#50967 = CARTESIAN_POINT ( 'NONE',  ( 171.6880688175457408, 289.7684859944451432, 2.704731161792437888 ) ) ;
#50968 = DIRECTION ( 'NONE',  ( -0.8660254037844387076, -0.4999999999999998890, -0.000000000000000000 ) ) ;
#50969 = CARTESIAN_POINT ( 'NONE',  ( 81.17742577809939064, 43.43109523646555203, -9.910019672670513202 ) ) ;
#50970 = DIRECTION ( 'NONE',  ( -0.7492053821869066876, -0.6623377501714446947, 0.000000000000000000 ) ) ;
#50971 = CARTESIAN_POINT ( 'NONE',  ( 14.51920287573142510, 173.0643266524160424, 9.188101187500095079 ) ) ;
#50972 = CARTESIAN_POINT ( 'NONE',  ( 101.9066655502961964, 220.4548013555409511, -4.594050593750042211 ) ) ;
#50973 = CARTESIAN_POINT ( 'NONE',  ( 44.69460199273694911, 186.6115022471902023, -5.000000000000041744 ) ) ;
#50974 = CARTESIAN_POINT ( 'NONE',  ( 186.5064012131073810, 296.3665785887476432, -7.270687472978205612 ) ) ;
#50975 = CARTESIAN_POINT ( 'NONE',  ( 78.18546057057351106, 52.16385450527234013, 15.57755498089799850 ) ) ;
#50976 = DIRECTION ( 'NONE',  ( 0.5000000000000014433, -0.8660254037844378194, 0.000000000000000000 ) ) ;
#50977 = CARTESIAN_POINT ( 'NONE',  ( 153.1747891862213748, 277.6390251779605478, -8.000862867047169757 ) ) ;
#50978 = CARTESIAN_POINT ( 'NONE',  ( 194.8708600166808651, 293.1207648669033006, -14.79199694356877970 ) ) ;
#50979 = EDGE_CURVE ( 'NONE', #22323, #76711, #55182, .T. ) ;
#50980 = CARTESIAN_POINT ( 'NONE',  ( 84.19352825665725959, 50.57172232247530275, 13.77707419306082670 ) ) ;
#50981 = CARTESIAN_POINT ( 'NONE',  ( 182.9159104275373977, 268.0747678481671414, -14.89985435326638630 ) ) ;
#50982 = VECTOR ( 'NONE', #33107, 1000.000000000000000 ) ;
#50983 = CARTESIAN_POINT ( 'NONE',  ( 178.7452121208765448, 291.6717820129654228, -9.156458492754065759 ) ) ;
#50984 = EDGE_CURVE ( 'NONE', #52516, #76128, #70894, .T. ) ;
#50985 = CARTESIAN_POINT ( 'NONE',  ( 172.5304191843750345, 263.6019457708129039, -15.41392963016842721 ) ) ;
#50986 = CARTESIAN_POINT ( 'NONE',  ( 74.78872445064843077, 223.1744531367911293, 4.594050593750047540 ) ) ;
#50987 = EDGE_CURVE ( 'NONE', #82530, #23627, #71400, .T. ) ;
#50988 = EDGE_CURVE ( 'NONE', #49426, #85879, #40954, .T. ) ;
#50989 = CARTESIAN_POINT ( 'NONE',  ( -14.45613220355349426, 103.0143348366940046, 11.63587646907208573 ) ) ;
#50991 = CARTESIAN_POINT ( 'NONE',  ( 86.16743810126995129, 43.04331322985106567, -1.056965546583657822 ) ) ;
#50990 = CARTESIAN_POINT ( 'NONE',  ( 157.0848929289108469, 258.5679796760466047, 17.57466231005294688 ) ) ;
#50992 = CARTESIAN_POINT ( 'NONE',  ( 148.9671336697298045, 272.6283511565604840, 12.24371685916078611 ) ) ;
#50993 = CARTESIAN_POINT ( 'NONE',  ( 199.0363797504450929, 285.9058730480928716, -17.12190301149298222 ) ) ;
#50994 = CARTESIAN_POINT ( 'NONE',  ( 160.6734846709049691, 282.6943762970620924, -6.583290857611773461 ) ) ;
#50995 = CARTESIAN_POINT ( 'NONE',  ( 28.71100085020356474, 39.68290643055189548, 3.479690158560446702E-15 ) ) ;
#50996 = CARTESIAN_POINT ( 'NONE',  ( 192.6679047218190135, 296.9363953644068488, -13.34486378385621386 ) ) ;
#50997 = CARTESIAN_POINT ( 'NONE',  ( 127.3796741259112792, 255.8967562850346553, -4.648177544792955347E-16 ) ) ;
#50998 = EDGE_LOOP ( 'NONE', ( #89984, #28745, #24049, #60020 ) ) ;
#50999 = CARTESIAN_POINT ( 'NONE',  ( 20.42541317417268942, 33.83396525600390703, -2.839279412974133887 ) ) ;
#51000 = CARTESIAN_POINT ( 'NONE',  ( -29.91485116994501325, 25.08783183303773967, 10.00000000000000000 ) ) ;
#51001 = CARTESIAN_POINT ( 'NONE',  ( 192.4743214706506365, 297.2716913909250707, -12.17804856100553046 ) ) ;
#51002 = CARTESIAN_POINT ( 'NONE',  ( 60.28305926085680966, 205.6115022471902591, 10.00000000000009592 ) ) ;
#51003 = EDGE_CURVE ( 'NONE', #3615, #8702, #3502, .T. ) ;
#51004 = EDGE_CURVE ( 'NONE', #16059, #66385, #57663, .T. ) ;
#51005 = VERTEX_POINT ( 'NONE', #11103 ) ;
#51006 = CARTESIAN_POINT ( 'NONE',  ( 70.83557099577411975, 60.89137392342752975, 14.54819139492075841 ) ) ;
#51007 = DIRECTION ( 'NONE',  ( -0.8560416229147732592, -0.5169068966820244970, 0.000000000000000000 ) ) ;
#51008 = CARTESIAN_POINT ( 'NONE',  ( 193.8475705658754578, 288.0377294361514373, 16.93899091255358869 ) ) ;
#51009 = CARTESIAN_POINT ( 'NONE',  ( -19.65312891409030271, 93.06504152958497400, 10.00000000000000888 ) ) ;
#51010 = CARTESIAN_POINT ( 'NONE',  ( 130.8641296692885305, 256.3615022471903444, 5.000000000000046185 ) ) ;
#51011 = CARTESIAN_POINT ( 'NONE',  ( 205.1300674467857164, 275.3512963525735131, -12.60245643603069610 ) ) ;
#51012 = CARTESIAN_POINT ( 'NONE',  ( 75.37222269001998143, 53.48600193327490615, 16.03910331961625246 ) ) ;
#51013 = VERTEX_POINT ( 'NONE', #96720 ) ;
#51014 = CARTESIAN_POINT ( 'NONE',  ( 190.5844311467533316, 299.4370547860769989, -6.522056084446611557 ) ) ;
#51015 = CARTESIAN_POINT ( 'NONE',  ( 188.7150346277363155, 272.5491880637262057, 16.57045186533353487 ) ) ;
#51016 = ORIENTED_EDGE ( 'NONE', *, *, #92741, .T. ) ;
#51017 = CARTESIAN_POINT ( 'NONE',  ( 163.2442700311756596, 247.8996255919473697, 11.14021925110252020 ) ) ;
#51018 = CARTESIAN_POINT ( 'NONE',  ( 81.51603451045065185, 42.23037173800174315, -8.032388100303403888 ) ) ;
#51019 = CARTESIAN_POINT ( 'NONE',  ( 77.30032487123098406, 63.32994978619627346, -15.17488454575836521 ) ) ;
#51020 = ORIENTED_EDGE ( 'NONE', *, *, #83508, .F. ) ;
#51021 = CARTESIAN_POINT ( 'NONE',  ( 191.1374494863389373, 291.0598754717474890, 14.59185211929525749 ) ) ;
#51022 = CARTESIAN_POINT ( 'NONE',  ( 158.8391802440265508, 255.5294649151923636, 17.60341940305819364 ) ) ;
#51023 = CARTESIAN_POINT ( 'NONE',  ( 151.1618603905361624, 248.8923013555409796, 4.594050593750050204 ) ) ;
#51024 = CARTESIAN_POINT ( 'NONE',  ( 205.1877054856971938, 273.8747620413109871, 10.81913124959201689 ) ) ;
#51025 = CARTESIAN_POINT ( 'NONE',  ( 201.1755594471486859, 282.2007051268825535, -18.15567516623250910 ) ) ;
#51026 = AXIS2_PLACEMENT_3D ( 'NONE', #43719, #98947, #30019 ) ;
#51027 = CARTESIAN_POINT ( 'NONE',  ( 34.90123498099573851, 22.01110640527294393, 2.839279412974134775 ) ) ;
#51028 = FACE_OUTER_BOUND ( 'NONE', #7815, .T. ) ;
#51029 = FACE_OUTER_BOUND ( 'NONE', #74837, .T. ) ;
#51031 = VECTOR ( 'NONE', #15286, 1000.000000000000000 ) ;
#51030 = CARTESIAN_POINT ( 'NONE',  ( 87.64858773784966672, 45.45714736155468927, 6.714362014711301896 ) ) ;
#51032 = EDGE_LOOP ( 'NONE', ( #78816, #52304, #48168, #76488 ) ) ;
#51033 = CARTESIAN_POINT ( 'NONE',  ( 86.70911053808110580, 46.89117940024963360, 10.21290512048939902 ) ) ;
#51035 = CARTESIAN_POINT ( 'NONE',  ( 162.7552554279882031, 272.8056902114326476, -16.37138898352977634 ) ) ;
#51034 = CARTESIAN_POINT ( 'NONE',  ( 163.8040269124969939, 246.9300982336122559, 6.025552750865228013 ) ) ;
#51036 = CARTESIAN_POINT ( 'NONE',  ( 85.54106661513783649, 48.65811287445264810, 12.45824154186499833 ) ) ;
#51037 = CYLINDRICAL_SURFACE ( 'NONE', #26276, 10.00000000000010658 ) ;
#51038 = CARTESIAN_POINT ( 'NONE',  ( 152.5423653171682474, 268.4358682943698682, -15.78187745328793490 ) ) ;
#51039 = CARTESIAN_POINT ( 'NONE',  ( 82.15463706511576447, 40.84277258114416753, 1.595534587534163995 ) ) ;
#51040 = CARTESIAN_POINT ( 'NONE',  ( 167.1313658916855900, 286.5916946420441604, -4.904932445929851781 ) ) ;
#51041 = CARTESIAN_POINT ( 'NONE',  ( 169.5532941354267962, 267.3202395055815259, 16.92450780793635090 ) ) ;
#51042 = CARTESIAN_POINT ( 'NONE',  ( 180.9973211531476238, 256.8713260056199488, 4.953687155094200101 ) ) ;
#51043 = CARTESIAN_POINT ( 'NONE',  ( 100.7969837277561282, 222.8768266524159856, -9.188101187500091527 ) ) ;
#51044 = VERTEX_POINT ( 'NONE', #65278 ) ;
#51045 = CARTESIAN_POINT ( 'NONE',  ( 190.8623743139412454, 300.0636657654615647, 8.577953960666059530 ) ) ;
#51046 = CARTESIAN_POINT ( 'NONE',  ( 166.8260628573998474, 278.3289732347862468, -13.29658692297307176 ) ) ;
#51047 = EDGE_LOOP ( 'NONE', ( #58789, #79890 ) ) ;
#51048 = AXIS2_PLACEMENT_3D ( 'NONE', #9684, #49651, #32952 ) ;
#51049 = ORIENTED_EDGE ( 'NONE', *, *, #32096, .T. ) ;
#51050 = CARTESIAN_POINT ( 'NONE',  ( 87.10310940712852812, 46.00011840676027219, -8.174603884307702018 ) ) ;
#51051 = CARTESIAN_POINT ( 'NONE',  ( 176.9023546970497875, 292.4662729303109927, -2.727046248897896596 ) ) ;
#51052 = CARTESIAN_POINT ( 'NONE',  ( 157.5520850189458884, 257.7587792392113215, 16.71892742266126319 ) ) ;
#51053 = CARTESIAN_POINT ( 'NONE',  ( 7.357472841178069878, 27.18080186712591484, 3.090169943749475401 ) ) ;
#51054 = LINE ( 'NONE', #97211, #18824 ) ;
#51055 = EDGE_LOOP ( 'NONE', ( #59994, #14792, #49814, #80658, #61751, #87391, #36961, #44258, #12701, #46519, #19920, #88098, #69944, #34124, #23713, #89691, #93946, #26144, #96073, #94059 ) ) ;
#51056 = VECTOR ( 'NONE', #31018, 1000.000000000000227 ) ;
#51057 =( BOUNDED_CURVE ( )  B_SPLINE_CURVE ( 2, ( #55698, #1036, #49137, #23818, #17218, #31915, #62819, #85692, #93775 ),
 .UNSPECIFIED., .F., .F. ) 
 B_SPLINE_CURVE_WITH_KNOTS ( ( 3, 2, 2, 2, 3 ),
 ( 0.4959677419354838745, 0.4973118279569892497, 0.5000000000000000000, 0.5026881720430107503, 0.5040322580645161255 ),
 .UNSPECIFIED. ) 
 CURVE ( )  GEOMETRIC_REPRESENTATION_ITEM ( )  RATIONAL_B_SPLINE_CURVE ( ( 0.9330127018922194093, 0.9330127018922194093, 1.000000000000000000, 0.8660254037844387076, 1.000000000000000000, 0.8660254037844387076, 1.000000000000000000, 0.9330127018922194093, 0.9330127018922194093 ) ) 
 REPRESENTATION_ITEM ( '' )  );
#51058 = CARTESIAN_POINT ( 'NONE',  ( 187.1504858166771896, 267.1035762790165222, -14.63698944013293968 ) ) ;
#51059 = DIRECTION ( 'NONE',  ( -0.5000000000000011102, -0.8660254037844380415, 0.000000000000000000 ) ) ;
#51060 = ORIENTED_EDGE ( 'NONE', *, *, #86050, .F. ) ;
#51061 = CARTESIAN_POINT ( 'NONE',  ( 70.78770575672112386, 64.97714170464311678, 12.24875154412454314 ) ) ;
#51062 = ADVANCED_FACE ( 'NONE', ( #58168 ), #89152, .F. ) ;
#51063 = CARTESIAN_POINT ( 'NONE',  ( 191.4217213000991364, 263.9549948794881971, -7.974474884843431255 ) ) ;
#51064 = CARTESIAN_POINT ( 'NONE',  ( 13.95070015838929400, 188.8615022471903160, 5.000000000000046185 ) ) ;
#51065 = CARTESIAN_POINT ( 'NONE',  ( 83.42856800471859913, 47.51705139073896333, 11.98419555216981003 ) ) ;
#51067 = CARTESIAN_POINT ( 'NONE',  ( 69.64257305926975050, 62.32707857316431443, -13.51840679933402711 ) ) ;
#51066 = CARTESIAN_POINT ( 'NONE',  ( 127.4808708382166316, 256.6589784336661637, -6.496448406907675876E-16 ) ) ;
#51068 = PLANE ( 'NONE',  #13891 ) ;
#51069 = ORIENTED_EDGE ( 'NONE', *, *, #31427, .F. ) ;
#51070 = CARTESIAN_POINT ( 'NONE',  ( 204.9134960529544287, 275.7264090101555212, 14.56629498631681408 ) ) ;
#51071 = CARTESIAN_POINT ( 'NONE',  ( 81.82384807472087118, 49.02608080520630551, 13.57111770008744500 ) ) ;
#51072 = CARTESIAN_POINT ( 'NONE',  ( 82.36513698948819240, 40.35680866276053536, -0.9065428034150362357 ) ) ;
#51073 = CARTESIAN_POINT ( 'NONE',  ( 192.9064638172013417, 270.9369261147751331, 14.92505667092759758 ) ) ;
#51075 = EDGE_CURVE ( 'NONE', #21534, #88756, #41080, .T. ) ;
#51074 = CARTESIAN_POINT ( 'NONE',  ( 178.6016452153454850, 285.1529245495667624, 13.66975983559747831 ) ) ;
#51076 = CARTESIAN_POINT ( 'NONE',  ( 76.12676022442599333, 51.56486861732116012, -16.17662836183246711 ) ) ;
#51077 = ADVANCED_FACE ( 'NONE', ( #66279 ), #41620, .T. ) ;
#51078 = CARTESIAN_POINT ( 'NONE',  ( 196.0123035030964047, 280.0493583844649947, -16.77947975799478542 ) ) ;
#51079 = CARTESIAN_POINT ( 'NONE',  ( 142.9371257517045137, 259.7655487066560340, -7.305945665944389766 ) ) ;
#51080 = CARTESIAN_POINT ( 'NONE',  ( 79.32243881128263752, 47.71223523376870190, 13.60867400304461050 ) ) ;
#51081 = CARTESIAN_POINT ( 'NONE',  ( 206.8014039808918199, 271.9024147334357053, 6.414352906864584369 ) ) ;
#51082 = CARTESIAN_POINT ( 'NONE',  ( 206.8317058779879574, 272.4039721336197317, -10.41591514895975834 ) ) ;
#51083 = LINE ( 'NONE', #59164, #9507 ) ;
#51084 = CARTESIAN_POINT ( 'NONE',  ( 163.3723087697842971, 247.6778559913402091, -10.08585062664141319 ) ) ;
#51085 = EDGE_CURVE ( 'NONE', #95597, #31449, #22062, .T. ) ;
#51086 = DIRECTION ( 'NONE',  ( -0.8660254037844387076, -0.4999999999999998890, -0.000000000000000000 ) ) ;
#51087 = VECTOR ( 'NONE', #72913, 1000.000000000000000 ) ;
#51088 = CARTESIAN_POINT ( 'NONE',  ( 185.9501193373536125, 265.4400708382679568, 13.68843392893370314 ) ) ;
#51089 = CARTESIAN_POINT ( 'NONE',  ( -22.47745507583526958, 59.95093256704510054, -10.00000000000000000 ) ) ;
#51090 = CARTESIAN_POINT ( 'NONE',  ( 29.61202869050421427, 35.83478043621390441, -8.090169943749479842 ) ) ;
#51091 = CARTESIAN_POINT ( 'NONE',  ( -57.88150100324660485, 35.92665207732902388, -10.00000000000000000 ) ) ;
#51092 = LINE ( 'NONE', #64824, #33060 ) ;
#51093 = CARTESIAN_POINT ( 'NONE',  ( 50.40832357593285451, 87.79023373031367328, -10.00000000000000000 ) ) ;
#51094 = AXIS2_PLACEMENT_3D ( 'NONE', #5829, #52419, #4855 ) ;
#51095 = CARTESIAN_POINT ( 'NONE',  ( 83.98302130751108052, 43.28427656522794820, -6.397989684056143211 ) ) ;
#51096 = EDGE_CURVE ( 'NONE', #48833, #40485, #20906, .T. ) ;
#51097 = CARTESIAN_POINT ( 'NONE',  ( 15.54743449484293372, 179.7833772461660544, -9.188101187500095079 ) ) ;
#51098 = CARTESIAN_POINT ( 'NONE',  ( 207.3567728362337732, 271.1044343289145218, 2.587868728010163100 ) ) ;
#51099 = ORIENTED_EDGE ( 'NONE', *, *, #27553, .F. ) ;
#51100 = EDGE_CURVE ( 'NONE', #73348, #41972, #26001, .T. ) ;
#51101 = CARTESIAN_POINT ( 'NONE',  ( 87.19358828159984398, 46.06351791880832991, 8.846884648199045742 ) ) ;
#51102 = ADVANCED_FACE ( 'NONE', ( #93424 ), #18397, .T. ) ;
#51103 = DIRECTION ( 'NONE',  ( -0.3074612162317687525, 0.9515606131578174809, 0.000000000000000000 ) ) ;
#51104 = CARTESIAN_POINT ( 'NONE',  ( 164.4405316900629259, 245.8276396196081350, -6.144538123479245328 ) ) ;
#51105 = CARTESIAN_POINT ( 'NONE',  ( -19.65312891409030271, 93.06504152958497400, -10.00000000000000888 ) ) ;
#51106 = CARTESIAN_POINT ( 'NONE',  ( 51.43353571204313823, 194.3768266524159856, -9.188101187500093303 ) ) ;
#51107 = CARTESIAN_POINT ( 'NONE',  ( 86.78549426258130950, 45.83013854792883990, 8.849882187839872572 ) ) ;
#51108 = CARTESIAN_POINT ( 'NONE',  ( 171.5767533171608932, 286.7469205890667467, 7.455704898055432572 ) ) ;
#51109 = CARTESIAN_POINT ( 'NONE',  ( 190.4240181651484818, 300.8229208869809668, -4.214281362166949485 ) ) ;
#51110 = CARTESIAN_POINT ( 'NONE',  ( 42.17466224797323804, 36.30066082961425877, -10.00000000000000533 ) ) ;
#51111 = CARTESIAN_POINT ( 'NONE',  ( 178.3571982967953602, 292.6181790745828835, -7.174879954037646002 ) ) ;
#51112 = CARTESIAN_POINT ( 'NONE',  ( 147.0721334091522294, 275.9105878882373304, 0.7242168585908188572 ) ) ;
#51113 = EDGE_CURVE ( 'NONE', #16838, #77804, #86342, .T. ) ;
#51114 = VECTOR ( 'NONE', #5486, 1000.000000000000000 ) ;
#51115 = CARTESIAN_POINT ( 'NONE',  ( 176.1048462933576388, 274.8593126533075974, 17.09347264305319314 ) ) ;
#51116 = LINE ( 'NONE', #80076, #29537 ) ;
#51117 = CARTESIAN_POINT ( 'NONE',  ( 68.55506308078156508, 67.87136273880065573, -7.775597205189836991 ) ) ;
#51118 = EDGE_CURVE ( 'NONE', #87111, #28084, #96763, .T. ) ;
#51119 = CARTESIAN_POINT ( 'NONE',  ( 88.69951781898578247, 222.0177522451418781, -10.00000000000009592 ) ) ;
#51120 = ADVANCED_FACE ( 'NONE', ( #88853 ), #73592, .F. ) ;
#51121 = CARTESIAN_POINT ( 'NONE',  ( -4.429217378738782962, 26.01694505731172313, -10.00000000000000000 ) ) ;
#51122 = CARTESIAN_POINT ( 'NONE',  ( 105.6772241758911832, 218.4865022471901455, 1.119607411625061291E-15 ) ) ;
#51123 = FACE_OUTER_BOUND ( 'NONE', #45277, .T. ) ;
#51124 = CARTESIAN_POINT ( 'NONE',  ( 161.6384288741144815, 267.7291502596664259, -17.04636140397435895 ) ) ;
#51125 = VERTEX_POINT ( 'NONE', #12294 ) ;
#51126 = CARTESIAN_POINT ( 'NONE',  ( 64.42391676880970408, 201.8768266524159856, -9.188101187500091527 ) ) ;
#51127 = VERTEX_POINT ( 'NONE', #43153 ) ;
#51128 = CARTESIAN_POINT ( 'NONE',  ( 11.62691283633230377, 30.21091486745859811, -1.111400068045478839E-16 ) ) ;
#51129 = CARTESIAN_POINT ( 'NONE',  ( 146.8201187048455267, 276.3470901603510015, 4.112223577763169047 ) ) ;
#51130 = CARTESIAN_POINT ( 'NONE',  ( 67.17471155831628948, 67.15864351149404854, -8.572145057571571414 ) ) ;
#51131 = ORIENTED_EDGE ( 'NONE', *, *, #43638, .F. ) ;
#51132 = CARTESIAN_POINT ( 'NONE',  ( 171.3634068529735828, 286.5179807154004834, 7.728413769772275899 ) ) ;
#51133 = CARTESIAN_POINT ( 'NONE',  ( 207.2824254892180704, 271.6233028670009162, 6.274396967990798046 ) ) ;
#51134 = CARTESIAN_POINT ( 'NONE',  ( 78.08206365161463225, 61.83366292688850763, -15.70979438352861735 ) ) ;
#51135 = CARTESIAN_POINT ( 'NONE',  ( 28.38624132378439313, 39.49540643055189548, 3.479690158560446702E-15 ) ) ;
#51136 = CARTESIAN_POINT ( 'NONE',  ( 185.9440050421480919, 263.4269226037905014, 11.01369690752849984 ) ) ;
#51137 = CARTESIAN_POINT ( 'NONE',  ( 174.5432515410337544, 282.4104588529930311, -15.15290805577315680 ) ) ;
#51138 = CARTESIAN_POINT ( 'NONE',  ( 204.3531539698473978, 276.6969499677158524, 13.47943239092699841 ) ) ;
#51139 = ORIENTED_EDGE ( 'NONE', *, *, #17486, .F. ) ;
#51140 = CARTESIAN_POINT ( 'NONE',  ( 11.72364552993787967, 24.95586893147754282, 7.433330006724141015 ) ) ;
#51141 = LINE ( 'NONE', #81109, #33274 ) ;
#51142 = CARTESIAN_POINT ( 'NONE',  ( 70.89819722514211264, 70.25179532443134178, -6.076314343069640245 ) ) ;
#51143 = DIRECTION ( 'NONE',  ( -0.000000000000000000, 0.000000000000000000, -1.000000000000000000 ) ) ;
#51144 = ORIENTED_EDGE ( 'NONE', *, *, #85057, .F. ) ;
#51145 = CARTESIAN_POINT ( 'NONE',  ( 181.7035363212127379, 283.7571070694220907, 14.95731429925001343 ) ) ;
#51146 = B_SPLINE_CURVE_WITH_KNOTS ( 'NONE', 3,
 ( #66945, #58349, #28448, #28964, #82212, #81702, #66459, #13276, #4667, #76081, #89327, #82709, #97384, #27952, #50750, #43136, #58833, #52731, #83694, #21360, #45142, #89799, #19880, #51244 ),
 .UNSPECIFIED., .F., .F.,
 ( 4, 2, 2, 2, 2, 2, 2, 2, 2, 2, 2, 4 ),
 ( 0.000000000000000000, 0.1249999999999907851, 0.2499999999999815703, 0.3749999999999723554, 0.4374999999999739098, 0.4999999999999754641, 0.5624999999999769074, 0.6249999999999784617, 0.6874999999999799050, 0.7499999999999814593, 0.8749999999999906741, 1.000000000000000000 ),
 .UNSPECIFIED. ) ;
#51147 = CARTESIAN_POINT ( 'NONE',  ( 190.8860811105559208, 300.0226043892405414, 8.636347304323541252 ) ) ;
#51148 = CARTESIAN_POINT ( 'NONE',  ( 206.0930919633010774, 273.6832889610345774, -9.866500005465628220 ) ) ;
#51149 = ORIENTED_EDGE ( 'NONE', *, *, #31981, .T. ) ;
#51150 = ORIENTED_EDGE ( 'NONE', *, *, #49173, .F. ) ;
#51152 = FACE_OUTER_BOUND ( 'NONE', #12680, .T. ) ;
#51151 = CARTESIAN_POINT ( 'NONE',  ( 161.5757715694810770, 250.7895496999525449, -14.51803553215175135 ) ) ;
#51153 = CARTESIAN_POINT ( 'NONE',  ( -14.83262083840144996, 124.7156766241961208, 37.49999999999998579 ) ) ;
#51154 = ORIENTED_EDGE ( 'NONE', *, *, #22347, .F. ) ;
#51155 = CARTESIAN_POINT ( 'NONE',  ( 65.93191908977979665, 69.03888066652848465, -2.102623230407007604 ) ) ;
#51156 = CARTESIAN_POINT ( 'NONE',  ( 47.57035326562169075, 72.63383583914733777, -10.00000000000000000 ) ) ;
#51157 = CARTESIAN_POINT ( 'NONE',  ( 48.23560136428436351, 110.1272893647940521, 177.5919119679930134 ) ) ;
#51158 = CARTESIAN_POINT ( 'NONE',  ( 78.26468621063266085, 61.69794584189649811, -15.76854286150912010 ) ) ;
#51159 = EDGE_CURVE ( 'NONE', #43174, #98545, #35578, .T. ) ;
#51160 = CARTESIAN_POINT ( 'NONE',  ( 129.3483248890680954, 254.6744531367911577, 4.594050593750047540 ) ) ;
#51161 = CARTESIAN_POINT ( 'NONE',  ( 191.0900422946452011, 299.6693332556258724, 8.872191398975367349 ) ) ;
#51162 = CARTESIAN_POINT ( 'NONE',  ( 72.21491844529387549, 53.64441083166271085, 0.000000000000000000 ) ) ;
#51163 = CARTESIAN_POINT ( 'NONE',  ( 183.6064328101875844, 289.8855053871136533, -13.59221500815075423 ) ) ;
#51164 = AXIS2_PLACEMENT_3D ( 'NONE', #243, #16437, #78257 ) ;
#51165 = ORIENTED_EDGE ( 'NONE', *, *, #66531, .F. ) ;
#51166 = CARTESIAN_POINT ( 'NONE',  ( 163.9354095869165633, 246.7025367662834014, -7.289870401565430313 ) ) ;
#51167 = ORIENTED_EDGE ( 'NONE', *, *, #38061, .T. ) ;
#51168 = ORIENTED_EDGE ( 'NONE', *, *, #37013, .T. ) ;
#51169 = CARTESIAN_POINT ( 'NONE',  ( 159.6898930778639283, 254.0559870643349143, 16.90891900388599822 ) ) ;
#51170 = DIRECTION ( 'NONE',  ( 1.000000000000000000, 0.000000000000000000, 0.000000000000000000 ) ) ;
#51171 = CARTESIAN_POINT ( 'NONE',  ( 79.95842099707557793, 204.7202760586659167, -5.415160957724236172E-17 ) ) ;
#51172 = ORIENTED_EDGE ( 'NONE', *, *, #24311, .T. ) ;
#51173 = CARTESIAN_POINT ( 'NONE',  ( 47.46694519036041982, 73.19305994210745325, 177.5919119679930134 ) ) ;
#51174 = CARTESIAN_POINT ( 'NONE',  ( 150.4255120825602887, 270.1023656488765710, 15.17857413906334507 ) ) ;
#51175 = CARTESIAN_POINT ( 'NONE',  ( 171.8445276903575518, 276.6680178762132982, 16.23204015318158966 ) ) ;
#51176 = ORIENTED_EDGE ( 'NONE', *, *, #28876, .F. ) ;
#51177 = CARTESIAN_POINT ( 'NONE',  ( 75.74815782865833569, 62.74121906712248631, -15.01347554402796192 ) ) ;
#51178 = CARTESIAN_POINT ( 'NONE',  ( 201.4463813434794019, 281.7316278426353620, -17.16864527463587820 ) ) ;
#51179 = CARTESIAN_POINT ( 'NONE',  ( 203.0862352702880003, 278.8913175244117610, -15.09542727681365015 ) ) ;
#51180 = EDGE_LOOP ( 'NONE', ( #28267, #32713 ) ) ;
#51181 = CARTESIAN_POINT ( 'NONE',  ( 191.9824032073976241, 287.6194387751458521, -17.05427143794285882 ) ) ;
#51182 = CARTESIAN_POINT ( 'NONE',  ( 163.8291868588114255, 260.4160011549212754, -16.17568023803453414 ) ) ;
#51183 = CARTESIAN_POINT ( 'NONE',  ( 77.35605062658235909, 53.90549147004347930, -16.44166418353362502 ) ) ;
#51184 = EDGE_CURVE ( 'NONE', #56966, #17015, #44155, .T. ) ;
#51185 = CARTESIAN_POINT ( 'NONE',  ( 53.12030748017507165, 208.1427522451419350, 10.00000000000009415 ) ) ;
#51186 = CARTESIAN_POINT ( 'NONE',  ( 1.638219116881074022, 26.38162155862026736, 177.5919119679930134 ) ) ;
#51187 = CYLINDRICAL_SURFACE ( 'NONE', #85297, 70.00000000000002842 ) ;
#51188 = CARTESIAN_POINT ( 'NONE',  ( 126.7502486777147794, 253.1744531367911009, 4.594050593750047540 ) ) ;
#51189 = ORIENTED_EDGE ( 'NONE', *, *, #86793, .F. ) ;
#51190 = AXIS2_PLACEMENT_3D ( 'NONE', #35865, #3010, #66766 ) ;
#51191 = CARTESIAN_POINT ( 'NONE',  ( 191.0862225170008628, 299.6759493045793192, -9.402218231374108726 ) ) ;
#51192 = CARTESIAN_POINT ( 'NONE',  ( 87.11349487006070547, 46.19076519147612458, 8.411924245371466213 ) ) ;
#51193 = CARTESIAN_POINT ( 'NONE',  ( 205.4608097893652996, 273.5822659152986489, -10.72688443308411088 ) ) ;
#51194 = EDGE_CURVE ( 'NONE', #57311, #57476, #80741, .T. ) ;
#51195 = VECTOR ( 'NONE', #19331, 1000.000000000000114 ) ;
#51196 = CARTESIAN_POINT ( 'NONE',  ( 204.8189571845487080, 275.8901551335242175, 13.43702398685204358 ) ) ;
#51197 = EDGE_CURVE ( 'NONE', #14773, #27771, #12236, .T. ) ;
#51198 = CARTESIAN_POINT ( 'NONE',  ( 40.34888600819125060, 126.6204015641749834, 10.00000000000000000 ) ) ;
#51199 = CARTESIAN_POINT ( 'NONE',  ( 178.7600897929267774, 254.1784503161647706, 4.743017227330367014 ) ) ;
#51200 = ORIENTED_EDGE ( 'NONE', *, *, #27516, .T. ) ;
#51201 = CARTESIAN_POINT ( 'NONE',  ( 76.71780308168534646, 55.72448719287293528, 16.16777461468364052 ) ) ;
#51202 = CARTESIAN_POINT ( 'NONE',  ( 126.8768043691498377, 237.3927522451418497, 10.00000000000009948 ) ) ;
#51203 = CARTESIAN_POINT ( 'NONE',  ( 72.57809076984500507, 71.31855580840982611, -5.985130625757507872 ) ) ;
#51204 = CARTESIAN_POINT ( 'NONE',  ( 152.8894687064977234, 278.3516875449029158, -6.243347624783317507 ) ) ;
#51205 = CARTESIAN_POINT ( 'NONE',  ( 198.5119022532241786, 266.2458289876958588, 0.9081415792431625222 ) ) ;
#51206 = DIRECTION ( 'NONE',  ( -0.7886751345948034286, 0.2113248654051702868, 0.5773502691896449379 ) ) ;
#51207 = CARTESIAN_POINT ( 'NONE',  ( 68.30570690293387770, 69.17111502577031956, 4.863477417514607382 ) ) ;
#51208 = B_SPLINE_CURVE_WITH_KNOTS ( 'NONE', 3,
 ( #68996, #44694, #61398, #46183, #90871, #68010, #22410 ),
 .UNSPECIFIED., .F., .F.,
 ( 4, 1, 2, 4 ),
 ( 0.000000000000000000, 0.1620005363610098892, 0.2430008045415152085, 0.3240010727220205000 ),
 .UNSPECIFIED. ) ;
#51209 = CARTESIAN_POINT ( 'NONE',  ( 204.7519188734507622, 276.0062688943993408, -12.76027478560537531 ) ) ;
#51210 = CARTESIAN_POINT ( 'NONE',  ( 194.0638893473842757, 269.5056305575998863, 12.07270889207231157 ) ) ;
#51211 = CARTESIAN_POINT ( 'NONE',  ( 10.23294337622180628, 30.00034080476288878, -1.878358725466461243E-16 ) ) ;
#51212 = CARTESIAN_POINT ( 'NONE',  ( 190.2935937139882299, 301.0488226629397559, 4.649863831023156813 ) ) ;
#51213 = PLANE ( 'NONE',  #27285 ) ;
#51214 = DIRECTION ( 'NONE',  ( 0.000000000000000000, 0.000000000000000000, 1.000000000000000000 ) ) ;
#51215 = CARTESIAN_POINT ( 'NONE',  ( 155.5066938333533528, 261.3015006940112244, -18.40036130547566273 ) ) ;
#51216 = CARTESIAN_POINT ( 'NONE',  ( 161.5454122949074645, 250.8421335059953776, 14.24337924419696932 ) ) ;
#51217 = ADVANCED_FACE ( 'NONE', ( #60840 ), #91801, .T. ) ;
#51218 = CARTESIAN_POINT ( 'NONE',  ( 140.5888732624034674, 238.6427522451417644, 1.119607411625061291E-15 ) ) ;
#51219 = CARTESIAN_POINT ( 'NONE',  ( 175.9353947587521816, 285.3059048581015986, -12.02703367433279169 ) ) ;
#51220 = ORIENTED_EDGE ( 'NONE', *, *, #42423, .T. ) ;
#51221 = CARTESIAN_POINT ( 'NONE',  ( 196.4351339088274813, 290.4113630087520050, 17.20526457544535504 ) ) ;
#51222 = CARTESIAN_POINT ( 'NONE',  ( 151.2964716097791325, 268.5938194963972592, -15.66250187539618111 ) ) ;
#51223 = CARTESIAN_POINT ( 'NONE',  ( 3.802138503898990329, 166.8768266524160140, 9.188101187500096856 ) ) ;
#51224 = AXIS2_PLACEMENT_3D ( 'NONE', #84409, #32159, #31150 ) ;
#51225 = CARTESIAN_POINT ( 'NONE',  ( 48.02338713675939630, 198.5333772461660828, 9.188101187500095079 ) ) ;
#51226 = CARTESIAN_POINT ( 'NONE',  ( 85.93706912677129139, 45.09247296462667265, 8.501039739313545951 ) ) ;
#51227 = CARTESIAN_POINT ( 'NONE',  ( 25.69932979004302709, 23.03677371833802212, 10.00000000000000533 ) ) ;
#51228 = CARTESIAN_POINT ( 'NONE',  ( 85.81856918057869166, 48.58455003273027017, 12.27698013059672455 ) ) ;
#51229 = CARTESIAN_POINT ( 'NONE',  ( 157.4211152037729562, 257.9856256133486454, -16.71526195140576831 ) ) ;
#51231 = AXIS2_PLACEMENT_3D ( 'NONE', #3103, #79616, #42545 ) ;
#51230 = CARTESIAN_POINT ( 'NONE',  ( 191.9832910268169996, 291.9740856320129296, -14.33083625909805825 ) ) ;
#51232 = CARTESIAN_POINT ( 'NONE',  ( 74.21788993013733204, 55.48536492223286842, -16.11972369606550259 ) ) ;
#51233 = CARTESIAN_POINT ( 'NONE',  ( 167.4739133672058529, 256.7134934739360688, 13.89013134216980738 ) ) ;
#51234 = EDGE_CURVE ( 'NONE', #68688, #14532, #66582, .T. ) ;
#51235 = CARTESIAN_POINT ( 'NONE',  ( 181.1603734054039876, 255.6401209734635529, 2.176029259874446176 ) ) ;
#51236 = CARTESIAN_POINT ( 'NONE',  ( 150.4572752258758612, 270.0473502708459250, 15.21885120838634187 ) ) ;
#51237 = VECTOR ( 'NONE', #86888, 1000.000000000000114 ) ;
#51238 = B_SPLINE_CURVE_WITH_KNOTS ( 'NONE', 3,
 ( #787, #91533, #92533, #6893, #85964, #52994, #39269, #31673, #78310, #100117, #8891, #54465, #39760, #7387, #84929, #45869 ),
 .UNSPECIFIED., .F., .F.,
 ( 4, 2, 2, 2, 2, 2, 2, 4 ),
 ( 0.0001980335298249143758, 0.0002838333738372856088, 0.0003267332958434711982, 0.0003696332178496568419, 0.0004125331398558424855, 0.0004554330618620280749, 0.0005412329058743169628, 0.0008844322819235596843 ),
 .UNSPECIFIED. ) ;
#51239 = CARTESIAN_POINT ( 'NONE',  ( 54.65389413625798909, 192.3615022471901739, 5.000000000000051514 ) ) ;
#51240 = DIRECTION ( 'NONE',  ( 0.8660254037844383745, 0.5000000000000003331, -0.000000000000000000 ) ) ;
#51241 = CARTESIAN_POINT ( 'NONE',  ( 189.8314329296643450, 301.8493086226544619, -0.8085564604676659384 ) ) ;
#51242 = CARTESIAN_POINT ( 'NONE',  ( 11.67712314985746858, 186.7369531367911293, -4.594050593750048428 ) ) ;
#51243 = CARTESIAN_POINT ( 'NONE',  ( 72.86910405259972379, 71.04354916989078106, -7.648857478963559942 ) ) ;
#51244 = CARTESIAN_POINT ( 'NONE',  ( 78.70150085959764397, 59.83202584994826623, 16.12694553795978081 ) ) ;
#51245 = CARTESIAN_POINT ( 'NONE',  ( 31.19238438139944947, 38.98502408145593989, -5.678558825948271327 ) ) ;
#51246 = CARTESIAN_POINT ( 'NONE',  ( 155.5207183646172950, 261.6826666266933898, -16.99780945766855922 ) ) ;
#51247 = CARTESIAN_POINT ( 'NONE',  ( 179.7554519724740487, 276.9442998558859586, 16.29670716075235859 ) ) ;
#51248 = CARTESIAN_POINT ( 'NONE',  ( 185.0684497205900527, 286.3477220876792444, 16.15350733335134237 ) ) ;
#51249 = CARTESIAN_POINT ( 'NONE',  ( 148.6023484834014425, 275.2601776331305814, 7.517535991345212665 ) ) ;
#51250 = CARTESIAN_POINT ( 'NONE',  ( 176.9896994409250510, 260.9405379847559630, -13.11837235889534625 ) ) ;
#51251 =( NAMED_UNIT ( * ) SI_UNIT ( $, .STERADIAN. ) SOLID_ANGLE_UNIT ( ) );
#51252 = EDGE_CURVE ( 'NONE', #69843, #90334, #74, .T. ) ;
#51253 = CARTESIAN_POINT ( 'NONE',  ( 11.72364552993787967, 24.95586893147754282, 7.433330006724141015 ) ) ;
#51254 = CARTESIAN_POINT ( 'NONE',  ( 71.94719849994383765, 72.57089041204893931, 1.653882010069143815 ) ) ;
#51255 = CARTESIAN_POINT ( 'NONE',  ( 82.66013068336778247, 54.08499358714050942, 15.52290316209530019 ) ) ;
#51256 = CARTESIAN_POINT ( 'NONE',  ( 183.8754313647489198, 256.5225093191261294, -2.022205659181245174 ) ) ;
#51257 = CARTESIAN_POINT ( 'NONE',  ( 193.8913555215501390, 294.8173164187117550, 15.40725395879721837 ) ) ;
#51258 = ORIENTED_EDGE ( 'NONE', *, *, #97670, .T. ) ;
#51259 = AXIS2_PLACEMENT_3D ( 'NONE', #62267, #14201, #60764 ) ;
#51260 = CARTESIAN_POINT ( 'NONE',  ( 85.74058674982732953, 45.55718474559918008, -8.560518791363312729 ) ) ;
#51261 = CARTESIAN_POINT ( 'NONE',  ( 27.53097578467762219, 16.86426979415090699, -3.090169943749474069 ) ) ;
#51262 = CARTESIAN_POINT ( 'NONE',  ( 159.9470087484377814, 253.6106496594791508, -16.54933891566789939 ) ) ;
#51263 = ORIENTED_EDGE ( 'NONE', *, *, #13159, .T. ) ;
#51264 = CARTESIAN_POINT ( 'NONE',  ( 153.4619471835925708, 264.8431057800031567, 16.95044998314351758 ) ) ;
#51265 = CARTESIAN_POINT ( 'NONE',  ( 67.93373562898584339, 69.81538817605719771, 0.4299488895426710755 ) ) ;
#51266 = VECTOR ( 'NONE', #5182, 1000.000000000000114 ) ;
#51267 = CARTESIAN_POINT ( 'NONE',  ( 48.21858077004885246, 104.0489273421469818, 10.00000000000000000 ) ) ;
#51268 = CARTESIAN_POINT ( 'NONE',  ( 203.1044072055706806, 278.8598428092302584, -16.67109798570195878 ) ) ;
#51269 = ORIENTED_EDGE ( 'NONE', *, *, #75084, .T. ) ;
#51271 = CARTESIAN_POINT ( 'NONE',  ( 164.3010377730689981, 246.0692501711882869, 7.247566249275159578 ) ) ;
#51270 = CARTESIAN_POINT ( 'NONE',  ( 164.1439264839012822, 246.7246349093515221, -4.787792474024944234 ) ) ;
#51272 = CARTESIAN_POINT ( 'NONE',  ( 153.4289928607825573, 264.9001843414388873, 17.27358709529985958 ) ) ;
#51273 = ORIENTED_EDGE ( 'NONE', *, *, #57176, .F. ) ;
#51274 = FACE_OUTER_BOUND ( 'NONE', #28126, .T. ) ;
#51275 = CARTESIAN_POINT ( 'NONE',  ( 80.48346613340457623, 57.68579040447578166, -16.59506630531065241 ) ) ;
#51276 = CARTESIAN_POINT ( 'NONE',  ( 177.9668643227034579, 263.6129378440573987, 15.31797677519840306 ) ) ;
#51277 = VERTEX_POINT ( 'NONE', #23347 ) ;
#51278 = CARTESIAN_POINT ( 'NONE',  ( 87.69946696010549658, 45.28426313102758627, -6.325214577564480578 ) ) ;
#51279 = CARTESIAN_POINT ( 'NONE',  ( 88.50303165573761532, 43.87208881218895584, -0.02088647746843486086 ) ) ;
#51280 = CARTESIAN_POINT ( 'NONE',  ( 80.84441418302719740, 43.48202404113703068, 9.388955441769184063 ) ) ;
#51281 = ORIENTED_EDGE ( 'NONE', *, *, #74704, .F. ) ;
#51282 = CARTESIAN_POINT ( 'NONE',  ( 164.3939401533646958, 245.9083385283718712, 2.844462461176849200 ) ) ;
#51283 = CARTESIAN_POINT ( 'NONE',  ( 73.98106629984819449, 60.92745772619367273, 15.22512809013772106 ) ) ;
#51284 = ORIENTED_EDGE ( 'NONE', *, *, #97710, .T. ) ;
#51285 = CARTESIAN_POINT ( 'NONE',  ( 177.8477507594193412, 279.4524148463787583, -16.32274502148586492 ) ) ;
#51286 = CARTESIAN_POINT ( 'NONE',  ( 172.3780232790210789, 263.7810319789855384, -15.48897907228803206 ) ) ;
#51287 = EDGE_LOOP ( 'NONE', ( #71757, #15381, #17372, #66318 ) ) ;
#51288 = CARTESIAN_POINT ( 'NONE',  ( 41.22093855302744458, 25.92755873383628895, 6.180339887498953466 ) ) ;
#51289 = ORIENTED_EDGE ( 'NONE', *, *, #59614, .F. ) ;
#51290 = CARTESIAN_POINT ( 'NONE',  ( 157.6127312046615145, 268.8539850385699879, 15.63345059891010891 ) ) ;
#51291 = ORIENTED_EDGE ( 'NONE', *, *, #71565, .F. ) ;
#51292 = CARTESIAN_POINT ( 'NONE',  ( 156.4161679080374370, 267.1311002716061012, -16.29285210311729060 ) ) ;
#51293 = CARTESIAN_POINT ( 'NONE',  ( 146.8516045228164160, 276.2925551239072774, 3.995954059407343273 ) ) ;
#51294 = DIRECTION ( 'NONE',  ( -0.4813790724697843970, -0.8765125147926470239, 0.000000000000000000 ) ) ;
#51295 = DIRECTION ( 'NONE',  ( -0.3984034379159046013, 0.9172102815912979157, 0.000000000000000000 ) ) ;
#51296 = CARTESIAN_POINT ( 'NONE',  ( 192.1859061758433143, 297.7712413352111298, 11.15082371775444336 ) ) ;
#51297 = CARTESIAN_POINT ( 'NONE',  ( 86.48513059569856409, 43.16329677770136186, 0.5072759017112983271 ) ) ;
#51298 = CARTESIAN_POINT ( 'NONE',  ( 197.0632481487482437, 289.3234372322515924, -16.88857388075149046 ) ) ;
#51299 = ORIENTED_EDGE ( 'NONE', *, *, #42975, .F. ) ;
#51300 = CARTESIAN_POINT ( 'NONE',  ( 76.86804935198983912, 57.06628021550515939, -16.17658353980281305 ) ) ;
#51301 = AXIS2_PLACEMENT_3D ( 'NONE', #30026, #60910, #91877 ) ;
#51302 = CARTESIAN_POINT ( 'NONE',  ( 165.0087721269838710, 244.8434183119457543, 2.604344609212914108 ) ) ;
#51304 = CARTESIAN_POINT ( 'NONE',  ( 164.4573439719129340, 245.7985198932525748, 1.541132361166968501 ) ) ;
#51303 = CARTESIAN_POINT ( 'NONE',  ( 77.40115397588131430, 49.73071544000705302, -15.49217368967964426 ) ) ;
#51306 = ORIENTED_EDGE ( 'NONE', *, *, #62519, .F. ) ;
#51305 = LINE ( 'NONE', #18448, #28281 ) ;
#51307 = CARTESIAN_POINT ( 'NONE',  ( 170.4038350149297685, 287.7086646401646135, 4.116642393818346513 ) ) ;
#51308 = CARTESIAN_POINT ( 'NONE',  ( 49.09245556086620610, 93.56363653685789927, -10.00000000000000000 ) ) ;
#51309 = VECTOR ( 'NONE', #13397, 1000.000000000000000 ) ;
#51310 = VERTEX_POINT ( 'NONE', #98393 ) ;
#51311 = CARTESIAN_POINT ( 'NONE',  ( 71.44228484409906343, 68.27790281458665334, 9.600800115958856296 ) ) ;
#51312 = CARTESIAN_POINT ( 'NONE',  ( 42.72569090598236841, 207.0217562850347690, 4.570193772333722408E-14 ) ) ;
#51313 = CARTESIAN_POINT ( 'NONE',  ( 179.5569193005887030, 256.8711241645506220, 9.238826761386862430 ) ) ;
#51314 = EDGE_CURVE ( 'NONE', #13779, #64640, #17024, .T. ) ;
#51315 = CARTESIAN_POINT ( 'NONE',  ( 198.6322367969459322, 286.6058691770745099, -18.00064234861828538 ) ) ;
#51316 = EDGE_CURVE ( 'NONE', #48457, #75612, #61688, .T. ) ;
#51317 = CARTESIAN_POINT ( 'NONE',  ( 190.5563804489516713, 300.5936626864281607, -0.2587918834769942222 ) ) ;
#51318 = VERTEX_POINT ( 'NONE', #14035 ) ;
#51319 = CARTESIAN_POINT ( 'NONE',  ( 208.1912724900461740, 270.0491336852600170, -0.9856800448607289100 ) ) ;
#51320 = VECTOR ( 'NONE', #78395, 1000.000000000000000 ) ;
#51321 = CARTESIAN_POINT ( 'NONE',  ( 205.5714613402004431, 274.0961078821768524, 10.65137002167587887 ) ) ;
#51322 = CARTESIAN_POINT ( 'NONE',  ( 153.0790963368640689, 265.5062228982576471, -17.74594954892339160 ) ) ;
#51323 = VECTOR ( 'NONE', #37280, 1000.000000000000000 ) ;
#51324 = EDGE_CURVE ( 'NONE', #24132, #56530, #90079, .T. ) ;
#51325 = CARTESIAN_POINT ( 'NONE',  ( 207.6918009085542849, 270.9142438413412037, 7.009114282139513818 ) ) ;
#51326 = ADVANCED_FACE ( 'NONE', ( #82977 ), #66246, .T. ) ;
#51327 = CARTESIAN_POINT ( 'NONE',  ( 40.20209520705726192, 184.0177522451417929, 5.000000000000051514 ) ) ;
#51328 = CARTESIAN_POINT ( 'NONE',  ( 117.0621101165238542, 229.2048013555409796, 4.594050593750051981 ) ) ;
#51329 = CARTESIAN_POINT ( 'NONE',  ( 183.2680676362570296, 295.8844131031794404, -2.692372112000086748 ) ) ;
#51330 = CARTESIAN_POINT ( 'NONE',  ( 165.0908032838305530, 280.5488345782329134, -11.11949073998667892 ) ) ;
#51331 = FACE_OUTER_BOUND ( 'NONE', #70215, .T. ) ;
#51332 = CARTESIAN_POINT ( 'NONE',  ( 162.8491774010308575, 248.5839461010540390, 10.21539626359008146 ) ) ;
#51333 = CARTESIAN_POINT ( 'NONE',  ( 37.03551627836181126, 198.3149278399160664, 9.188101187500093303 ) ) ;
#51334 = CARTESIAN_POINT ( 'NONE',  ( 82.16683981089441602, 40.63021946778572868, 3.442904079118366933 ) ) ;
#51335 = VERTEX_POINT ( 'NONE', #52037 ) ;
#51336 = VECTOR ( 'NONE', #54547, 1000.000000000000114 ) ;
#51337 = ORIENTED_EDGE ( 'NONE', *, *, #33649, .T. ) ;
#51338 = DIRECTION ( 'NONE',  ( -0.000000000000000000, -1.000000000000000000, -0.000000000000000000 ) ) ;
#51339 = CARTESIAN_POINT ( 'NONE',  ( 74.44907505376188794, 68.07791596852769089, -11.61944736710526627 ) ) ;
#51340 = DIRECTION ( 'NONE',  ( -0.000000000000000000, -0.000000000000000000, 1.000000000000000000 ) ) ;
#51341 = B_SPLINE_CURVE_WITH_KNOTS ( 'NONE', 3,
 ( #7382, #60076, #99112, #52000, #82465, #67192, #14000, #43889, #45864, #59070, #52486, #98115 ),
 .UNSPECIFIED., .F., .F.,
 ( 4, 2, 2, 2, 2, 4 ),
 ( 0.002214587119218288519, 0.002343824639362031628, 0.002473062159505774738, 0.002731537199793260522, 0.003248487280368166173, 0.004282387441517975304 ),
 .UNSPECIFIED. ) ;
#51342 = CARTESIAN_POINT ( 'NONE',  ( 76.59722600259529202, 51.27521344558854111, 16.05611726275148854 ) ) ;
#51343 = CARTESIAN_POINT ( 'NONE',  ( 82.01427717811640150, 41.38653749815328098, -5.922201023369847661 ) ) ;
#51344 = DIRECTION ( 'NONE',  ( -0.8660254037844387076, -0.4999999999999998890, -0.000000000000000000 ) ) ;
#51345 =( BOUNDED_CURVE ( )  B_SPLINE_CURVE ( 2, ( #90668, #7002, #98232, #83051, #21225, #60186, #99224 ),
 .UNSPECIFIED., .F., .T. ) 
 B_SPLINE_CURVE_WITH_KNOTS ( ( 3, 2, 2, 3 ),
 ( 0.9875000000000000444, 0.9899999999999999911, 0.9949999999999999956, 1.000000000000000000 ),
 .UNSPECIFIED. ) 
 CURVE ( )  GEOMETRIC_REPRESENTATION_ITEM ( )  RATIONAL_B_SPLINE_CURVE ( ( 0.9755282581475767101, 0.9755282581475772652, 1.000000000000000000, 0.9510565162951535312, 1.000000000000000000, 0.9510565162951535312, 1.000000000000000000 ) ) 
 REPRESENTATION_ITEM ( '' )  );
#51346 = LINE ( 'NONE', #29067, #49842 ) ;
#51347 = CARTESIAN_POINT ( 'NONE',  ( 168.1712790018757460, 251.6228654270802849, 10.65815083953225084 ) ) ;
#51348 = VECTOR ( 'NONE', #18506, 1000.000000000000114 ) ;
#51349 = CARTESIAN_POINT ( 'NONE',  ( 93.96783902534114929, 218.3927522451417929, -10.00000000000009059 ) ) ;
#51350 = ORIENTED_EDGE ( 'NONE', *, *, #14912, .F. ) ;
#51351 = CARTESIAN_POINT ( 'NONE',  ( 78.96380797632824056, 59.43460744216077529, -16.52597720501995937 ) ) ;
#51352 = CARTESIAN_POINT ( 'NONE',  ( 154.9707648754391016, 280.5157924140515320, -2.443790094235759547 ) ) ;
#51353 = CARTESIAN_POINT ( 'NONE',  ( 207.5886452961740076, 271.0929146030698007, -1.661373005306138184 ) ) ;
#51354 = CARTESIAN_POINT ( 'NONE',  ( 16.57566611395445477, 186.5024278399161233, 9.188101187500095079 ) ) ;
#51355 = CARTESIAN_POINT ( 'NONE',  ( 151.3124059063077311, 268.5662204852269497, -14.45542936000225609 ) ) ;
#51356 = CARTESIAN_POINT ( 'NONE',  ( 74.14312167556930433, 66.30466486950707861, 1.224646799147354045E-15 ) ) ;
#51357 = CARTESIAN_POINT ( 'NONE',  ( 71.63950284402343982, 58.95762851674515304, -15.87121227278351299 ) ) ;
#51358 = CARTESIAN_POINT ( 'NONE',  ( 71.94179174019755862, 72.17120852766012717, -1.676876488574577717 ) ) ;
#51359 = CARTESIAN_POINT ( 'NONE',  ( 61.77188751760236585, 194.2202760586659736, -5.415160957724236172E-17 ) ) ;
#51360 = CARTESIAN_POINT ( 'NONE',  ( 164.2647213391612979, 246.1321520798662164, -5.830872732487307530 ) ) ;
#51361 = CARTESIAN_POINT ( 'NONE',  ( 164.3961040135806968, 245.9045906125373904, 7.095190383188031191 ) ) ;
#51362 = CARTESIAN_POINT ( 'NONE',  ( 70.33000752277322931, 70.07220943294167625, 5.706326222802051262 ) ) ;
#51363 = CARTESIAN_POINT ( 'NONE',  ( 66.11301736082367597, 68.60463451963875059, -4.424701819410488568 ) ) ;
#51364 =( BOUNDED_CURVE ( )  B_SPLINE_CURVE ( 2, ( #48347, #80800, #86905, #25548, #11377, #79296, #42227, #9866, #2260, #33142, #56436, #17962, #48858 ),
 .UNSPECIFIED., .F., .T. ) 
 B_SPLINE_CURVE_WITH_KNOTS ( ( 3, 2, 2, 2, 2, 2, 3 ),
 ( 0.08750000000000000833, 0.08999999999999999667, 0.09500000000000000111, 0.1000000000000000056, 0.1049999999999999961, 0.1100000000000000006, 0.1125000000000000028 ),
 .UNSPECIFIED. ) 
 CURVE ( )  GEOMETRIC_REPRESENTATION_ITEM ( )  RATIONAL_B_SPLINE_CURVE ( ( 0.9755282581475768211, 0.9755282581475768211, 1.000000000000000000, 0.9510565162951535312, 1.000000000000000000, 0.9510565162951535312, 1.000000000000000000, 0.9510565162951535312, 1.000000000000000000, 0.9510565162951535312, 1.000000000000000000, 0.9755282581475768211, 0.9755282581475768211 ) ) 
 REPRESENTATION_ITEM ( '' )  );
#51365 = ORIENTED_EDGE ( 'NONE', *, *, #97697, .F. ) ;
#51366 = CARTESIAN_POINT ( 'NONE',  ( 164.4698008747318738, 245.7769439046653019, -6.272955660526681854 ) ) ;
#51367 = CARTESIAN_POINT ( 'NONE',  ( 9.692741923115875124, 169.7365022471902023, -10.00000000000009059 ) ) ;
#51368 = CARTESIAN_POINT ( 'NONE',  ( 201.5036534377215958, 270.3153034880852488, -10.25451236307256409 ) ) ;
#51369 = CARTESIAN_POINT ( 'NONE',  ( 113.7598676209481994, 245.6744531367911293, 4.594050593750047540 ) ) ;
#51370 = CARTESIAN_POINT ( 'NONE',  ( 24.44820476603448611, 26.06628583063842086, -9.188101187500006262 ) ) ;
#51371 = CARTESIAN_POINT ( 'NONE',  ( 164.9718327055057898, 244.9073992667478876, 1.131110055229076039 ) ) ;
#51372 = CARTESIAN_POINT ( 'NONE',  ( 83.81305692926204642, 51.81190264249386956, -14.87427321595085417 ) ) ;
#51373 = CARTESIAN_POINT ( 'NONE',  ( 76.55703705082244426, 63.73850827144991626, 14.88124462962344552 ) ) ;
#51375 = CARTESIAN_POINT ( 'NONE',  ( 189.3632560013180353, 289.9061821024489518, 14.46060578062359880 ) ) ;
#51374 = CARTESIAN_POINT ( 'NONE',  ( 33.47037235539275457, 49.41749479597460493, -10.00000000000000000 ) ) ;
#51376 = CARTESIAN_POINT ( 'NONE',  ( 150.5629864978592707, 269.8642529768378040, -13.73391103862138607 ) ) ;
#51377 = VERTEX_POINT ( 'NONE', #81483 ) ;
#51378 = CARTESIAN_POINT ( 'NONE',  ( 151.4327733764141612, 268.3577379114237829, 14.90862905801242100 ) ) ;
#51379 = CARTESIAN_POINT ( 'NONE',  ( 208.1511065278944557, 270.1187031724418830, -0.2859582466342852625 ) ) ;
#51381 = ADVANCED_FACE ( 'NONE', ( #44425 ), #98661, .F. ) ;
#51380 = AXIS2_PLACEMENT_3D ( 'NONE', #93973, #24526, #71661 ) ;
#51382 = CARTESIAN_POINT ( 'NONE',  ( 151.4581065015725869, 268.7005504512642915, -14.40868859785765999 ) ) ;
#51383 = CARTESIAN_POINT ( 'NONE',  ( 173.0391163831423569, 268.2137988250248668, -16.30552455123574873 ) ) ;
#51384 = CARTESIAN_POINT ( 'NONE',  ( 194.0277586765656963, 270.7140688648943865, -14.04450335696146723 ) ) ;
#51385 = ORIENTED_EDGE ( 'NONE', *, *, #91274, .T. ) ;
#51386 = CARTESIAN_POINT ( 'NONE',  ( 70.86876320951611774, 70.15810021654870354, 6.178032208043940265 ) ) ;
#51387 = VECTOR ( 'NONE', #95182, 1000.000000000000000 ) ;
#51388 = CARTESIAN_POINT ( 'NONE',  ( 85.22997224006158490, 42.06997850247606152, -1.831231488640648664 ) ) ;
#51389 = B_SPLINE_SURFACE_WITH_KNOTS ( 'NONE', 3, 1, ( 
 ( #18788, #49668 ),
 ( #26881, #35466 ),
 ( #28359, #65371 ),
 ( #66370, #44043 ),
 ( #81126, #65859 ),
 ( #50658, #82625 ),
 ( #57760, #43560 ),
 ( #97301, #58749 ),
 ( #96819, #13187 ),
 ( #19307, #88736 ),
 ( #20282, #11693 ),
 ( #74499, #5077 ),
 ( #73002, #80624 ),
 ( #35958, #66860 ),
 ( #3592, #42552 ),
 ( #97789, #90212 ),
 ( #20785, #34000 ),
 ( #27377, #64885 ),
 ( #26384, #84114 ),
 ( #53159, #91693 ),
 ( #7054, #29371 ),
 ( #38442, #61745 ),
 ( #99278, #90720 ),
 ( #83600, #13671 ),
 ( #22256, #22766 ),
 ( #14167, #52645 ),
 ( #29861, #75478 ),
 ( #46033, #5564 ),
 ( #60731, #92212 ),
 ( #45542, #6062 ),
 ( #36956, #69356 ),
 ( #67867, #53643 ),
 ( #59749, #14666 ),
 ( #46538, #84598 ) ),
 .UNSPECIFIED., .T., .F., .F.,
 ( 4, 2, 2, 2, 2, 2, 2, 2, 2, 2, 2, 2, 2, 2, 2, 2, 4 ),
 ( 2, 2 ),
 ( 0.000000000000000000, 0.06250000000000000000, 0.1250000000000000000, 0.1875000000000000000, 0.2500000000000000000, 0.3125000000000000000, 0.3750000000000000000, 0.4375000000000000000, 0.5000000000000000000, 0.5625000000000000000, 0.6250000000000000000, 0.6875000000000000000, 0.7500000000000000000, 0.8125000000000000000, 0.8750000000000000000, 0.9375000000000000000, 1.000000000000000000 ),
 ( 0.000000000000000000, 1.000000000000000000 ),
 .UNSPECIFIED. ) ;
#51390 = CARTESIAN_POINT ( 'NONE',  ( 85.92346940974357494, 46.00060071795214611, 9.032556752206142292 ) ) ;
#51391 = CARTESIAN_POINT ( 'NONE',  ( 196.2821550604401466, 270.8744879265028658, 12.03960231697079664 ) ) ;
#51393 = CARTESIAN_POINT ( 'NONE',  ( 185.6230494993405671, 297.1728990862582691, 5.637358840499950396 ) ) ;
#51392 = B_SPLINE_CURVE_WITH_KNOTS ( 'NONE', 3,
 ( #59790, #74535, #45580, #35994, #29895, #60768, #13226, #14205, #53196, #84151, #5605, #14697, #29407, #75515, #98324, #28397, #67399, #44581, #90254, #60276, #52683, #4614, #66409, #97335, #99809, #70903, #39968, #54168, #55174, #1511, #94232, #85134, #24783, #998, #47087, #69885, #61286, #77514, #15683, #84632, #23279, #86158, #8599, #31878, #16692, #46576, #70389, #86652, #8105, #30894 ),
 .UNSPECIFIED., .F., .F.,
 ( 4, 2, 2, 2, 2, 2, 2, 2, 2, 2, 2, 2, 2, 2, 2, 2, 2, 2, 2, 2, 2, 2, 2, 2, 4 ),
 ( 0.0001611619350887445517, 0.001178274281826848739, 0.001686830455195882997, 0.001813969498538121287, 0.001941108541880359577, 0.002068247585222597433, 0.002195386628564835723, 0.002449664715249311436, 0.002703942801933786715, 0.003212498975302860871, 0.004229611322040959312, 0.005246723668779058186, 0.005755279842148062520, 0.006009557928832644919, 0.006263836015517227317, 0.006327405537188392215, 0.006390975058859557113, 0.006454544580530722012, 0.006518114102201886910, 0.006772392188886545636, 0.007280948362255976712, 0.007535226448940692684, 0.007789504535625407788, 0.008043782622310124628, 0.008298060708994839732 ),
 .UNSPECIFIED. ) ;
#51394 = CARTESIAN_POINT ( 'NONE',  ( 208.1303168694798273, 270.1547119170880364, -0.9257663487928086132 ) ) ;
#51395 = DIRECTION ( 'NONE',  ( -1.000000000000000000, 0.000000000000000000, 0.000000000000000000 ) ) ;
#51396 = MECHANICAL_DESIGN_GEOMETRIC_PRESENTATION_REPRESENTATION (  '', ( #70786 ), #19036 ) ;
#51397 = ORIENTED_EDGE ( 'NONE', *, *, #82460, .F. ) ;
#51398 = DIRECTION ( 'NONE',  ( 0.000000000000000000, 0.000000000000000000, 1.000000000000000000 ) ) ;
#51399 = CARTESIAN_POINT ( 'NONE',  ( 8.916318567990060728, 28.08080186712591342, -3.090169943749475845 ) ) ;
#51400 = LINE ( 'NONE', #7288, #66014 ) ;
#51401 = ORIENTED_EDGE ( 'NONE', *, *, #58928, .T. ) ;
#51402 = FACE_OUTER_BOUND ( 'NONE', #972, .T. ) ;
#51403 = ADVANCED_FACE ( 'NONE', ( #12555 ), #98156, .F. ) ;
#51404 = PLANE ( 'NONE',  #72612 ) ;
#51405 = ORIENTED_EDGE ( 'NONE', *, *, #88562, .T. ) ;
#51406 = CARTESIAN_POINT ( 'NONE',  ( 147.2999496562918296, 275.5159985734018164, -0.1418322875769767455 ) ) ;
#51407 = CARTESIAN_POINT ( 'NONE',  ( 204.7070208051621876, 272.9836748357583360, -9.755963162871239547 ) ) ;
#51408 = AXIS2_PLACEMENT_3D ( 'NONE', #44034, #52144, #83093 ) ;
#51409 = CARTESIAN_POINT ( 'NONE',  ( 204.5831314780710954, 276.2986172388744421, 13.28075685133257089 ) ) ;
#51410 = LINE ( 'NONE', #90469, #36625 ) ;
#51411 = ORIENTED_EDGE ( 'NONE', *, *, #96924, .T. ) ;
#51412 = CARTESIAN_POINT ( 'NONE',  ( 88.29356841273579448, 221.7833772461660544, -9.188101187500095079 ) ) ;
#51413 = LINE ( 'NONE', #21042, #9607 ) ;
#51414 = VECTOR ( 'NONE', #47181, 1000.000000000000000 ) ;
#51415 = LINE ( 'NONE', #42797, #69055 ) ;
#51416 = CARTESIAN_POINT ( 'NONE',  ( 178.8786591484599455, 269.4121626077708243, -17.24761370402104177 ) ) ;
#51417 = CARTESIAN_POINT ( 'NONE',  ( 81.20875893632040743, 42.29378956363321862, -7.416406876933310244 ) ) ;
#51418 = ORIENTED_EDGE ( 'NONE', *, *, #82817, .F. ) ;
#51419 = ORIENTED_EDGE ( 'NONE', *, *, #62203, .T. ) ;
#51420 = CARTESIAN_POINT ( 'NONE',  ( 88.37416949021037738, 43.79857776338975839, 0.1607882160166531627 ) ) ;
#51421 = VERTEX_POINT ( 'NONE', #32217 ) ;
#51422 = CARTESIAN_POINT ( 'NONE',  ( 193.6538297768585153, 294.3106073703939387, 13.99927879369582406 ) ) ;
#51423 = ORIENTED_EDGE ( 'NONE', *, *, #26875, .F. ) ;
#51424 = CARTESIAN_POINT ( 'NONE',  ( 159.1608936441631670, 258.2911997636435899, 17.40761412644028994 ) ) ;
#51425 = CARTESIAN_POINT ( 'NONE',  ( 202.8549823380854491, 279.2918593523859272, -16.39745931995414807 ) ) ;
#51426 = ORIENTED_EDGE ( 'NONE', *, *, #92487, .F. ) ;
#51427 = CARTESIAN_POINT ( 'NONE',  ( 206.9008466447795627, 272.2842168126622369, -7.000122840392532630 ) ) ;
#51428 = AXIS2_PLACEMENT_3D ( 'NONE', #7489, #38382, #85031 ) ;
#51429 = LINE ( 'NONE', #220, #87061 ) ;
#51430 = DIRECTION ( 'NONE',  ( 0.4458072818673325943, 0.8951289669282637140, 0.000000000000000000 ) ) ;
#51431 = CARTESIAN_POINT ( 'NONE',  ( 194.6356465353167948, 293.5281665672507643, -16.13180903283129197 ) ) ;
#51432 = CARTESIAN_POINT ( 'NONE',  ( 72.34345819658318533, 68.24918517509843241, -10.24609853730615328 ) ) ;
#51433 = CARTESIAN_POINT ( 'NONE',  ( 164.8232333123806654, 265.1872998416218934, -16.61854591372365419 ) ) ;
#51434 = VERTEX_POINT ( 'NONE', #7939 ) ;
#51435 = CARTESIAN_POINT ( 'NONE',  ( 77.01662391835196786, 61.79474988883485764, 15.54209892090687362 ) ) ;
#51436 = CARTESIAN_POINT ( 'NONE',  ( 14.11662529016922640, 10.01110640527290663, 2.839279412974134775 ) ) ;
#51437 = ORIENTED_EDGE ( 'NONE', *, *, #90256, .T. ) ;
#51438 = CARTESIAN_POINT ( 'NONE',  ( 167.1384944754526032, 284.3002062084726731, 9.379343144590123416 ) ) ;
#51440 = ORIENTED_EDGE ( 'NONE', *, *, #77637, .T. ) ;
#51439 = CARTESIAN_POINT ( 'NONE',  ( 199.9340980646776700, 270.2282918247154839, 9.381492668529142875 ) ) ;
#51441 = CARTESIAN_POINT ( 'NONE',  ( -13.87263394856965704, 104.4305210064043052, 10.52386804011639221 ) ) ;
#51442 = CARTESIAN_POINT ( 'NONE',  ( -9.181706736895311138, 177.0530062829863027, -4.648177544792955347E-16 ) ) ;
#51443 = CARTESIAN_POINT ( 'NONE',  ( 170.9564544596932194, 287.9465792427529323, -5.428517921301809324 ) ) ;
#51444 = CARTESIAN_POINT ( 'NONE',  ( 149.1928685617267831, 276.2413934580336559, -5.465481129197618415 ) ) ;
#51445 = CARTESIAN_POINT ( 'NONE',  ( 82.21190057601546641, 49.98264421458685547, -14.46497528049439474 ) ) ;
#51446 = CARTESIAN_POINT ( 'NONE',  ( 192.8028085474765021, 292.0655250527965450, -15.27648668737578141 ) ) ;
#51447 = CARTESIAN_POINT ( 'NONE',  ( 84.46833194923661381, 42.11454976261988037, 1.216645073941585720 ) ) ;
#51448 = CARTESIAN_POINT ( 'NONE',  ( 88.36865033182888851, 43.96674011622069855, -2.220889795100837283 ) ) ;
#51449 = ORIENTED_EDGE ( 'NONE', *, *, #10130, .F. ) ;
#51450 = CARTESIAN_POINT ( 'NONE',  ( 182.0923320409109465, 271.6029700406237453, -15.99347964086035567 ) ) ;
#51451 = CARTESIAN_POINT ( 'NONE',  ( 76.74769370342797004, 61.59959995924427290, -15.56961045695145351 ) ) ;
#51452 = VERTEX_POINT ( 'NONE', #83976 ) ;
#51453 = AXIS2_PLACEMENT_3D ( 'NONE', #4274, #97030, #69058 ) ;
#51454 = CARTESIAN_POINT ( 'NONE',  ( 160.5373035959516415, 275.8859140749689232, 12.69512463838454508 ) ) ;
#51455 = ADVANCED_FACE ( 'NONE', ( #23109 ), #46922, .F. ) ;
#51456 = CARTESIAN_POINT ( 'NONE',  ( 190.8252190424821890, 261.7436831218522002, 6.354606126879223105 ) ) ;
#51457 = CARTESIAN_POINT ( 'NONE',  ( 204.1742785453265299, 277.0067712912111233, -14.60822391153214461 ) ) ;
#51458 = LINE ( 'NONE', #42351, #65648 ) ;
#51459 = AXIS2_PLACEMENT_3D ( 'NONE', #44222, #7222, #31021 ) ;
#51460 = CARTESIAN_POINT ( 'NONE',  ( 160.8117895914568010, 272.6511186442759822, 15.47829891388946244 ) ) ;
#51462 = CARTESIAN_POINT ( 'NONE',  ( 88.05378287308985819, 43.82556038557744671, 2.467578420128283767 ) ) ;
#51461 = CARTESIAN_POINT ( 'NONE',  ( -13.87062626178347813, 171.9869531367911293, 4.594050593750046652 ) ) ;
#51463 = CARTESIAN_POINT ( 'NONE',  ( 200.2706162234322562, 268.0192582847963081, 6.103686053348833518 ) ) ;
#51464 = EDGE_LOOP ( 'NONE', ( #70076, #48433, #56740, #87174 ) ) ;
#51465 = CIRCLE ( 'NONE', #61210, 17.82106496071138935 ) ;
#51466 = EDGE_LOOP ( 'NONE', ( #65823, #63855, #94439, #2457 ) ) ;
#51467 = LINE ( 'NONE', #37743, #48426 ) ;
#51468 = CARTESIAN_POINT ( 'NONE',  ( 185.2570508126727873, 282.0811717828997303, -17.42469797758589678 ) ) ;
#51469 = CARTESIAN_POINT ( 'NONE',  ( 85.49318370521093868, 48.99722645306705715, -12.73116331006621493 ) ) ;
#51470 = CARTESIAN_POINT ( 'NONE',  ( 171.7460074610065135, 289.4413739377905017, 2.655714547348211330 ) ) ;
#51471 = CARTESIAN_POINT ( 'NONE',  ( 153.4477557824949940, 264.8676860077344486, 17.16010094972647693 ) ) ;
#51472 = AXIS2_PLACEMENT_3D ( 'NONE', #73425, #71930, #2534 ) ;
#51473 = DIRECTION ( 'NONE',  ( -0.000000000000000000, -1.000000000000000000, -0.000000000000000000 ) ) ;
#51474 = CARTESIAN_POINT ( 'NONE',  ( 42.52953848327577191, 205.3615022471903160, 5.000000000000046185 ) ) ;
#51475 = CARTESIAN_POINT ( 'NONE',  ( -0.04102277327696322862, 170.7833772461660828, -9.188101187500095079 ) ) ;
#51476 = CARTESIAN_POINT ( 'NONE',  ( 105.1271107466783121, 225.3768266524159856, 9.188101187500098632 ) ) ;
#51477 = CARTESIAN_POINT ( 'NONE',  ( 79.57426776854913442, 46.24084366570346560, -13.18946159588284139 ) ) ;
#51478 = CARTESIAN_POINT ( 'NONE',  ( 180.0732687355215944, 254.9075906842349752, -2.440557160824225136 ) ) ;
#51479 = CARTESIAN_POINT ( 'NONE',  ( 77.87326056917984829, 50.90737332642450497, 15.27958365935661611 ) ) ;
#51480 = VECTOR ( 'NONE', #84551, 1000.000000000000000 ) ;
#51481 = CARTESIAN_POINT ( 'NONE',  ( 80.14583156672975406, 53.55993809145104478, -15.68071144708088660 ) ) ;
#51482 = DIRECTION ( 'NONE',  ( 0.5840252505817197237, 0.000000000000000000, -0.8117354905897360418 ) ) ;
#51483 = CARTESIAN_POINT ( 'NONE',  ( 30.34687108590969373, 93.06504152958497400, 60.00000000000000000 ) ) ;
#51484 = CARTESIAN_POINT ( 'NONE',  ( 194.6356465353167948, 293.5281665672507643, -16.13180903283129197 ) ) ;
#51485 = CARTESIAN_POINT ( 'NONE',  ( -69.42519150082246426, 45.64199051378594874, -10.00000000000000000 ) ) ;
#51486 = CARTESIAN_POINT ( 'NONE',  ( 195.3144667888438164, 266.4868967755442100, 7.916038506172456302 ) ) ;
#51487 = CARTESIAN_POINT ( 'NONE',  ( 55.65629887206635829, 191.3932355074535678, -2.679491924311248496 ) ) ;
#51488 = CARTESIAN_POINT ( 'NONE',  ( 163.3712170204604774, 252.4875253277900526, -12.92986515194776587 ) ) ;
#51489 = FACE_OUTER_BOUND ( 'NONE', #2231, .T. ) ;
#51490 = AXIS2_PLACEMENT_3D ( 'NONE', #90069, #74363, #59602 ) ;
#51491 = CARTESIAN_POINT ( 'NONE',  ( 172.5050055919510328, 263.7176657671190583, -15.44007813853843736 ) ) ;
#51492 = CARTESIAN_POINT ( 'NONE',  ( 81.79837788435251866, 218.0333772461660544, 9.188101187500095079 ) ) ;
#51493 = CARTESIAN_POINT ( 'NONE',  ( 4.600586583810874153, 20.84336893147753500, -7.433330006724137462 ) ) ;
#51494 = CARTESIAN_POINT ( 'NONE',  ( 190.8001679306945277, 300.1714103817999444, 7.815449226872675403 ) ) ;
#51495 = CARTESIAN_POINT ( 'NONE',  ( 33.63888670793727442, 47.67824751478843126, 10.00000000000000000 ) ) ;
#51497 = CARTESIAN_POINT ( 'NONE',  ( 200.3816788769131279, 283.5757466096723078, 17.26062989396512393 ) ) ;
#51496 = CARTESIAN_POINT ( 'NONE',  ( 195.7291850945597957, 291.6341022226063160, 17.08310330964873813 ) ) ;
#51498 = CARTESIAN_POINT ( 'NONE',  ( 196.4758289992203117, 290.3408770445727782, 16.47704128718402572 ) ) ;
#51499 = CARTESIAN_POINT ( 'NONE',  ( 75.91719666336339856, 65.48793379249461566, 14.32281418338180856 ) ) ;
#51500 = CARTESIAN_POINT ( 'NONE',  ( 204.5203606882526230, 276.0073328462628979, -12.85725516468893836 ) ) ;
#51502 = EDGE_CURVE ( 'NONE', #20047, #7177, #42154, .T. ) ;
#51501 = VECTOR ( 'NONE', #36516, 1000.000000000000000 ) ;
#51503 = CARTESIAN_POINT ( 'NONE',  ( 40.59535201087842182, 25.29860640527295601, -2.839279412974138328 ) ) ;
#51504 = CARTESIAN_POINT ( 'NONE',  ( 147.1034852426517148, 275.8562849197056153, -3.648177088342072327 ) ) ;
#51505 = DIRECTION ( 'NONE',  ( 0.000000000000000000, 0.6050222638427527055, 0.7962085532412914723 ) ) ;
#51506 = ORIENTED_EDGE ( 'NONE', *, *, #60318, .T. ) ;
#51507 = CARTESIAN_POINT ( 'NONE',  ( 23.58217936225004863, 25.56628583063841376, 9.188101187500006262 ) ) ;
#51508 = CARTESIAN_POINT ( 'NONE',  ( 6.430760413625676186, 27.21091486745858390, -1.111400068045478839E-16 ) ) ;
#51509 = CARTESIAN_POINT ( 'NONE',  ( 192.6170194583582429, 297.0245312260774995, -11.90166228306590490 ) ) ;
#51510 = CARTESIAN_POINT ( 'NONE',  ( 187.9734438986738780, 286.0035705317766315, -16.48521393606941743 ) ) ;
#51511 = VERTEX_POINT ( 'NONE', #820 ) ;
#51512 = CARTESIAN_POINT ( 'NONE',  ( 70.83041700687917341, 60.97177786998932447, 15.04209849889492823 ) ) ;
#51513 = CARTESIAN_POINT ( 'NONE',  ( 198.2040940955416488, 287.3474340887963763, 16.95806375232200480 ) ) ;
#51515 = ADVANCED_FACE ( 'NONE', ( #47413 ), #53517, .F. ) ;
#51514 = CARTESIAN_POINT ( 'NONE',  ( 157.0099022660245112, 268.5004079842800593, 15.67285573416865674 ) ) ;
#51516 = CARTESIAN_POINT ( 'NONE',  ( 189.6957203118188318, 279.0266125994497202, 17.78851986857808853 ) ) ;
#51517 = CARTESIAN_POINT ( 'NONE',  ( 87.40678246761487458, 44.84425702272720571, -6.651126967624185760 ) ) ;
#51518 = CARTESIAN_POINT ( 'NONE',  ( 136.9984762794283881, 243.2365022471902023, -10.00000000000009059 ) ) ;
#51519 = CARTESIAN_POINT ( 'NONE',  ( 70.02414138031360835, 62.78214778883172187, 13.38063900663788885 ) ) ;
#51520 = EDGE_LOOP ( 'NONE', ( #3630, #29238, #10404, #88959 ) ) ;
#51521 = CARTESIAN_POINT ( 'NONE',  ( 86.81641918289878390, 45.77657501471897916, -8.750901752256119437 ) ) ;
#51522 = VECTOR ( 'NONE', #69995, 1000.000000000000227 ) ;
#51523 = ORIENTED_EDGE ( 'NONE', *, *, #50830, .T. ) ;
#51524 = DIRECTION ( 'NONE',  ( 0.3940053768033583426, -0.6824373310787393843, 0.6156614753256619554 ) ) ;
#51525 = CARTESIAN_POINT ( 'NONE',  ( 82.97960392506115568, 41.21894294556930305, 0.3178262756287024704 ) ) ;
#51526 = EDGE_CURVE ( 'NONE', #56977, #16138, #76822, .T. ) ;
#51527 = EDGE_LOOP ( 'NONE', ( #26171, #67495, #83165, #4794 ) ) ;
#51528 = CARTESIAN_POINT ( 'NONE',  ( -22.42236680055709641, 157.8615022471902591, 0.000000000000000000 ) ) ;
#51529 = EDGE_LOOP ( 'NONE', ( #54009, #49545, #80400, #65485 ) ) ;
#51530 = AXIS2_PLACEMENT_3D ( 'NONE', #40025, #32451, #39520 ) ;
#51531 = CARTESIAN_POINT ( 'NONE',  ( 49.45774171355136417, 189.3615022471902023, 5.000000000000051514 ) ) ;
#51532 = CARTESIAN_POINT ( 'NONE',  ( 205.6353699412782703, 274.4760867589209852, 10.94919351699760668 ) ) ;
#51533 = CARTESIAN_POINT ( 'NONE',  ( 194.1209507349113039, 280.7511396460085962, -17.56060529715742291 ) ) ;
#51534 = CARTESIAN_POINT ( 'NONE',  ( 204.1149192591630026, 272.7050794302332406, 11.20582280168199318 ) ) ;
#51535 = CARTESIAN_POINT ( 'NONE',  ( 201.3715986869907510, 281.8611552031986776, -17.89433714524984964 ) ) ;
#51536 = VECTOR ( 'NONE', #58524, 1000.000000000000000 ) ;
#51537 = VECTOR ( 'NONE', #54489, 1000.000000000000000 ) ;
#51538 = CARTESIAN_POINT ( 'NONE',  ( 33.58239374649102871, 42.49540643055190259, 3.479690158560446702E-15 ) ) ;
#51539 = FACE_OUTER_BOUND ( 'NONE', #58848, .T. ) ;
#51540 = CARTESIAN_POINT ( 'NONE',  ( 165.9163065983553906, 275.1867875828022534, 14.76689463513480938 ) ) ;
#51541 = CARTESIAN_POINT ( 'NONE',  ( 63.31414817410230000, 217.3615022471903160, 5.000000000000046185 ) ) ;
#51542 = ORIENTED_EDGE ( 'NONE', *, *, #88908, .T. ) ;
#51543 = ORIENTED_EDGE ( 'NONE', *, *, #26638, .F. ) ;
#51544 = CARTESIAN_POINT ( 'NONE',  ( 178.0285553443036974, 273.4130338747266933, 17.82266553853486712 ) ) ;
#51545 = VECTOR ( 'NONE', #99869, 1000.000000000000114 ) ;
#51547 = DIRECTION ( 'NONE',  ( -0.000000000000000000, -0.000000000000000000, -1.000000000000000000 ) ) ;
#51546 = CARTESIAN_POINT ( 'NONE',  ( 204.9780665305064531, 275.6145696623662502, 14.10615427165218883 ) ) ;
#51548 = CARTESIAN_POINT ( 'NONE',  ( 85.30407614177579489, 48.45294084599412088, 12.40582119231524949 ) ) ;
#51549 = DIRECTION ( 'NONE',  ( -0.9954322480537365347, -0.09547062131715938760, 0.000000000000000000 ) ) ;
#51550 = CARTESIAN_POINT ( 'NONE',  ( 72.57276282155493163, 61.54530475149964985, -14.72551858661936031 ) ) ;
#51551 = CARTESIAN_POINT ( 'NONE',  ( 82.38478773084463569, 40.37679422933422302, 1.032346012429565807 ) ) ;
#51552 = CARTESIAN_POINT ( 'NONE',  ( 167.0998337208708904, 286.2756947182164708, -4.828926102446922108 ) ) ;
#51553 = CARTESIAN_POINT ( 'NONE',  ( 76.91165928263828278, 63.32913628365751180, -15.47028109333149715 ) ) ;
#51554 = CARTESIAN_POINT ( 'NONE',  ( 78.92848498041493599, 59.73641368792644357, 16.49589861780994227 ) ) ;
#51555 = CARTESIAN_POINT ( 'NONE',  ( 88.50972766791686297, 234.1589784336661637, -6.496448406907675876E-16 ) ) ;
#51556 = ORIENTED_EDGE ( 'NONE', *, *, #61708, .F. ) ;
#51557 = DIRECTION ( 'NONE',  ( 0.000000000000000000, 0.000000000000000000, 1.000000000000000000 ) ) ;
#51558 = CARTESIAN_POINT ( 'NONE',  ( 165.4582102121029550, 271.3011006785229711, 17.16042223052847859 ) ) ;
#51559 = CARTESIAN_POINT ( 'NONE',  ( 165.4201252317303101, 277.4485869903318189, -13.43193553334254808 ) ) ;
#51560 = ORIENTED_EDGE ( 'NONE', *, *, #70067, .T. ) ;
#51561 = AXIS2_PLACEMENT_3D ( 'NONE', #45600, #91753, #22316 ) ;
#51562 = ORIENTED_EDGE ( 'NONE', *, *, #38452, .T. ) ;
#51563 = EDGE_CURVE ( 'NONE', #5854, #56559, #63619, .T. ) ;
#51564 = CARTESIAN_POINT ( 'NONE',  ( 87.00169912441755571, 45.80253757415765392, -8.636720921146656238 ) ) ;
#51565 = EDGE_CURVE ( 'NONE', #64000, #38047, #41303, .T. ) ;
#51566 = CARTESIAN_POINT ( 'NONE',  ( 71.41016749218992743, 59.45273978182970609, 15.19346469599747174 ) ) ;
#51567 = CARTESIAN_POINT ( 'NONE',  ( 164.3163527186429178, 249.7635482851873974, 9.980485951392335409 ) ) ;
#51568 = LINE ( 'NONE', #21670, #41922 ) ;
#51569 = PLANE ( 'NONE',  #64150 ) ;
#51570 = ORIENTED_EDGE ( 'NONE', *, *, #73902, .T. ) ;
#51571 = EDGE_CURVE ( 'NONE', #74292, #34443, #49921, .T. ) ;
#51572 = ORIENTED_EDGE ( 'NONE', *, *, #83461, .F. ) ;
#51573 = B_SPLINE_CURVE_WITH_KNOTS ( 'NONE', 3,
 ( #413, #30816, #38397, #62190, #24704, #8517, #31792, #39386, #55096, #40390, #86083, #16605, #39882, #70818, #32307 ),
 .UNSPECIFIED., .F., .F.,
 ( 4, 2, 2, 2, 1, 2, 2, 4 ),
 ( 0.02192660554268253612, 0.1441857798498459853, 0.2664449541570094726, 0.5109633027713375020, 0.6332224770785018775, 0.6943520642320850644, 0.7554816513856682514, 1.000000000000000000 ),
 .UNSPECIFIED. ) ;
#51574 = CARTESIAN_POINT ( 'NONE',  ( 162.7738416911812180, 248.7144313781379310, -11.09964294874192525 ) ) ;
#51575 = VERTEX_POINT ( 'NONE', #25634 ) ;
#51576 = ADVANCED_FACE ( 'NONE', ( #34225 ), #47902, .T. ) ;
#51577 = CARTESIAN_POINT ( 'NONE',  ( 192.7686961758011250, 263.9209412561240811, -8.347089341778378468 ) ) ;
#51578 = CARTESIAN_POINT ( 'NONE',  ( 13.06432082636536762, 189.8967562850346837, -4.648177544792955347E-16 ) ) ;
#51579 = CARTESIAN_POINT ( 'NONE',  ( 84.10316667629699339, 50.25482096114932773, 13.62407874060527213 ) ) ;
#51581 = CARTESIAN_POINT ( 'NONE',  ( 69.60117505803954430, 62.41877665539861653, -13.45126974014724475 ) ) ;
#51580 = CARTESIAN_POINT ( 'NONE',  ( 138.6312950077063135, 250.8458772461660260, 9.188101187500095079 ) ) ;
#51582 = CARTESIAN_POINT ( 'NONE',  ( 32.30839531297598910, 123.0650415295850593, 25.00000000000000000 ) ) ;
#51583 = ORIENTED_EDGE ( 'NONE', *, *, #80026, .F. ) ;
#51584 = PLANE ( 'NONE',  #54540 ) ;
#51585 = ADVANCED_FACE ( 'NONE', ( #55993 ), #63121, .T. ) ;
#51586 = CARTESIAN_POINT ( 'NONE',  ( 82.60448357664856189, 52.47690334010501800, 14.99630412890038933 ) ) ;
#51587 = CARTESIAN_POINT ( 'NONE',  ( 82.22603995272856992, 41.23397994388041354, -3.464870737315245641 ) ) ;
#51588 = ADVANCED_FACE ( 'NONE', ( #40301 ), #11936, .T. ) ;
#51589 = CARTESIAN_POINT ( 'NONE',  ( 173.0281810805265081, 251.5097863470425068, -0.2592435778029959503 ) ) ;
#51590 = CARTESIAN_POINT ( 'NONE',  ( 33.84893051719189572, 201.8967562850347122, -4.648177544792955347E-16 ) ) ;
#51591 = CARTESIAN_POINT ( 'NONE',  ( 71.86232962023154869, 72.24313703945740883, 3.263832247265275210 ) ) ;
#51592 = CARTESIAN_POINT ( 'NONE',  ( 198.9203168616069206, 282.2040875469349999, -16.77493235761543744 ) ) ;
#51593 = DIRECTION ( 'NONE',  ( -0.6625377181876236365, -0.7490285521785782219, 0.000000000000000000 ) ) ;
#51594 = CARTESIAN_POINT ( 'NONE',  ( 80.71439172754905655, 53.75030299096716391, 15.68586089724884047 ) ) ;
#51595 = CARTESIAN_POINT ( 'NONE',  ( 168.5910505471324257, 286.4687829538495976, 8.106709794022206594 ) ) ;
#51596 = VECTOR ( 'NONE', #23025, 1000.000000000000114 ) ;
#51597 = CARTESIAN_POINT ( 'NONE',  ( 64.07166007881600933, 216.9869531367911293, 4.594050593750046652 ) ) ;
#51598 = FACE_OUTER_BOUND ( 'NONE', #82244, .T. ) ;
#51599 = CARTESIAN_POINT ( 'NONE',  ( 77.69476712368373228, 61.97275371516123244, 15.64124197209477707 ) ) ;
#51600 = CARTESIAN_POINT ( 'NONE',  ( 184.1240780222136095, 289.0015729834078684, -14.54488561116068901 ) ) ;
#51602 = CARTESIAN_POINT ( 'NONE',  ( 71.47384123275855927, 72.35069954344790233, 1.100233114707630300 ) ) ;
#51601 = CIRCLE ( 'NONE', #4670, 70.00000000000001421 ) ;
#51603 = AXIS2_PLACEMENT_3D ( 'NONE', #95754, #18708, #65782 ) ;
#51604 = AXIS2_PLACEMENT_3D ( 'NONE', #58553, #12486, #92484 ) ;
#51605 = FACE_OUTER_BOUND ( 'NONE', #77848, .T. ) ;
#51606 = CARTESIAN_POINT ( 'NONE',  ( -10.10185872486829517, 176.5217562850347974, 2.586156800657061008E-14 ) ) ;
#51607 = CARTESIAN_POINT ( 'NONE',  ( 16.16012747849099540, 9.734156793818206310, 1.333680081654574804E-15 ) ) ;
#51608 = CARTESIAN_POINT ( 'NONE',  ( 190.4234964968757424, 262.2385936383186049, -7.810700279455712547 ) ) ;
#51609 = DIRECTION ( 'NONE',  ( 0.000000000000000000, 0.5906904945688776776, -0.8068982213550696114 ) ) ;
#51610 = FACE_OUTER_BOUND ( 'NONE', #83492, .T. ) ;
#51611 = CARTESIAN_POINT ( 'NONE',  ( 72.12859001842100781, 72.20979474176914437, 3.988024951247655991 ) ) ;
#51612 = VECTOR ( 'NONE', #90818, 1000.000000000000000 ) ;
#51613 = CARTESIAN_POINT ( 'NONE',  ( 16.49491010205593255, 171.1423013555409796, -4.594050593750043987 ) ) ;
#51614 = CARTESIAN_POINT ( 'NONE',  ( 71.01399855574825892, 72.00622678233665397, 1.913033562013090272 ) ) ;
#51615 = VERTEX_POINT ( 'NONE', #12432 ) ;
#51616 = CARTESIAN_POINT ( 'NONE',  ( 186.2134270706513632, 260.6652835500024707, -9.163389403908340114 ) ) ;
#51617 = CARTESIAN_POINT ( 'NONE',  ( 199.5045416813903785, 277.5812092268299693, 15.20258081764992220 ) ) ;
#51618 = FACE_OUTER_BOUND ( 'NONE', #15001, .T. ) ;
#51619 = CARTESIAN_POINT ( 'NONE',  ( 164.0854748117396582, 246.4426161724408928, -5.757837433625331514 ) ) ;
#51620 = CARTESIAN_POINT ( 'NONE',  ( 71.66369827319218189, 72.02185750324218816, -1.551229696566575056 ) ) ;
#51621 = CARTESIAN_POINT ( 'NONE',  ( 48.48320281069610616, 207.9869531367911009, 4.594050593750046652 ) ) ;
#51622 = VECTOR ( 'NONE', #74828, 999.9999999999998863 ) ;
#51623 = EDGE_CURVE ( 'NONE', #50345, #12913, #89422, .T. ) ;
#51624 = CARTESIAN_POINT ( 'NONE',  ( 87.34667321826604791, 45.97495992385612595, 8.598559468654661586 ) ) ;
#51625 = CARTESIAN_POINT ( 'NONE',  ( 156.6812872898450735, 261.2670451491295012, 0.000000000000000000 ) ) ;
#51626 = CARTESIAN_POINT ( 'NONE',  ( 146.7879906441258129, 276.4027375938661635, 4.347255311287614887 ) ) ;
#51627 = CARTESIAN_POINT ( 'NONE',  ( 6.852252633650415703, 22.14336893147753571, 7.433330006724141015 ) ) ;
#51628 = CARTESIAN_POINT ( 'NONE',  ( 202.9355525415089687, 270.0989142730967387, -6.790151509681939146 ) ) ;
#51629 = CARTESIAN_POINT ( 'NONE',  ( 176.9907319409991544, 291.8589342268469977, 2.570357995431835185 ) ) ;
#51630 = CARTESIAN_POINT ( 'NONE',  ( 179.7109432054668332, 276.7948752059230060, 16.30604964765089093 ) ) ;
#51631 = CARTESIAN_POINT ( 'NONE',  ( 73.25272225934853054, 63.87170619894617829, 13.86221949118336916 ) ) ;
#51632 = CARTESIAN_POINT ( 'NONE',  ( 73.77985862123976801, 67.40099183159448160, -11.80460429102062925 ) ) ;
#51633 = B_SPLINE_SURFACE_WITH_KNOTS ( 'NONE', 3, 1, ( 
 ( #52624, #28851 ),
 ( #53136, #98261 ),
 ( #45524, #76455 ),
 ( #29841, #75973 ),
 ( #68827, #38422 ),
 ( #60215, #84580 ),
 ( #82600, #74962 ),
 ( #13166, #61227 ),
 ( #5545, #92192 ),
 ( #14143, #59730 ),
 ( #36430, #22745 ),
 ( #52132, #53624 ),
 ( #37423, #67337 ),
 ( #21253, #83082 ),
 ( #13652, #15119 ),
 ( #46013, #69337 ),
 ( #76929, #44524 ),
 ( #75455, #68331 ),
 ( #60711, #6040 ),
 ( #100258, #91179 ),
 ( #36936, #61726 ),
 ( #67848, #98769 ),
 ( #83582, #6549 ),
 ( #99256, #45031 ),
 ( #85074, #93170 ),
 ( #63238, #9041 ),
 ( #69831, #10050 ),
 ( #16139, #94180 ),
 ( #17133, #46520 ),
 ( #77457, #47037 ),
 ( #944, #40423 ) ),
 .UNSPECIFIED., .F., .F., .F.,
 ( 4, 3, 3, 3, 3, 3, 3, 3, 3, 3, 4 ),
 ( 2, 2 ),
 ( 0.000000000000000000, 0.1122669598086646486, 0.2243161639709420618, 0.3396355846219054064, 0.4553962076585019170, 0.5677860799922325175, 0.6749047109689453317, 0.7773884377078321695, 0.8775581155834190072, 0.9782364162377876760, 1.000000000000000000 ),
 ( 0.000000000000000000, 1.000000000000000000 ),
 .UNSPECIFIED. ) ;
#51634 = CARTESIAN_POINT ( 'NONE',  ( 108.6181021060278198, 243.5177522451419065, 5.000000000000046185 ) ) ;
#51635 = EDGE_CURVE ( 'NONE', #40420, #36946, #69965, .T. ) ;
#51636 = B_SPLINE_CURVE_WITH_KNOTS ( 'NONE', 3,
 ( #80932, #11501, #42353, #73285 ),
 .UNSPECIFIED., .F., .F.,
 ( 4, 4 ),
 ( 0.009298372984062181629, 0.01507961473026592919 ),
 .UNSPECIFIED. ) ;
#51637 = CARTESIAN_POINT ( 'NONE',  ( -19.65312891409030271, 93.06504152958497400, -25.00000000000000000 ) ) ;
#51638 = CARTESIAN_POINT ( 'NONE',  ( 92.68684311912451790, 230.9865022471903444, -10.00000000000009415 ) ) ;
#51639 = CARTESIAN_POINT ( 'NONE',  ( 167.5421813246326792, 287.5986610761024167, 3.969292590682533373 ) ) ;
#51640 = B_SPLINE_CURVE_WITH_KNOTS ( 'NONE', 3,
 ( #26142, #94568, #57020, #48436, #18048, #64134, #79384, #72258, #26639, #2350 ),
 .UNSPECIFIED., .F., .F.,
 ( 4, 2, 2, 2, 4 ),
 ( 0.000000000000000000, 0.1244049413672969895, 0.2488098827345939235, 0.3732148241018908852, 0.4976197654691878469 ),
 .UNSPECIFIED. ) ;
#51641 = CARTESIAN_POINT ( 'NONE',  ( 165.2023859949471785, 269.8983204201427384, -16.28018730636620148 ) ) ;
#51642 = ORIENTED_EDGE ( 'NONE', *, *, #68937, .T. ) ;
#51643 = CARTESIAN_POINT ( 'NONE',  ( 57.73936995728981714, 194.9548013555410080, -4.594050593750042211 ) ) ;
#51644 = ORIENTED_EDGE ( 'NONE', *, *, #54036, .F. ) ;
#51645 = CARTESIAN_POINT ( 'NONE',  ( 166.5418805794664934, 264.7512503615053561, 17.71810435351582669 ) ) ;
#51646 = CARTESIAN_POINT ( 'NONE',  ( 190.9559560067148425, 299.9015775189195665, -4.895152914295826108 ) ) ;
#51647 = EDGE_CURVE ( 'NONE', #7148, #26012, #89953, .T. ) ;
#51648 = PLANE ( 'NONE',  #56362 ) ;
#51649 = ORIENTED_EDGE ( 'NONE', *, *, #81877, .F. ) ;
#51650 = CARTESIAN_POINT ( 'NONE',  ( -80.27490717900100492, 58.06504152958491005, -10.00000000000000888 ) ) ;
#51651 = CARTESIAN_POINT ( 'NONE',  ( 49.10122569834316408, 93.29622288527660601, 10.00000000000000000 ) ) ;
#51652 = DIRECTION ( 'NONE',  ( 1.000000000000000000, 0.000000000000000000, 0.000000000000000000 ) ) ;
#51653 = CARTESIAN_POINT ( 'NONE',  ( 25.47001115121704373, 36.74646525600391556, 2.839279412974139660 ) ) ;
#51654 = CARTESIAN_POINT ( 'NONE',  ( 186.6908513136935426, 264.0735798317851959, 10.85260789151241667 ) ) ;
#51655 = CARTESIAN_POINT ( 'NONE',  ( 48.91227514082039107, 78.96591507484177441, 177.5919119679930134 ) ) ;
#51656 = CARTESIAN_POINT ( 'NONE',  ( 204.9214210856886496, 275.7126824508080176, 13.23219655298346709 ) ) ;
#51657 = ORIENTED_EDGE ( 'NONE', *, *, #66927, .T. ) ;
#51658 = CARTESIAN_POINT ( 'NONE',  ( 19.86428432551159418, 29.65586893147756342, -7.433330006724137462 ) ) ;
#51659 = LINE ( 'NONE', #74485, #55873 ) ;
#51660 = CARTESIAN_POINT ( 'NONE',  ( 166.1279696197224496, 286.9939195634048588, -3.073011414649855499 ) ) ;
#51661 = CARTESIAN_POINT ( 'NONE',  ( 16.19390013444010279, 21.30066082961420904, -10.00000000000000533 ) ) ;
#51662 = EDGE_CURVE ( 'NONE', #3834, #43292, #88999, .T. ) ;
#51663 = ORIENTED_EDGE ( 'NONE', *, *, #74586, .F. ) ;
#51664 = CARTESIAN_POINT ( 'NONE',  ( -51.42721978966704910, 42.16899896210639298, 54.99999999999999289 ) ) ;
#51665 = CARTESIAN_POINT ( 'NONE',  ( 151.0778907302193943, 268.9724126853576536, 15.84769371787143832 ) ) ;
#51666 = EDGE_CURVE ( 'NONE', #54888, #63156, #76113, .T. ) ;
#51667 = LINE ( 'NONE', #91191, #2757 ) ;
#51668 = ORIENTED_EDGE ( 'NONE', *, *, #65390, .F. ) ;
#51669 = EDGE_LOOP ( 'NONE', ( #66654, #33755, #13943, #94338 ) ) ;
#51670 =( BOUNDED_CURVE ( )  B_SPLINE_CURVE ( 2, ( #1287, #41634, #32171, #10760, #85946, #38256, #8384, #46355, #54967 ),
 .UNSPECIFIED., .F., .F. ) 
 B_SPLINE_CURVE_WITH_KNOTS ( ( 3, 2, 2, 2, 3 ),
 ( 0.2217741935483870941, 0.2231182795698924692, 0.2258064516129032195, 0.2284946236559139698, 0.2298387096774193450 ),
 .UNSPECIFIED. ) 
 CURVE ( )  GEOMETRIC_REPRESENTATION_ITEM ( )  RATIONAL_B_SPLINE_CURVE ( ( 0.9330127018922194093, 0.9330127018922194093, 1.000000000000000000, 0.8660254037844387076, 1.000000000000000000, 0.8660254037844387076, 1.000000000000000000, 0.9330127018922194093, 0.9330127018922194093 ) ) 
 REPRESENTATION_ITEM ( '' )  );
#51672 = CARTESIAN_POINT ( 'NONE',  ( 89.18655626861058749, 155.9036630683315821, 0.000000000000000000 ) ) ;
#51671 = CARTESIAN_POINT ( 'NONE',  ( 159.8725050261465128, 283.2831117594137709, -3.366638177617166772 ) ) ;
#51673 = CARTESIAN_POINT ( 'NONE',  ( 149.3141802193904368, 272.0272488999566463, -11.40332369054239336 ) ) ;
#51674 = VERTEX_POINT ( 'NONE', #38179 ) ;
#51675 = CARTESIAN_POINT ( 'NONE',  ( 66.47396703475773450, 68.78583434973192823, -2.171907785482437347 ) ) ;
#51676 = DIRECTION ( 'NONE',  ( -0.8660254037844387076, -0.4999999999999998890, -0.000000000000000000 ) ) ;
#51677 = LINE ( 'NONE', #35467, #93660 ) ;
#51678 = CARTESIAN_POINT ( 'NONE',  ( 163.0435180267337216, 264.1668671365804926, -16.76137116000093386 ) ) ;
#51679 = CARTESIAN_POINT ( 'NONE',  ( 121.5540962550081190, 250.1744531367911009, 4.594050593750047540 ) ) ;
#51680 = VECTOR ( 'NONE', #96039, 1000.000000000000114 ) ;
#51681 = CARTESIAN_POINT ( 'NONE',  ( 150.6790040019602088, 269.6633047651677089, 15.38315204620803378 ) ) ;
#51682 = ORIENTED_EDGE ( 'NONE', *, *, #10193, .F. ) ;
#51683 = CARTESIAN_POINT ( 'NONE',  ( 173.5938284679934895, 265.1703973603451345, 16.93138633957164529 ) ) ;
#51684 = CARTESIAN_POINT ( 'NONE',  ( -17.42236680055705023, 149.2012482093457777, 0.000000000000000000 ) ) ;
#51685 = ORIENTED_EDGE ( 'NONE', *, *, #39701, .T. ) ;
#51686 = AXIS2_PLACEMENT_3D ( 'NONE', #48774, #27475, #50251 ) ;
#51687 = CARTESIAN_POINT ( 'NONE',  ( 148.9935118239307315, 275.4129331016238211, 7.652191349186828973 ) ) ;
#51688 = ORIENTED_EDGE ( 'NONE', *, *, #12703, .F. ) ;
#51689 = VERTEX_POINT ( 'NONE', #30608 ) ;
#51690 = EDGE_CURVE ( 'NONE', #26616, #71493, #99591, .T. ) ;
#51691 = CARTESIAN_POINT ( 'NONE',  ( 198.3150362131025588, 287.1552767044814800, 18.53472937702030521 ) ) ;
#51692 = CARTESIAN_POINT ( 'NONE',  ( 75.01075065425354182, 66.36200818202817686, -13.12054805335453622 ) ) ;
#51693 = CARTESIAN_POINT ( 'NONE',  ( 74.27495573685769159, 207.5643266524160424, 9.188101187500095079 ) ) ;
#51694 = CARTESIAN_POINT ( 'NONE',  ( 25.50001727096127979, 173.9824982072973967, 3.021315404115420679E-15 ) ) ;
#51695 = CARTESIAN_POINT ( 'NONE',  ( 81.50870630197763944, 56.04945151212235999, 16.05838072277431650 ) ) ;
#51696 = CARTESIAN_POINT ( 'NONE',  ( 150.9462701294987141, 269.2003862531290110, 13.98983978186602073 ) ) ;
#51697 = CARTESIAN_POINT ( 'NONE',  ( 175.7055647658949056, 278.3009567096344767, 15.59727287267344664 ) ) ;
#51698 = VERTEX_POINT ( 'NONE', #31089 ) ;
#51699 = VECTOR ( 'NONE', #14485, 1000.000000000000000 ) ;
#51700 = EDGE_CURVE ( 'NONE', #77384, #10835, #15379, .T. ) ;
#51701 = CARTESIAN_POINT ( 'NONE',  ( 71.36058271582115253, 63.95108385012159147, -13.16758000239697957 ) ) ;
#51702 = CARTESIAN_POINT ( 'NONE',  ( 153.0444155045374544, 265.5662918618958201, -16.15173036748435109 ) ) ;
#51703 = B_SPLINE_SURFACE_WITH_KNOTS ( 'NONE', 3, 1, ( 
 ( #93898, #15333 ),
 ( #55333, #32556 ),
 ( #63454, #46228 ),
 ( #94390, #17347 ),
 ( #79201, #7754 ),
 ( #35039, #94888 ),
 ( #2671, #87827 ),
 ( #2168, #42631 ),
 ( #72583, #87338 ),
 ( #18870, #25450 ),
 ( #42141, #56339 ),
 ( #26466, #3189 ),
 ( #50734, #19867 ),
 ( #25972, #63948 ),
 ( #26957, #81689 ),
 ( #17870, #34072 ),
 ( #33049, #80197 ),
 ( #64963, #48767 ),
 ( #79700, #57840 ),
 ( #72069, #10262 ),
 ( #33561, #41131 ),
 ( #64456, #95416 ),
 ( #10766, #56842 ),
 ( #18366, #49261 ),
 ( #88820, #41640 ),
 ( #95908, #49753 ),
 ( #57342, #12262 ),
 ( #88316, #80705 ),
 ( #11281, #3671 ),
 ( #73073, #34549 ),
 ( #65447, #81199 ),
 ( #96392, #19386 ),
 ( #50245, #11768 ),
 ( #73560, #4144 ) ),
 .UNSPECIFIED., .T., .F., .F.,
 ( 4, 2, 2, 2, 2, 2, 2, 2, 2, 2, 2, 2, 2, 2, 2, 2, 4 ),
 ( 2, 2 ),
 ( 0.000000000000000000, 0.06250000000000000000, 0.1250000000000000000, 0.1875000000000000000, 0.2500000000000000000, 0.3125000000000000000, 0.3750000000000000000, 0.4375000000000000000, 0.5000000000000000000, 0.5625000000000000000, 0.6250000000000000000, 0.6875000000000000000, 0.7500000000000000000, 0.8125000000000000000, 0.8750000000000000000, 0.9375000000000000000, 1.000000000000000000 ),
 ( 0.000000000000000000, 1.000000000000000000 ),
 .UNSPECIFIED. ) ;
#51704 = LINE ( 'NONE', #82147, #60914 ) ;
#51705 = ORIENTED_EDGE ( 'NONE', *, *, #21665, .F. ) ;
#51706 = LINE ( 'NONE', #75011, #46886 ) ;
#51707 = CARTESIAN_POINT ( 'NONE',  ( 33.84893051719189572, 201.8967562850347122, -4.648177544792955347E-16 ) ) ;
#51708 = CARTESIAN_POINT ( 'NONE',  ( 173.9947827226785364, 253.3674607417906088, -7.620349097399602201 ) ) ;
#51709 = EDGE_CURVE ( 'NONE', #19318, #95962, #88169, .T. ) ;
#51710 = EDGE_CURVE ( 'NONE', #59362, #62248, #71119, .T. ) ;
#51711 = CARTESIAN_POINT ( 'NONE',  ( 200.3160299054414395, 283.2016034839092526, -16.83023095068803343 ) ) ;
#51712 = DIRECTION ( 'NONE',  ( -0.9576970189910627429, -0.2877784213863714968, 0.000000000000000000 ) ) ;
#51713 = VECTOR ( 'NONE', #67720, 1000.000000000000000 ) ;
#51714 = CARTESIAN_POINT ( 'NONE',  ( 196.4501996009505831, 290.3852684645433442, -17.82325615854289680 ) ) ;
#51715 = CARTESIAN_POINT ( 'NONE',  ( 198.7848905689980086, 281.0584550262959738, 16.97065934373781815 ) ) ;
#51716 = DIRECTION ( 'NONE',  ( -0.000000000000000000, 0.000000000000000000, 1.000000000000000000 ) ) ;
#51717 = ADVANCED_FACE ( 'NONE', ( #63000 ), #27920, .F. ) ;
#51718 = CARTESIAN_POINT ( 'NONE',  ( 135.5998589986957086, 261.3464784336661637, 1.353441290958777327E-15 ) ) ;
#51719 = ORIENTED_EDGE ( 'NONE', *, *, #47417, .F. ) ;
#51720 = CARTESIAN_POINT ( 'NONE',  ( 88.05889915941182267, 44.40447472371889148, 4.714184461739164611 ) ) ;
#51721 = CARTESIAN_POINT ( 'NONE',  ( 86.87034215171701135, 45.69404419005449824, 7.858360242176417820 ) ) ;
#51722 = CARTESIAN_POINT ( 'NONE',  ( 155.9056400618096916, 261.9057474521822542, -16.97057099444750605 ) ) ;
#51723 = CARTESIAN_POINT ( 'NONE',  ( 73.04277380876571613, 70.56196896876863889, 7.835544939490339367 ) ) ;
#51724 = FACE_OUTER_BOUND ( 'NONE', #3229, .T. ) ;
#51725 = CARTESIAN_POINT ( 'NONE',  ( -19.65312891409030271, 93.06504152958497400, 177.5919119679930134 ) ) ;
#51726 = ORIENTED_EDGE ( 'NONE', *, *, #80152, .T. ) ;
#51727 = CARTESIAN_POINT ( 'NONE',  ( 34.97213163436671124, 51.32435524152969464, -10.00000000000000000 ) ) ;
#51728 = CARTESIAN_POINT ( 'NONE',  ( 184.8621414469888862, 277.3522383734357959, -16.75809678382782053 ) ) ;
#51729 = CARTESIAN_POINT ( 'NONE',  ( 167.5934518032285325, 249.2213856889920578, -5.568558665174853317 ) ) ;
#51730 = CARTESIAN_POINT ( 'NONE',  ( 80.49625421685304616, 49.43199229230145875, 14.16045356324821292 ) ) ;
#51731 = CARTESIAN_POINT ( 'NONE',  ( 73.71083753633998015, 69.42096255681319406, -9.886876304414311534 ) ) ;
#51732 = CARTESIAN_POINT ( 'NONE',  ( 198.6207901071857691, 266.0158434972533996, 0.2628236463959363056 ) ) ;
#51733 = CARTESIAN_POINT ( 'NONE',  ( 190.9441801652054096, 299.9219738747156043, -4.765040093794296716 ) ) ;
#51734 = B_SPLINE_CURVE_WITH_KNOTS ( 'NONE', 3,
 ( #43537, #20764, #6041, #82601 ),
 .UNSPECIFIED., .F., .F.,
 ( 4, 4 ),
 ( 0.04073415133443882008, 0.04887066958154930030 ),
 .UNSPECIFIED. ) ;
#51735 = CARTESIAN_POINT ( 'NONE',  ( 71.64460139743449929, 72.06580075763625359, -0.2659531731967009760 ) ) ;
#51736 = CARTESIAN_POINT ( 'NONE',  ( 157.1539462478114615, 258.4483758192793061, -17.96006278656275867 ) ) ;
#51737 = CARTESIAN_POINT ( 'NONE',  ( 193.2382381725520872, 268.8873971962033806, 12.20118083718656443 ) ) ;
#51738 = CARTESIAN_POINT ( 'NONE',  ( 14.54318666465499632, 27.13478043621387314, 8.090169943749478065 ) ) ;
#51739 = CARTESIAN_POINT ( 'NONE',  ( 149.6676065383367416, 271.4150965588098074, 11.80358707172367261 ) ) ;
#51740 = DIRECTION ( 'NONE',  ( 1.000000000000000000, 1.830829162166278276E-15, 0.000000000000000000 ) ) ;
#51741 = CARTESIAN_POINT ( 'NONE',  ( 28.46864935082048831, 149.7156766241961350, -22.49999999999983658 ) ) ;
#51742 = CARTESIAN_POINT ( 'NONE',  ( 191.2190380946134951, 260.9445496458436651, 3.106810577783889915 ) ) ;
#51743 = CARTESIAN_POINT ( 'NONE',  ( 72.27876543856895353, 72.05160118724565166, -3.335218298938914749 ) ) ;
#51744 = CARTESIAN_POINT ( 'NONE',  ( 136.2587462434811982, 256.1427522451419350, 10.00000000000009237 ) ) ;
#51745 = CARTESIAN_POINT ( 'NONE',  ( 175.4001851152161464, 286.5081113820362475, -12.63027609277786567 ) ) ;
#51746 = ORIENTED_EDGE ( 'NONE', *, *, #17475, .T. ) ;
#51747 = VECTOR ( 'NONE', #25133, 1000.000000000000000 ) ;
#51748 = CARTESIAN_POINT ( 'NONE',  ( 66.48609986787805326, 67.91412938167108848, -6.639081268635919741 ) ) ;
#51749 = CARTESIAN_POINT ( 'NONE',  ( 199.2383506163646132, 285.5560492466715345, -17.78808061564097898 ) ) ;
#51750 = CARTESIAN_POINT ( 'NONE',  ( 17.65854496445001587, 174.8768266524159856, -9.188101187500093303 ) ) ;
#51751 = CARTESIAN_POINT ( 'NONE',  ( 176.7567624778341440, 257.9301109217140038, -10.40897364086542254 ) ) ;
#51752 = CARTESIAN_POINT ( 'NONE',  ( 20.44528175232247591, 34.73705186507753950, -3.090169943749475845 ) ) ;
#51753 = CARTESIAN_POINT ( 'NONE',  ( 85.21216800587870921, 49.06579667261281230, 12.45646816431239223 ) ) ;
#51754 = CARTESIAN_POINT ( 'NONE',  ( 204.6149525604204769, 276.2435015074934199, -13.22810747389629960 ) ) ;
#51755 = LINE ( 'NONE', #70302, #80876 ) ;
#51756 = FACE_OUTER_BOUND ( 'NONE', #41249, .T. ) ;
#51758 = CARTESIAN_POINT ( 'NONE',  ( 66.61587002248256795, 219.2677522451419065, -5.000000000000047962 ) ) ;
#51757 = CARTESIAN_POINT ( 'NONE',  ( 22.90194105960797089, 172.4824982072973967, 3.021315404115420679E-15 ) ) ;
#51759 = CARTESIAN_POINT ( 'NONE',  ( 181.4632975752175525, 255.1188003790442167, 1.936479460681336695 ) ) ;
#51760 = CARTESIAN_POINT ( 'NONE',  ( 198.7430995078048284, 286.4138493292020371, 18.01120443222870193 ) ) ;
#51761 = CARTESIAN_POINT ( 'NONE',  ( 179.4303423924146443, 294.0762619279377077, 1.040177563636374147 ) ) ;
#51762 = CARTESIAN_POINT ( 'NONE',  ( 51.98364914125590985, 207.4865022471902876, 10.00000000000009237 ) ) ;
#51763 = CARTESIAN_POINT ( 'NONE',  ( 184.7458354044235591, 293.7380398689933827, 9.593738941526117614 ) ) ;
#51764 = CARTESIAN_POINT ( 'NONE',  ( 190.2476911738421848, 301.1283281946692796, -1.360079143321618611 ) ) ;
#51765 = CARTESIAN_POINT ( 'NONE',  ( 21.44705901024191874, 189.3149278399161233, 9.188101187500093303 ) ) ;
#51766 = CARTESIAN_POINT ( 'NONE',  ( 166.0706209929512340, 285.2106937319115332, 4.119889468574966074 ) ) ;
#51767 = CARTESIAN_POINT ( 'NONE',  ( 13.08467475460494001, 168.3615022471902023, 5.000000000000051514 ) ) ;
#51768 = CARTESIAN_POINT ( 'NONE',  ( 40.74993669414823927, 32.03085787977766330, 9.188101187500006262 ) ) ;
#51769 = LINE ( 'NONE', #7137, #33616 ) ;
#51770 = EDGE_CURVE ( 'NONE', #75836, #65652, #24035, .T. ) ;
#51771 = CARTESIAN_POINT ( 'NONE',  ( 207.6007741873543750, 271.0719067473055475, 7.587922723682903658 ) ) ;
#51772 = CARTESIAN_POINT ( 'NONE',  ( 185.5568049818104726, 266.1438378612298834, 14.60334785453874140 ) ) ;
#51773 = DIRECTION ( 'NONE',  ( -0.4999999999999997780, -0.8660254037844387076, 0.000000000000000000 ) ) ;
#51774 = CARTESIAN_POINT ( 'NONE',  ( 160.1884772505443379, 280.3385904657917536, 9.408981587793775248 ) ) ;
#51775 = DIRECTION ( 'NONE',  ( 1.000000000000000000, 0.000000000000000000, 0.000000000000000000 ) ) ;
#51776 = CARTESIAN_POINT ( 'NONE',  ( 19.20273687360401027, 16.80170272979925628, 7.433330006724137462 ) ) ;
#51777 = LINE ( 'NONE', #46131, #53123 ) ;
#51778 = CARTESIAN_POINT ( 'NONE',  ( 82.75953659669094975, 53.91263660082293541, 15.45461559304629340 ) ) ;
#51779 = AXIS2_PLACEMENT_3D ( 'NONE', #52975, #12506, #51988 ) ;
#51780 = CARTESIAN_POINT ( 'NONE',  ( -31.49356256989596758, 94.88921800892812541, 45.19948692389422717 ) ) ;
#51781 = CARTESIAN_POINT ( 'NONE',  ( 194.1153812227096864, 294.4292925221022870, 15.54001482840963710 ) ) ;
#51782 = VERTEX_POINT ( 'NONE', #11698 ) ;
#51783 = CARTESIAN_POINT ( 'NONE',  ( 181.5727239729958455, 289.2385163777758521, 12.59120802838236663 ) ) ;
#51784 = CARTESIAN_POINT ( 'NONE',  ( 112.6979501180548766, 224.3262482093458061, 3.021315404115420679E-15 ) ) ;
#51785 = CARTESIAN_POINT ( 'NONE',  ( 48.38981961164311940, 109.5014996615669105, 10.00000000000000000 ) ) ;
#51786 = EDGE_CURVE ( 'NONE', #55413, #95379, #97797, .T. ) ;
#51787 = ORIENTED_EDGE ( 'NONE', *, *, #78226, .T. ) ;
#51788 = CARTESIAN_POINT ( 'NONE',  ( 196.6401797514039629, 289.6109730388196226, -16.42068076416023459 ) ) ;
#51789 = CARTESIAN_POINT ( 'NONE',  ( 68.52305094706389355, 70.17018868913098117, -0.3349893018502964059 ) ) ;
#51790 = FACE_OUTER_BOUND ( 'NONE', #18823, .T. ) ;
#51791 = EDGE_CURVE ( 'NONE', #44322, #21181, #44050, .T. ) ;
#51792 = CARTESIAN_POINT ( 'NONE',  ( 154.8786460229866577, 262.3893114111486398, -18.06164891362396929 ) ) ;
#51793 = EDGE_LOOP ( 'NONE', ( #86934, #93023, #68258, #54998 ) ) ;
#51794 = ORIENTED_EDGE ( 'NONE', *, *, #57037, .F. ) ;
#51796 = CARTESIAN_POINT ( 'NONE',  ( 32.80507291521585955, 117.6754530847557874, 59.99999999999999289 ) ) ;
#51795 = CARTESIAN_POINT ( 'NONE',  ( 164.3636283963731159, 246.5961090085728245, -4.466486389993993278 ) ) ;
#51797 = CARTESIAN_POINT ( 'NONE',  ( 192.6470966816805230, 296.9724359471326807, 11.11268290051284424 ) ) ;
#51798 = ORIENTED_EDGE ( 'NONE', *, *, #56258, .F. ) ;
#51799 = CARTESIAN_POINT ( 'NONE',  ( 88.07576543976308869, 43.78748546321877910, -2.154750241475199335 ) ) ;
#51800 = CARTESIAN_POINT ( 'NONE',  ( 80.44110801039052205, 57.53904330600535388, -16.59063950305211677 ) ) ;
#51801 = CARTESIAN_POINT ( 'NONE',  ( 54.19488099963222538, 190.5494855054051868, -2.679491924311248496 ) ) ;
#51802 = ORIENTED_EDGE ( 'NONE', *, *, #54833, .F. ) ;
#51803 = FACE_OUTER_BOUND ( 'NONE', #9569, .T. ) ;
#51804 = ORIENTED_EDGE ( 'NONE', *, *, #78524, .T. ) ;
#51805 = CARTESIAN_POINT ( 'NONE',  ( 164.9103019330012216, 245.0139736909548560, 2.841678961959298810 ) ) ;
#51806 = CARTESIAN_POINT ( 'NONE',  ( 74.78917493913915848, 64.52558641573418186, 14.02150606163593949 ) ) ;
#51807 = EDGE_LOOP ( 'NONE', ( #44027, #56613, #64952, #86270 ) ) ;
#51808 = CARTESIAN_POINT ( 'NONE',  ( 175.0586189538327346, 277.5951793296135861, -15.65476470407738852 ) ) ;
#51809 = APPLICATION_CONTEXT ( 'automotive_design' ) ;
#51810 = CARTESIAN_POINT ( 'NONE',  ( 169.5394509045560767, 261.5465616151283257, -16.63734821970730948 ) ) ;
#51811 = ORIENTED_EDGE ( 'NONE', *, *, #36752, .F. ) ;
#51812 = CARTESIAN_POINT ( 'NONE',  ( 41.80956963312145547, 25.10801979619932567, 3.090169943749476733 ) ) ;
#51813 = CARTESIAN_POINT ( 'NONE',  ( 192.4335622838504207, 297.3422883733380786, -12.83044365323471325 ) ) ;
#51814 = ORIENTED_EDGE ( 'NONE', *, *, #25001, .T. ) ;
#51815 = ORIENTED_EDGE ( 'NONE', *, *, #50811, .T. ) ;
#51816 = EDGE_CURVE ( 'NONE', #75490, #45639, #30009, .T. ) ;
#51817 = CARTESIAN_POINT ( 'NONE',  ( 156.6873744850167611, 266.6461852411879931, -16.20640834931786500 ) ) ;
#51818 = CARTESIAN_POINT ( 'NONE',  ( 147.4317198359019301, 275.2877659273946733, 3.797273160043843188 ) ) ;
#51819 = LINE ( 'NONE', #5217, #78742 ) ;
#51820 = DIRECTION ( 'NONE',  ( -0.8660254037844387076, -0.4999999999999998890, -0.000000000000000000 ) ) ;
#51821 = CARTESIAN_POINT ( 'NONE',  ( 192.1640094933931096, 297.8091675017319062, 12.36911124822534447 ) ) ;
#51822 = CARTESIAN_POINT ( 'NONE',  ( 147.2990839561455800, 275.5174980100389348, 0.1083234189483078536 ) ) ;
#51823 = CARTESIAN_POINT ( 'NONE',  ( 191.0604813119340690, 299.7205343796033503, -9.270812881586136811 ) ) ;
#51824 = VERTEX_POINT ( 'NONE', #57765 ) ;
#51825 = ADVANCED_FACE ( 'NONE', ( #42557 ), #58755, .T. ) ;
#51826 = LINE ( 'NONE', #83243, #94981 ) ;
#51827 = LINE ( 'NONE', #37104, #7352 ) ;
#51829 = CARTESIAN_POINT ( 'NONE',  ( -15.61417992190811788, 23.18166087982996970, -10.00000000000000000 ) ) ;
#51828 = CARTESIAN_POINT ( 'NONE',  ( 196.7130436017243653, 289.9300093007386749, -16.33278734947153765 ) ) ;
#51830 = CARTESIAN_POINT ( 'NONE',  ( 79.98829826350832661, 44.59498145193617802, 11.76229303994366049 ) ) ;
#51831 = CARTESIAN_POINT ( 'NONE',  ( 168.5642857825677368, 286.4821439168015331, 4.072950439418188573 ) ) ;
#51832 = CARTESIAN_POINT ( 'NONE',  ( 44.95821123098112082, 116.5722627105190270, -10.00000000000000000 ) ) ;
#51833 = ORIENTED_EDGE ( 'NONE', *, *, #33898, .F. ) ;
#51834 = CARTESIAN_POINT ( 'NONE',  ( 149.2987140599570921, 272.0540370738933689, -11.50637251393979454 ) ) ;
#51835 = CARTESIAN_POINT ( 'NONE',  ( 78.86497519275886248, 53.26976081405998542, -15.76972371277651064 ) ) ;
#51836 = EDGE_CURVE ( 'NONE', #17132, #12659, #84549, .T. ) ;
#51837 = CARTESIAN_POINT ( 'NONE',  ( 202.7516255845870603, 278.9848387806140977, 15.23277972257327129 ) ) ;
#51838 = CARTESIAN_POINT ( 'NONE',  ( 79.43760634492710437, 46.26763820643595437, 12.65635740753111449 ) ) ;
#51839 = CARTESIAN_POINT ( 'NONE',  ( 198.6984454753927594, 286.4911923821024970, -17.36054842559500599 ) ) ;
#51840 = CARTESIAN_POINT ( 'NONE',  ( -75.14068524134967220, 52.46521621197197760, 10.00000000000000000 ) ) ;
#51841 = CIRCLE ( 'NONE', #98783, 14.21260523776213347 ) ;
#51842 = EDGE_LOOP ( 'NONE', ( #63717, #38954, #53629, #17640 ) ) ;
#51843 = CARTESIAN_POINT ( 'NONE',  ( 170.4725219931047207, 255.4922488510977132, -11.62136048534125798 ) ) ;
#51844 = CARTESIAN_POINT ( 'NONE',  ( 205.5791761573774181, 272.5734172477073116, 10.13670412909801044 ) ) ;
#51845 = CARTESIAN_POINT ( 'NONE',  ( 206.9878665138179770, 272.1334939782196329, 6.566295309274049252 ) ) ;
#51846 = CARTESIAN_POINT ( 'NONE',  ( 37.60401899570393880, 182.5177522451417929, 5.000000000000051514 ) ) ;
#51847 = CARTESIAN_POINT ( 'NONE',  ( 114.4640339051705666, 227.7048013555410080, 4.594050593750051981 ) ) ;
#51848 = CARTESIAN_POINT ( 'NONE',  ( 151.1451503555562113, 268.8559155969762742, -15.81507177720227553 ) ) ;
#51849 = CARTESIAN_POINT ( 'NONE',  ( 164.2528612105914192, 280.3318051388083063, -11.32557250155417705 ) ) ;
#51850 = CARTESIAN_POINT ( 'NONE',  ( 196.0034224882197975, 291.1591091234520263, 17.53794140922627776 ) ) ;
#51851 = CARTESIAN_POINT ( 'NONE',  ( 172.4983949698107892, 251.2745399082947415, -3.985004546235816569 ) ) ;
#51852 = CARTESIAN_POINT ( 'NONE',  ( 41.20343708195693466, 194.5958772461660544, -9.188101187500095079 ) ) ;
#51853 = CARTESIAN_POINT ( 'NONE',  ( 147.7567117497646052, 276.1838835526310731, -2.437780156652150421 ) ) ;
#51854 = ORIENTED_EDGE ( 'NONE', *, *, #2597, .T. ) ;
#51855 = CARTESIAN_POINT ( 'NONE',  ( -52.57320609282758994, 32.70376883311633520, -10.00000000000000000 ) ) ;
#51856 = CARTESIAN_POINT ( 'NONE',  ( 181.8794332036203798, 266.9208721406195082, 15.44781841919039600 ) ) ;
#51857 = B_SPLINE_CURVE_WITH_KNOTS ( 'NONE', 3,
 ( #20868, #12267, #82700, #4656, #35549, #66451, #97377, #36534, #58826, #89787, #95911, #14737, #7128, #38011, #68430, #37036, #68925, #23323, #76071, #75555, #99357, #91773, #6140, #83181, #59833, #21351, #13741, #77026, #21841, #7633, #6650, #45620, #52236, #84188, #91275, #46112, #29936, #22338, #53236, #52724, #15217, #99850, #76549, #60813, #30434, #29442, #44621, #49, #37524, #54210 ),
 .UNSPECIFIED., .F., .F.,
 ( 4, 2, 2, 2, 2, 2, 2, 2, 2, 2, 2, 2, 2, 2, 2, 2, 2, 2, 2, 2, 2, 2, 2, 2, 4 ),
 ( 0.001289879915731821603, 0.001760445656852789847, 0.002231011397973757873, 0.002466294268534241670, 0.002583935703814484001, 0.002701577139094726333, 0.002819218574374968665, 0.002936860009655210997, 0.003172142880215804515, 0.003642708621336909584, 0.004113274362458015088, 0.005054405844700225227, 0.005995537326942436233, 0.006466103068063580768, 0.006936668809184724435, 0.007054310244465032687, 0.007113130962105199823, 0.007171951679745365224, 0.007289593115025630975, 0.007407234550305896725, 0.007642517420866428227, 0.007877800291426959728, 0.008113083161987491229, 0.008348366032548022730, 0.008818931773669085733 ),
 .UNSPECIFIED. ) ;
#51858 = CARTESIAN_POINT ( 'NONE',  ( 28.14990833772381151, 180.3927522451418497, 10.00000000000009948 ) ) ;
#51859 = CARTESIAN_POINT ( 'NONE',  ( 82.10527917775937112, 41.44314374168844495, -5.931418479470229599 ) ) ;
#51860 = EDGE_CURVE ( 'NONE', #37198, #57617, #2358, .T. ) ;
#51861 = CARTESIAN_POINT ( 'NONE',  ( 207.8431546909062320, 270.6520914003897360, -6.441273666418043220 ) ) ;
#51862 = CARTESIAN_POINT ( 'NONE',  ( 179.3101858657603884, 287.6933342559568132, -12.46481062744024726 ) ) ;
#51863 = CARTESIAN_POINT ( 'NONE',  ( 164.1895775543868581, 249.9821507493112733, 11.20547600539854116 ) ) ;
#51864 = CARTESIAN_POINT ( 'NONE',  ( 92.59663213601581333, 214.2677522451417929, -5.000000000000041744 ) ) ;
#51865 = ORIENTED_EDGE ( 'NONE', *, *, #55148, .F. ) ;
#51867 = EDGE_CURVE ( 'NONE', #31869, #50517, #78579, .T. ) ;
#51866 = B_SPLINE_CURVE_WITH_KNOTS ( 'NONE', 3,
 ( #75193, #59953, #42756, #35171, #98497, #6270, #38658, #37649, #54855, #30063, #168, #61941, #14376, #85308, #76668, #61454, #15854, #663, #8764, #93402, #60952, #16363, #84310, #7256, #53841, #38139, #41648, #48263, #80714, #16856, #79211, #9785, #24462, #72590, #18880, #42148, #40141, #71583, #78680, #64464, #2680, #71083 ),
 .UNSPECIFIED., .F., .F.,
 ( 4, 2, 2, 2, 2, 2, 2, 2, 2, 2, 2, 2, 2, 2, 2, 2, 2, 2, 2, 2, 4 ),
 ( 0.002125255516391542313, 0.002560878705408519730, 0.002778690299917009957, 0.002996501894425500617, 0.003105407691679724913, 0.003214313488933949643, 0.003432125083442451145, 0.003867748272459595963, 0.004738994650493884297, 0.005610241028528172198, 0.006481487406562460099, 0.006917110595579561982, 0.007352733784596663866, 0.007461639581850977934, 0.007516092480478200888, 0.007570545379105423842, 0.007679451176359996384, 0.007788356973614568926, 0.008223980162633185223, 0.008659603351651801520, 0.009095226540670417817 ),
 .UNSPECIFIED. ) ;
#51868 = CARTESIAN_POINT ( 'NONE',  ( 198.7995061717253975, 267.7512988405533179, -8.185998893406019050 ) ) ;
#51869 = CARTESIAN_POINT ( 'NONE',  ( 162.6476498368881494, 248.9330020812748785, 10.75824100428386743 ) ) ;
#51870 = CARTESIAN_POINT ( 'NONE',  ( 153.8835784885725104, 264.7437728202501148, 16.55976697655874119 ) ) ;
#51871 = CARTESIAN_POINT ( 'NONE',  ( 23.85612603422365297, 175.3923013555409796, 4.594050593750050204 ) ) ;
#51872 = FACE_OUTER_BOUND ( 'NONE', #58180, .T. ) ;
#51873 = CARTESIAN_POINT ( 'NONE',  ( 192.3798651076289445, 272.0250015905760961, 14.19073807892398698 ) ) ;
#51874 = CARTESIAN_POINT ( 'NONE',  ( 71.63738353716577478, 58.87189805328393533, -15.39703515908747811 ) ) ;
#51875 = CARTESIAN_POINT ( 'NONE',  ( -19.65312891409030271, 93.06504152958497400, 10.00000000000000888 ) ) ;
#51876 = CARTESIAN_POINT ( 'NONE',  ( 53.57110205792969282, 210.9244531367911577, -4.594050593750046652 ) ) ;
#51877 = CARTESIAN_POINT ( 'NONE',  ( 164.3890147726454813, 245.9168695380243435, -6.010262808998044548 ) ) ;
#51878 = CARTESIAN_POINT ( 'NONE',  ( 204.0436569602353245, 275.5599050935638843, 13.20187375397782858 ) ) ;
#51879 = CARTESIAN_POINT ( 'NONE',  ( 167.5861325596884797, 256.5095974891418109, 15.03189046419509367 ) ) ;
#51880 = CARTESIAN_POINT ( 'NONE',  ( 150.1819311511804642, 277.9734069837974744, -1.930257866626041707 ) ) ;
#51881 = ORIENTED_EDGE ( 'NONE', *, *, #76478, .T. ) ;
#51882 = CARTESIAN_POINT ( 'NONE',  ( 21.81709757609801770, 176.7365022471902023, 10.00000000000009592 ) ) ;
#51883 = DIRECTION ( 'NONE',  ( -0.7135562106085678868, 0.7005979833698787740, 0.000000000000000000 ) ) ;
#51884 = CARTESIAN_POINT ( 'NONE',  ( 138.1979352100490530, 262.8464784336661637, 1.353441290958777327E-15 ) ) ;
#51885 = CARTESIAN_POINT ( 'NONE',  ( 29.48197064213787044, 19.94754757982090609, 5.678558825948272215 ) ) ;
#51886 = CARTESIAN_POINT ( 'NONE',  ( 207.5676051492868339, 271.1293572064768682, -7.361967423939656641 ) ) ;
#51887 = DIRECTION ( 'NONE',  ( -0.3940053768033626169, 0.6824373310787468228, 0.6156614753256509642 ) ) ;
#51888 = DIRECTION ( 'NONE',  ( -0.6201213960746324583, 0.7845058662179964504, 0.000000000000000000 ) ) ;
#51890 = CARTESIAN_POINT ( 'NONE',  ( 185.8092585116022804, 288.0989997903241147, 14.76281570939348775 ) ) ;
#51889 = CARTESIAN_POINT ( 'NONE',  ( 81.67891891309422192, 41.47871809714329316, -5.216020542643499347 ) ) ;
#51891 = CARTESIAN_POINT ( 'NONE',  ( 68.54052320776597185, 64.24254624729013585, 11.78809861305686901 ) ) ;
#51892 = ORIENTED_EDGE ( 'NONE', *, *, #28321, .T. ) ;
#51893 = CARTESIAN_POINT ( 'NONE',  ( 198.0816276881963915, 264.5915495180347534, -1.723934393811154182E-14 ) ) ;
#51894 = CARTESIAN_POINT ( 'NONE',  ( 163.6574618462221906, 247.1839563750149011, 8.953931665434316400 ) ) ;
#51895 = CARTESIAN_POINT ( 'NONE',  ( 29.30989995549245464, 44.80713248141895377, 10.00000000000000000 ) ) ;
#51896 = CARTESIAN_POINT ( 'NONE',  ( 169.6026530775712331, 266.0157843702824039, -17.26773840881970656 ) ) ;
#51897 = CARTESIAN_POINT ( 'NONE',  ( 2.730238736670421940, 24.68290643055184930, 3.479690158560446702E-15 ) ) ;
#51898 = EDGE_LOOP ( 'NONE', ( #17735, #87510, #87616, #80662 ) ) ;
#51899 = DIRECTION ( 'NONE',  ( 0.2165469281463284490, -0.9762722099447412871, 0.000000000000000000 ) ) ;
#51900 = DIRECTION ( 'NONE',  ( 0.000000000000000000, 0.000000000000000000, -1.000000000000000000 ) ) ;
#51901 = EDGE_CURVE ( 'NONE', #42456, #52395, #48675, .T. ) ;
#51902 = CARTESIAN_POINT ( 'NONE',  ( 200.5914588262792222, 282.7033700937254821, -16.73555027083989444 ) ) ;
#51903 = CARTESIAN_POINT ( 'NONE',  ( 196.2456956133878521, 270.8883091705321249, 12.07148411369787055 ) ) ;
#51904 = CARTESIAN_POINT ( 'NONE',  ( 185.8273479531363250, 296.6862851380694792, 4.675326410034602809 ) ) ;
#51905 = EDGE_CURVE ( 'NONE', #2096, #23710, #49170, .T. ) ;
#51906 = LINE ( 'NONE', #82846, #87440 ) ;
#51907 = VECTOR ( 'NONE', #51398, 1000.000000000000000 ) ;
#51908 = CARTESIAN_POINT ( 'NONE',  ( 149.7609858458625638, 276.9949590675715285, -0.0001241879625487765464 ) ) ;
#51909 = DIRECTION ( 'NONE',  ( 0.5000000000000002220, -0.8660254037844384856, -0.000000000000000000 ) ) ;
#51910 = ADVANCED_FACE ( 'NONE', ( #95816 ), #57245, .F. ) ;
#51911 = CARTESIAN_POINT ( 'NONE',  ( 12.48001537019352192, 22.90829794293879473, 10.00000000000000355 ) ) ;
#51912 = DIRECTION ( 'NONE',  ( -0.8660254037844387076, -0.4999999999999998890, -0.000000000000000000 ) ) ;
#51913 = ORIENTED_EDGE ( 'NONE', *, *, #67685, .T. ) ;
#51914 = CARTESIAN_POINT ( 'NONE',  ( 168.3139509857544454, 277.6662850288790310, 15.73022063764310730 ) ) ;
#51915 = DIRECTION ( 'NONE',  ( 0.1162373735601320568, 0.9932214622066130039, 0.000000000000000000 ) ) ;
#51916 = CARTESIAN_POINT ( 'NONE',  ( 157.2489658521533613, 262.6752155823469934, -16.93568676516632365 ) ) ;
#51917 = ORIENTED_EDGE ( 'NONE', *, *, #26405, .F. ) ;
#51918 = CARTESIAN_POINT ( 'NONE',  ( 191.1747001918821525, 299.5227014763493116, -9.654804683100723040 ) ) ;
#51919 = DIRECTION ( 'NONE',  ( -0.8660254037844387076, -0.4999999999999998890, -0.000000000000000000 ) ) ;
#51920 = CARTESIAN_POINT ( 'NONE',  ( 204.3371846825755824, 276.7246095846310823, 14.72513001683937262 ) ) ;
#51921 = CARTESIAN_POINT ( 'NONE',  ( 74.71494119846802562, 53.60965191683258269, 16.08410365026011846 ) ) ;
#51922 = ORIENTED_EDGE ( 'NONE', *, *, #21916, .T. ) ;
#51923 = CARTESIAN_POINT ( 'NONE',  ( 87.77910550741502504, 230.6744531367911293, 4.594050593750047540 ) ) ;
#51924 = CARTESIAN_POINT ( 'NONE',  ( 202.9132053460394900, 279.1910141444395776, 16.06438581368443863 ) ) ;
#51925 = CARTESIAN_POINT ( 'NONE',  ( 182.7359208079271014, 258.3743599538522062, -5.878668705868922650 ) ) ;
#51926 = ADVANCED_FACE ( 'NONE', ( #93804 ), #63857, .F. ) ;
#51927 = ORIENTED_EDGE ( 'NONE', *, *, #57166, .T. ) ;
#51928 = ORIENTED_EDGE ( 'NONE', *, *, #6611, .T. ) ;
#51929 = DIRECTION ( 'NONE',  ( -0.9481851146622203297, -0.3177184104407421716, 0.000000000000000000 ) ) ;
#51930 = ORIENTED_EDGE ( 'NONE', *, *, #70214, .F. ) ;
#51931 = CARTESIAN_POINT ( 'NONE',  ( 82.05352392983871823, 53.80490633333712225, 15.54385313613422426 ) ) ;
#51932 = EDGE_LOOP ( 'NONE', ( #39842, #94933, #76957, #55951, #7422 ) ) ;
#51933 = CARTESIAN_POINT ( 'NONE',  ( 48.53010236944518851, 101.9116055364396090, -10.00000000000000000 ) ) ;
#51934 = ORIENTED_EDGE ( 'NONE', *, *, #34687, .F. ) ;
#51935 = CARTESIAN_POINT ( 'NONE',  ( 207.4508013134534110, 271.3316673846591129, -6.981098720164411908 ) ) ;
#51936 = ADVANCED_FACE ( 'NONE', ( #97288 ), #99812, .F. ) ;
#51937 = DIRECTION ( 'NONE',  ( -0.5000000000000014433, 0.8660254037844379305, 0.000000000000000000 ) ) ;
#51938 = PLANE ( 'NONE',  #39795 ) ;
#51939 = CARTESIAN_POINT ( 'NONE',  ( 194.4826705584825390, 293.7931287314651740, -16.11258321617245315 ) ) ;
#51940 = CARTESIAN_POINT ( 'NONE',  ( 29.42114147039228200, 17.39040679176983772, 1.333680081654574804E-15 ) ) ;
#51941 = CARTESIAN_POINT ( 'NONE',  ( 164.7413213274116117, 265.1114538392643567, -16.62100242902791791 ) ) ;
#51942 = ORIENTED_EDGE ( 'NONE', *, *, #54440, .T. ) ;
#51943 = CARTESIAN_POINT ( 'NONE',  ( 76.51060883434578841, 58.77893196432874134, 16.01845725252526265 ) ) ;
#51944 = CARTESIAN_POINT ( 'NONE',  ( 12.93244592517074487, 8.262165230724926701, -2.296566073217252530E-15 ) ) ;
#51945 = ORIENTED_EDGE ( 'NONE', *, *, #1316, .T. ) ;
#51946 = CARTESIAN_POINT ( 'NONE',  ( 167.0371890489551845, 283.5610238238203351, 9.003790523892211795 ) ) ;
#51948 = ORIENTED_EDGE ( 'NONE', *, *, #7869, .T. ) ;
#51947 = CARTESIAN_POINT ( 'NONE',  ( 199.9947097613220706, 270.1151134968761767, 10.21374482337263245 ) ) ;
#51949 = CARTESIAN_POINT ( 'NONE',  ( -18.95853632553436086, 41.33786475637849378, 59.99999999999999289 ) ) ;
#51950 = CARTESIAN_POINT ( 'NONE',  ( 206.8659638600981623, 272.3446355680395641, -10.26115277030573125 ) ) ;
#51951 = CARTESIAN_POINT ( 'NONE',  ( 149.0807665407234026, 276.4376266709116408, -5.539133476438467873 ) ) ;
#51952 = CARTESIAN_POINT ( 'NONE',  ( 165.3590881290603534, 246.8046831517908686, -1.872135347154431084 ) ) ;
#51953 = LINE ( 'NONE', #37722, #1073 ) ;
#51954 = CARTESIAN_POINT ( 'NONE',  ( 86.99204085828590394, 44.40222714392293568, 5.125783883892307990 ) ) ;
#51955 = CARTESIAN_POINT ( 'NONE',  ( 194.7141629039813040, 292.6873139064718998, 15.09280609635813342 ) ) ;
#51956 =( BOUNDED_CURVE ( )  B_SPLINE_CURVE ( 2, ( #77999, #8592, #62260, #1, #80410, #93216, #39456, #92721, #88027, #70381, #61773, #62770, #93729 ),
 .UNSPECIFIED., .F., .T. ) 
 B_SPLINE_CURVE_WITH_KNOTS ( ( 3, 2, 2, 2, 2, 2, 3 ),
 ( 0.3375000000000000222, 0.3400000000000000244, 0.3449999999999999734, 0.3499999999999999778, 0.3549999999999999822, 0.3599999999999999867, 0.3624999999999999889 ),
 .UNSPECIFIED. ) 
 CURVE ( )  GEOMETRIC_REPRESENTATION_ITEM ( )  RATIONAL_B_SPLINE_CURVE ( ( 0.9755282581475768211, 0.9755282581475768211, 1.000000000000000000, 0.9510565162951535312, 1.000000000000000000, 0.9510565162951535312, 1.000000000000000000, 0.9510565162951535312, 1.000000000000000000, 0.9510565162951535312, 1.000000000000000000, 0.9755282581475768211, 0.9755282581475768211 ) ) 
 REPRESENTATION_ITEM ( '' )  );
#51957 = EDGE_LOOP ( 'NONE', ( #17264, #39704, #32461, #5857 ) ) ;
#51958 = CARTESIAN_POINT ( 'NONE',  ( 194.3703447720679094, 293.9876827005354585, -15.62866922547675941 ) ) ;
#51959 = CARTESIAN_POINT ( 'NONE',  ( 73.36977505992142312, 62.78772663851135860, -14.42615283414499316 ) ) ;
#51960 = ORIENTED_EDGE ( 'NONE', *, *, #99830, .T. ) ;
#51961 = CARTESIAN_POINT ( 'NONE',  ( 160.7849810028513673, 275.7942143859138469, 12.80952477407467249 ) ) ;
#51962 = DIRECTION ( 'NONE',  ( 0.000000000000000000, 0.000000000000000000, 1.000000000000000000 ) ) ;
#51963 = CARTESIAN_POINT ( 'NONE',  ( 204.2530634011613131, 276.8703119180381691, -15.12695148340227647 ) ) ;
#51964 = CARTESIAN_POINT ( 'NONE',  ( 83.44519214171087640, 44.67505360890212529, -9.064355971954283220 ) ) ;
#51965 = EDGE_CURVE ( 'NONE', #24162, #41583, #27404, .T. ) ;
#51966 = FACE_OUTER_BOUND ( 'NONE', #27529, .T. ) ;
#51968 = CARTESIAN_POINT ( 'NONE',  ( 75.99625379708062667, 65.54331796600069993, 13.91730801885865354 ) ) ;
#51967 = CARTESIAN_POINT ( 'NONE',  ( -2.449395605728673875, 160.2048013555409796, 4.594050593750051981 ) ) ;
#51969 = CARTESIAN_POINT ( 'NONE',  ( 189.0874221891241689, 297.0145170083281982, 8.224122883010650753 ) ) ;
#51970 = VERTEX_POINT ( 'NONE', #50157 ) ;
#51971 = ORIENTED_EDGE ( 'NONE', *, *, #69578, .F. ) ;
#51972 = CARTESIAN_POINT ( 'NONE',  ( -19.65312891409030271, 93.06504152958497400, 59.99999999999999289 ) ) ;
#51973 = CYLINDRICAL_SURFACE ( 'NONE', #72342, 10.00000000000001066 ) ;
#51974 = CARTESIAN_POINT ( 'NONE',  ( 85.67156739209939076, 48.86885130997027460, -12.09209206581120455 ) ) ;
#51975 = CARTESIAN_POINT ( 'NONE',  ( 171.6778415374343467, 289.4884753385041449, 2.667625303753221377 ) ) ;
#51976 = CARTESIAN_POINT ( 'NONE',  ( 86.21810832699266314, 43.22812469855217188, 2.504907440873156421 ) ) ;
#51977 = VECTOR ( 'NONE', #33077, 1000.000000000000000 ) ;
#51978 = CARTESIAN_POINT ( 'NONE',  ( 84.84478398652468911, 48.04838981413973187, 11.80738860868059703 ) ) ;
#51979 = DIRECTION ( 'NONE',  ( 0.000000000000000000, 0.000000000000000000, 1.000000000000000000 ) ) ;
#51980 = CARTESIAN_POINT ( 'NONE',  ( 24.91150772114469092, 179.0643266524160424, 9.188101187500095079 ) ) ;
#51981 = CARTESIAN_POINT ( 'NONE',  ( 111.3514947884964670, 235.0958772461660544, -9.188101187500095079 ) ) ;
#51982 = CARTESIAN_POINT ( 'NONE',  ( -19.65312891409030271, 93.06504152958497400, 177.5919119679930134 ) ) ;
#51983 = DIRECTION ( 'NONE',  ( -1.000000000000000000, -9.785293164109648193E-14, 0.000000000000000000 ) ) ;
#51984 = B_SPLINE_CURVE_WITH_KNOTS ( 'NONE', 3,
 ( #97252, #50119, #51098, #73432, #38259, #99597, #43504, #43989, #96760, #58211, #27328, #68672 ),
 .UNSPECIFIED., .F., .F.,
 ( 4, 2, 2, 2, 2, 4 ),
 ( 0.001395616302646774960, 0.001599850232781533516, 0.001804084162916292072, 0.002212552023185749769, 0.002621019883455207033, 0.003029487743724664298 ),
 .UNSPECIFIED. ) ;
#51985 = CARTESIAN_POINT ( 'NONE',  ( 78.91055811150361876, 55.69949448062589425, 16.11633552490014765 ) ) ;
#51986 = CARTESIAN_POINT ( 'NONE',  ( 177.5915495411956329, 283.6330961496328769, -15.30728232117395571 ) ) ;
#51987 = CARTESIAN_POINT ( 'NONE',  ( 189.9405379874402513, 299.8870043450095295, -5.547851184193374863 ) ) ;
#51988 = DIRECTION ( 'NONE',  ( 0.4999999999999992784, -0.8660254037844390407, 0.000000000000000000 ) ) ;
#51989 = CARTESIAN_POINT ( 'NONE',  ( 161.8668411317136986, 250.2854024296290447, -13.43522912998426655 ) ) ;
#51990 = CARTESIAN_POINT ( 'NONE',  ( 194.9636675848471441, 292.9600174435121289, -15.57898232594655319 ) ) ;
#51991 = CARTESIAN_POINT ( 'NONE',  ( 84.95191157424133621, 50.11551264433204267, 13.67402201518260441 ) ) ;
#51992 = CARTESIAN_POINT ( 'NONE',  ( 196.0051728737935832, 265.8263463907475170, 8.406970388261065352 ) ) ;
#51993 = CARTESIAN_POINT ( 'NONE',  ( 9.830230629461709668, 30.95267373526312227, 10.00000000000000000 ) ) ;
#51994 = CARTESIAN_POINT ( 'NONE',  ( 162.8384627734353387, 250.8402808221231624, -13.07578932517241732 ) ) ;
#51995 = CARTESIAN_POINT ( 'NONE',  ( 48.42933654300939139, 198.7677522451418781, 10.00000000000009592 ) ) ;
#51996 = CARTESIAN_POINT ( 'NONE',  ( 172.5032623719975220, 263.6776432955721816, -15.43083978726737726 ) ) ;
#51997 = CARTESIAN_POINT ( 'NONE',  ( 91.05385083941617097, 229.5024278399160949, -9.188101187500093303 ) ) ;
#51998 = CARTESIAN_POINT ( 'NONE',  ( 7.290083236948966317, 25.18502408145589655, 5.678558825948277544 ) ) ;
#51999 = CARTESIAN_POINT ( 'NONE',  ( 67.66477494612622934, 65.93994996590180335, 10.43000742999573838 ) ) ;
#52000 = CARTESIAN_POINT ( 'NONE',  ( 159.1193133772090675, 259.3124530707970052, -17.41573675653881637 ) ) ;
#52002 = CARTESIAN_POINT ( 'NONE',  ( 83.98768872710463995, 42.26923717846278095, -3.638105868026994649 ) ) ;
#52001 = CARTESIAN_POINT ( 'NONE',  ( 195.8449251089225811, 291.4336346372613775, 16.14492769602857081 ) ) ;
#52003 = LINE ( 'NONE', #46368, #4423 ) ;
#52004 = CARTESIAN_POINT ( 'NONE',  ( 199.0773057068961123, 285.8349872121713702, -17.17316764978006560 ) ) ;
#52005 = CARTESIAN_POINT ( 'NONE',  ( 80.07887604596260189, 44.31141191799963508, 11.46520868211218414 ) ) ;
#52006 = CARTESIAN_POINT ( 'NONE',  ( 38.63056705113294953, 37.70171378149921537, -9.188101187500004485 ) ) ;
#52007 = CARTESIAN_POINT ( 'NONE',  ( 147.0314375879888757, 275.9810751181479986, -5.168577011192616588 ) ) ;
#52008 = FACE_OUTER_BOUND ( 'NONE', #83232, .T. ) ;
#52009 = ORIENTED_EDGE ( 'NONE', *, *, #99095, .T. ) ;
#52010 = CARTESIAN_POINT ( 'NONE',  ( 20.80007953598619963, 32.98502408145593279, -5.678558825948271327 ) ) ;
#52012 = CARTESIAN_POINT ( 'NONE',  ( 180.2721358938293861, 265.6478004954673793, 15.92854085767422134 ) ) ;
#52011 = B_SPLINE_CURVE_WITH_KNOTS ( 'NONE', 3,
 ( #83475, #21162, #75866, #67742, #14041, #51030, #5448, #81986, #6445, #97669, #90597, #37324, #28236, #99148, #29735, #60610, #91564, #83981, #59112, #20653, #58623, #43434, #84474, #55016 ),
 .UNSPECIFIED., .F., .F.,
 ( 4, 2, 2, 2, 2, 2, 2, 2, 2, 2, 2, 4 ),
 ( 0.000000000000000000, 0.1250000000000062450, 0.2500000000000124900, 0.3750000000000187628, 0.4375000000000228151, 0.5000000000000268674, 0.5625000000000308642, 0.6250000000000348610, 0.6875000000000388578, 0.7500000000000429656, 0.8750000000000215383, 1.000000000000000000 ),
 .UNSPECIFIED. ) ;
#52013 = CARTESIAN_POINT ( 'NONE',  ( 147.4271219180435253, 275.2957297547342819, -3.800519706258907782 ) ) ;
#52014 = CARTESIAN_POINT ( 'NONE',  ( 188.2550976195534815, 286.0444469117322228, -16.18375812693026461 ) ) ;
#52015 = ORIENTED_EDGE ( 'NONE', *, *, #7772, .F. ) ;
#52016 = EDGE_CURVE ( 'NONE', #90285, #58638, #51141, .T. ) ;
#52017 = CARTESIAN_POINT ( 'NONE',  ( -23.73952538801239598, 24.43184193311134678, 10.00000000000000000 ) ) ;
#52018 = CARTESIAN_POINT ( 'NONE',  ( -2.590881078880516331, 25.17631125121048541, 177.5919119679930134 ) ) ;
#52019 = CARTESIAN_POINT ( 'NONE',  ( 155.6995334974659215, 267.8060086419009735, 15.80633252148572510 ) ) ;
#52020 = EDGE_CURVE ( 'NONE', #62608, #63400, #51659, .T. ) ;
#52021 = CARTESIAN_POINT ( 'NONE',  ( 170.4685145883027815, 252.7986105568807886, -8.763900896819295738 ) ) ;
#52022 = CARTESIAN_POINT ( 'NONE',  ( 143.4214980241629576, 243.6115022471902023, -5.000000000000041744 ) ) ;
#52023 = LINE ( 'NONE', #38160, #47225 ) ;
#52024 = EDGE_LOOP ( 'NONE', ( #77211, #77321, #22998, #39936 ) ) ;
#52025 = CARTESIAN_POINT ( 'NONE',  ( 85.18019808382288716, 46.01488486704433001, -10.22134979624012452 ) ) ;
#52026 = ORIENTED_EDGE ( 'NONE', *, *, #57421, .F. ) ;
#52027 = DIRECTION ( 'NONE',  ( 0.4999999999999992784, -0.8660254037844390407, 0.000000000000000000 ) ) ;
#52028 = CARTESIAN_POINT ( 'NONE',  ( 81.41513720620088179, 41.93548059953372587, -7.650316833348846934 ) ) ;
#52029 = ADVANCED_FACE ( 'NONE', ( #97774 ), #58247, .F. ) ;
#52030 = CARTESIAN_POINT ( 'NONE',  ( 87.65749775821140588, 44.27781399121202810, 3.602933735144415728 ) ) ;
#52031 = ORIENTED_EDGE ( 'NONE', *, *, #13280, .T. ) ;
#52032 = CARTESIAN_POINT ( 'NONE',  ( 167.5505310038667517, 261.6318463984700315, 17.07012949051403439 ) ) ;
#52033 = CARTESIAN_POINT ( 'NONE',  ( 158.5390849126119974, 256.0492452763162987, 17.54477686596875330 ) ) ;
#52034 = CARTESIAN_POINT ( 'NONE',  ( 84.64741752562134991, 50.25350151326510684, 13.85721388315136693 ) ) ;
#52035 = CARTESIAN_POINT ( 'NONE',  ( 204.0780454880880370, 272.9041813273606749, 11.05065144861194959 ) ) ;
#52036 = CARTESIAN_POINT ( 'NONE',  ( 152.9251141908703175, 265.7729277985770864, -16.20110192949203309 ) ) ;
#52037 = CARTESIAN_POINT ( 'NONE',  ( 88.33748333995926316, 44.07075497373335793, -2.898134731201833070 ) ) ;
#52038 = CARTESIAN_POINT ( 'NONE',  ( 36.24780089259745353, 32.87878583063844218, -9.188101187500006262 ) ) ;
#52039 = CARTESIAN_POINT ( 'NONE',  ( 80.35194745355103407, 44.33500143762700674, 11.34211166093983358 ) ) ;
#52040 = CARTESIAN_POINT ( 'NONE',  ( 71.50101329703264241, 60.99057979258904538, -14.67061923267852919 ) ) ;
#52041 = CARTESIAN_POINT ( 'NONE',  ( 173.6535785093707318, 257.7390071365238668, 13.58861338155497833 ) ) ;
#52042 = CARTESIAN_POINT ( 'NONE',  ( 190.2204363742943656, 300.4646209966566062, -1.328626404316530739E-11 ) ) ;
#52043 = ORIENTED_EDGE ( 'NONE', *, *, #55653, .T. ) ;
#52044 = VECTOR ( 'NONE', #59599, 1000.000000000000227 ) ;
#52045 = ORIENTED_EDGE ( 'NONE', *, *, #57233, .F. ) ;
#52046 = CARTESIAN_POINT ( 'NONE',  ( 180.9205682475781600, 274.4254913274602359, 17.80862408263999441 ) ) ;
#52048 = CARTESIAN_POINT ( 'NONE',  ( 162.2191009146380622, 272.3218988927615101, -16.01639894604743830 ) ) ;
#52047 = CARTESIAN_POINT ( 'NONE',  ( 174.4931704626366979, 257.1244136714613546, -12.18714520188626871 ) ) ;
#52049 = DIRECTION ( 'NONE',  ( -0.8660254037844387076, -0.4999999999999998890, -0.000000000000000000 ) ) ;
#52050 = DIRECTION ( 'NONE',  ( -0.06142469166374898287, -0.9981117208278906805, 0.000000000000000000 ) ) ;
#52051 = CARTESIAN_POINT ( 'NONE',  ( 201.8011112540905856, 277.2526834103201168, 15.54517447768417249 ) ) ;
#52052 = CARTESIAN_POINT ( 'NONE',  ( 82.45869220239580955, 40.41366995031415144, 0.9483679617909533954 ) ) ;
#52053 = CARTESIAN_POINT ( 'NONE',  ( 170.6405224136658489, 288.4786343240789392, -4.060171941529054251 ) ) ;
#52054 = CARTESIAN_POINT ( 'NONE',  ( 77.07149570696485341, 63.73492570656748057, -15.36167024187155228 ) ) ;
#52055 = CARTESIAN_POINT ( 'NONE',  ( 78.87398835131222086, 59.62348996268822532, 16.50394892759813459 ) ) ;
#52056 = CARTESIAN_POINT ( 'NONE',  ( 116.3854409958760385, 231.8768266524160140, -9.188101187500091527 ) ) ;
#52057 = ORIENTED_EDGE ( 'NONE', *, *, #92557, .T. ) ;
#52058 = CARTESIAN_POINT ( 'NONE',  ( 148.3413330264368710, 274.8204906787375990, -6.989116326937312884 ) ) ;
#52059 = CARTESIAN_POINT ( 'NONE',  ( 191.9162138939681483, 293.2888617811998415, -14.67284693752439217 ) ) ;
#52060 = EDGE_LOOP ( 'NONE', ( #49782, #18665, #4878, #79894 ) ) ;
#52061 = CYLINDRICAL_SURFACE ( 'NONE', #93506, 17.82106496071139645 ) ;
#52062 = DIRECTION ( 'NONE',  ( 0.3371987438498061929, -0.9414334852479556703, 0.000000000000000000 ) ) ;
#52063 = CARTESIAN_POINT ( 'NONE',  ( 195.7291534503633272, 291.6341570319625021, 16.44925029361851543 ) ) ;
#52064 = CARTESIAN_POINT ( 'NONE',  ( 34.04375301561599798, 21.78380873178788946, -6.180339887498949025 ) ) ;
#52065 = CARTESIAN_POINT ( 'NONE',  ( 13.51707852204697069, 30.73705186507753240, -3.090169943749475845 ) ) ;
#52066 = ORIENTED_EDGE ( 'NONE', *, *, #53150, .T. ) ;
#52067 = ORIENTED_EDGE ( 'NONE', *, *, #7066, .T. ) ;
#52068 = DIRECTION ( 'NONE',  ( -1.000000000000000000, 0.000000000000000000, 0.000000000000000000 ) ) ;
#52069 = ORIENTED_EDGE ( 'NONE', *, *, #4573, .F. ) ;
#52070 = FACE_OUTER_BOUND ( 'NONE', #7861, .T. ) ;
#52071 = CARTESIAN_POINT ( 'NONE',  ( -11.89580835203306997, 175.4860189848785410, -2.679491924311245832 ) ) ;
#52072 = ADVANCED_FACE ( 'NONE', ( #20267 ), #89226, .T. ) ;
#52073 = CARTESIAN_POINT ( 'NONE',  ( 67.06678242535858203, 68.82311105335894297, -3.689783056880661771 ) ) ;
#52075 = CARTESIAN_POINT ( 'NONE',  ( 69.50673298128731403, 63.05023952497469963, -13.62172798439030608 ) ) ;
#52074 = CARTESIAN_POINT ( 'NONE',  ( 186.5376491172117994, 290.3301725222095229, -13.38673431320972185 ) ) ;
#52076 = CARTESIAN_POINT ( 'NONE',  ( 201.3715986869907510, 281.8611552031986776, -17.89433714524984964 ) ) ;
#52077 = ORIENTED_EDGE ( 'NONE', *, *, #31466, .T. ) ;
#52078 = CARTESIAN_POINT ( 'NONE',  ( 190.4976253092930278, 300.6954295735222900, -5.764807383508308902 ) ) ;
#52079 = CARTESIAN_POINT ( 'NONE',  ( 82.21065643673749435, 50.51336489522484641, 14.24654085560588435 ) ) ;
#52080 = CARTESIAN_POINT ( 'NONE',  ( 190.0207397430023661, 264.2850639489738001, -9.260904495796658864 ) ) ;
#52081 = CARTESIAN_POINT ( 'NONE',  ( 173.6074067815649471, 251.0877831565759379, -1.045464715229854846 ) ) ;
#52082 = DIRECTION ( 'NONE',  ( 1.000000000000000000, 0.000000000000000000, -0.000000000000000000 ) ) ;
#52083 = EDGE_CURVE ( 'NONE', #40804, #50302, #20476, .T. ) ;
#52084 = CARTESIAN_POINT ( 'NONE',  ( -19.65312891409030271, 93.06504152958497400, 177.5919119679930134 ) ) ;
#52085 = CARTESIAN_POINT ( 'NONE',  ( 130.8844835975280887, 234.8262482093457493, 3.021315404115420679E-15 ) ) ;
#52086 = CARTESIAN_POINT ( 'NONE',  ( 79.69316575823049220, 48.95429064770711847, 14.15326268420492006 ) ) ;
#52087 = CARTESIAN_POINT ( 'NONE',  ( 69.54162092933202644, 70.29952225041016334, -3.646433943178841286 ) ) ;
#52088 = CARTESIAN_POINT ( 'NONE',  ( 60.68900866710680475, 205.8458772461660544, 9.188101187500095079 ) ) ;
#52089 = CARTESIAN_POINT ( 'NONE',  ( 206.7408728089182546, 272.5612996242556960, -10.63134519248043475 ) ) ;
#52090 = CARTESIAN_POINT ( 'NONE',  ( -13.11024591527723615, 27.99999999999999645, -32.50000000000017053 ) ) ;
#52091 = CARTESIAN_POINT ( 'NONE',  ( 178.6049202613385773, 292.1719165999419943, -5.671730975596174673 ) ) ;
#52092 = EDGE_CURVE ( 'NONE', #7443, #47283, #3618, .T. ) ;
#52093 = CARTESIAN_POINT ( 'NONE',  ( 207.8996209429610360, 270.5542889829179103, -5.987818313449536411 ) ) ;
#52094 = CARTESIAN_POINT ( 'NONE',  ( 160.7489855951974675, 254.2215850144021658, 15.85577744295692248 ) ) ;
#52096 = DIRECTION ( 'NONE',  ( 0.000000000000000000, 0.000000000000000000, -1.000000000000000000 ) ) ;
#52095 = CARTESIAN_POINT ( 'NONE',  ( 73.59487243717410365, 69.71703543845904960, -9.441731441278315984 ) ) ;
#52097 = SURFACE_STYLE_FILL_AREA ( #22708 ) ;
#52098 = CARTESIAN_POINT ( 'NONE',  ( 40.84394904227130496, 31.78052372038643725, -10.00000000000000355 ) ) ;
#52099 = CARTESIAN_POINT ( 'NONE',  ( 57.06414817410222895, 218.1868197944957330, 17.47570218321535762 ) ) ;
#52100 = CARTESIAN_POINT ( 'NONE',  ( 196.0034224882197975, 291.1591091234520263, 17.53794140922627776 ) ) ;
#52101 = CARTESIAN_POINT ( 'NONE',  ( 72.06396613292808695, 72.31755342346831128, 3.440598478083119804 ) ) ;
#52102 = CARTESIAN_POINT ( 'NONE',  ( 30.59497298136257726, 176.2202760586660020, -5.415160957724236172E-17 ) ) ;
#52103 = CARTESIAN_POINT ( 'NONE',  ( 196.4351339088274813, 290.4113630087520050, 17.20526457544535504 ) ) ;
#52104 = CARTESIAN_POINT ( 'NONE',  ( 81.49351603733306604, 42.61972550722757092, -7.674745181728958698 ) ) ;
#52105 = FACE_OUTER_BOUND ( 'NONE', #22233, .T. ) ;
#52106 = CARTESIAN_POINT ( 'NONE',  ( 72.09026212718839588, 72.27200742537389999, -1.505500128747980337 ) ) ;
#52107 = CARTESIAN_POINT ( 'NONE',  ( 46.94050828626381389, 210.1589784336661637, -6.496448406907676862E-16 ) ) ;
#52108 = CARTESIAN_POINT ( 'NONE',  ( 28.47099635789628280, 18.29860640527293114, -2.839279412974138328 ) ) ;
#52109 = CARTESIAN_POINT ( 'NONE',  ( 199.0773057068961123, 285.8349872121713702, -17.17316764978006560 ) ) ;
#52110 = CARTESIAN_POINT ( 'NONE',  ( 196.5114383562724072, 290.2791998289336561, -17.87308875047256862 ) ) ;
#52111 = CARTESIAN_POINT ( 'NONE',  ( 12.70933400901951416, 9.198606405272903075, 2.839279412974134775 ) ) ;
#52112 = CARTESIAN_POINT ( 'NONE',  ( 202.9443444632182434, 270.0342760574297358, -6.450216370591072668 ) ) ;
#52113 = CARTESIAN_POINT ( 'NONE',  ( 175.6179495818389000, 291.0503388302134340, 2.344001588397030655 ) ) ;
#52114 = CARTESIAN_POINT ( 'NONE',  ( 180.0951113711093114, 276.2838145191387298, 17.28842147576117938 ) ) ;
#52115 = CARTESIAN_POINT ( 'NONE',  ( 72.32152639495393487, 60.34245158586753632, 15.08100388408858272 ) ) ;
#52116 = CARTESIAN_POINT ( 'NONE',  ( 74.42984188155799075, 67.24162272381263961, -12.24555194031338701 ) ) ;
#52117 = CARTESIAN_POINT ( 'NONE',  ( 163.3226323906401376, 255.9179029620415804, -14.86657747175461886 ) ) ;
#52118 = CARTESIAN_POINT ( 'NONE',  ( 74.26842774264412128, 57.07890938945873671, -16.02166782049268789 ) ) ;
#52119 = CARTESIAN_POINT ( 'NONE',  ( 98.02733310912854847, 240.7365022471903444, 2.944929066748280225E-16 ) ) ;
#52120 = CARTESIAN_POINT ( 'NONE',  ( 172.7264208856190919, 290.8582626858774347, 2.771863430787652849 ) ) ;
#52121 = CARTESIAN_POINT ( 'NONE',  ( 194.6050500505458842, 285.5465367126718093, -17.70104686455487553 ) ) ;
#52122 = VERTEX_POINT ( 'NONE', #92680 ) ;
#52123 = CARTESIAN_POINT ( 'NONE',  ( 54.19381813872350762, 202.0958772461660544, -9.188101187500095079 ) ) ;
#52124 = ORIENTED_EDGE ( 'NONE', *, *, #75790, .T. ) ;
#52125 = ADVANCED_FACE ( 'NONE', ( #23232 ), #60295, .T. ) ;
#52126 = FACE_OUTER_BOUND ( 'NONE', #94172, .T. ) ;
#52127 = CARTESIAN_POINT ( 'NONE',  ( 146.8058449195592061, 276.3718130816831149, 4.181814292810413392 ) ) ;
#52128 = DIRECTION ( 'NONE',  ( 0.7071067811865462405, 0.000000000000000000, 0.7071067811865489050 ) ) ;
#52129 = EDGE_CURVE ( 'NONE', #14868, #51421, #51415, .T. ) ;
#52130 = ORIENTED_EDGE ( 'NONE', *, *, #83285, .F. ) ;
#52131 = DIRECTION ( 'NONE',  ( 0.5000000000000048850, -0.8660254037844358210, 0.000000000000000000 ) ) ;
#52132 = CARTESIAN_POINT ( 'NONE',  ( 79.15299089334158111, 45.92879069919392521, -13.14368370819105714 ) ) ;
#52133 = FACE_OUTER_BOUND ( 'NONE', #8373, .T. ) ;
#52134 = CARTESIAN_POINT ( 'NONE',  ( 176.7483101607716094, 274.5073097362626982, -16.69060033052792136 ) ) ;
#52135 = DIRECTION ( 'NONE',  ( 0.4827766168686632997, 0.5834231310750495059, -0.6531035050674843800 ) ) ;
#52136 = CARTESIAN_POINT ( 'NONE',  ( 157.1886094632603772, 258.3883373689681093, 18.40926891635499985 ) ) ;
#52138 = ORIENTED_EDGE ( 'NONE', *, *, #29834, .F. ) ;
#52137 = AXIS2_PLACEMENT_3D ( 'NONE', #58632, #89606, #81994 ) ;
#52139 = CARTESIAN_POINT ( 'NONE',  ( 26.24098094315136009, 17.01110640527292972, 2.839279412974134775 ) ) ;
#52140 = CARTESIAN_POINT ( 'NONE',  ( 76.51987890029035100, 63.61070592637643983, 14.91914813192731337 ) ) ;
#52141 = CARTESIAN_POINT ( 'NONE',  ( 71.31409814852831630, 70.28103913945014369, -6.532773565772590274 ) ) ;
#52142 = CARTESIAN_POINT ( 'NONE',  ( 75.31048316780064056, 66.81495650182517920, -12.93102085071238072 ) ) ;
#52143 = EDGE_LOOP ( 'NONE', ( #5684, #31883, #90109, #21878 ) ) ;
#52144 = DIRECTION ( 'NONE',  ( -0.8660254037844387076, -0.4999999999999998890, -0.000000000000000000 ) ) ;
#52145 = CARTESIAN_POINT ( 'NONE',  ( 168.4094709548043909, 262.4968943922261815, 16.00215286889127952 ) ) ;
#52146 = CARTESIAN_POINT ( 'NONE',  ( 206.0946696452135427, 273.6805563358039421, -10.19627505985792837 ) ) ;
#52147 = ORIENTED_EDGE ( 'NONE', *, *, #72532, .F. ) ;
#52149 = CARTESIAN_POINT ( 'NONE',  ( 57.52260328274599033, 204.0177522451418497, -10.00000000000009592 ) ) ;
#52148 = CARTESIAN_POINT ( 'NONE',  ( 70.34454795188869980, 61.29844696716961749, 14.78467410895967760 ) ) ;
#52150 = CARTESIAN_POINT ( 'NONE',  ( 162.7738416911812180, 248.7144313781379310, -11.09964294874192525 ) ) ;
#52151 = CARTESIAN_POINT ( 'NONE',  ( 66.12920851151632462, 68.57659062400610139, -2.240737289274019606 ) ) ;
#52152 = CARTESIAN_POINT ( 'NONE',  ( 188.6709712689815888, 295.3709411350409937, -11.33238897680398161 ) ) ;
#52153 = CARTESIAN_POINT ( 'NONE',  ( 154.8332767207531901, 280.7459370637686220, -0.9958211956073632631 ) ) ;
#52154 = CARTESIAN_POINT ( 'NONE',  ( 164.5265381092526695, 265.3812344335186140, -16.69521587732905843 ) ) ;
#52155 = CARTESIAN_POINT ( 'NONE',  ( 127.1025053677084742, 238.0643266524160424, -9.188101187500093303 ) ) ;
#52156 = VECTOR ( 'NONE', #2763, 1000.000000000000000 ) ;
#52157 = LINE ( 'NONE', #73990, #22991 ) ;
#52158 = ORIENTED_EDGE ( 'NONE', *, *, #51252, .T. ) ;
#52159 = CARTESIAN_POINT ( 'NONE',  ( 170.8702574392256111, 263.9852486083733538, 15.82437772357654993 ) ) ;
#52160 = CARTESIAN_POINT ( 'NONE',  ( 187.1230481695341439, 299.1666633132790594, 2.832346326993921082 ) ) ;
#52161 = ORIENTED_EDGE ( 'NONE', *, *, #8873, .T. ) ;
#52162 = CARTESIAN_POINT ( 'NONE',  ( 200.9622342365141208, 281.7300170448321524, 16.66537280693965783 ) ) ;
#52163 = ORIENTED_EDGE ( 'NONE', *, *, #4083, .F. ) ;
#52164 = ORIENTED_EDGE ( 'NONE', *, *, #23725, .F. ) ;
#52165 = CARTESIAN_POINT ( 'NONE',  ( 17.55280445478281592, 33.77154675864928635, -10.00000000000000000 ) ) ;
#52166 = CARTESIAN_POINT ( 'NONE',  ( 75.32621823817197537, 66.64820785908354139, -13.05086397426676648 ) ) ;
#52167 = CARTESIAN_POINT ( 'NONE',  ( 197.9354048063467246, 286.8717951656539640, 16.93488075601821308 ) ) ;
#52168 = CARTESIAN_POINT ( 'NONE',  ( 191.8453338867844877, 298.3611298435110371, -9.039024722281077118 ) ) ;
#52169 = CARTESIAN_POINT ( 'NONE',  ( 81.68833537920569654, 55.69874641368435420, 15.98167401408987587 ) ) ;
#52170 = CARTESIAN_POINT ( 'NONE',  ( 154.8556227199321427, 262.4291889417971788, 17.77326384500479861 ) ) ;
#52171 = CARTESIAN_POINT ( 'NONE',  ( 71.16602909547167144, 66.01008435473005420, 11.62282365756693103 ) ) ;
#52172 = ORIENTED_CLOSED_SHELL ( 'NONE', *, #78266, .F. );
#52173 = CARTESIAN_POINT ( 'NONE',  ( 87.43576499144317893, 45.00137247461037049, 6.922634181320210800 ) ) ;
#52174 = ORIENTED_EDGE ( 'NONE', *, *, #4780, .T. ) ;
#52175 = CARTESIAN_POINT ( 'NONE',  ( 200.6680263064462792, 283.0797783131037022, -17.21821073473145347 ) ) ;
#52176 = CARTESIAN_POINT ( 'NONE',  ( 155.1398527401465230, 261.9368881057492899, -17.02245700497956449 ) ) ;
#52177 = ORIENTED_EDGE ( 'NONE', *, *, #4992, .F. ) ;
#52178 = CARTESIAN_POINT ( 'NONE',  ( 206.9985020284622408, 270.1150727264914053, 3.388313042214953441 ) ) ;
#52179 = CARTESIAN_POINT ( 'NONE',  ( 76.13068126100937150, 51.50493480594106899, -15.67342808751774008 ) ) ;
#52180 = CARTESIAN_POINT ( 'NONE',  ( 174.4614454034193614, 253.2380414006159413, -7.790172112357452328 ) ) ;
#52181 = CARTESIAN_POINT ( 'NONE',  ( 164.2801755739368446, 246.1053845600426087, 2.518777461081745717 ) ) ;
#52182 = EDGE_CURVE ( 'NONE', #69479, #65130, #39807, .T. ) ;
#52183 = CARTESIAN_POINT ( 'NONE',  ( 195.1641141409822353, 279.2228943756692274, 16.33334675340180908 ) ) ;
#52184 = CARTESIAN_POINT ( 'NONE',  ( 208.2939409893161553, 269.8713066281881083, 2.523744790997269227 ) ) ;
#52185 = CARTESIAN_POINT ( 'NONE',  ( 139.2268610206906203, 245.0643266524160140, 9.188101187500095079 ) ) ;
#52186 = ORIENTED_EDGE ( 'NONE', *, *, #61524, .F. ) ;
#52187 = DIRECTION ( 'NONE',  ( 0.000000000000000000, 0.000000000000000000, 1.000000000000000000 ) ) ;
#52188 = CARTESIAN_POINT ( 'NONE',  ( 86.21660337353470993, 44.60933949929385989, 6.554422449840823006 ) ) ;
#52189 = EDGE_CURVE ( 'NONE', #62377, #759, #56703, .T. ) ;
#52190 = CARTESIAN_POINT ( 'NONE',  ( -19.65312891409030271, 93.06504152958497400, 59.99999999999999289 ) ) ;
#52191 = B_SPLINE_CURVE_WITH_KNOTS ( 'NONE', 3,
 ( #39132, #91906, #68060, #22462, #21962, #44746, #52855, #76191, #53357, #14854 ),
 .UNSPECIFIED., .F., .F.,
 ( 4, 2, 2, 2, 4 ),
 ( 0.000000000000000000, 0.2500000000000000000, 0.5000000000000000000, 0.7500000000000000000, 1.000000000000000000 ),
 .UNSPECIFIED. ) ;
#52192 = CARTESIAN_POINT ( 'NONE',  ( 72.99805664120070503, 70.78149395872682703, 8.185774945494653565 ) ) ;
#52193 = CARTESIAN_POINT ( 'NONE',  ( 178.5408147360961379, 254.5644880976646220, 4.355285803803885081 ) ) ;
#52194 = VERTEX_POINT ( 'NONE', #22009 ) ;
#52195 = CARTESIAN_POINT ( 'NONE',  ( 76.70704513412616166, 55.66840412848188890, 16.16585368749594664 ) ) ;
#52196 = CARTESIAN_POINT ( 'NONE',  ( 182.4010281170673693, 275.0942260036622429, -17.56270495112026708 ) ) ;
#52197 = CARTESIAN_POINT ( 'NONE',  ( 72.63019387209214983, 71.43162966861650887, -5.787168193185468823 ) ) ;
#52198 = CARTESIAN_POINT ( 'NONE',  ( 185.9727729040138797, 263.9344659017438630, -12.79113566482517328 ) ) ;
#52199 = CARTESIAN_POINT ( 'NONE',  ( 202.0157110946482248, 267.6599266906877119, 0.8488657683144487098 ) ) ;
#52200 = EDGE_CURVE ( 'NONE', #20252, #14275, #24502, .T. ) ;
#52201 = CARTESIAN_POINT ( 'NONE',  ( 190.1813752874636805, 301.2431906792259042, -4.710625539811892359 ) ) ;
#52202 = CARTESIAN_POINT ( 'NONE',  ( 70.92638144461730576, 71.59949221093340554, 0.8533387835500414464 ) ) ;
#52203 = B_SPLINE_CURVE_WITH_KNOTS ( 'NONE', 3,
 ( #36871, #99188, #46446, #98702 ),
 .UNSPECIFIED., .F., .F.,
 ( 4, 4 ),
 ( 0.004322650378965082335, 0.009836291497043285481 ),
 .UNSPECIFIED. ) ;
#52204 = VECTOR ( 'NONE', #32807, 1000.000000000000000 ) ;
#52205 = AXIS2_PLACEMENT_3D ( 'NONE', #58360, #81714, #36054 ) ;
#52206 = CARTESIAN_POINT ( 'NONE',  ( 193.0262075147481937, 268.6915971079139922, 12.26736561304707251 ) ) ;
#52208 = EDGE_CURVE ( 'NONE', #65003, #79412, #48270, .T. ) ;
#52207 = AXIS2_PLACEMENT_3D ( 'NONE', #36065, #77582, #31950 ) ;
#52209 = B_SPLINE_SURFACE_WITH_KNOTS ( 'NONE', 3, 1, ( 
 ( #95293, #56728 ),
 ( #25328, #32925 ),
 ( #31918, #9137 ),
 ( #49140, #93778 ),
 ( #23821, #62822 ),
 ( #24336, #16731 ),
 ( #80074, #55213 ),
 ( #63829, #86195 ),
 ( #56214, #31421 ),
 ( #40009, #39014 ),
 ( #535, #70949 ),
 ( #1552, #32435 ),
 ( #85695, #94271 ),
 ( #62310, #16234 ),
 ( #63330, #55701 ),
 ( #17221, #48128 ),
 ( #87211, #89200 ),
 ( #4029, #95788 ),
 ( #88694, #81567 ),
 ( #26342, #51112 ),
 ( #65813, #96270 ),
 ( #80581, #73938 ),
 ( #57218, #58221 ),
 ( #96774, #88193 ),
 ( #35918, #72961 ),
 ( #3553, #72463 ),
 ( #11160, #27829 ),
 ( #82077, #34915 ),
 ( #27340, #19748 ),
 ( #50613, #42027 ),
 ( #49626, #43517 ),
 ( #34431, #58705 ),
 ( #12138, #43000 ),
 ( #66330, #65331 ) ),
 .UNSPECIFIED., .T., .F., .F.,
 ( 4, 2, 2, 2, 2, 2, 2, 2, 2, 2, 2, 2, 2, 2, 2, 2, 4 ),
 ( 2, 2 ),
 ( 0.000000000000000000, 0.06250000000000000000, 0.1250000000000000000, 0.1875000000000000000, 0.2500000000000000000, 0.3125000000000000000, 0.3750000000000000000, 0.4375000000000000000, 0.5000000000000000000, 0.5625000000000000000, 0.6250000000000000000, 0.6875000000000000000, 0.7500000000000000000, 0.8125000000000000000, 0.8750000000000000000, 0.9375000000000000000, 1.000000000000000000 ),
 ( 0.000000000000000000, 1.000000000000000000 ),
 .UNSPECIFIED. ) ;
#52210 = CARTESIAN_POINT ( 'NONE',  ( 23.91155070014810136, 29.50829794293881392, -10.00000000000000355 ) ) ;
#52211 = EDGE_CURVE ( 'NONE', #98884, #30031, #37725, .T. ) ;
#52212 = CARTESIAN_POINT ( 'NONE',  ( -21.31413092498266693, 24.33771760303832465, 10.00000000000000000 ) ) ;
#52213 = CARTESIAN_POINT ( 'NONE',  ( 167.6010540021560189, 247.4270797612363708, 3.638657435017179864 ) ) ;
#52214 = CARTESIAN_POINT ( 'NONE',  ( 71.04154053766541210, 69.33027533991680968, -8.669517590967728893 ) ) ;
#52215 = CARTESIAN_POINT ( 'NONE',  ( 160.0105735053945182, 253.5005522708592594, 16.10371386499367929 ) ) ;
#52216 = CARTESIAN_POINT ( 'NONE',  ( 72.05072980389924453, 71.77788221706620675, -3.931438730150958349 ) ) ;
#52217 = CARTESIAN_POINT ( 'NONE',  ( 150.2594902713296676, 250.8927522451418213, 10.00000000000009592 ) ) ;
#52218 = CARTESIAN_POINT ( 'NONE',  ( 172.9107215740591244, 283.7979364891335194, -12.27551315198952331 ) ) ;
#52219 = VERTEX_POINT ( 'NONE', #37027 ) ;
#52220 = B_SPLINE_CURVE_WITH_KNOTS ( 'NONE', 3,
 ( #58578, #95149, #10504, #79943, #2419, #34785, #88066, #65201, #89077, #11523 ),
 .UNSPECIFIED., .F., .F.,
 ( 4, 2, 2, 2, 4 ),
 ( 0.000000000000000000, 0.0002622400424272841352, 0.0005244800848545682704, 0.0007867201272818524597, 0.001048960169709136541 ),
 .UNSPECIFIED. ) ;
#52222 = CARTESIAN_POINT ( 'NONE',  ( 66.71298768300009385, 67.40120186928047019, -6.723713196347710586 ) ) ;
#52221 = VECTOR ( 'NONE', #30588, 1000.000000000000000 ) ;
#52223 = CARTESIAN_POINT ( 'NONE',  ( 72.73113476598997806, 70.26322447592292519, -8.050895442633969168 ) ) ;
#52224 = CARTESIAN_POINT ( 'NONE',  ( 198.6363782946250183, 286.5986958926748116, -18.50260615857378355 ) ) ;
#52225 = CARTESIAN_POINT ( 'NONE',  ( 4.668163907683432257, 167.3768266524159856, -9.188101187500093303 ) ) ;
#52226 = CARTESIAN_POINT ( 'NONE',  ( 181.9027420907709143, 275.9322372300953816, -16.46933526673500126 ) ) ;
#52227 = CARTESIAN_POINT ( 'NONE',  ( 30.56436172585706146, 22.81029122506296147, 8.090169943749479842 ) ) ;
#52228 = LINE ( 'NONE', #83173, #25427 ) ;
#52229 = CARTESIAN_POINT ( 'NONE',  ( 6.499607544075114873, 41.35827422038750001, 59.99999999999999289 ) ) ;
#52230 = LINE ( 'NONE', #6137, #66209 ) ;
#52231 = FACE_OUTER_BOUND ( 'NONE', #75829, .T. ) ;
#52232 = B_SPLINE_SURFACE_WITH_KNOTS ( 'NONE', 3, 1, ( 
 ( #93245, #60784 ),
 ( #14223, #54689 ),
 ( #68902, #84166 ),
 ( #92265, #78024 ),
 ( #31897, #91250 ),
 ( #37499, #85673 ),
 ( #69413, #14712 ),
 ( #76527, #21814 ),
 ( #53693, #76044 ),
 ( #6624, #68406 ),
 ( #46091, #99334 ),
 ( #37990, #30413 ),
 ( #61303, #77003 ),
 ( #38498, #24 ),
 ( #32900, #17721 ),
 ( #3044, #95268 ),
 ( #94742, #32412 ),
 ( #10116, #42005 ),
 ( #40495, #24315 ),
 ( #2529, #33411 ),
 ( #63810, #71425 ),
 ( #48103, #48623 ),
 ( #16708, #49115 ),
 ( #55190, #71926 ),
 ( #86174, #25305 ),
 ( #47601, #78529 ),
 ( #87690, #25831 ),
 ( #9114, #72438 ),
 ( #72939, #70926 ),
 ( #26319, #64312 ),
 ( #3530, #11134 ),
 ( #62801, #56707 ),
 ( #56192, #39986 ),
 ( #93757, #18221 ) ),
 .UNSPECIFIED., .T., .F., .F.,
 ( 4, 2, 2, 2, 2, 2, 2, 2, 2, 2, 2, 2, 2, 2, 2, 2, 4 ),
 ( 2, 2 ),
 ( 0.000000000000000000, 0.06250000000000000000, 0.1250000000000000000, 0.1875000000000000000, 0.2500000000000000000, 0.3125000000000000000, 0.3750000000000000000, 0.4375000000000000000, 0.5000000000000000000, 0.5625000000000000000, 0.6250000000000000000, 0.6875000000000000000, 0.7500000000000000000, 0.8125000000000000000, 0.8750000000000000000, 0.9375000000000000000, 1.000000000000000000 ),
 ( 0.000000000000000000, 1.000000000000000000 ),
 .UNSPECIFIED. ) ;
#52233 = EDGE_CURVE ( 'NONE', #92904, #213, #38514, .T. ) ;
#52235 = CARTESIAN_POINT ( 'NONE',  ( 74.91528014208348907, 207.3927522451417929, 10.00000000000009592 ) ) ;
#52234 = CARTESIAN_POINT ( 'NONE',  ( 196.2760436623706823, 269.3890986055657208, -10.67377300597419776 ) ) ;
#52236 = CARTESIAN_POINT ( 'NONE',  ( 175.5289232728569004, 253.5710909141142224, -3.838295042954765979 ) ) ;
#52237 = CARTESIAN_POINT ( 'NONE',  ( 150.7108765041139691, 269.6080999720726936, 13.72660302980452407 ) ) ;
#52238 = EDGE_CURVE ( 'NONE', #62095, #53306, #7169, .T. ) ;
#52239 = CARTESIAN_POINT ( 'NONE',  ( 179.1211563714144859, 294.1662014525638256, 1.054073793073138532 ) ) ;
#52240 = CARTESIAN_POINT ( 'NONE',  ( 66.70608100559145726, 195.9865022471901455, 1.119607411625061291E-15 ) ) ;
#52241 = CARTESIAN_POINT ( 'NONE',  ( 84.55537670905214043, 50.62155581810766591, -14.09136642048689936 ) ) ;
#52242 = CARTESIAN_POINT ( 'NONE',  ( 190.3144310910409445, 301.0127312671879167, -1.334877248546042949 ) ) ;
#52243 = CARTESIAN_POINT ( 'NONE',  ( 15.38488118375084390, 185.8149278399160949, -9.188101187500095079 ) ) ;
#52244 = CARTESIAN_POINT ( 'NONE',  ( 164.2608904025049128, 285.0127816252062303, 4.307465260048421563 ) ) ;
#52245 = CARTESIAN_POINT ( 'NONE',  ( -56.29836151245349640, 34.88994676555962116, -10.00000000000000000 ) ) ;
#52246 = CARTESIAN_POINT ( 'NONE',  ( 33.90715327291019321, 42.68290643055189548, 3.479690158560446702E-15 ) ) ;
#52247 = DIRECTION ( 'NONE',  ( -0.9995486091367047354, 0.03004293549037833494, 0.000000000000000000 ) ) ;
#52248 = CARTESIAN_POINT ( 'NONE',  ( 165.0387478276132072, 244.7914988754632191, -2.473354058663827626 ) ) ;
#52249 = ADVANCED_FACE ( 'NONE', ( #69914 ), #70424, .T. ) ;
#52250 = CARTESIAN_POINT ( 'NONE',  ( 189.1815913259335105, 268.0942611344048032, 13.94827899188442721 ) ) ;
#52251 = CARTESIAN_POINT ( 'NONE',  ( 127.3796741259112792, 255.8967562850346553, -4.648177544792955347E-16 ) ) ;
#52252 = CARTESIAN_POINT ( 'NONE',  ( 160.7682838322721466, 280.9513019390540194, 9.562328407288063659 ) ) ;
#52253 = CARTESIAN_POINT ( 'NONE',  ( 16.17646586176480739, 17.84335787977762067, 9.188101187500006262 ) ) ;
#52254 = CARTESIAN_POINT ( 'NONE',  ( 116.4123307400877820, 248.0177522451419065, 5.000000000000046185 ) ) ;
#52255 = CARTESIAN_POINT ( 'NONE',  ( 82.61367695794857013, 54.13558619510798309, 15.54525242622692716 ) ) ;
#52256 = CARTESIAN_POINT ( 'NONE',  ( 71.39729339694994792, 59.37714758514961488, 15.71381503284779235 ) ) ;
#52257 = EDGE_CURVE ( 'NONE', #63007, #71681, #38565, .T. ) ;
#52258 = CARTESIAN_POINT ( 'NONE',  ( 155.0197698005585494, 262.1448778582381465, 18.42918111182112284 ) ) ;
#52259 = ORIENTED_EDGE ( 'NONE', *, *, #76177, .T. ) ;
#52260 = CARTESIAN_POINT ( 'NONE',  ( 184.6389624118809252, 290.5370850536020271, 12.15673895467454280 ) ) ;
#52261 = CARTESIAN_POINT ( 'NONE',  ( 79.96327294300282063, 46.17232751745272168, -12.99524731289856483 ) ) ;
#52262 = ADVANCED_FACE ( 'NONE', ( #25322 ), #28766, .F. ) ;
#52263 = CARTESIAN_POINT ( 'NONE',  ( 74.99593504773368124, 53.54266265287736815, -16.54118947238006854 ) ) ;
#52264 = CARTESIAN_POINT ( 'NONE',  ( 81.43085985942128957, 41.98340591695951218, 7.714366660622415495 ) ) ;
#52265 = ORIENTED_EDGE ( 'NONE', *, *, #50367, .F. ) ;
#52266 = CARTESIAN_POINT ( 'NONE',  ( 81.99104559367746958, 58.71166190940888185, -0.01744974835124876722 ) ) ;
#52267 = CARTESIAN_POINT ( 'NONE',  ( 70.22199747613832699, 222.8967562850346837, -4.648177544792955347E-16 ) ) ;
#52268 = CARTESIAN_POINT ( 'NONE',  ( 72.52170310386408403, 57.33936031854678106, 16.32555210529406153 ) ) ;
#52269 = CARTESIAN_POINT ( 'NONE',  ( 202.7973612924478743, 279.3916619310153919, -15.54732529288344089 ) ) ;
#52270 = ORIENTED_EDGE ( 'NONE', *, *, #65455, .F. ) ;
#52271 = VERTEX_POINT ( 'NONE', #35676 ) ;
#52273 = CARTESIAN_POINT ( 'NONE',  ( -27.42236680055714260, 166.5217562850347406, 1.224646799147364892E-15 ) ) ;
#52272 = DIRECTION ( 'NONE',  ( 0.4999999999999992784, -0.8660254037844390407, 0.000000000000000000 ) ) ;
#52274 = ORIENTED_EDGE ( 'NONE', *, *, #64311, .T. ) ;
#52275 = CARTESIAN_POINT ( 'NONE',  ( 150.6487462746963502, 269.7157126861102370, 15.18501655901553704 ) ) ;
#52276 = CARTESIAN_POINT ( 'NONE',  ( 84.14312167556933275, 48.98415679381830756, 0.000000000000000000 ) ) ;
#52277 = CARTESIAN_POINT ( 'NONE',  ( 80.41409615687595647, 57.98253562157035645, -16.60360993379744343 ) ) ;
#52278 = DIRECTION ( 'NONE',  ( 0.000000000000000000, 0.000000000000000000, -1.000000000000000000 ) ) ;
#52279 = ORIENTED_EDGE ( 'NONE', *, *, #67209, .T. ) ;
#52280 = CARTESIAN_POINT ( 'NONE',  ( -56.06787742410712383, 34.75406423768147590, -10.00000000000000000 ) ) ;
#52281 = ORIENTED_EDGE ( 'NONE', *, *, #22388, .T. ) ;
#52282 = CARTESIAN_POINT ( 'NONE',  ( 164.7297297678022403, 245.3267338555121455, 3.020078936458732599 ) ) ;
#52283 = CARTESIAN_POINT ( 'NONE',  ( 74.66885986973987599, 63.97112931501096256, 14.24837920079651887 ) ) ;
#52284 = ORIENTED_EDGE ( 'NONE', *, *, #63108, .T. ) ;
#52285 = CARTESIAN_POINT ( 'NONE',  ( 190.7805732161387766, 300.2053494229706985, 4.237982805666590025 ) ) ;
#52286 = CARTESIAN_POINT ( 'NONE',  ( 172.2019080879319120, 264.1397931956042271, -16.46918750876103132 ) ) ;
#52287 = VECTOR ( 'NONE', #70832, 1000.000000000000000 ) ;
#52288 = ORIENTED_EDGE ( 'NONE', *, *, #5435, .T. ) ;
#52289 = CARTESIAN_POINT ( 'NONE',  ( 158.6117737028674242, 274.9709143987748803, -12.58280590594613813 ) ) ;
#52290 = DIRECTION ( 'NONE',  ( -0.8279987035736638967, -0.5607300124661883656, 0.000000000000000000 ) ) ;
#52291 = CARTESIAN_POINT ( 'NONE',  ( -19.65312891409030271, 93.06504152958497400, 10.00000000000000888 ) ) ;
#52292 = ORIENTED_EDGE ( 'NONE', *, *, #68143, .F. ) ;
#52293 = ORIENTED_EDGE ( 'NONE', *, *, #44210, .T. ) ;
#52294 = CARTESIAN_POINT ( 'NONE',  ( 73.43067314555278813, 69.84183981607019120, 9.192079101480102210 ) ) ;
#52296 = VECTOR ( 'NONE', #19023, 1000.000000000000114 ) ;
#52295 = CARTESIAN_POINT ( 'NONE',  ( 168.9434124915611903, 272.5888371849330838, 17.32495137616924907 ) ) ;
#52297 = CARTESIAN_POINT ( 'NONE',  ( 190.9559560067148425, 299.9015775189195665, -4.895152914295826108 ) ) ;
#52298 = CARTESIAN_POINT ( 'NONE',  ( 188.4285301707691076, 298.9031352353757711, -5.166013069444586492 ) ) ;
#52299 = DIRECTION ( 'NONE',  ( 0.4999999999999992784, -0.8660254037844390407, 0.000000000000000000 ) ) ;
#52300 = CARTESIAN_POINT ( 'NONE',  ( 192.4202172926039793, 297.3654025762033370, 10.98569444949570872 ) ) ;
#52301 = CARTESIAN_POINT ( 'NONE',  ( 191.4524900926791702, 299.0415552543392437, 8.268219431103382533 ) ) ;
#52302 = CARTESIAN_POINT ( 'NONE',  ( 191.3041230083617563, 299.2985345825480863, -9.819045872446528378 ) ) ;
#52303 = AXIS2_PLACEMENT_3D ( 'NONE', #60315, #69432, #13264 ) ;
#52304 = ORIENTED_EDGE ( 'NONE', *, *, #74823, .F. ) ;
#52305 = CARTESIAN_POINT ( 'NONE',  ( 72.70796915197145438, 58.43460131349139175, -15.66698973594322197 ) ) ;
#52306 = CARTESIAN_POINT ( 'NONE',  ( 30.83758659773572575, 40.73705186507756082, -3.090169943749475845 ) ) ;
#52308 = CARTESIAN_POINT ( 'NONE',  ( -54.45295541630240166, 33.76759809053437067, 10.00000000000000000 ) ) ;
#52307 = CARTESIAN_POINT ( 'NONE',  ( 196.8104339078508076, 289.7613243423628546, -16.40335862274955403 ) ) ;
#52309 = CARTESIAN_POINT ( 'NONE',  ( 21.15788363470973366, 37.74176219324819215, -10.00000000000000000 ) ) ;
#52310 = CARTESIAN_POINT ( 'NONE',  ( 170.6717880471474871, 287.9187896612353370, 4.129465665201498936 ) ) ;
#52311 = CARTESIAN_POINT ( 'NONE',  ( 168.8244094625508751, 257.0541383169796745, -14.93690306707719628 ) ) ;
#52312 = VERTEX_POINT ( 'NONE', #75683 ) ;
#52313 = CARTESIAN_POINT ( 'NONE',  ( 149.2693755472542136, 272.1048528685130350, -13.07444463944290547 ) ) ;
#52314 = CARTESIAN_POINT ( 'NONE',  ( 75.40682597281998767, 54.41795888520695001, -16.12013989205779296 ) ) ;
#52315 = CARTESIAN_POINT ( 'NONE',  ( 202.6833006059332263, 277.5892208352050829, 15.45935665133711900 ) ) ;
#52316 = CARTESIAN_POINT ( 'NONE',  ( 79.70436563710978817, 46.00489109485927486, 12.97891914157378679 ) ) ;
#52317 = DIRECTION ( 'NONE',  ( -0.8660254037844387076, -0.4999999999999998890, -0.000000000000000000 ) ) ;
#52318 = DIRECTION ( 'NONE',  ( -0.9825923819316307872, -0.1857746241280658905, 0.000000000000000000 ) ) ;
#52319 = VERTEX_POINT ( 'NONE', #13389 ) ;
#52320 = CARTESIAN_POINT ( 'NONE',  ( 170.7306893209106988, 255.3552208224515425, -12.88177093387596450 ) ) ;
#52321 = DIRECTION ( 'NONE',  ( 0.9946578707245736783, 0.1032265479692960342, 0.000000000000000000 ) ) ;
#52322 = CARTESIAN_POINT ( 'NONE',  ( 207.3502731283117555, 271.5057873089173768, 6.280625384230454245 ) ) ;
#52323 = CARTESIAN_POINT ( 'NONE',  ( 47.99632384111720995, 188.5177522451417929, 5.000000000000051514 ) ) ;
#52324 = CARTESIAN_POINT ( 'NONE',  ( 123.8009570636627785, 230.0327760586659451, 1.948934522072302763E-15 ) ) ;
#52325 = EDGE_CURVE ( 'NONE', #44408, #47896, #28070, .T. ) ;
#52326 = CARTESIAN_POINT ( 'NONE',  ( 180.4629368410562620, 294.6297622202381490, -3.542282447166476445 ) ) ;
#52327 = CARTESIAN_POINT ( 'NONE',  ( 156.9763224152064822, 271.9908631200777904, -15.29896765642516776 ) ) ;
#52328 = CARTESIAN_POINT ( 'NONE',  ( 103.2234855318352373, 223.7365022471902023, -10.00000000000009237 ) ) ;
#52329 = CARTESIAN_POINT ( 'NONE',  ( 173.7730331013573277, 252.4040569639470846, -3.903565288969256475 ) ) ;
#52330 = CARTESIAN_POINT ( 'NONE',  ( 43.63930707798317599, 189.8768266524159856, -9.188101187500091527 ) ) ;
#52331 = CARTESIAN_POINT ( 'NONE',  ( 147.8030175879119099, 276.3716628640393651, -2.406150248769625133 ) ) ;
#52332 = ORIENTED_EDGE ( 'NONE', *, *, #23907, .F. ) ;
#52333 = CARTESIAN_POINT ( 'NONE',  ( 190.4867865949766781, 299.1946217176854930, 7.408943446041265979 ) ) ;
#52334 = CARTESIAN_POINT ( 'NONE',  ( 180.6467591333264409, 267.4216841736908350, 15.01138547461691530 ) ) ;
#52335 = EDGE_CURVE ( 'NONE', #41077, #24776, #51866, .T. ) ;
#52336 = CARTESIAN_POINT ( 'NONE',  ( 69.94542627262927681, 71.02953153408785170, -0.005637359706063728958 ) ) ;
#52337 = EDGE_CURVE ( 'NONE', #22391, #77084, #60266, .T. ) ;
#52338 = CARTESIAN_POINT ( 'NONE',  ( 146.8195026170398023, 276.3481572557323034, 4.765869558735466249 ) ) ;
#52339 = CARTESIAN_POINT ( 'NONE',  ( 81.85412157328340754, 41.19605074857211946, -5.694832249283913406 ) ) ;
#52340 = CYLINDRICAL_SURFACE ( 'NONE', #17144, 16.60714546451156792 ) ;
#52341 = CARTESIAN_POINT ( 'NONE',  ( -15.31269525828471068, 104.2312461070085021, 45.19948692389422717 ) ) ;
#52342 = CARTESIAN_POINT ( 'NONE',  ( 68.48351335520325733, 64.33043610559428771, -12.33486862999595601 ) ) ;
#52343 = CARTESIAN_POINT ( 'NONE',  ( 105.1540004908901693, 221.5177522451418213, 5.000000000000051514 ) ) ;
#52344 = VERTEX_POINT ( 'NONE', #55217 ) ;
#52345 = CARTESIAN_POINT ( 'NONE',  ( 195.0119942166254248, 266.5109991209683358, -7.745506184336903743 ) ) ;
#52346 = CARTESIAN_POINT ( 'NONE',  ( 155.2511492336869310, 280.0303029816861908, -2.338817866916156785 ) ) ;
#52347 = CARTESIAN_POINT ( 'NONE',  ( 154.4564338973504789, 263.9603729957919995, 16.89342759845790809 ) ) ;
#52348 = CLOSED_SHELL ( 'NONE', ( #49198, #36063, #6735, #68783, #97478, #57939, #66269, #45442, #12960, #85855, #1502, #79496, #29363, #15853, #45545, #56561, #42618, #75835, #47058, #67238, #77027, #76630, #84078, #43046, #70613, #73703, #7158, #40789, #40600, #61476, #22780, #2170, #28058, #2775, #12353, #33627, #2120, #91695, #8305, #72787, #4503, #37830, #67290, #71769, #43957, #19976, #12854, #63995, #6677, #18157, #95755, #59364, #49114, #42059, #41860, #4010, #82902, #27673, #1618, #41363, #82381, #83122, #26749, #44246, #59797, #2077, #97972, #63598, #50299, #52445, #94838, #98806, #28290, #85135, #81036, #88125, #16013, #70856, #33995, #66877, #80808, #31761, #71501, #3165, #91986, #49146, #75413, #53395, #23038, #57847, #75783, #61693, #13045, #51102, #85396, #87556, #91793, #39508, #1440, #87756, #58509, #60014, #12225, #4088, #84882, #66005, #84196, #48039, #92122, #67775, #57252, #4008, #40347, #49383, #24364, #6725, #68189, #61678, #18182, #13768, #86272, #4134, #56348, #10182, #1326, #51825, #96265, #16102, #59803, #7284, #76350, #32705, #56620, #61270, #29042, #98087, #32237, #64178, #72589, #94978, #52828, #24908, #69080, #25500, #65385, #66434, #4339, #67812, #32441, #83869, #5818, #64697, #83166, #14482, #62272, #77212, #76383, #88475, #47600, #70216, #99108, #43830, #35150, #61144, #10301, #54760, #36079, #48694, #77244, #21279, #92374, #22834, #82141, #70597, #64566, #96559, #52896, #57, #69606, #28831, #60406, #53025, #17147, #30070, #31082, #42495, #77289, #2634, #32106, #84384, #65268, #49497, #70193, #66067, #82611, #79799, #86373, #31825, #86611, #27776, #68027, #55491, #75530, #55975, #36891, #88673, #25442, #94499, #66685, #59432, #98148, #5041, #33259, #225, #52777, #39739, #27785, #83678, #85546, #88185, #7866, #38642, #38167, #90638, #58189, #79228, #31645, #9581, #1032, #57976, #20716, #97005, #21047, #92237, #18333, #9784, #5843, #70850, #37873, #8558, #93129, #14426, #42966, #38465, #26256, #46730, #96509, #90298, #79978, #95780, #13835, #58311, #42959, #32878, #61640, #16314, #25638, #12087, #79031, #44101, #2769, #55256, #72055, #71429, #86047, #51326, #25958, #62065, #82562, #18982, #56231, #30726, #81484, #48555, #49711, #62018, #23757, #100137, #45870, #15974, #95094, #74422, #47776, #10070, #54900, #22190, #58801, #84763, #9721, #928, #94516, #90462, #491, #39142, #30289, #28320, #41086, #83996, #55442, #71827, #64059, #85363, #63806, #5266, #89195, #39308, #50298, #48952, #17197, #26280, #64368, #87835, #12610, #50536, #2721, #45014, #7046, #82247, #81347, #2400, #46294, #49915, #344, #35103, #32741, #96283, #5356, #73336, #31294, #59143, #22406, #39060, #54769, #99210, #23284, #65505, #16224, #98468, #8243, #79109, #42485, #33042, #47572, #25426, #90156, #4657, #8351, #31134, #77286, #33179, #43576, #44623, #35639, #90693, #48751, #27089, #20012, #94650, #50418, #90712, #58624, #31139, #18651, #93459, #7995, #90741, #78000, #78759, #96218, #25158, #9564, #43314, #71615, #66282, #74180, #5692, #57453, #98694, #14156, #67112, #51717, #100207, #77754, #7632, #86215, #82501, #48425, #63437, #71055, #52818, #91831, #6210, #27945, #22642, #6468, #11785, #46589, #48038, #49349, #29838, #92753, #44996, #3417, #20220, #50317, #95204, #83180, #80818, #44807, #6520, #3468, #61448, #68078, #59305, #79368, #30587, #48942, #35194, #89981, #85655, #2044, #7533, #57669, #18065, #27094, #25717, #11720, #53814, #37467, #15848, #55517, #42418, #52262, #47337, #36783, #70187, #40594, #83293, #88306, #94024, #69218, #63098, #39365, #20801, #89491, #21263, #39769, #77503, #57404, #42621, #35777, #4397, #85724, #37532, #56483, #6531, #67526, #33920, #82392, #76408, #35576, #39241, #53161, #15881, #3231, #73394, #87766, #45496, #49443, #43, #60446, #86056, #19609, #84427, #89602, #43990, #72724, #65425, #72904, #4452, #12425, #79188, #79659, #71191, #8665, #81437, #76937, #1588, #82868, #74410, #10751, #65009, #6466, #4257, #41026, #86406, #23785, #44403, #21599, #13388, #23150, #61130, #85953, #24929, #82395, #95157, #78560, #37635, #29510, #69152, #63463, #31929, #8221, #14040, #31376, #13265, #99292 ) ) ;
#52349 = CARTESIAN_POINT ( 'NONE',  ( 11.29875767934929520, 168.1423013555409796, -4.594050593750043987 ) ) ;
#52350 = CARTESIAN_POINT ( 'NONE',  ( 68.72758243515100673, 68.85043676914649780, -7.310471056669800127 ) ) ;
#52351 = CARTESIAN_POINT ( 'NONE',  ( -15.81198528973881778, 105.8575200343950229, 44.14166339942401152 ) ) ;
#52352 = CARTESIAN_POINT ( 'NONE',  ( 71.90368585207026797, 59.31677128024832513, -15.31322431433719800 ) ) ;
#52353 = DIRECTION ( 'NONE',  ( -0.06442261589617466477, -0.9979227057047523886, 0.000000000000000000 ) ) ;
#52355 = CARTESIAN_POINT ( 'NONE',  ( 43.17879721251643588, 204.9244531367911293, -4.594050593750046652 ) ) ;
#52354 = CARTESIAN_POINT ( 'NONE',  ( 196.2529602075856303, 276.1688732195831335, -15.37645340877904232 ) ) ;
#52356 = CARTESIAN_POINT ( 'NONE',  ( 207.8060684685902686, 270.7163266217015689, 2.015725026008670540 ) ) ;
#52357 = CARTESIAN_POINT ( 'NONE',  ( 73.13084643241136007, 57.37954916538377148, 15.88987484405033435 ) ) ;
#52358 = CARTESIAN_POINT ( 'NONE',  ( 71.07628154480391913, 71.06296950484041020, 4.311319492879813531 ) ) ;
#52359 = CARTESIAN_POINT ( 'NONE',  ( 66.13815982364135948, 68.48623413791136727, -4.821830553978275091 ) ) ;
#52360 = ORIENTED_EDGE ( 'NONE', *, *, #37387, .F. ) ;
#52361 = VECTOR ( 'NONE', #95335, 1000.000000000000227 ) ;
#52362 = EDGE_CURVE ( 'NONE', #89390, #50887, #64847, .T. ) ;
#52363 = CARTESIAN_POINT ( 'NONE',  ( 4.352251933111777049, 179.9865022471903160, -10.00000000000009415 ) ) ;
#52364 = CARTESIAN_POINT ( 'NONE',  ( 164.4989226152910646, 245.7265035704120351, -6.575810094723514965 ) ) ;
#52365 = CIRCLE ( 'NONE', #45916, 17.82106496071138224 ) ;
#52366 = CARTESIAN_POINT ( 'NONE',  ( 133.7599021114188247, 248.0333772461660544, 9.188101187500095079 ) ) ;
#52367 = CARTESIAN_POINT ( 'NONE',  ( 28.47099635789628280, 18.29860640527293114, -2.839279412974138328 ) ) ;
#52368 = CARTESIAN_POINT ( 'NONE',  ( 207.4128166479680999, 271.3974587551883246, -8.231682050742898937 ) ) ;
#52369 = CARTESIAN_POINT ( 'NONE',  ( 83.82342001511069896, 52.04024975599947567, -14.96847033955516260 ) ) ;
#52370 = EDGE_CURVE ( 'NONE', #69971, #22854, #77346, .T. ) ;
#52371 = LINE ( 'NONE', #60455, #9310 ) ;
#52372 = AXIS2_PLACEMENT_3D ( 'NONE', #12158, #27357, #89219 ) ;
#52374 = CARTESIAN_POINT ( 'NONE',  ( 186.1237447414861208, 288.2118312591220501, 14.66121385500803243 ) ) ;
#52373 = CARTESIAN_POINT ( 'NONE',  ( 88.13962338646859962, 43.88173199026378057, 2.505344897735778620 ) ) ;
#52375 = ADVANCED_FACE ( 'NONE', ( #88699 ), #19270, .F. ) ;
#52376 = CARTESIAN_POINT ( 'NONE',  ( 69.03268662160444080, 64.48878135178121340, 12.45710446990803000 ) ) ;
#52377 = ORIENTED_EDGE ( 'NONE', *, *, #91127, .F. ) ;
#52378 = CARTESIAN_POINT ( 'NONE',  ( 150.7226148805041817, 269.5877685077668957, 15.52819754351937576 ) ) ;
#52379 = CARTESIAN_POINT ( 'NONE',  ( 208.4117778882290395, 269.6672071322645934, -0.9948548485616270920 ) ) ;
#52380 = DIRECTION ( 'NONE',  ( -0.3473291852295006810, 0.6015917957689992379, 0.7193398003386451967 ) ) ;
#52381 = CARTESIAN_POINT ( 'NONE',  ( 171.6540594275769820, 267.3410371765079958, -16.37976297547299254 ) ) ;
#52382 = CARTESIAN_POINT ( 'NONE',  ( 197.2267182245235801, 273.1434563419713868, -13.38223132498687740 ) ) ;
#52383 = EDGE_LOOP ( 'NONE', ( #23876, #61375, #95746, #48696, #56526 ) ) ;
#52384 = CARTESIAN_POINT ( 'NONE',  ( 70.37731676418549398, 69.40210544723913699, 7.051632179388870547 ) ) ;
#52385 = LINE ( 'NONE', #81837, #58722 ) ;
#52386 = ADVANCED_FACE ( 'NONE', ( #13152 ), #65919, .T. ) ;
#52387 = LINE ( 'NONE', #61960, #26347 ) ;
#52388 = CARTESIAN_POINT ( 'NONE',  ( 196.3539419194680704, 270.6706703227201842, 13.29218896581975962 ) ) ;
#52389 = DIRECTION ( 'NONE',  ( -0.3473291852295006810, 0.6015917957689992379, 0.7193398003386451967 ) ) ;
#52390 = CARTESIAN_POINT ( 'NONE',  ( 68.62404369657433278, 69.88680614121496149, 3.169402490526867844 ) ) ;
#52391 = FACE_OUTER_BOUND ( 'NONE', #75244, .T. ) ;
#52392 = CARTESIAN_POINT ( 'NONE',  ( 190.8353261179822766, 280.9707072899906848, 16.64952221345274808 ) ) ;
#52393 = CARTESIAN_POINT ( 'NONE',  ( 17.56085832715719164, 11.10801979619927948, 3.090169943749476733 ) ) ;
#52394 = CARTESIAN_POINT ( 'NONE',  ( 83.73797956718067326, 47.25317760063183670, 12.19094957233783738 ) ) ;
#52395 = VERTEX_POINT ( 'NONE', #35819 ) ;
#52396 = CARTESIAN_POINT ( 'NONE',  ( 79.14312167556931854, 57.64441083166269664, 0.000000000000000000 ) ) ;
#52397 = CARTESIAN_POINT ( 'NONE',  ( 86.35458572345136474, 46.97350791603361131, -10.52386536561717811 ) ) ;
#52398 = CARTESIAN_POINT ( 'NONE',  ( 80.47941278984953328, 45.63198079188786238, -11.75349558557117469 ) ) ;
#52399 = ORIENTED_EDGE ( 'NONE', *, *, #30655, .F. ) ;
#52400 = LINE ( 'NONE', #74741, #606 ) ;
#52401 = CARTESIAN_POINT ( 'NONE',  ( 179.0685761320505947, 258.5468394390073286, -11.57600102548048149 ) ) ;
#52402 = CARTESIAN_POINT ( 'NONE',  ( 204.6780326111993986, 276.1342436545999703, 14.85609018352459287 ) ) ;
#52403 = CARTESIAN_POINT ( 'NONE',  ( 74.81496871025450446, 53.36391971156190550, 16.05853747727076453 ) ) ;
#52404 = ORIENTED_EDGE ( 'NONE', *, *, #90618, .T. ) ;
#52405 = CARTESIAN_POINT ( 'NONE',  ( 94.43719644265542001, 216.1423013555410080, -4.594050593750043987 ) ) ;
#52406 = CARTESIAN_POINT ( 'NONE',  ( 155.0836044121125212, 262.0343130677450745, 18.31269374395214200 ) ) ;
#52407 = CARTESIAN_POINT ( 'NONE',  ( 67.34378090123340144, 69.79098680214323736, 2.519322243948931561 ) ) ;
#52408 = CARTESIAN_POINT ( 'NONE',  ( 81.62852022226142878, 42.64977674016488152, -7.599251380822039437 ) ) ;
#52409 = EDGE_LOOP ( 'NONE', ( #96441, #50404, #91097, #83948 ) ) ;
#52410 = ORIENTED_EDGE ( 'NONE', *, *, #35652, .F. ) ;
#52411 = VERTEX_POINT ( 'NONE', #66714 ) ;
#52412 = DIRECTION ( 'NONE',  ( -0.5000000000000002220, 0.8660254037844384856, 0.000000000000000000 ) ) ;
#52414 = VERTEX_POINT ( 'NONE', #13535 ) ;
#52413 = EDGE_CURVE ( 'NONE', #42773, #99043, #29716, .T. ) ;
#52415 = CARTESIAN_POINT ( 'NONE',  ( 76.20055470335279324, 65.09253202017347917, 14.18943646504600054 ) ) ;
#52416 = ORIENTED_EDGE ( 'NONE', *, *, #33375, .T. ) ;
#52417 = CARTESIAN_POINT ( 'NONE',  ( 164.3990608653545848, 245.8994691950343565, 2.256889790035259136 ) ) ;
#52418 = CARTESIAN_POINT ( 'NONE',  ( 82.66777534764520396, 40.88273136510965600, 3.288167606857240521 ) ) ;
#52420 = ADVANCED_FACE ( 'NONE', ( #84455 ), #53054, .T. ) ;
#52419 = DIRECTION ( 'NONE',  ( -0.7886751345948271874, 0.2113248654051755882, -0.5773502691896106320 ) ) ;
#52421 = CARTESIAN_POINT ( 'NONE',  ( -23.43310877838089112, 99.78231651504889044, 45.19940739266792207 ) ) ;
#52422 = CARTESIAN_POINT ( 'NONE',  ( 66.75966942117048575, 68.13366762939419630, -5.218020817821980017 ) ) ;
#52423 = CARTESIAN_POINT ( 'NONE',  ( 165.0952605416836718, 264.4120569475813340, -17.48790325852768746 ) ) ;
#52424 = ORIENTED_EDGE ( 'NONE', *, *, #8357, .F. ) ;
#52425 = CARTESIAN_POINT ( 'NONE',  ( 198.8683739244561082, 276.4215138120039796, -15.93986209720707414 ) ) ;
#52426 = CARTESIAN_POINT ( 'NONE',  ( 8.697374518098678564, 25.99752408145590366, 5.678558825948277544 ) ) ;
#52427 = ORIENTED_EDGE ( 'NONE', *, *, #60429, .T. ) ;
#52428 = CARTESIAN_POINT ( 'NONE',  ( 164.2034818126556388, 281.6578577422810099, 8.819376076490621941 ) ) ;
#52430 = EDGE_LOOP ( 'NONE', ( #41417, #42899, #209, #46400 ) ) ;
#52429 = LINE ( 'NONE', #13942, #65454 ) ;
#52431 = CARTESIAN_POINT ( 'NONE',  ( 202.4323889586180201, 280.0238125565655878, 15.69595176008160919 ) ) ;
#52432 = CARTESIAN_POINT ( 'NONE',  ( 188.1054269039565554, 260.7416112581689731, 2.841567442216401229 ) ) ;
#52433 = CARTESIAN_POINT ( 'NONE',  ( 160.7588997986945856, 282.5491429314030825, -6.341079064894056927 ) ) ;
#52434 = CARTESIAN_POINT ( 'NONE',  ( 79.79559376127615167, 44.73722406975080190, 11.30977224791904057 ) ) ;
#52435 = DIRECTION ( 'NONE',  ( -0.000000000000000000, -0.000000000000000000, 1.000000000000000000 ) ) ;
#52436 = AXIS2_PLACEMENT_3D ( 'NONE', #72085, #71589, #95432 ) ;
#52437 = CARTESIAN_POINT ( 'NONE',  ( 171.3610447788964848, 255.5874900960222078, 11.20421736224005471 ) ) ;
#52438 = CARTESIAN_POINT ( 'NONE',  ( 157.7190474710035062, 281.4620898344580837, 1.428472196222973389 ) ) ;
#52439 = ORIENTED_EDGE ( 'NONE', *, *, #40547, .F. ) ;
#52440 = CARTESIAN_POINT ( 'NONE',  ( 194.4754212959730353, 293.8056848224490523, -15.50536285337042486 ) ) ;
#52441 = CARTESIAN_POINT ( 'NONE',  ( 72.49894385216839510, 63.03176572407281952, -14.06401512292728206 ) ) ;
#52442 = CARTESIAN_POINT ( 'NONE',  ( 193.8271347420676420, 294.1030254116506626, -14.13191673250339164 ) ) ;
#52443 = CARTESIAN_POINT ( 'NONE',  ( -4.903394573382326094, 174.6427522451419350, -10.00000000000009415 ) ) ;
#52445 = ADVANCED_FACE ( 'NONE', ( #54739 ), #70455, .T. ) ;
#52444 = VECTOR ( 'NONE', #59731, 1000.000000000000114 ) ;
#52446 = CARTESIAN_POINT ( 'NONE',  ( 194.2120287517171846, 268.3159770147244103, -10.84597068469714110 ) ) ;
#52447 = CARTESIAN_POINT ( 'NONE',  ( 174.6775312387305519, 281.2009762962929358, -14.18005191487551997 ) ) ;
#52448 = CARTESIAN_POINT ( 'NONE',  ( 163.3833816344594538, 247.6586772271373889, -8.552920238416389154 ) ) ;
#52449 = CARTESIAN_POINT ( 'NONE',  ( 173.2717237769409451, 287.6101323724053032, -10.33903262687377023 ) ) ;
#52450 = CARTESIAN_POINT ( 'NONE',  ( 161.0428786693140637, 272.6820104255564274, 15.30257686379266602 ) ) ;
#52452 = CARTESIAN_POINT ( 'NONE',  ( -6.467605121757557640, 178.6199935810940929, 2.679491924311251605 ) ) ;
#52451 = CARTESIAN_POINT ( 'NONE',  ( -6.102853504003019403, 155.0327760586659451, 1.948934522072303157E-15 ) ) ;
#52453 = CARTESIAN_POINT ( 'NONE',  ( 185.8119420094102168, 295.3841422132845196, 8.236304765045641574 ) ) ;
#52454 = VERTEX_POINT ( 'NONE', #47148 ) ;
#52455 = VERTEX_POINT ( 'NONE', #7659 ) ;
#52456 = DIRECTION ( 'NONE',  ( -0.9825427565607343094, 0.1860369090531061309, 0.000000000000000000 ) ) ;
#52457 = CARTESIAN_POINT ( 'NONE',  ( 170.8054577101068219, 287.4915981561377976, 8.526299399445241178 ) ) ;
#52458 = ADVANCED_FACE ( 'NONE', ( #61843 ), #97524, .T. ) ;
#52459 = CARTESIAN_POINT ( 'NONE',  ( 175.1279731406782787, 290.6895847248729865, 2.563404365050127698 ) ) ;
#52460 = CYLINDRICAL_SURFACE ( 'NONE', #85812, 10.00000000000010658 ) ;
#52461 = ADVANCED_FACE ( 'NONE', ( #63785 ), #32389, .F. ) ;
#52462 = DIRECTION ( 'NONE',  ( -0.5000000000000019984, 0.8660254037844374864, 0.000000000000000000 ) ) ;
#52463 = CARTESIAN_POINT ( 'NONE',  ( 84.20940321838243392, 46.16460512702312258, 10.34873203983212164 ) ) ;
#52464 = CARTESIAN_POINT ( 'NONE',  ( 150.2998784792504807, 276.6058365846234324, 3.694584881749327643 ) ) ;
#52465 = CARTESIAN_POINT ( 'NONE',  ( 28.37560933628243731, 181.0643266524159856, -9.188101187500093303 ) ) ;
#52466 = CARTESIAN_POINT ( 'NONE',  ( 120.4447615282330588, 240.3458772461660544, 9.188101187500095079 ) ) ;
#52467 = LINE ( 'NONE', #83412, #35373 ) ;
#52468 = LINE ( 'NONE', #83919, #54425 ) ;
#52469 = CARTESIAN_POINT ( 'NONE',  ( 79.07729678290289144, 56.72051478397521862, 16.18859796109226679 ) ) ;
#52470 = CARTESIAN_POINT ( 'NONE',  ( 178.4791421146993571, 283.9042546283926072, -14.94796090157607971 ) ) ;
#52471 = CARTESIAN_POINT ( 'NONE',  ( 69.21394623383595501, 200.7677522451417929, -5.000000000000041744 ) ) ;
#52472 = PLANE ( 'NONE',  #64723 ) ;
#52473 = CARTESIAN_POINT ( 'NONE',  ( 183.9255502157922422, 275.0530541881162776, 16.36233669867407414 ) ) ;
#52474 = CYLINDRICAL_SURFACE ( 'NONE', #64554, 70.00000000000002842 ) ;
#52475 = DIRECTION ( 'NONE',  ( 0.1384676192453727639, -0.9903669614948382716, 0.000000000000000000 ) ) ;
#52476 = CARTESIAN_POINT ( 'NONE',  ( 84.43483225515912238, 50.68154273191345283, 13.76020688952911364 ) ) ;
#52477 = CARTESIAN_POINT ( 'NONE',  ( 186.8181860056460550, 298.9265138730379476, -0.6012193119006525865 ) ) ;
#52478 = CARTESIAN_POINT ( 'NONE',  ( 46.83931157395847578, 209.3967562850346837, 1.101618078115930403E-13 ) ) ;
#52479 = CARTESIAN_POINT ( 'NONE',  ( 64.52297529667023923, 201.3927522451418213, 10.00000000000009948 ) ) ;
#52480 = DIRECTION ( 'NONE',  ( 0.000000000000000000, -0.000000000000000000, -1.000000000000000000 ) ) ;
#52481 = ADVANCED_FACE ( 'NONE', ( #56168 ), #96228, .F. ) ;
#52482 = CARTESIAN_POINT ( 'NONE',  ( 181.8281974864600272, 268.1150286880662748, 15.00885672120805481 ) ) ;
#52483 = CARTESIAN_POINT ( 'NONE',  ( 94.00418374076319594, 215.8923013555410080, 4.594050593750050204 ) ) ;
#52484 = CARTESIAN_POINT ( 'NONE',  ( 161.8882824960653579, 250.2482648971885340, -13.83574485983625557 ) ) ;
#52485 = CARTESIAN_POINT ( 'NONE',  ( 68.22205435738101187, 65.90345407221148832, 10.80313017757570826 ) ) ;
#52486 = CARTESIAN_POINT ( 'NONE',  ( 157.8230096946041954, 258.6542051802886135, -16.94987972545947841 ) ) ;
#52488 = CARTESIAN_POINT ( 'NONE',  ( 152.5108720042611026, 266.4904163124226670, 16.32854172121686531 ) ) ;
#52487 = CARTESIAN_POINT ( 'NONE',  ( 157.8740713127050981, 257.2010826190796706, 17.31862062017425075 ) ) ;
#52489 = CARTESIAN_POINT ( 'NONE',  ( 201.1851683271005413, 270.3619535279936485, -10.11376747734130532 ) ) ;
#52490 = CARTESIAN_POINT ( 'NONE',  ( -22.42236680055709641, 157.8615022471902591, 0.000000000000000000 ) ) ;
#52491 = CARTESIAN_POINT ( 'NONE',  ( 173.4606779374792325, 267.5814416807811540, -17.58000433512257032 ) ) ;
#52492 = CARTESIAN_POINT ( 'NONE',  ( 40.74993669414823216, 32.03085787977766330, 9.188101187500006262 ) ) ;
#52493 = CARTESIAN_POINT ( 'NONE',  ( 147.4323331177958494, 275.2867036919951147, -5.064030047414062707 ) ) ;
#52494 = FACE_BOUND ( 'NONE', #25546, .T. ) ;
#52495 = ORIENTED_EDGE ( 'NONE', *, *, #87890, .F. ) ;
#52496 = CARTESIAN_POINT ( 'NONE',  ( 22.44070990177030112, 31.14336893147756413, 7.433330006724141015 ) ) ;
#52497 = CARTESIAN_POINT ( 'NONE',  ( 156.3709700504638818, 275.5026625584495719, -12.72272160619075088 ) ) ;
#52498 = CARTESIAN_POINT ( 'NONE',  ( 147.4563929227680603, 275.2450308873625886, -3.847749617713808412 ) ) ;
#52499 = CARTESIAN_POINT ( 'NONE',  ( 149.3801359649374092, 271.9130101976182914, -11.41245530317637424 ) ) ;
#52500 = VERTEX_POINT ( 'NONE', #20198 ) ;
#52501 = CARTESIAN_POINT ( 'NONE',  ( 70.58272931436614783, 60.86286632090516235, 14.50022832024369279 ) ) ;
#52502 = CARTESIAN_POINT ( 'NONE',  ( 75.80192922086310148, 65.84738460970490337, -14.09986028324621898 ) ) ;
#52503 = CIRCLE ( 'NONE', #89790, 70.00000000000001421 ) ;
#52504 = CARTESIAN_POINT ( 'NONE',  ( 22.01921768174555893, 36.21091486745860522, -1.111400068045478839E-16 ) ) ;
#52505 = CARTESIAN_POINT ( 'NONE',  ( 173.0163677133065789, 253.2660320162962080, -9.300034630933833313 ) ) ;
#52506 = CARTESIAN_POINT ( 'NONE',  ( 75.15191903146568109, 52.97183600650499358, -16.48001256439864903 ) ) ;
#52507 = CARTESIAN_POINT ( 'NONE',  ( 148.6176504468695896, 246.6115022471902023, -5.000000000000041744 ) ) ;
#52508 = ORIENTED_EDGE ( 'NONE', *, *, #80079, .F. ) ;
#52509 = CARTESIAN_POINT ( 'NONE',  ( 86.94711308317737064, 232.5530062829863027, -4.648177544792955347E-16 ) ) ;
#52510 = ORIENTED_EDGE ( 'NONE', *, *, #16007, .F. ) ;
#52511 = CARTESIAN_POINT ( 'NONE',  ( 163.1332433029523372, 248.0919295262283981, 11.24052392390482957 ) ) ;
#52512 = FACE_OUTER_BOUND ( 'NONE', #51807, .T. ) ;
#52513 = EDGE_LOOP ( 'NONE', ( #59234, #29663, #55717, #62610, #54804, #95520, #17909, #87999, #86681, #86629, #50628, #12367, #66406, #82385, #56285, #20035, #91966, #27767, #84245, #62778 ) ) ;
#52514 = CARTESIAN_POINT ( 'NONE',  ( 184.8823494725930345, 293.3934917266262232, -10.47977162542887797 ) ) ;
#52516 = VERTEX_POINT ( 'NONE', #97705 ) ;
#52515 = VECTOR ( 'NONE', #57221, 1000.000000000000000 ) ;
#52517 = PLANE ( 'NONE',  #29611 ) ;
#52518 = PLANE ( 'NONE',  #20081 ) ;
#52519 = CARTESIAN_POINT ( 'NONE',  ( 190.6920532893590234, 278.3349890342503272, -16.61725499987922916 ) ) ;
#52520 = CARTESIAN_POINT ( 'NONE',  ( 153.4580622222703710, 264.8498347303985838, -17.93314668316356375 ) ) ;
#52521 = CARTESIAN_POINT ( 'NONE',  ( 152.8651171364917900, 265.8768457450651113, -16.25664868183201861 ) ) ;
#52522 = EDGE_CURVE ( 'NONE', #44273, #74117, #26792, .T. ) ;
#52523 = CARTESIAN_POINT ( 'NONE',  ( 33.72069078606260462, 37.65586893147758474, -7.433330006724137462 ) ) ;
#52524 = CARTESIAN_POINT ( 'NONE',  ( 149.2341712975190546, 276.7904698848887506, 4.784570376893943155 ) ) ;
#52525 = CARTESIAN_POINT ( 'NONE',  ( -32.97666635132488011, 94.88921800892812541, 43.93259070532314325 ) ) ;
#52526 = LINE ( 'NONE', #35841, #4388 ) ;
#52527 = EDGE_LOOP ( 'NONE', ( #29622, #48119, #19824, #43259 ) ) ;
#52528 = ORIENTED_EDGE ( 'NONE', *, *, #26131, .F. ) ;
#52529 = LINE ( 'NONE', #83984, #47457 ) ;
#52530 = CARTESIAN_POINT ( 'NONE',  ( 81.09122451980682911, 42.49663464562407711, 7.855986980898610916 ) ) ;
#52531 =( BOUNDED_CURVE ( )  B_SPLINE_CURVE ( 2, ( #96836, #97810, #28378, #89737, #66389 ),
 .UNSPECIFIED., .F., .T. ) 
 B_SPLINE_CURVE_WITH_KNOTS ( ( 3, 2, 3 ),
 ( 0.000000000000000000, 0.002688172043010752903, 0.004032258064516129788 ),
 .UNSPECIFIED. ) 
 CURVE ( )  GEOMETRIC_REPRESENTATION_ITEM ( )  RATIONAL_B_SPLINE_CURVE ( ( 1.000000000000000000, 0.8660254037844387076, 1.000000000000000000, 0.9330127018922194093, 0.9330127018922194093 ) ) 
 REPRESENTATION_ITEM ( '' )  );
#52533 = CARTESIAN_POINT ( 'NONE',  ( 162.3275777969640785, 272.2924995007368238, -15.82782416072089582 ) ) ;
#52532 = CARTESIAN_POINT ( 'NONE',  ( 164.3961040135806968, 245.9045906125373904, 7.095190383188031191 ) ) ;
#52534 = CARTESIAN_POINT ( 'NONE',  ( 164.8329707752360491, 245.1479151852119855, -0.9471001479485156027 ) ) ;
#52535 = CARTESIAN_POINT ( 'NONE',  ( 68.51164798075079432, 68.66491985411187216, 7.416875103192704266 ) ) ;
#52536 = CARTESIAN_POINT ( 'NONE',  ( 148.0427192501136062, 274.2294838985851015, 9.385226820296049155 ) ) ;
#52537 = CARTESIAN_POINT ( 'NONE',  ( 167.8377799047650853, 286.2760919531912123, -4.720521751261225418 ) ) ;
#52538 = CARTESIAN_POINT ( 'NONE',  ( 77.23555989339968164, 62.99091516456967099, -15.27956704681999156 ) ) ;
#52539 = B_SPLINE_CURVE_WITH_KNOTS ( 'NONE', 3,
 ( #6323, #68610, #6818, #45795 ),
 .UNSPECIFIED., .F., .F.,
 ( 4, 4 ),
 ( 0.009431354028234023926, 0.01481778605290438866 ),
 .UNSPECIFIED. ) ;
#52540 = CARTESIAN_POINT ( 'NONE',  ( 185.8250471888061099, 286.2195783377563316, -15.25737745182902927 ) ) ;
#52541 = CARTESIAN_POINT ( 'NONE',  ( 114.4904897814500515, 249.1589784336661069, -6.496448406907675876E-16 ) ) ;
#52542 = CARTESIAN_POINT ( 'NONE',  ( 183.6651092691634801, 260.0572973937465804, -9.581159380197425079 ) ) ;
#52543 = CARTESIAN_POINT ( 'NONE',  ( 31.37760429443829224, 33.51421378149921537, -9.188101187500004485 ) ) ;
#52544 = CARTESIAN_POINT ( 'NONE',  ( 189.2781344870356861, 274.0445645723327743, 15.70124837302617316 ) ) ;
#52545 = ORIENTED_EDGE ( 'NONE', *, *, #87317, .F. ) ;
#52546 = AXIS2_PLACEMENT_3D ( 'NONE', #77708, #54877, #30092 ) ;
#52547 = CARTESIAN_POINT ( 'NONE',  ( 74.09769653082098273, 68.87686179987508694, -11.21282387169916284 ) ) ;
#52548 = CARTESIAN_POINT ( 'NONE',  ( 164.8050118924691958, 246.2012700071148572, -2.717544611603450733 ) ) ;
#52549 = CARTESIAN_POINT ( 'NONE',  ( 157.1837449796689725, 258.3967629017010381, 16.97243084443542216 ) ) ;
#52550 = DIRECTION ( 'NONE',  ( -0.9923183454821322691, -0.1237105541964931832, 0.000000000000000000 ) ) ;
#52551 = CARTESIAN_POINT ( 'NONE',  ( 21.91939736263385541, 14.78380873178786636, -6.180339887498949025 ) ) ;
#52552 = VERTEX_POINT ( 'NONE', #74414 ) ;
#52553 = FACE_OUTER_BOUND ( 'NONE', #98399, .T. ) ;
#52554 = ORIENTED_EDGE ( 'NONE', *, *, #47452, .F. ) ;
#52555 = DIRECTION ( 'NONE',  ( -0.000000000000000000, -0.000000000000000000, -1.000000000000000000 ) ) ;
#52556 = ORIENTED_EDGE ( 'NONE', *, *, #61642, .F. ) ;
#52557 = CARTESIAN_POINT ( 'NONE',  ( 205.9240884482826175, 273.9760116357041966, 10.27504561427317142 ) ) ;
#52558 = CARTESIAN_POINT ( 'NONE',  ( 195.6450799796529054, 265.3427675445001910, 4.393462682352039295 ) ) ;
#52559 = CARTESIAN_POINT ( 'NONE',  ( -15.31269525828471068, 104.2312461070085021, 45.19948692389422717 ) ) ;
#52560 = CARTESIAN_POINT ( 'NONE',  ( 83.31942950123568892, 47.18081731595467687, 11.75718208460381220 ) ) ;
#52562 = CYLINDRICAL_SURFACE ( 'NONE', #41472, 17.82106496071139645 ) ;
#52561 = FACE_OUTER_BOUND ( 'NONE', #27792, .T. ) ;
#52563 = CARTESIAN_POINT ( 'NONE',  ( 199.1744935446041893, 274.6029352898955267, -14.95876376616611125 ) ) ;
#52564 = VERTEX_POINT ( 'NONE', #4999 ) ;
#52565 = CARTESIAN_POINT ( 'NONE',  ( 157.2674082780516471, 258.2518538181732879, 18.34755329151241554 ) ) ;
#52566 = CARTESIAN_POINT ( 'NONE',  ( -42.72532191160158987, 28.29708160126037697, -10.00000000000000000 ) ) ;
#52567 = CARTESIAN_POINT ( 'NONE',  ( 82.28788541374279930, 41.26664830668678974, -3.453415047302514029 ) ) ;
#52568 = CARTESIAN_POINT ( 'NONE',  ( 170.0871025661366787, 249.0337905125704765, -0.2639721576281350846 ) ) ;
#52569 = CARTESIAN_POINT ( 'NONE',  ( 191.9809540880537497, 271.5427279282940276, -14.38588033665278410 ) ) ;
#52570 = EDGE_CURVE ( 'NONE', #72875, #1030, #48013, .T. ) ;
#52571 = CARTESIAN_POINT ( 'NONE',  ( 72.00818181938288376, 72.30390281540809383, 3.363530094501221424 ) ) ;
#52572 = AXIS2_PLACEMENT_3D ( 'NONE', #60499, #68117, #13448 ) ;
#52573 = DIRECTION ( 'NONE',  ( -1.000000000000000000, 0.000000000000000000, 0.000000000000000000 ) ) ;
#52574 = ADVANCED_FACE ( 'NONE', ( #35876 ), #57674, .F. ) ;
#52575 = LINE ( 'NONE', #44977, #88417 ) ;
#52576 = CARTESIAN_POINT ( 'NONE',  ( 191.1760382422123428, 283.2354439422711039, -16.61270921724900518 ) ) ;
#52577 = CARTESIAN_POINT ( 'NONE',  ( 82.71327011143105779, 53.60354310397067934, -15.74390733313335566 ) ) ;
#52578 = EDGE_CURVE ( 'NONE', #93829, #59249, #16683, .T. ) ;
#52579 = CARTESIAN_POINT ( 'NONE',  ( 85.88519558028406209, 211.2048013555409796, 4.594050593750051981 ) ) ;
#52580 = CARTESIAN_POINT ( 'NONE',  ( 206.6298919378964740, 272.7535241315335384, -9.267551915974392429 ) ) ;
#52581 = CARTESIAN_POINT ( 'NONE',  ( 77.71677981826302073, 61.99014014597172206, 15.64018103715309316 ) ) ;
#52582 = DIRECTION ( 'NONE',  ( -0.7763215174174871169, 0.6303371332823493045, 0.000000000000000000 ) ) ;
#52583 = EDGE_CURVE ( 'NONE', #46006, #73115, #8255, .T. ) ;
#52584 = AXIS2_PLACEMENT_3D ( 'NONE', #41660, #80728, #4162 ) ;
#52585 = CARTESIAN_POINT ( 'NONE',  ( 161.5083988044524119, 250.9062427520286178, -14.53522982831775856 ) ) ;
#52586 = DIRECTION ( 'NONE',  ( -0.9506327454577433445, -0.3103181967972122313, 0.000000000000000000 ) ) ;
#52588 = CARTESIAN_POINT ( 'NONE',  ( 79.58936028502597537, 59.22294857574253513, 16.56770033466462166 ) ) ;
#52587 = CARTESIAN_POINT ( 'NONE',  ( 108.7544814380518403, 222.0494855054051868, -2.679491924311248496 ) ) ;
#52589 = CARTESIAN_POINT ( 'NONE',  ( 43.71482552144721723, 26.20801979619932354, -3.090169943749474069 ) ) ;
#52590 = CARTESIAN_POINT ( 'NONE',  ( 182.5686778644665083, 296.6873302901632314, 1.787712280751329708 ) ) ;
#52591 = CARTESIAN_POINT ( 'NONE',  ( 82.67645095449901760, 54.06173429938865382, 15.51329239322386577 ) ) ;
#52592 = CARTESIAN_POINT ( 'NONE',  ( 72.26106983447931498, 71.98033296937877878, 3.564000903169437517 ) ) ;
#52593 = CARTESIAN_POINT ( 'NONE',  ( 22.39418752168989712, 192.9244531367911293, -4.594050593750046652 ) ) ;
#52594 = DIRECTION ( 'NONE',  ( 1.000000000000000000, 0.000000000000000000, 0.000000000000000000 ) ) ;
#52595 = CARTESIAN_POINT ( 'NONE',  ( 81.34288284027337568, 42.53142883239708993, -7.672663453570639724 ) ) ;
#52596 = DIRECTION ( 'NONE',  ( -0.07193265315671491800, 0.9974094913373522386, 0.000000000000000000 ) ) ;
#52597 = CARTESIAN_POINT ( 'NONE',  ( 40.45322629432754269, 23.75978393459168458, -1.583844403245396437 ) ) ;
#52598 = CARTESIAN_POINT ( 'NONE',  ( 56.25097556847656932, 191.0327760586659451, 1.948934522072302763E-15 ) ) ;
#52599 = AXIS2_PLACEMENT_3D ( 'NONE', #12231, #4113, #28404 ) ;
#52600 = CARTESIAN_POINT ( 'NONE',  ( 19.06802872841732110, 31.98502408145592568, -5.678558825948271327 ) ) ;
#52601 = DIRECTION ( 'NONE',  ( -0.4999999999999987788, 0.8660254037844392627, 0.000000000000000000 ) ) ;
#52602 = CARTESIAN_POINT ( 'NONE',  ( -6.813555604197667037, 155.3262482093457777, -6.972266317189433020E-16 ) ) ;
#52603 = CARTESIAN_POINT ( 'NONE',  ( 43.20833262110986084, 30.11029122506297995, -8.090169943749478065 ) ) ;
#52604 = CARTESIAN_POINT ( 'NONE',  ( 204.8878784573704195, 275.7707799872745795, -14.13380496213581594 ) ) ;
#52605 = CARTESIAN_POINT ( 'NONE',  ( 197.7454084947095225, 287.3707299168542590, 17.08123495905502764 ) ) ;
#52606 = CARTESIAN_POINT ( 'NONE',  ( -14.22851846967002487, 105.1940860163543476, 43.89948692389422291 ) ) ;
#52607 = CARTESIAN_POINT ( 'NONE',  ( 180.0410653043650484, 276.3720869110510421, 17.51637908678287303 ) ) ;
#52608 = CARTESIAN_POINT ( 'NONE',  ( 73.58277243495972186, 65.12260290344103453, 13.28827523339052696 ) ) ;
#52609 = CARTESIAN_POINT ( 'NONE',  ( 153.1402462294643385, 276.7372565758790302, 7.179079264927311854 ) ) ;
#52610 = CARTESIAN_POINT ( 'NONE',  ( 163.3011861648808178, 256.0630655445800130, -14.91776478601246048 ) ) ;
#52611 = FACE_OUTER_BOUND ( 'NONE', #88854, .T. ) ;
#52612 = CARTESIAN_POINT ( 'NONE',  ( 87.77567103309253582, 45.10408226285451150, -6.743331934586553444 ) ) ;
#52613 = CARTESIAN_POINT ( 'NONE',  ( 94.05805000844988228, 235.1115022471902876, -5.000000000000047962 ) ) ;
#52614 = CARTESIAN_POINT ( 'NONE',  ( 161.1611771195837548, 251.5076483517112536, 14.17749514252127163 ) ) ;
#52615 = CARTESIAN_POINT ( 'NONE',  ( 194.7136160084532719, 285.5689873031276989, -17.40128518539645697 ) ) ;
#52616 = ORIENTED_EDGE ( 'NONE', *, *, #33215, .T. ) ;
#52617 = CARTESIAN_POINT ( 'NONE',  ( 66.15596757637857195, 202.8768266524160140, 9.188101187500098632 ) ) ;
#52618 = VERTEX_POINT ( 'NONE', #19218 ) ;
#52619 = CARTESIAN_POINT ( 'NONE',  ( 185.5568049818104726, 266.1438378612298834, 14.60334785453874140 ) ) ;
#52620 = CARTESIAN_POINT ( 'NONE',  ( 190.3625087333586521, 300.9294583479858147, -4.271886578030237303 ) ) ;
#52621 = CARTESIAN_POINT ( 'NONE',  ( -22.42236680055709641, 157.8615022471902591, 0.000000000000000000 ) ) ;
#52622 = ORIENTED_EDGE ( 'NONE', *, *, #64617, .F. ) ;
#52623 = CARTESIAN_POINT ( 'NONE',  ( 9.827979128326980174, 29.57595373812807082, 10.00000000000000000 ) ) ;
#52624 = CARTESIAN_POINT ( 'NONE',  ( 79.36263291412585374, 45.67866562560195831, -12.88899626214226579 ) ) ;
#52625 = LINE ( 'NONE', #59214, #2291 ) ;
#52626 = LINE ( 'NONE', #83584, #7721 ) ;
#52627 = CARTESIAN_POINT ( 'NONE',  ( 206.9068930164517894, 271.8479423001995769, -5.981710879645867784 ) ) ;
#52628 = EDGE_CURVE ( 'NONE', #34863, #59430, #90119, .T. ) ;
#52629 = CARTESIAN_POINT ( 'NONE',  ( 204.8467418195402843, 275.8420307340491036, 13.15258587511997135 ) ) ;
#52630 = ORIENTED_EDGE ( 'NONE', *, *, #71134, .T. ) ;
#52631 = CARTESIAN_POINT ( 'NONE',  ( 16.40018271037384068, 27.65586893147755987, -7.433330006724137462 ) ) ;
#52632 = CARTESIAN_POINT ( 'NONE',  ( 75.82607876426669691, 58.94255996486501914, 15.94889058982140995 ) ) ;
#52633 = CARTESIAN_POINT ( 'NONE',  ( 175.4496532655798262, 254.2869214701858880, 7.959120167633201071 ) ) ;
#52634 = CARTESIAN_POINT ( 'NONE',  ( 176.5950604002042326, 276.4255102086987108, 17.53915386444770519 ) ) ;
#52635 = ORIENTED_EDGE ( 'NONE', *, *, #30513, .T. ) ;
#52636 = CARTESIAN_POINT ( 'NONE',  ( -64.74139798177010618, 41.16849083240310847, 10.00000000000000000 ) ) ;
#52637 = CARTESIAN_POINT ( 'NONE',  ( 159.6962080797732710, 254.0450491601782232, -15.33973334987084947 ) ) ;
#52638 = AXIS2_PLACEMENT_3D ( 'NONE', #67368, #61256, #35965 ) ;
#52639 = ORIENTED_EDGE ( 'NONE', *, *, #20338, .F. ) ;
#52640 = ORIENTED_EDGE ( 'NONE', *, *, #45134, .F. ) ;
#52642 = CARTESIAN_POINT ( 'NONE',  ( -59.66199281916092900, 60.27061997932485582, 59.99999999999999289 ) ) ;
#52641 = CARTESIAN_POINT ( 'NONE',  ( 72.51499028565849869, 68.19712414860103422, 10.98850085807369048 ) ) ;
#52643 = CARTESIAN_POINT ( 'NONE',  ( 68.16895862681424489, 70.45982571230283042, -0.9782046817701681718 ) ) ;
#52644 = CARTESIAN_POINT ( 'NONE',  ( 204.7610021263893429, 275.9905362388115577, 13.36619428527026976 ) ) ;
#52645 = CARTESIAN_POINT ( 'NONE',  ( 159.9671766634011192, 253.5757178060795809, 16.49140845334465411 ) ) ;
#52646 = CARTESIAN_POINT ( 'NONE',  ( 81.43364589948765797, 55.81991725365188017, 16.38199963144059268 ) ) ;
#52647 = CARTESIAN_POINT ( 'NONE',  ( 164.4290154601662550, 264.9784679568533079, -16.63390713968286860 ) ) ;
#52648 = ADVANCED_FACE ( 'NONE', ( #34389 ), #51068, .F. ) ;
#52650 = CARTESIAN_POINT ( 'NONE',  ( 127.8056303646358032, 256.8464784336661637, 1.353441290958777525E-15 ) ) ;
#52649 = AXIS2_PLACEMENT_3D ( 'NONE', #96413, #13284, #3691 ) ;
#52651 = CARTESIAN_POINT ( 'NONE',  ( 160.2740869459746023, 254.0686150970925610, -15.36085255641610914 ) ) ;
#52652 = B_SPLINE_CURVE_WITH_KNOTS ( 'NONE', 3,
 ( #14344, #45718, #99456, #59927 ),
 .UNSPECIFIED., .F., .F.,
 ( 4, 4 ),
 ( 0.004744422519644171318, 0.01275308626033747235 ),
 .UNSPECIFIED. ) ;
#52653 = CARTESIAN_POINT ( 'NONE',  ( 68.75404378773190217, 204.3768266524160140, 9.188101187500098632 ) ) ;
#52654 = ORIENTED_EDGE ( 'NONE', *, *, #54389, .T. ) ;
#52656 = CARTESIAN_POINT ( 'NONE',  ( 174.1529052279448706, 265.6236375338058906, 16.55384635694815287 ) ) ;
#52655 = B_SPLINE_CURVE_WITH_KNOTS ( 'NONE', 3,
 ( #60346, #58370, #14271, #75094, #76101, #98396, #59349, #13771, #27971, #19899 ),
 .UNSPECIFIED., .F., .F.,
 ( 4, 2, 2, 2, 4 ),
 ( 0.000000000000000000, 0.0002622400424272964409, 0.0005244800848545928817, 0.0007867201272818888889, 0.001048960169709184896 ),
 .UNSPECIFIED. ) ;
#52657 = CARTESIAN_POINT ( 'NONE',  ( -13.11024591527734451, 6.000000000000000000, 45.00000000000000000 ) ) ;
#52658 = EDGE_LOOP ( 'NONE', ( #95727, #32709, #88096 ) ) ;
#52659 = CARTESIAN_POINT ( 'NONE',  ( 166.7004263218490223, 257.9657675534214718, 15.99763568028711092 ) ) ;
#52660 = EDGE_LOOP ( 'NONE', ( #77090, #4541, #94445, #64234 ) ) ;
#52661 = EDGE_LOOP ( 'NONE', ( #37436, #54286, #96337, #83477, #25091, #25122, #69108, #53890 ) ) ;
#52662 = FACE_BOUND ( 'NONE', #66990, .T. ) ;
#52663 = CARTESIAN_POINT ( 'NONE',  ( 67.00504814593276137, 67.59751109484044207, 6.664452144992148774 ) ) ;
#52664 = CARTESIAN_POINT ( 'NONE',  ( 194.7767398707621282, 285.0350113515720523, 17.12152913950285082 ) ) ;
#52665 = CARTESIAN_POINT ( 'NONE',  ( 147.2592533090473239, 275.5864867145116932, -0.3770461397900867762 ) ) ;
#52666 = CARTESIAN_POINT ( 'NONE',  ( 81.43364589948765797, 55.81991725365188017, 16.38199963144059268 ) ) ;
#52667 = CARTESIAN_POINT ( 'NONE',  ( 194.4904290197884507, 293.7796906822950973, 14.50206953321744940 ) ) ;
#52668 = CARTESIAN_POINT ( 'NONE',  ( 77.17055463465335663, 215.3615022471902591, -10.00000000000009592 ) ) ;
#52669 = CARTESIAN_POINT ( 'NONE',  ( 87.62362232749241286, 45.09856358269392729, 6.901305344596347702 ) ) ;
#52670 = VERTEX_POINT ( 'NONE', #50575 ) ;
#52671 = CARTESIAN_POINT ( 'NONE',  ( -65.10162659358719850, 39.48459004765182812, -10.00000000000000000 ) ) ;
#52672 = VERTEX_POINT ( 'NONE', #43470 ) ;
#52673 = CARTESIAN_POINT ( 'NONE',  ( 76.04118372992293473, 51.31859880959181197, -16.13611964362921114 ) ) ;
#52674 = CARTESIAN_POINT ( 'NONE',  ( 174.5345741576458920, 253.2528832121751634, -7.801788862502708533 ) ) ;
#52675 = CARTESIAN_POINT ( 'NONE',  ( 191.0843498247698733, 299.6791929026704793, 6.354791142140047810 ) ) ;
#52676 = CARTESIAN_POINT ( 'NONE',  ( 206.5479446040613141, 272.8954610772809133, 10.74757481123993230 ) ) ;
#52677 = VECTOR ( 'NONE', #89413, 1000.000000000000000 ) ;
#52678 = CARTESIAN_POINT ( 'NONE',  ( 37.33338606056913989, 202.3615022471903160, 5.000000000000046185 ) ) ;
#52679 = CARTESIAN_POINT ( 'NONE',  ( 198.4160757083882345, 267.1808215963346242, -8.346050686629251203 ) ) ;
#52680 = CARTESIAN_POINT ( 'NONE',  ( 138.1714793337695824, 241.3923013555409796, 4.594050593750050204 ) ) ;
#52681 = VERTEX_POINT ( 'NONE', #49582 ) ;
#52682 = CARTESIAN_POINT ( 'NONE',  ( 87.80215979260032100, 44.26138434534234278, 4.729176973005308149 ) ) ;
#52683 = CARTESIAN_POINT ( 'NONE',  ( 183.1817924123992327, 258.9247982590615607, 6.387075791788588752 ) ) ;
#52684 = ADVANCED_FACE ( 'NONE', ( #66289 ), #66780, .T. ) ;
#52685 = CARTESIAN_POINT ( 'NONE',  ( 87.92881912668997302, 44.04200394344634617, -1.750241744287725609 ) ) ;
#52686 = VECTOR ( 'NONE', #1879, 999.9999999999998863 ) ;
#52687 = CARTESIAN_POINT ( 'NONE',  ( 147.7840609055601817, 276.6774932931532476, -0.9735537997635442808 ) ) ;
#52688 = CARTESIAN_POINT ( 'NONE',  ( 73.03196327561725809, 66.92845420574971627, -11.83911326526495067 ) ) ;
#52689 = ORIENTED_EDGE ( 'NONE', *, *, #14832, .T. ) ;
#52690 = CARTESIAN_POINT ( 'NONE',  ( 199.4720805209845196, 266.1420231043892954, 4.760232788326643316 ) ) ;
#52691 = CARTESIAN_POINT ( 'NONE',  ( 188.2520712372829621, 265.6420100395978920, -13.17850047611677766 ) ) ;
#52692 = CARTESIAN_POINT ( 'NONE',  ( 47.84007798744509898, 106.1754093786579318, -10.00000000000000000 ) ) ;
#52693 = CARTESIAN_POINT ( 'NONE',  ( 80.15658303621371772, 48.28644400875573695, 13.66130757313470312 ) ) ;
#52694 = CARTESIAN_POINT ( 'NONE',  ( 198.8095285574927118, 266.4036850393262625, 0.8273979317567071723 ) ) ;
#52695 = CARTESIAN_POINT ( 'NONE',  ( 197.8117387002072860, 265.8538865084539111, 0.8196971304707719730 ) ) ;
#52696 = ADVANCED_FACE ( 'NONE', ( #65773 ), #82539, .F. ) ;
#52697 = CARTESIAN_POINT ( 'NONE',  ( 190.2648877593310317, 301.0985428348857340, -4.426259207433023590 ) ) ;
#52698 = CARTESIAN_POINT ( 'NONE',  ( 185.3455588379956112, 281.9002770091811385, 16.19074574515159526 ) ) ;
#52699 = CIRCLE ( 'NONE', #75379, 3.299999999999998934 ) ;
#52700 = AXIS2_PLACEMENT_3D ( 'NONE', #53099, #89662, #20725 ) ;
#52701 = CARTESIAN_POINT ( 'NONE',  ( 157.7847820078105201, 257.3557362317297361, -18.02899742403477035 ) ) ;
#52702 = FACE_BOUND ( 'NONE', #1500, .T. ) ;
#52703 = CARTESIAN_POINT ( 'NONE',  ( 22.83062064355499032, 21.38052372038641380, 10.00000000000000533 ) ) ;
#52704 = CARTESIAN_POINT ( 'NONE',  ( 86.10128179547638183, 47.01522930412662760, 10.71950609365847917 ) ) ;
#52705 = CARTESIAN_POINT ( 'NONE',  ( 205.3750807262146907, 274.5182765027618075, 11.14488729068320616 ) ) ;
#52706 = CARTESIAN_POINT ( 'NONE',  ( 70.56976607031667470, 69.33912239971135705, -8.253513271727511480 ) ) ;
#52707 = AXIS2_PLACEMENT_3D ( 'NONE', #62179, #85558, #54574 ) ;
#52708 = CARTESIAN_POINT ( 'NONE',  ( 159.6419305724666344, 254.1390605605417079, 16.92015248457581933 ) ) ;
#52709 = CARTESIAN_POINT ( 'NONE',  ( 72.30143066935100649, 72.00106423939931233, -3.615897486538043548 ) ) ;
#52710 = CARTESIAN_POINT ( 'NONE',  ( 143.2591182574054187, 253.5177522451418497, -10.00000000000009592 ) ) ;
#52711 = CARTESIAN_POINT ( 'NONE',  ( 175.9106323274208705, 285.6143439489698039, -11.86405137256001296 ) ) ;
#52712 = ORIENTED_EDGE ( 'NONE', *, *, #670, .T. ) ;
#52713 = PRODUCT_DEFINITION_FORMATION_WITH_SPECIFIED_SOURCE ( 'ANY', '', #89683, .NOT_KNOWN. ) ;
#52714 = CARTESIAN_POINT ( 'NONE',  ( 66.77293986438145623, 68.13932227484529847, -6.519502098149898117 ) ) ;
#52715 = CARTESIAN_POINT ( 'NONE',  ( 72.64601778605843663, 70.71744408260791204, -7.969226289351840187 ) ) ;
#52716 = CARTESIAN_POINT ( 'NONE',  ( 198.7357616895271804, 286.4265588032756114, -17.04018524297827497 ) ) ;
#52717 = CARTESIAN_POINT ( 'NONE',  ( 2.773212693257451900, 184.6589784336661637, -6.496448406907676862E-16 ) ) ;
#52718 = CARTESIAN_POINT ( 'NONE',  ( 181.7028333219653291, 276.2859026444305073, -16.76116147531152833 ) ) ;
#52719 = CARTESIAN_POINT ( 'NONE',  ( 22.60804823384966156, 31.79103043416549923, 8.090169943749478065 ) ) ;
#52720 = CARTESIAN_POINT ( 'NONE',  ( 85.91498916281075537, 48.46192805135255099, 12.13455285288522667 ) ) ;
#52721 = CARTESIAN_POINT ( 'NONE',  ( 171.3171204526115616, 271.4791138034659070, -17.75561031716327420 ) ) ;
#52722 = CARTESIAN_POINT ( 'NONE',  ( 71.94430347986846641, 71.72799717812090137, -3.886761019894646729 ) ) ;
#52723 = CARTESIAN_POINT ( 'NONE',  ( 149.9796301194747343, 276.8100220917153251, 4.535783967717629928 ) ) ;
#52724 = CARTESIAN_POINT ( 'NONE',  ( 175.5717179822201217, 253.3804273325372378, -3.507250143043896262 ) ) ;
#52725 = CARTESIAN_POINT ( 'NONE',  ( 198.7564336180209068, 286.3907539728338634, 17.89468790901915796 ) ) ;
#52726 = CARTESIAN_POINT ( 'NONE',  ( 56.31377616017817900, 189.9865022471901455, 1.119607411625061291E-15 ) ) ;
#52727 = CARTESIAN_POINT ( 'NONE',  ( 76.26946404230703536, 64.97317754398874001, 14.67006731301516176 ) ) ;
#52728 = CARTESIAN_POINT ( 'NONE',  ( 190.1158090214649405, 301.3567547831981983, -1.340987185199551845 ) ) ;
#52729 = CARTESIAN_POINT ( 'NONE',  ( 16.87327557256410060, 189.7369531367911293, -4.594050593750048428 ) ) ;
#52730 = CARTESIAN_POINT ( 'NONE',  ( 72.57773168451072365, 70.69087215581753014, -7.948841485240758509 ) ) ;
#52731 = CARTESIAN_POINT ( 'NONE',  ( 78.91212607377818244, 60.09823531620596526, 16.11286148787682393 ) ) ;
#52732 = CARTESIAN_POINT ( 'NONE',  ( 110.0000000000000000, 0.000000000000000000, 59.99999999999999289 ) ) ;
#52733 = LINE ( 'NONE', #22350, #6115 ) ;
#52734 = CARTESIAN_POINT ( 'NONE',  ( -22.42236680055709641, 157.8615022471902591, 0.000000000000000000 ) ) ;
#52735 = CARTESIAN_POINT ( 'NONE',  ( 188.6005607789109320, 267.5261675405737378, 14.22050808917637887 ) ) ;
#52736 = CARTESIAN_POINT ( 'NONE',  ( 153.8480465357228013, 265.0660884932569843, -16.61306390558784685 ) ) ;
#52737 = CARTESIAN_POINT ( 'NONE',  ( 164.2037877926934470, 281.4932537616303421, 9.235950372291741317 ) ) ;
#52738 = APPLICATION_PROTOCOL_DEFINITION ( 'draft international standard', 'automotive_design', 1998, #18827 ) ;
#52739 = CARTESIAN_POINT ( 'NONE',  ( 19.11131643181922968, 13.96004757982089473, -5.678558825948276656 ) ) ;
#52740 = CARTESIAN_POINT ( 'NONE',  ( 148.4049257185216106, 273.6021238924720365, 8.639190357831699529 ) ) ;
#52741 = CARTESIAN_POINT ( 'NONE',  ( 71.81391265307100014, 59.05408711125518550, 15.37230141137981754 ) ) ;
#52743 = ADVANCED_FACE ( 'NONE', ( #65287 ), #3987, .F. ) ;
#52742 = AXIS2_PLACEMENT_3D ( 'NONE', #20463, #67537, #90399 ) ;
#52744 = CARTESIAN_POINT ( 'NONE',  ( 203.6925490392534925, 269.5270927311577793, 7.084861529579629114 ) ) ;
#52745 = VERTEX_POINT ( 'NONE', #13103 ) ;
#52746 = CARTESIAN_POINT ( 'NONE',  ( 86.41880224017843659, 45.50969932908875393, -7.944645677213507895 ) ) ;
#52747 = CARTESIAN_POINT ( 'NONE',  ( -71.61465314115659453, 63.06504152958490295, 25.00000000000000000 ) ) ;
#52748 = CARTESIAN_POINT ( 'NONE',  ( 81.46654924364905526, 42.47797946394854307, 7.469209086924764485 ) ) ;
#52749 = EDGE_CURVE ( 'NONE', #77084, #7044, #85640, .T. ) ;
#52750 = ORIENTED_EDGE ( 'NONE', *, *, #20094, .T. ) ;
#52751 = CARTESIAN_POINT ( 'NONE',  ( 79.99999999999998579, 9.999999999999985789, 2.622423327744133559 ) ) ;
#52752 = FACE_OUTER_BOUND ( 'NONE', #98802, .T. ) ;
#52753 = CARTESIAN_POINT ( 'NONE',  ( 20.44528175232247591, 34.73705186507753950, -3.090169943749475845 ) ) ;
#52754 = CARTESIAN_POINT ( 'NONE',  ( 154.8545429534089237, 262.4310591522755089, -17.81746354318405778 ) ) ;
#52755 = ORIENTED_EDGE ( 'NONE', *, *, #81928, .T. ) ;
#52756 = EDGE_LOOP ( 'NONE', ( #83614, #78070, #90610, #43421 ) ) ;
#52758 = CARTESIAN_POINT ( 'NONE',  ( 204.9004517216375518, 275.7490024547470853, 14.55104398969427670 ) ) ;
#52757 = FACE_OUTER_BOUND ( 'NONE', #34584, .T. ) ;
#52759 = ORIENTED_EDGE ( 'NONE', *, *, #67637, .T. ) ;
#52760 = CARTESIAN_POINT ( 'NONE',  ( 151.2648146047323507, 268.6486510375538614, 15.71323890031163550 ) ) ;
#52761 = CARTESIAN_POINT ( 'NONE',  ( 71.93357406896315354, 69.69179662921422391, 8.874436160946375551 ) ) ;
#52762 = CARTESIAN_POINT ( 'NONE',  ( 80.39015929397758953, 57.47250276623566378, -16.58917374605577777 ) ) ;
#52763 = CARTESIAN_POINT ( 'NONE',  ( 67.84059961315651321, 69.51487248268222174, -4.691999901035240228 ) ) ;
#52765 = EDGE_CURVE ( 'NONE', #99548, #48481, #4484, .T. ) ;
#52764 = EDGE_LOOP ( 'NONE', ( #76377, #55768, #96495, #91666 ) ) ;
#52766 = DIRECTION ( 'NONE',  ( 0.4999999999999998890, -0.8660254037844385966, 0.000000000000000000 ) ) ;
#52767 = CARTESIAN_POINT ( 'NONE',  ( 196.8435556370661459, 289.7039558245273838, -16.43899056939217118 ) ) ;
#52768 = VERTEX_POINT ( 'NONE', #36368 ) ;
#52769 = CARTESIAN_POINT ( 'NONE',  ( 206.5318754762992910, 272.9232936229979032, 10.63244694018452741 ) ) ;
#52770 = AXIS2_PLACEMENT_3D ( 'NONE', #75004, #5094, #18805 ) ;
#52771 = CARTESIAN_POINT ( 'NONE',  ( 194.5725374088679871, 291.6374747806817140, -16.23208319182986870 ) ) ;
#52772 = VERTEX_POINT ( 'NONE', #11115 ) ;
#52773 = CARTESIAN_POINT ( 'NONE',  ( 190.8187029736043883, 300.1393067457597681, 3.941064102378585954 ) ) ;
#52774 = CARTESIAN_POINT ( 'NONE',  ( 200.0577211067540873, 278.4141957227807325, 16.45782674848881300 ) ) ;
#52775 = ORIENTED_EDGE ( 'NONE', *, *, #64436, .T. ) ;
#52776 = CARTESIAN_POINT ( 'NONE',  ( -6.926766666751215773, 73.70349067594094095, 14.94635119574900450 ) ) ;
#52777 = ADVANCED_FACE ( 'NONE', ( #91119 ), #22684, .T. ) ;
#52778 = CARTESIAN_POINT ( 'NONE',  ( 188.7267243920021542, 295.1910411013678299, 11.79826141631466463 ) ) ;
#52779 = CARTESIAN_POINT ( 'NONE',  ( 27.76992210170819675, 43.29297894285233639, -10.00000000000000000 ) ) ;
#52781 = VECTOR ( 'NONE', #11599, 1000.000000000000227 ) ;
#52780 = CARTESIAN_POINT ( 'NONE',  ( 83.32631514680937812, 52.40275339355609674, 14.85530416217961047 ) ) ;
#52782 = ORIENTED_EDGE ( 'NONE', *, *, #95988, .T. ) ;
#52783 = ORIENTED_EDGE ( 'NONE', *, *, #93713, .T. ) ;
#52784 = CARTESIAN_POINT ( 'NONE',  ( 78.48876124178367775, 51.94357913415533545, -15.95536876511241964 ) ) ;
#52785 = CARTESIAN_POINT ( 'NONE',  ( 83.05016518402850068, 42.76510943801325482, -6.363870132515760503 ) ) ;
#52786 = CARTESIAN_POINT ( 'NONE',  ( 190.8683709797118411, 300.0532792356709706, -4.461919767133968762 ) ) ;
#52787 = CARTESIAN_POINT ( 'NONE',  ( 190.5969391768923913, 300.5234129089444650, -0.7564693504096553500 ) ) ;
#52788 = CARTESIAN_POINT ( 'NONE',  ( 18.86034532297697908, 34.61239144260638767, 177.5919119679930134 ) ) ;
#52789 = CARTESIAN_POINT ( 'NONE',  ( -22.42236680055709641, 157.8615022471902591, 0.000000000000000000 ) ) ;
#52790 = DIRECTION ( 'NONE',  ( 0.1710100716628310258, -0.2961981327260192476, 0.9396926207859104263 ) ) ;
#52791 = CARTESIAN_POINT ( 'NONE',  ( 146.6138605399200117, 276.7043397814778132, -0.5394499176159462950 ) ) ;
#52792 = B_SPLINE_CURVE_WITH_KNOTS ( 'NONE', 3,
 ( #34740, #3379, #42823, #43833, #42334, #65148, #65642, #5350, #66642, #19076, #97096, #27664, #58532, #82887, #89506, #50938, #81887, #36231, #35746, #97572, #89030, #74282, #72788, #12972, #12463, #96096, #43334, #49952, #96597, #59014, #89983, #26654, #20561, #51439, #74772, #88514, #27161, #67137, #98059, #28636, #59519, #90498, #21071, #51947, #13461, #37232, #68130, #77229 ),
 .UNSPECIFIED., .F., .F.,
 ( 4, 2, 2, 2, 2, 2, 2, 2, 2, 2, 2, 2, 2, 2, 2, 2, 2, 2, 2, 2, 2, 2, 2, 4 ),
 ( 0.0008860715642980536997, 0.0009820465975983500191, 0.001078021630898646230, 0.001173996664198942441, 0.001269971697499238869, 0.001461921764099907185, 0.001653871830700575935, 0.002421672097103298640, 0.003957272629908744482, 0.004725072896311395196, 0.005108973029512683256, 0.005300923096113327286, 0.005396898129413611571, 0.005444885646063752846, 0.005492873162713894121, 0.005540860679364035396, 0.005588848196014176671, 0.005684823229314512130, 0.005876773295915232488, 0.006068723362515953713, 0.006260673429116674071, 0.006452623495717395297, 0.006644573562318115655, 0.007028473695519553768 ),
 .UNSPECIFIED. ) ;
#52793 = CARTESIAN_POINT ( 'NONE',  ( 75.09455210346366982, 57.68713258346969042, -16.03622425841626509 ) ) ;
#52794 = DIRECTION ( 'NONE',  ( -0.8660254037844387076, -0.4999999999999998890, -0.000000000000000000 ) ) ;
#52795 = CARTESIAN_POINT ( 'NONE',  ( -19.65312891409030271, 93.06504152958497400, 10.00000000000000888 ) ) ;
#52796 = CARTESIAN_POINT ( 'NONE',  ( 67.14666838648643932, 66.78363720521792857, 8.171468515940333077 ) ) ;
#52797 = CARTESIAN_POINT ( 'NONE',  ( 171.3163111156538321, 289.1506865685547041, 4.320660422964803793 ) ) ;
#52798 = B_SPLINE_CURVE_WITH_KNOTS ( 'NONE', 3,
 ( #16697, #47589, #70910, #48090, #79032, #9621, #40484, #2004, #25293, #58673, #96741, #20206, #67282, #19718, #57684, #51078, #35388, #98208, #89645, #65783, #49592, #97714, #27304, #66788, #20704, #58188, #88661, #82039, #12614, #28792, #4493, #50583, #13112, #43478, #74423, #5007, #51592, #88162, #35885, #82547, #90132, #41993 ),
 .UNSPECIFIED., .F., .F.,
 ( 4, 2, 2, 2, 2, 2, 2, 2, 2, 2, 2, 2, 2, 2, 2, 2, 2, 2, 2, 2, 4 ),
 ( 0.003272589128710177292, 0.003466937949059250689, 0.003564112359233767655, 0.003661286769408285055, 0.003758461179582802021, 0.003855635589757318987, 0.004049984410106313021, 0.004438682050804295884, 0.004827379691502279614, 0.005604774972898246208, 0.006382170254294213668, 0.007936960817085992465, 0.008131309637435015988, 0.008155603239978690550, 0.008179896842522363376, 0.008204190445066034468, 0.008228484047609709029, 0.008325658457784452376, 0.008714356098483127394, 0.009103053739181800677, 0.009491751379880475695 ),
 .UNSPECIFIED. ) ;
#52799 = LINE ( 'NONE', #55780, #56099 ) ;
#52800 = ORIENTED_EDGE ( 'NONE', *, *, #17035, .F. ) ;
#52801 = CARTESIAN_POINT ( 'NONE',  ( 149.5520331575485500, 271.6152755263370295, -13.01004061128467626 ) ) ;
#52802 = EDGE_CURVE ( 'NONE', #65018, #30521, #32483, .T. ) ;
#52803 = CARTESIAN_POINT ( 'NONE',  ( 74.51860651786539336, 54.69479437051430892, -16.14050065589297844 ) ) ;
#52804 = ADVANCED_FACE ( 'NONE', ( #67781 ), #29290, .F. ) ;
#52805 = CARTESIAN_POINT ( 'NONE',  ( 85.72891561183703857, 43.80477521659179274, 6.542285751333638544 ) ) ;
#52806 = CARTESIAN_POINT ( 'NONE',  ( 79.69883455371483194, 45.99209036072507928, 12.97227174178035192 ) ) ;
#52807 = CARTESIAN_POINT ( 'NONE',  ( 191.8650071060532412, 297.4868766427842388, -10.36821096227007288 ) ) ;
#52808 = CARTESIAN_POINT ( 'NONE',  ( 79.41561859137864587, 54.73972641915754878, -16.40726218708634931 ) ) ;
#52809 = CARTESIAN_POINT ( 'NONE',  ( 169.2499022714398791, 285.3069777449377398, -7.727577981700628484 ) ) ;
#52810 = ORIENTED_EDGE ( 'NONE', *, *, #84255, .T. ) ;
#52812 = EDGE_CURVE ( 'NONE', #38189, #97286, #79533, .T. ) ;
#52811 = CARTESIAN_POINT ( 'NONE',  ( 163.1096928939807924, 248.1327200311062882, -9.690381021358412283 ) ) ;
#52813 = CARTESIAN_POINT ( 'NONE',  ( 206.8106726053982811, 272.4404028303941914, -10.47827087991598560 ) ) ;
#52814 = CYLINDRICAL_SURFACE ( 'NONE', #22445, 10.00000000000001066 ) ;
#52815 = CARTESIAN_POINT ( 'NONE',  ( 42.00631479827482195, 188.3927522451418213, -10.00000000000009059 ) ) ;
#52816 = CARTESIAN_POINT ( 'NONE',  ( 121.5815934185826421, 234.8768266524159856, -9.188101187500093303 ) ) ;
#52817 = CARTESIAN_POINT ( 'NONE',  ( 180.7189620564184054, 294.1892054117222415, -3.206099072908067615 ) ) ;
#52818 = ADVANCED_FACE ( 'NONE', ( #61162 ), #74043, .F. ) ;
#52819 = CARTESIAN_POINT ( 'NONE',  ( -65.66987298107781612, 17.49999999999999645, -10.00000000000000178 ) ) ;
#52820 = CARTESIAN_POINT ( 'NONE',  ( 195.7291534503633272, 291.6341570319625021, 16.44925029361851543 ) ) ;
#52821 = CARTESIAN_POINT ( 'NONE',  ( 175.4457714882561561, 253.5523854228639493, -3.987518762506754744 ) ) ;
#52822 = CARTESIAN_POINT ( 'NONE',  ( 28.75397480679061246, 199.6589784336661637, -6.496448406907675876E-16 ) ) ;
#52823 = AXIS2_PLACEMENT_3D ( 'NONE', #94988, #77242, #63536 ) ;
#52824 = FACE_OUTER_BOUND ( 'NONE', #66620, .T. ) ;
#52825 = VECTOR ( 'NONE', #68514, 1000.000000000000000 ) ;
#52826 = ORIENTED_EDGE ( 'NONE', *, *, #89306, .T. ) ;
#52828 = ADVANCED_FACE ( 'NONE', ( #32766 ), #24175, .T. ) ;
#52827 = CARTESIAN_POINT ( 'NONE',  ( 72.78342027449815532, 68.81891707817121073, 9.930820707867006547 ) ) ;
#52829 = CARTESIAN_POINT ( 'NONE',  ( 178.0210747266523867, 265.4709656426701940, 15.86782561207190945 ) ) ;
#52830 = EDGE_CURVE ( 'NONE', #52219, #26620, #25165, .T. ) ;
#52831 = B_SPLINE_SURFACE_WITH_KNOTS ( 'NONE', 3, 1, ( 
 ( #62555, #8385 ),
 ( #39252, #78293 ),
 ( #23063, #32172 ),
 ( #14493, #63076 ),
 ( #45856, #31658 ),
 ( #70163, #772 ),
 ( #24075, #69171 ),
 ( #45373, #54969 ),
 ( #92515, #17996 ),
 ( #79331, #64589 ),
 ( #88444, #72203 ),
 ( #94519, #3790 ),
 ( #48387, #24571 ),
 ( #71708, #1793 ),
 ( #32676, #2300 ),
 ( #95026, #9382 ),
 ( #48890, #87464 ),
 ( #41260, #26089 ),
 ( #9899, #80839 ),
 ( #10392, #63575 ),
 ( #19003, #25071 ),
 ( #25588, #40757 ),
 ( #55456, #33182 ),
 ( #95542, #55949 ),
 ( #64081, #56475 ),
 ( #41769, #79824 ),
 ( #16968, #86945 ),
 ( #2808, #33696 ),
 ( #56964, #87950 ),
 ( #17478, #18494 ),
 ( #40260, #86441 ),
 ( #26590, #49380 ),
 ( #80323, #94020 ),
 ( #10893, #57463 ) ),
 .UNSPECIFIED., .T., .F., .F.,
 ( 4, 2, 2, 2, 2, 2, 2, 2, 2, 2, 2, 2, 2, 2, 2, 2, 4 ),
 ( 2, 2 ),
 ( 0.000000000000000000, 0.06250000000000000000, 0.1250000000000000000, 0.1875000000000000000, 0.2500000000000000000, 0.3125000000000000000, 0.3750000000000000000, 0.4375000000000000000, 0.5000000000000000000, 0.5625000000000000000, 0.6250000000000000000, 0.6875000000000000000, 0.7500000000000000000, 0.8125000000000000000, 0.8750000000000000000, 0.9375000000000000000, 1.000000000000000000 ),
 ( 0.000000000000000000, 1.000000000000000000 ),
 .UNSPECIFIED. ) ;
#52832 =( BOUNDED_CURVE ( )  B_SPLINE_CURVE ( 2, ( #88318, #81691, #18873, #27471, #65449, #4654, #72585, #73562, #65946 ),
 .UNSPECIFIED., .F., .T. ) 
 B_SPLINE_CURVE_WITH_KNOTS ( ( 3, 2, 2, 2, 3 ),
 ( 0.5201612903225806273, 0.5215053763440860024, 0.5241935483870967527, 0.5268817204301075030, 0.5282258064516128782 ),
 .UNSPECIFIED. ) 
 CURVE ( )  GEOMETRIC_REPRESENTATION_ITEM ( )  RATIONAL_B_SPLINE_CURVE ( ( 0.9330127018922194093, 0.9330127018922194093, 1.000000000000000000, 0.8660254037844387076, 1.000000000000000000, 0.8660254037844387076, 1.000000000000000000, 0.9330127018922194093, 0.9330127018922194093 ) ) 
 REPRESENTATION_ITEM ( '' )  );
#52833 = DIRECTION ( 'NONE',  ( 0.4999999999999997780, -0.8660254037844388186, 0.000000000000000000 ) ) ;
#52834 = VECTOR ( 'NONE', #23144, 1000.000000000000000 ) ;
#52835 = CYLINDRICAL_SURFACE ( 'NONE', #40251, 49.99999999999999289 ) ;
#52836 = CARTESIAN_POINT ( 'NONE',  ( 81.98204644740465596, 41.14170829992954026, -5.380964918555401155 ) ) ;
#52837 = B_SPLINE_CURVE_WITH_KNOTS ( 'NONE', 3,
 ( #26166, #82772, #13339, #44696, #36606, #80407, #20440, #4741 ),
 .UNSPECIFIED., .F., .F.,
 ( 4, 2, 2, 4 ),
 ( 0.1732562812666568475, 0.5866281406333284654, 0.7933140703166642327, 1.000000000000000000 ),
 .UNSPECIFIED. ) ;
#52838 = CARTESIAN_POINT ( 'NONE',  ( -16.99542894172669349, 24.36904009834038476, -10.00000000000000000 ) ) ;
#52839 = CARTESIAN_POINT ( 'NONE',  ( 181.9343943630181855, 262.2755151286456794, 13.05455344133680207 ) ) ;
#52840 =( BOUNDED_CURVE ( )  B_SPLINE_CURVE ( 2, ( #40411, #79475, #87098, #31317, #17638, #48536, #33328, #8041, #54104 ),
 .UNSPECIFIED., .F., .T. ) 
 B_SPLINE_CURVE_WITH_KNOTS ( ( 3, 2, 2, 2, 3 ),
 ( 0.1733870967741935609, 0.1747311827956989361, 0.1774193548387096864, 0.1801075268817204367, 0.1814516129032258118 ),
 .UNSPECIFIED. ) 
 CURVE ( )  GEOMETRIC_REPRESENTATION_ITEM ( )  RATIONAL_B_SPLINE_CURVE ( ( 0.9330127018922194093, 0.9330127018922194093, 1.000000000000000000, 0.8660254037844387076, 1.000000000000000000, 0.8660254037844387076, 1.000000000000000000, 0.9330127018922194093, 0.9330127018922194093 ) ) 
 REPRESENTATION_ITEM ( '' )  );
#52841 = CARTESIAN_POINT ( 'NONE',  ( 103.4219496833212162, 240.5177522451419350, 5.000000000000046185 ) ) ;
#52842 = ORIENTED_EDGE ( 'NONE', *, *, #13925, .T. ) ;
#52843 = B_SPLINE_CURVE_WITH_KNOTS ( 'NONE', 3,
 ( #17595, #39864, #70801, #94133, #1410, #63192, #48504, #10007, #33291, #64193 ),
 .UNSPECIFIED., .F., .F.,
 ( 4, 2, 2, 2, 4 ),
 ( 0.000000000000000000, 0.0002622400424272842436, 0.0005244800848545684872, 0.0007867201272818526766, 0.001048960169709136974 ),
 .UNSPECIFIED. ) ;
#52844 = CARTESIAN_POINT ( 'NONE',  ( 201.5074933251657399, 279.6257787853921286, 16.58790246189369100 ) ) ;
#52845 = CARTESIAN_POINT ( 'NONE',  ( 158.8095040752041882, 282.2712473417889782, -1.635881903422608419 ) ) ;
#52846 = LINE ( 'NONE', #21460, #5934 ) ;
#52847 = CARTESIAN_POINT ( 'NONE',  ( 3.585285057187872493, 179.0024278399160949, 9.188101187500095079 ) ) ;
#52848 = CARTESIAN_POINT ( 'NONE',  ( 3.540199675970839177, 23.81751292744053217, -6.180339887498951690 ) ) ;
#52849 = CARTESIAN_POINT ( 'NONE',  ( 196.1470069647167804, 273.5382448026506381, 15.10109762947431022 ) ) ;
#52850 = CARTESIAN_POINT ( 'NONE',  ( 71.86919472611239712, 59.31234992600734302, -15.30864741555868846 ) ) ;
#52851 = CARTESIAN_POINT ( 'NONE',  ( 84.06604358195920668, 51.46910565605918464, 14.65639964578790533 ) ) ;
#52853 = CARTESIAN_POINT ( 'NONE',  ( 68.45643432912224569, 201.1423013555409796, -4.594050593750043987 ) ) ;
#52852 = CARTESIAN_POINT ( 'NONE',  ( 175.5129311542572736, 286.7531494202563067, 10.50704365649472116 ) ) ;
#52854 = CARTESIAN_POINT ( 'NONE',  ( 207.5408646414791178, 271.1756731246201753, 3.050859480894625886 ) ) ;
#52855 = CARTESIAN_POINT ( 'NONE',  ( 74.02416338248266925, 55.20782277953769324, 16.12359275168059369 ) ) ;
#52856 = DIRECTION ( 'NONE',  ( 0.4805540241036304616, 0.8769651246872975925, 0.000000000000000000 ) ) ;
#52857 = CARTESIAN_POINT ( 'NONE',  ( 66.08289746408667042, 68.56685657833568825, -4.488094959726262267 ) ) ;
#52858 = VERTEX_POINT ( 'NONE', #72300 ) ;
#52859 = VECTOR ( 'NONE', #10091, 1000.000000000000227 ) ;
#52860 = CARTESIAN_POINT ( 'NONE',  ( 20.01287798488040437, 182.3615022471902591, -10.00000000000009592 ) ) ;
#52861 = CARTESIAN_POINT ( 'NONE',  ( 164.0854748117396582, 246.4426161724408928, -5.757837433625331514 ) ) ;
#52862 = CARTESIAN_POINT ( 'NONE',  ( 130.4037065759891334, 258.3464784336661637, 1.353441290958777327E-15 ) ) ;
#52863 = CARTESIAN_POINT ( 'NONE',  ( 20.18904385193075868, 29.84336893147756342, -7.433330006724137462 ) ) ;
#52864 = FACE_OUTER_BOUND ( 'NONE', #39070, .T. ) ;
#52865 = DIRECTION ( 'NONE',  ( -0.04056776950002415755, 0.9991767892008865948, 0.000000000000000000 ) ) ;
#52866 = CARTESIAN_POINT ( 'NONE',  ( 75.18533445981178431, 53.54581650303052243, -16.05318290065117282 ) ) ;
#52868 = CARTESIAN_POINT ( 'NONE',  ( 184.7889694759585666, 277.2988950505619528, -17.76348561330697962 ) ) ;
#52867 = CARTESIAN_POINT ( 'NONE',  ( 88.45605923504750479, 44.01628325393264873, 2.215908606781754830 ) ) ;
#52869 = CARTESIAN_POINT ( 'NONE',  ( 168.4449364156751585, 258.1664367055781213, -15.63070130756588938 ) ) ;
#52870 = VERTEX_POINT ( 'NONE', #24667 ) ;
#52871 = CARTESIAN_POINT ( 'NONE',  ( 165.3552783545318050, 246.2432519206945472, 4.078954813822171843 ) ) ;
#52872 = CARTESIAN_POINT ( 'NONE',  ( 185.9608592076092464, 288.5956984647530703, 15.36535719480430018 ) ) ;
#52873 = CARTESIAN_POINT ( 'NONE',  ( 172.4369982594507746, 275.8394585651928423, 17.18367144343603670 ) ) ;
#52874 = CARTESIAN_POINT ( 'NONE',  ( 156.5693519948572430, 280.4191655658614764, -5.442758104603233171 ) ) ;
#52875 = CARTESIAN_POINT ( 'NONE',  ( 196.6986986009438283, 272.8388821338493244, -13.37107033830584513 ) ) ;
#52876 = ORIENTED_EDGE ( 'NONE', *, *, #45220, .T. ) ;
#52877 = CARTESIAN_POINT ( 'NONE',  ( 206.8429133553250949, 272.3845602134468322, 7.956126979824590606 ) ) ;
#52878 = ADVANCED_FACE ( 'NONE', ( #10481 ), #56568, .F. ) ;
#52879 = B_SPLINE_CURVE_WITH_KNOTS ( 'NONE', 3,
 ( #46658, #60844, #83714, #91806, #6171, #29474, #69953, #84219, #77585, #53746, #78, #14272, #15246, #60347, #45648, #28988, #46142, #76576, #59863, #7157, #92313, #38044, #76102, #21380 ),
 .UNSPECIFIED., .F., .F.,
 ( 4, 2, 2, 2, 2, 2, 2, 2, 2, 2, 2, 4 ),
 ( 0.000000000000000000, 0.1249999999999653333, 0.2499999999999306666, 0.3749999999998959721, 0.4374999999999003020, 0.4999999999999046318, 0.5624999999999089617, 0.6249999999999132916, 0.6874999999999176215, 0.7499999999999218403, 0.8749999999999609201, 1.000000000000000000 ),
 .UNSPECIFIED. ) ;
#52880 = CARTESIAN_POINT ( 'NONE',  ( 170.9098063187821310, 283.9312053951169901, -11.13929243000735170 ) ) ;
#52881 = EDGE_CURVE ( 'NONE', #3988, #4641, #8477, .T. ) ;
#52882 = B_SPLINE_CURVE_WITH_KNOTS ( 'NONE', 3,
 ( #8905, #77827, #30213, #14524, #22115, #8411 ),
 .UNSPECIFIED., .F., .F.,
 ( 4, 2, 4 ),
 ( 0.02030182656484812165, 0.02486100877575732337, 0.02942019098666652857 ),
 .UNSPECIFIED. ) ;
#52883 = FACE_OUTER_BOUND ( 'NONE', #71005, .T. ) ;
#52884 = CARTESIAN_POINT ( 'NONE',  ( 7.868168403658736487, 186.8967562850346837, -4.648177544792955347E-16 ) ) ;
#52885 = CARTESIAN_POINT ( 'NONE',  ( 97.79278455872243114, 217.2677522451417644, -5.000000000000041744 ) ) ;
#52886 = CARTESIAN_POINT ( 'NONE',  ( 208.3226489551340990, 269.8215829728092103, -1.240262689467544366 ) ) ;
#52887 = LINE ( 'NONE', #14403, #61274 ) ;
#52888 = CARTESIAN_POINT ( 'NONE',  ( 193.8652130780152731, 280.5836658925297229, -17.72338988841175933 ) ) ;
#52889 = CARTESIAN_POINT ( 'NONE',  ( 19.46611421548295695, 12.20801979619928090, -3.090169943749474069 ) ) ;
#52890 = CARTESIAN_POINT ( 'NONE',  ( 83.97117539556700194, 48.10897359057201328, 12.72530908371034464 ) ) ;
#52891 = ORIENTED_EDGE ( 'NONE', *, *, #81421, .F. ) ;
#52892 = CARTESIAN_POINT ( 'NONE',  ( 190.0707697440390689, 301.4347651000360884, 4.271360729158901748 ) ) ;
#52893 = FACE_OUTER_BOUND ( 'NONE', #32508, .T. ) ;
#52894 = CARTESIAN_POINT ( 'NONE',  ( 189.3904159748659310, 297.2581566609080141, 8.144294695757311686 ) ) ;
#52896 = ADVANCED_FACE ( 'NONE', ( #39347 ), #87554, .T. ) ;
#52895 = ORIENTED_EDGE ( 'NONE', *, *, #62985, .T. ) ;
#52897 = CARTESIAN_POINT ( 'NONE',  ( 191.8232488616404225, 298.3993822291468518, -9.342381338555176384 ) ) ;
#52898 = DIRECTION ( 'NONE',  ( 0.000000000000000000, 0.000000000000000000, 1.000000000000000000 ) ) ;
#52899 = CARTESIAN_POINT ( 'NONE',  ( 164.2413944571582078, 246.1725554246774834, 7.304616466633322425 ) ) ;
#52900 = AXIS2_PLACEMENT_3D ( 'NONE', #88387, #2240, #18941 ) ;
#52901 = CARTESIAN_POINT ( 'NONE',  ( 21.19816502305182837, 13.20801979619928268, -3.090169943749474069 ) ) ;
#52902 = ORIENTED_EDGE ( 'NONE', *, *, #18879, .T. ) ;
#52903 = CARTESIAN_POINT ( 'NONE',  ( 90.37718171876834106, 232.1744531367911293, 4.594050593750047540 ) ) ;
#52904 = CARTESIAN_POINT ( 'NONE',  ( 198.7305186980039480, 282.8878823269354825, 17.40725258201084813 ) ) ;
#52905 = VECTOR ( 'NONE', #38825, 1000.000000000000114 ) ;
#52906 = CARTESIAN_POINT ( 'NONE',  ( 180.9789598105594450, 270.9731600656857040, -15.98183179343307891 ) ) ;
#52907 = CARTESIAN_POINT ( 'NONE',  ( 81.53796252524934118, 42.62971458812653935, -7.650143360278183202 ) ) ;
#52908 = ORIENTED_EDGE ( 'NONE', *, *, #36937, .T. ) ;
#52909 = EDGE_CURVE ( 'NONE', #36946, #68704, #44482, .T. ) ;
#52910 = EDGE_CURVE ( 'NONE', #91334, #55290, #31205, .T. ) ;
#52911 = ORIENTED_EDGE ( 'NONE', *, *, #87627, .T. ) ;
#52912 = CARTESIAN_POINT ( 'NONE',  ( 81.12979385446129754, 48.93447223002202406, 13.74866293976100806 ) ) ;
#52913 = VERTEX_POINT ( 'NONE', #66664 ) ;
#52914 = CARTESIAN_POINT ( 'NONE',  ( 148.3010860587701814, 276.5068540982774721, -3.904121881399305050 ) ) ;
#52915 = CARTESIAN_POINT ( 'NONE',  ( -19.65312891409030271, 93.06504152958497400, 177.5919119679930134 ) ) ;
#52916 = EDGE_LOOP ( 'NONE', ( #88353, #20142, #72490, #65575 ) ) ;
#52917 = CARTESIAN_POINT ( 'NONE',  ( 208.1415148974628266, 270.1353163636768500, 3.453641150550738725 ) ) ;
#52918 = VECTOR ( 'NONE', #50094, 1000.000000000000000 ) ;
#52919 = CYLINDRICAL_SURFACE ( 'NONE', #56246, 17.82106496071139645 ) ;
#52920 = AXIS2_PLACEMENT_3D ( 'NONE', #81439, #82933, #98107 ) ;
#52921 = DIRECTION ( 'NONE',  ( 0.8660254037844385966, 0.5000000000000001110, -0.000000000000000000 ) ) ;
#52922 = CARTESIAN_POINT ( 'NONE',  ( -23.40626505353419873, 99.76179925954940586, 45.19938068878172288 ) ) ;
#52923 = CARTESIAN_POINT ( 'NONE',  ( 82.74206721279597332, 53.66691124579689642, -15.75745978315255869 ) ) ;
#52924 = ORIENTED_EDGE ( 'NONE', *, *, #73643, .F. ) ;
#52925 = CARTESIAN_POINT ( 'NONE',  ( 66.18410330236099526, 68.78720517270650703, 0.1136469981348479652 ) ) ;
#52926 = CARTESIAN_POINT ( 'NONE',  ( 14.44441505419593064, 16.84335787977761711, 9.188101187500006262 ) ) ;
#52927 = CARTESIAN_POINT ( 'NONE',  ( 164.6189477058751720, 281.8792342857743165, 8.841444651024419343 ) ) ;
#52928 = CARTESIAN_POINT ( 'NONE',  ( 80.74781574657599492, 57.21644485803225422, 16.56566952311892749 ) ) ;
#52930 = ORIENTED_EDGE ( 'NONE', *, *, #39194, .F. ) ;
#52929 = CARTESIAN_POINT ( 'NONE',  ( 19.41748551623073027, 172.0177522451417929, 5.000000000000051514 ) ) ;
#52931 = B_SPLINE_CURVE_WITH_KNOTS ( 'NONE', 3,
 ( #99886, #30469, #14276, #61362, #85213, #68465, #75590, #92319, #53270, #15758, #53751, #45168, #67474, #69467 ),
 .UNSPECIFIED., .F., .F.,
 ( 4, 2, 2, 2, 2, 2, 4 ),
 ( 0.0008179948676130699859, 0.001094431477128116623, 0.001370868086643163477, 0.001647304696158210114, 0.001923741305673259136, 0.002476614524703403802, 0.003029487743733548684 ),
 .UNSPECIFIED. ) ;
#52932 = CARTESIAN_POINT ( 'NONE',  ( 186.4974067573569414, 258.2722711272355127, 3.096644213909161003 ) ) ;
#52933 = CARTESIAN_POINT ( 'NONE',  ( 160.6901349803147809, 282.6678928203291434, -6.515548818033365386 ) ) ;
#52934 = CARTESIAN_POINT ( 'NONE',  ( 79.73556474071195055, 44.84470626076887356, 11.43605411104022096 ) ) ;
#52935 = DIRECTION ( 'NONE',  ( 0.8660254037844394848, 0.4999999999999986122, 0.000000000000000000 ) ) ;
#52936 = CARTESIAN_POINT ( 'NONE',  ( 170.9161164754127924, 255.3377101464579937, 11.24084812399238231 ) ) ;
#52937 = CARTESIAN_POINT ( 'NONE',  ( 193.7393920959428613, 263.3242207741936340, -0.7651321868841867158 ) ) ;
#52938 = VERTEX_POINT ( 'NONE', #10997 ) ;
#52940 = EDGE_CURVE ( 'NONE', #67772, #22139, #81912, .T. ) ;
#52939 = CARTESIAN_POINT ( 'NONE',  ( 183.5431746618634747, 272.4062028040541463, -16.12888619052139205 ) ) ;
#52941 = VECTOR ( 'NONE', #89213, 1000.000000000000000 ) ;
#52942 = CARTESIAN_POINT ( 'NONE',  ( 86.70911053808110580, 46.89117940024963360, 10.21290512048939547 ) ) ;
#52943 = CARTESIAN_POINT ( 'NONE',  ( -58.10760318826260118, 36.06970723555269842, -10.00000000000000000 ) ) ;
#52944 = CARTESIAN_POINT ( 'NONE',  ( -2.160980794731627519, 182.8927522451419634, 2.944929066748280225E-16 ) ) ;
#52945 = EDGE_CURVE ( 'NONE', #20189, #36064, #97625, .T. ) ;
#52946 = CARTESIAN_POINT ( 'NONE',  ( 193.8848781386269309, 267.1185884883711879, -11.59377028749509364 ) ) ;
#52947 = EDGE_CURVE ( 'NONE', #100252, #51318, #10724, .T. ) ;
#52948 = CARTESIAN_POINT ( 'NONE',  ( 171.4375308913269009, 279.6678964921788975, -14.69119404553828367 ) ) ;
#52949 = CARTESIAN_POINT ( 'NONE',  ( 163.6998542325049755, 247.1105306081193760, -8.966021225103816050 ) ) ;
#52950 = CARTESIAN_POINT ( 'NONE',  ( 72.12653191652874796, 72.33473008883520095, 0.9717078169766214524 ) ) ;
#52951 = CARTESIAN_POINT ( 'NONE',  ( 72.99805664120070503, 70.78149395872682703, 8.185774945494646460 ) ) ;
#52953 = CARTESIAN_POINT ( 'NONE',  ( 113.6157903772485298, 229.7365022471902023, -10.00000000000009237 ) ) ;
#52952 = CARTESIAN_POINT ( 'NONE',  ( -12.32793173735119652, 169.8149278399160664, 9.188101187500093303 ) ) ;
#52954 = CARTESIAN_POINT ( 'NONE',  ( 58.82164138842261991, 214.7677522451419350, -5.000000000000047962 ) ) ;
#52955 = ORIENTED_EDGE ( 'NONE', *, *, #92160, .T. ) ;
#52956 = EDGE_CURVE ( 'NONE', #45286, #99390, #78422, .T. ) ;
#52957 = ORIENTED_EDGE ( 'NONE', *, *, #3177, .T. ) ;
#52958 = CARTESIAN_POINT ( 'NONE',  ( 47.54560441532652959, 78.55524412553474178, -10.00000000000000000 ) ) ;
#52959 = CYLINDRICAL_SURFACE ( 'NONE', #69041, 17.82106496071139645 ) ;
#52960 = CARTESIAN_POINT ( 'NONE',  ( 171.7868853588355194, 289.4288941846863850, 2.650751707507049915 ) ) ;
#52961 = CARTESIAN_POINT ( 'NONE',  ( 17.38248943320504836, 35.13769309531819829, -10.00000000000000000 ) ) ;
#52962 = CARTESIAN_POINT ( 'NONE',  ( 162.5139888333388001, 249.1645097304130445, -10.50570364880316987 ) ) ;
#52963 = CARTESIAN_POINT ( 'NONE',  ( 83.32045823979383670, 44.28835298952803612, 8.667801982703636554 ) ) ;
#52964 = DIRECTION ( 'NONE',  ( 1.000000000000000000, 0.000000000000000000, 0.000000000000000000 ) ) ;
#52965 = CARTESIAN_POINT ( 'NONE',  ( 16.08835327644320401, 192.3464784336661637, 1.353441290958777525E-15 ) ) ;
#52966 = CARTESIAN_POINT ( 'NONE',  ( 126.7777458412893026, 237.8768266524160140, -9.188101187500091527 ) ) ;
#52967 = CARTESIAN_POINT ( 'NONE',  ( 180.8060382252356817, 293.0948058857328533, -6.206326745275219103 ) ) ;
#52968 = DIRECTION ( 'NONE',  ( -0.4755282581475737680, 0.8236391035463299648, -0.3090169943749573878 ) ) ;
#52969 = CARTESIAN_POINT ( 'NONE',  ( 75.58214075417596689, 65.23491603964201602, 14.35294216029143399 ) ) ;
#52970 = B_SPLINE_CURVE_WITH_KNOTS ( 'NONE', 3,
 ( #47125, #86196, #24827, #17223, #2554, #48131, #32436, #94272, #33437, #8141, #69922, #98770, #58239, #13167, #29352, #6550 ),
 .UNSPECIFIED., .F., .F.,
 ( 4, 1, 2, 2, 2, 1, 2, 2, 4 ),
 ( 0.000000000000000000, 0.1250000000000044964, 0.1875000000000050238, 0.2500000000000055511, 0.5000000000000083267, 0.6250000000000118794, 0.6875000000000123235, 0.7500000000000108802, 1.000000000000000000 ),
 .UNSPECIFIED. ) ;
#52971 = DIRECTION ( 'NONE',  ( 0.4999999999999998890, -0.8660254037844385966, 0.000000000000000000 ) ) ;
#52972 = VECTOR ( 'NONE', #39377, 1000.000000000000114 ) ;
#52973 = CARTESIAN_POINT ( 'NONE',  ( 76.68665551218811061, 54.72605516139766024, -16.09894948477438703 ) ) ;
#52974 = VECTOR ( 'NONE', #28575, 1000.000000000000000 ) ;
#52975 = CARTESIAN_POINT ( 'NONE',  ( -22.42236680055709641, 157.8615022471902591, 0.000000000000000000 ) ) ;
#52976 = LINE ( 'NONE', #100097, #35154 ) ;
#52977 = CARTESIAN_POINT ( 'NONE',  ( 188.2922251827820332, 283.6369852287460276, 16.32093764900332644 ) ) ;
#52978 = CARTESIAN_POINT ( 'NONE',  ( 165.0526092925929333, 249.7680750122055997, -10.69339827416780331 ) ) ;
#52979 = CARTESIAN_POINT ( 'NONE',  ( 186.8617808892419987, 298.9052062963050389, -0.5998036538631226211 ) ) ;
#52980 = CARTESIAN_POINT ( 'NONE',  ( 70.65108737845197595, 70.93011541185489932, 3.799750337262588040 ) ) ;
#52981 = CARTESIAN_POINT ( 'NONE',  ( 184.0948723531174096, 268.2408243536854116, -15.81992226484194752 ) ) ;
#52982 = CARTESIAN_POINT ( 'NONE',  ( -65.00000000000000000, 93.06504152958497400, 54.99999999999999289 ) ) ;
#52983 = AXIS2_PLACEMENT_3D ( 'NONE', #80869, #58008, #34702 ) ;
#52984 = CARTESIAN_POINT ( 'NONE',  ( 82.15581729306063608, 41.47318868828376281, -5.933381251846729931 ) ) ;
#52985 = EDGE_CURVE ( 'NONE', #48830, #47755, #3401, .T. ) ;
#52986 = CARTESIAN_POINT ( 'NONE',  ( 89.59260651841245249, 222.5333772461660544, 9.188101187500095079 ) ) ;
#52987 = CARTESIAN_POINT ( 'NONE',  ( 3.479571460297436136, 22.98502408145589726, -5.678558825948271327 ) ) ;
#52988 = CARTESIAN_POINT ( 'NONE',  ( 68.12716324602396867, 65.77153025955813348, 10.88064167488197143 ) ) ;
#52989 = CYLINDRICAL_SURFACE ( 'NONE', #88948, 10.00000000000001066 ) ;
#52991 = CARTESIAN_POINT ( 'NONE',  ( 85.28284199416806644, 42.68018856290509433, -2.168919532025619379 ) ) ;
#52990 = CARTESIAN_POINT ( 'NONE',  ( 157.2744851780909414, 258.2395962677452985, 18.17792129701959070 ) ) ;
#52992 = CARTESIAN_POINT ( 'NONE',  ( 202.9173117703535354, 271.9582023543367768, -9.750645975005012289 ) ) ;
#52993 = LINE ( 'NONE', #7906, #37410 ) ;
#52994 = CARTESIAN_POINT ( 'NONE',  ( 149.9292047088740674, 271.6423542473470434, -11.68677213707093010 ) ) ;
#52995 = CARTESIAN_POINT ( 'NONE',  ( 130.3409059842875877, 239.3927522451417929, -10.00000000000009237 ) ) ;
#52996 = CARTESIAN_POINT ( 'NONE',  ( 171.9845623806598667, 285.9329635774786880, -11.40154151993822040 ) ) ;
#52997 = ORIENTED_EDGE ( 'NONE', *, *, #39960, .T. ) ;
#52998 = CARTESIAN_POINT ( 'NONE',  ( 29.31840136419365805, 25.43085787977764056, -9.188101187500008038 ) ) ;
#52999 = CIRCLE ( 'NONE', #99952, 5.000000000000116351 ) ;
#53000 = CARTESIAN_POINT ( 'NONE',  ( -19.65312891409030271, 93.06504152958497400, -10.00000000000000888 ) ) ;
#53001 = CARTESIAN_POINT ( 'NONE',  ( 192.6789561813392595, 296.9172536750198219, -11.84591848451790952 ) ) ;
#53002 = CARTESIAN_POINT ( 'NONE',  ( 149.4456112649506281, 271.7996036513546869, -12.95648166494593667 ) ) ;
#53003 = VERTEX_POINT ( 'NONE', #74305 ) ;
#53004 = CARTESIAN_POINT ( 'NONE',  ( 70.36717637110562862, 61.12986366949047579, 14.33409245634332585 ) ) ;
#53005 = CARTESIAN_POINT ( 'NONE',  ( 198.5966822647444587, 286.6674514332866579, 17.25284514431582750 ) ) ;
#53006 = CARTESIAN_POINT ( 'NONE',  ( 180.5583831666531580, 263.2404611678256288, -12.85138873749756705 ) ) ;
#53007 = CARTESIAN_POINT ( 'NONE',  ( 173.2310685956476561, 253.5757068955384455, -9.200971831753770758 ) ) ;
#53008 = CARTESIAN_POINT ( 'NONE',  ( 192.0332533962074706, 298.0356437054567778, 11.70630383928353346 ) ) ;
#53009 = AXIS2_PLACEMENT_3D ( 'NONE', #44867, #5888, #67180 ) ;
#53010 = ORIENTED_EDGE ( 'NONE', *, *, #6634, .T. ) ;
#53011 = CARTESIAN_POINT ( 'NONE',  ( 73.10017469210082197, 69.78597432261236122, 9.621008654245756020 ) ) ;
#53012 = EDGE_LOOP ( 'NONE', ( #57739, #71402, #37712, #94055 ) ) ;
#53013 = CARTESIAN_POINT ( 'NONE',  ( 167.6676185881502477, 249.8298146214289943, 6.804182726411844406 ) ) ;
#53014 = CARTESIAN_POINT ( 'NONE',  ( 185.2439515868709350, 292.7630553371902806, -10.53029436427169507 ) ) ;
#53016 = ADVANCED_FACE ( 'NONE', ( #74795 ), #35768, .T. ) ;
#53015 = VERTEX_POINT ( 'NONE', #4886 ) ;
#53017 = CARTESIAN_POINT ( 'NONE',  ( 177.7634369230092091, 252.8608366103077856, -4.270187854574569275E-12 ) ) ;
#53018 = CARTESIAN_POINT ( 'NONE',  ( -15.01183432020139286, 145.0260834800747602, 0.000000000000000000 ) ) ;
#53019 = CARTESIAN_POINT ( 'NONE',  ( 190.5241654256948607, 278.7784361898847578, -16.51215372604780285 ) ) ;
#53020 = CARTESIAN_POINT ( 'NONE',  ( 192.7090279274952991, 296.8651678828053946, -12.06870058016504288 ) ) ;
#53021 = CARTESIAN_POINT ( 'NONE',  ( 188.0035612729766115, 279.2325960380115362, 17.82077010991123700 ) ) ;
#53022 = CARTESIAN_POINT ( 'NONE',  ( 41.28156676870083430, 26.76004757982093452, 5.678558825948272215 ) ) ;
#53023 = CARTESIAN_POINT ( 'NONE',  ( 164.2981700896163773, 253.9203781951923133, 14.63367134977796802 ) ) ;
#53025 = ADVANCED_FACE ( 'NONE', ( #26676 ), #18591, .T. ) ;
#53024 = CARTESIAN_POINT ( 'NONE',  ( 72.95814459691263210, 63.22145188874699073, -14.59938505178614498 ) ) ;
#53026 = CARTESIAN_POINT ( 'NONE',  ( -59.91704162537831735, 50.38415623799413368, 59.99999999999999289 ) ) ;
#53027 = EDGE_CURVE ( 'NONE', #38097, #71334, #48093, .T. ) ;
#53028 = ORIENTED_EDGE ( 'NONE', *, *, #45266, .T. ) ;
#53029 = EDGE_LOOP ( 'NONE', ( #18212, #50948, #83, #53543 ) ) ;
#53030 = DIRECTION ( 'NONE',  ( 0.000000000000000000, 0.000000000000000000, 1.000000000000000000 ) ) ;
#53031 = CARTESIAN_POINT ( 'NONE',  ( 169.3875294710099979, 269.0930465024870841, 17.17133023712824169 ) ) ;
#53033 = CARTESIAN_POINT ( 'NONE',  ( 165.5093369583051128, 275.0219039653110258, -16.16693748275729803 ) ) ;
#53032 = CARTESIAN_POINT ( 'NONE',  ( 164.4990934228277411, 245.7262077230798809, 6.470820838822735510 ) ) ;
#53034 = CARTESIAN_POINT ( 'NONE',  ( -19.62460808985983363, 93.20396705361855538, 59.99999999999999289 ) ) ;
#53035 = CARTESIAN_POINT ( 'NONE',  ( 186.0715527847238207, 298.7753624933060337, 1.084710433360843940 ) ) ;
#53036 = CARTESIAN_POINT ( 'NONE',  ( 202.6833006059332263, 277.5892208352050829, 15.45935665133711900 ) ) ;
#53037 = CARTESIAN_POINT ( 'NONE',  ( 190.3049670482083684, 301.0291234702190764, 0.2225066852051815758 ) ) ;
#53038 = CIRCLE ( 'NONE', #14212, 70.00000000000001421 ) ;
#53039 = CARTESIAN_POINT ( 'NONE',  ( 168.4778631746381734, 286.4770891300594258, -4.677790519826849902 ) ) ;
#53040 = CARTESIAN_POINT ( 'NONE',  ( 77.11998379669407200, 62.91817058770694615, -15.28160261259852959 ) ) ;
#53041 = CARTESIAN_POINT ( 'NONE',  ( 186.6454664138524606, 287.0855943654420344, -15.99430129440811754 ) ) ;
#53042 = CARTESIAN_POINT ( 'NONE',  ( 118.9835172072293403, 233.3768266524159856, -9.188101187500091527 ) ) ;
#53043 = EDGE_LOOP ( 'NONE', ( #25602, #65755, #41707, #82758, #39462, #48321 ) ) ;
#53045 = B_SPLINE_CURVE_WITH_KNOTS ( 'NONE', 3,
 ( #89814, #66960, #12798, #43661, #59343, #13292, #14265, #36556, #37546, #74604, #90321, #51783, #76568, #44644, #7149, #45157, #44152, #99873, #75087, #76095, #98390, #75578, #59857, #21373, #6669, #52260, #29959, #83201, #68452, #6164, #13765, #37061, #67967, #98885, #99380, #60836, #91797, #22360, #53258, #70978, #47643, #92789, #562, #48157, #77576, #8164, #16255, #85722 ),
 .UNSPECIFIED., .F., .F.,
 ( 4, 2, 2, 2, 2, 2, 2, 2, 2, 2, 2, 2, 2, 2, 2, 2, 2, 2, 2, 2, 2, 2, 2, 4 ),
 ( 0.002037292597442118790, 0.002480311735260100434, 0.002701821304169148719, 0.002923330873078197004, 0.003034085657532719846, 0.003144840441987242254, 0.003255595226441765529, 0.003366350010896287936, 0.003587859579805333619, 0.003809369148714379302, 0.004695407424350640097, 0.005581445699986900023, 0.006467483975623159950, 0.006910503113441253918, 0.007353522251259347019, 0.007464277035713889376, 0.007519654427941122390, 0.007575031820168354538, 0.007685786604622705208, 0.007796541389077054143, 0.008239560526894465498, 0.008682579664711875117, 0.008904089233620637173, 0.009125598802529399228 ),
 .UNSPECIFIED. ) ;
#53044 = CARTESIAN_POINT ( 'NONE',  ( 148.4608825321785446, 275.1491132871843206, -7.142904470870874434 ) ) ;
#53046 = CARTESIAN_POINT ( 'NONE',  ( 35.86231599663030067, 42.74646525600393687, 2.839279412974139660 ) ) ;
#53047 = CARTESIAN_POINT ( 'NONE',  ( 188.1090581172104805, 273.6250799618885026, 15.75090146302019889 ) ) ;
#53048 = VECTOR ( 'NONE', #42350, 1000.000000000000227 ) ;
#53049 = ORIENTED_EDGE ( 'NONE', *, *, #95857, .F. ) ;
#53050 = AXIS2_PLACEMENT_3D ( 'NONE', #75221, #98528, #5804 ) ;
#53051 = ORIENTED_EDGE ( 'NONE', *, *, #84417, .F. ) ;
#53052 = CARTESIAN_POINT ( 'NONE',  ( 74.16736989203016606, 68.80940149631990721, -11.31408104362165545 ) ) ;
#53054 = B_SPLINE_SURFACE_WITH_KNOTS ( 'NONE', 3, 1, ( 
 ( #52506, #53986 ),
 ( #21142, #91547 ),
 ( #92066, #76335 ),
 ( #67214, #44405 ),
 ( #37305, #68205 ),
 ( #22616, #24103 ),
 ( #94048, #2326 ),
 ( #16503, #47398 ),
 ( #78324, #24601 ),
 ( #71227, #48411 ),
 ( #25096, #9924 ),
 ( #40785, #96422 ),
 ( #77314, #23589 ),
 ( #31197, #93033 ),
 ( #20896, #67465 ),
 ( #4171, #65975 ),
 ( #12292, #75089 ),
 ( #6166, #74092 ),
 ( #52263, #29467 ),
 ( #27966, #89816 ),
 ( #37063, #60342 ),
 ( #50273, #58365 ),
 ( #89342, #58846 ),
 ( #4685, #82226 ),
 ( #14760, #71 ),
 ( #45642, #30459 ),
 ( #31945, #38038 ),
 ( #15744, #61351 ),
 ( #77578, #83709 ),
 ( #29962, #31446 ),
 ( #23847, #91799 ) ),
 .UNSPECIFIED., .F., .F., .F.,
 ( 4, 3, 3, 3, 3, 3, 3, 3, 3, 3, 4 ),
 ( 2, 2 ),
 ( 0.000000000000000000, 0.1122669598086783738, 0.2243161639709696786, 0.3396355846219157870, 0.4553962076585107988, 0.5677860799922528345, 0.6749047109689648716, 0.7773884377078369434, 0.8775581155834392133, 0.9782364162377953365, 1.000000000000000000 ),
 ( 0.000000000000000000, 1.000000000000000000 ),
 .UNSPECIFIED. ) ;
#53053 = CARTESIAN_POINT ( 'NONE',  ( 23.46864935082055226, 158.3759306620404743, 22.50000000000001776 ) ) ;
#53055 = CARTESIAN_POINT ( 'NONE',  ( 203.9648368022151601, 269.0477214045654364, 5.644613064108824574 ) ) ;
#53056 = CARTESIAN_POINT ( 'NONE',  ( 43.35468487962021555, 120.5828561944265687, 10.00000000000000000 ) ) ;
#53057 = ORIENTED_EDGE ( 'NONE', *, *, #53148, .T. ) ;
#53058 = CARTESIAN_POINT ( 'NONE',  ( 195.3331298895125201, 292.3200899603503444, 15.25153430865447390 ) ) ;
#53059 = PRESENTATION_LAYER_ASSIGNMENT (  '', '', ( #85513 ) ) ;
#53060 = ORIENTED_EDGE ( 'NONE', *, *, #51662, .F. ) ;
#53061 = EDGE_CURVE ( 'NONE', #80515, #87229, #20302, .T. ) ;
#53062 = CYLINDRICAL_SURFACE ( 'NONE', #49506, 10.00000000000001066 ) ;
#53063 = VERTEX_POINT ( 'NONE', #14939 ) ;
#53064 = DIRECTION ( 'NONE',  ( -0.8660254037844363761, -0.5000000000000039968, 0.000000000000000000 ) ) ;
#53065 = VECTOR ( 'NONE', #66807, 1000.000000000000000 ) ;
#53066 = CARTESIAN_POINT ( 'NONE',  ( 195.3876898667038517, 265.2072342455722946, 4.415210603996274408 ) ) ;
#53067 = DIRECTION ( 'NONE',  ( -0.000000000000000000, -0.000000000000000000, 1.000000000000000000 ) ) ;
#53068 = CARTESIAN_POINT ( 'NONE',  ( 67.12420765758699304, 68.84019135822225621, -3.751863413797577707 ) ) ;
#53070 = CARTESIAN_POINT ( 'NONE',  ( 157.0463493773329162, 280.1323627575716273, 5.834371214722025911 ) ) ;
#53069 = CARTESIAN_POINT ( 'NONE',  ( 151.3011447763744570, 269.1990464485573966, 14.21186556778774168 ) ) ;
#53071 = CARTESIAN_POINT ( 'NONE',  ( 152.9607371460978129, 265.7112270302071124, -16.17698032818104537 ) ) ;
#53072 = ORIENTED_EDGE ( 'NONE', *, *, #7315, .F. ) ;
#53073 = CARTESIAN_POINT ( 'NONE',  ( 190.1693911629507738, 301.2639477917662703, -5.112716700269980485 ) ) ;
#53075 = CARTESIAN_POINT ( 'NONE',  ( 72.62183550608976645, 66.39385476340312664, 12.02826447586101644 ) ) ;
#53074 = B_SPLINE_SURFACE_WITH_KNOTS ( 'NONE', 3, 1, ( 
 ( #83855, #60488 ),
 ( #98033, #5327 ),
 ( #14421, #58988 ),
 ( #20037, #76237 ),
 ( #58505, #21523 ),
 ( #51924, #52406 ),
 ( #99030, #82864 ),
 ( #91447, #68603 ),
 ( #81860, #20535 ),
 ( #75731, #89478 ),
 ( #29616, #82376 ),
 ( #22008, #13917 ),
 ( #50910, #12437 ),
 ( #12946, #13437 ),
 ( #75232, #43806 ),
 ( #43304, #74252 ),
 ( #5814, #74747 ),
 ( #4838, #36204 ),
 ( #35718, #67609 ),
 ( #44795, #66617 ),
 ( #62479, #78219 ),
 ( #100026, #206 ),
 ( #7302, #46804 ),
 ( #15896, #92448 ),
 ( #8311, #91960 ),
 ( #86365, #70600 ),
 ( #69601, #77206 ),
 ( #78720, #61497 ),
 ( #14898, #8804 ),
 ( #93444, #55380 ),
 ( #39672, #69099 ),
 ( #53885, #85349 ),
 ( #30110, #7811 ),
 ( #1211, #70092 ) ),
 .UNSPECIFIED., .T., .F., .F.,
 ( 4, 2, 2, 2, 2, 2, 2, 2, 2, 2, 2, 2, 2, 2, 2, 2, 4 ),
 ( 2, 2 ),
 ( 0.000000000000000000, 0.06250000000000000000, 0.1250000000000000000, 0.1875000000000000000, 0.2500000000000000000, 0.3125000000000000000, 0.3750000000000000000, 0.4375000000000000000, 0.5000000000000000000, 0.5625000000000000000, 0.6250000000000000000, 0.6875000000000000000, 0.7500000000000000000, 0.8125000000000000000, 0.8750000000000000000, 0.9375000000000000000, 1.000000000000000000 ),
 ( 0.000000000000000000, 1.000000000000000000 ),
 .UNSPECIFIED. ) ;
#53076 = CARTESIAN_POINT ( 'NONE',  ( 189.6282526764183842, 264.1678331799054149, -9.198679507049698501 ) ) ;
#53077 = EDGE_CURVE ( 'NONE', #8604, #40825, #76753, .T. ) ;
#53078 = CARTESIAN_POINT ( 'NONE',  ( -19.65312891409030271, 93.06504152958497400, 10.00000000000000888 ) ) ;
#53079 = CARTESIAN_POINT ( 'NONE',  ( 189.4677816960851544, 269.1499146606108752, -14.21597690008461257 ) ) ;
#53080 = CARTESIAN_POINT ( 'NONE',  ( 71.72870690310715247, 72.16142621409359492, 3.283488654313281963 ) ) ;
#53081 = CARTESIAN_POINT ( 'NONE',  ( 84.68957885917166095, 45.88504986743041059, 9.714594249952936522 ) ) ;
#53082 = CARTESIAN_POINT ( 'NONE',  ( 87.33294734268929460, 44.88192199842171703, 6.808005391826775110 ) ) ;
#53083 = CARTESIAN_POINT ( 'NONE',  ( 191.1909263933080751, 283.2087925905971701, -16.62349056250532797 ) ) ;
#53084 = AXIS2_PLACEMENT_3D ( 'NONE', #25567, #17980, #81306 ) ;
#53085 = CARTESIAN_POINT ( 'NONE',  ( 82.69574664279603837, 54.03060105484253484, -15.86596363536033039 ) ) ;
#53086 = CARTESIAN_POINT ( 'NONE',  ( 73.40858323730823543, 219.3149278399160664, 9.188101187500093303 ) ) ;
#53087 = CARTESIAN_POINT ( 'NONE',  ( 40.82928596147627331, 60.38352576601455723, -10.00000000000000000 ) ) ;
#53088 = CARTESIAN_POINT ( 'NONE',  ( 146.9700173529739970, 276.0874580858064746, -5.099093031535578469 ) ) ;
#53089 = CARTESIAN_POINT ( 'NONE',  ( 163.3409975114459485, 247.7320886816312111, -10.96358124877083640 ) ) ;
#53090 = CARTESIAN_POINT ( 'NONE',  ( 66.44089328032605124, 67.93038546761928842, 6.554334301446774091 ) ) ;
#53091 = CARTESIAN_POINT ( 'NONE',  ( 207.4541616930702617, 271.3258470364304458, -6.834942797545373594 ) ) ;
#53092 = DIRECTION ( 'NONE',  ( -0.4999999999999987788, 0.8660254037844392627, 0.000000000000000000 ) ) ;
#53094 = CARTESIAN_POINT ( 'NONE',  ( -20.95323109343049239, 95.11688455923321328, 45.19937630303414977 ) ) ;
#53093 = CARTESIAN_POINT ( 'NONE',  ( 73.41757211889691348, 69.17622104212573220, -9.975606977152791544 ) ) ;
#53095 = CARTESIAN_POINT ( 'NONE',  ( 1.988115337714555064, 24.08080186712590276, -3.090169943749475845 ) ) ;
#53096 = CARTESIAN_POINT ( 'NONE',  ( 41.55205903992003158, 29.15404122711137447, 8.090169943749479842 ) ) ;
#53097 = B_SPLINE_CURVE_WITH_KNOTS ( 'NONE', 3,
 ( #16653, #39431, #94197, #93697 ),
 .UNSPECIFIED., .F., .F.,
 ( 4, 4 ),
 ( 0.006120916150806869280, 0.01419598930506990771 ),
 .UNSPECIFIED. ) ;
#53098 = DIRECTION ( 'NONE',  ( -0.8660254037844387076, -0.4999999999999998890, -0.000000000000000000 ) ) ;
#53099 = CARTESIAN_POINT ( 'NONE',  ( 21.15788363470973366, 37.74176219324819215, -10.00000000000000000 ) ) ;
#53100 = CARTESIAN_POINT ( 'NONE',  ( 71.78913936505468030, 72.20160104369585952, 3.260718063500208430 ) ) ;
#53101 = EDGE_CURVE ( 'NONE', #36219, #9880, #84393, .T. ) ;
#53102 = CARTESIAN_POINT ( 'NONE',  ( 31.65035466828360100, 179.8923013555409796, 4.594050593750050204 ) ) ;
#53103 = EDGE_CURVE ( 'NONE', #18680, #78112, #75924, .T. ) ;
#53104 = CARTESIAN_POINT ( 'NONE',  ( 55.46605327235566563, 193.6423013555410080, -4.594050593750043987 ) ) ;
#53105 = CARTESIAN_POINT ( 'NONE',  ( 196.0395593785976018, 291.0965181932902510, 15.97855489120023087 ) ) ;
#53106 = CARTESIAN_POINT ( 'NONE',  ( 199.6508179728032815, 277.6496187303415013, 15.20395581979866861 ) ) ;
#53107 = VECTOR ( 'NONE', #30944, 1000.000000000000000 ) ;
#53108 = PLANE ( 'NONE',  #62687 ) ;
#53109 = CARTESIAN_POINT ( 'NONE',  ( 145.1264855360895751, 254.5958772461660544, -9.188101187500095079 ) ) ;
#53110 = CARTESIAN_POINT ( 'NONE',  ( 48.83545950068980801, 192.8768266524159856, -9.188101187500093303 ) ) ;
#53111 = CARTESIAN_POINT ( 'NONE',  ( 18.86656744736070124, 32.93396525600390845, 2.839279412974139660 ) ) ;
#53112 = CARTESIAN_POINT ( 'NONE',  ( 171.0170784859788000, 287.1471327868096637, 7.033863407631240960 ) ) ;
#53113 = CARTESIAN_POINT ( 'NONE',  ( 149.5390997184345281, 271.6376768999995761, -11.52989534384373016 ) ) ;
#53114 = CARTESIAN_POINT ( 'NONE',  ( 45.82169850708434922, 28.58380873178791504, 6.180339887498953466 ) ) ;
#53115 = CARTESIAN_POINT ( 'NONE',  ( 205.2121761402296443, 275.2090799237855094, -14.05269615702442465 ) ) ;
#53116 = CARTESIAN_POINT ( 'NONE',  ( 77.33488381500329467, 63.19222936695796733, 15.59520410795408196 ) ) ;
#53117 = CARTESIAN_POINT ( 'NONE',  ( 175.4120841302475071, 291.3965204062699286, 1.943475587933318982 ) ) ;
#53118 = VECTOR ( 'NONE', #78609, 1000.000000000000000 ) ;
#53119 = FACE_OUTER_BOUND ( 'NONE', #85354, .T. ) ;
#53120 = CARTESIAN_POINT ( 'NONE',  ( 182.3870610246802926, 280.6993384506884581, -16.15232590179551053 ) ) ;
#53121 = CARTESIAN_POINT ( 'NONE',  ( 149.1618037898029172, 275.5005916956379792, 7.607269316218690847 ) ) ;
#53122 = DIRECTION ( 'NONE',  ( 1.000000000000000000, 0.000000000000000000, 0.000000000000000000 ) ) ;
#53123 = VECTOR ( 'NONE', #31440, 1000.000000000000114 ) ;
#53125 =( BOUNDED_CURVE ( )  B_SPLINE_CURVE ( 2, ( #43969, #42962, #13596, #74907, #90643, #67280, #26797, #73904, #88659 ),
 .UNSPECIFIED., .F., .T. ) 
 B_SPLINE_CURVE_WITH_KNOTS ( ( 3, 2, 2, 2, 3 ),
 ( 0.8185483870967742437, 0.8198924731182796188, 0.8225806451612903691, 0.8252688172043011194, 0.8266129032258064946 ),
 .UNSPECIFIED. ) 
 CURVE ( )  GEOMETRIC_REPRESENTATION_ITEM ( )  RATIONAL_B_SPLINE_CURVE ( ( 0.9330127018922194093, 0.9330127018922194093, 1.000000000000000000, 0.8660254037844387076, 1.000000000000000000, 0.8660254037844387076, 1.000000000000000000, 0.9330127018922194093, 0.9330127018922194093 ) ) 
 REPRESENTATION_ITEM ( '' )  );
#53124 = CARTESIAN_POINT ( 'NONE',  ( 99.25420243115655694, 228.1115022471902307, 10.00000000000009592 ) ) ;
#53126 = CARTESIAN_POINT ( 'NONE',  ( 200.3765029811139584, 283.5847115241710981, 16.85207472104531590 ) ) ;
#53127 = CARTESIAN_POINT ( 'NONE',  ( 168.5165758536381873, 288.6662250410414003, -0.7359078604044604344 ) ) ;
#53128 = ORIENTED_EDGE ( 'NONE', *, *, #74241, .T. ) ;
#53129 = CARTESIAN_POINT ( 'NONE',  ( 61.98804677278346986, 206.5958772461660828, -9.188101187500095079 ) ) ;
#53130 = ORIENTED_EDGE ( 'NONE', *, *, #44772, .F. ) ;
#53131 = FACE_OUTER_BOUND ( 'NONE', #40174, .T. ) ;
#53132 = CARTESIAN_POINT ( 'NONE',  ( 190.2648877593310317, 301.0985428348857340, -4.426259207433023590 ) ) ;
#53133 = CARTESIAN_POINT ( 'NONE',  ( 183.8043731368310603, 268.5938253857621589, 16.29461355553033997 ) ) ;
#53134 = ORIENTED_EDGE ( 'NONE', *, *, #98609, .T. ) ;
#53135 = LINE ( 'NONE', #21252, #87880 ) ;
#53136 = CARTESIAN_POINT ( 'NONE',  ( 79.32826970724438809, 45.68448480011694812, -12.90705109908815906 ) ) ;
#53137 = CARTESIAN_POINT ( 'NONE',  ( 194.8432095198904221, 293.1686569321988145, -14.74101036184996616 ) ) ;
#53138 = CARTESIAN_POINT ( 'NONE',  ( 177.2942696745171247, 274.8600937621219487, -17.06932773013303262 ) ) ;
#53139 = LINE ( 'NONE', #98772, #86191 ) ;
#53140 = CARTESIAN_POINT ( 'NONE',  ( 156.7173554537088194, 259.2045732567815435, 17.96992492779905959 ) ) ;
#53141 = ORIENTED_EDGE ( 'NONE', *, *, #42937, .T. ) ;
#53142 = CARTESIAN_POINT ( 'NONE',  ( 22.66683848874176022, 18.80170272979926693, 7.433330006724137462 ) ) ;
#53143 = CARTESIAN_POINT ( 'NONE',  ( 75.31615383312099254, 56.31091532350969686, 16.14109913096982396 ) ) ;
#53144 = CARTESIAN_POINT ( 'NONE',  ( 71.17509266960550462, 70.27285362950316028, -6.380606852064568457 ) ) ;
#53145 = CARTESIAN_POINT ( 'NONE',  ( 172.3136996429396675, 274.9537642369339778, 17.36053840881438859 ) ) ;
#53146 = ORIENTED_EDGE ( 'NONE', *, *, #40273, .T. ) ;
#53148 = EDGE_CURVE ( 'NONE', #73330, #48184, #34787, .T. ) ;
#53147 = PLANE ( 'NONE',  #85439 ) ;
#53149 = CARTESIAN_POINT ( 'NONE',  ( 206.1062572280473546, 273.6604860535989587, -9.773577984388410300 ) ) ;
#53150 = EDGE_CURVE ( 'NONE', #57780, #19194, #50590, .T. ) ;
#53151 = ORIENTED_EDGE ( 'NONE', *, *, #61268, .F. ) ;
#53152 = ORIENTED_EDGE ( 'NONE', *, *, #49606, .F. ) ;
#53153 = CARTESIAN_POINT ( 'NONE',  ( 79.14672556360194733, 50.15886727742795870, -14.80520554370081854 ) ) ;
#53155 = DIRECTION ( 'NONE',  ( 1.000000000000000000, 0.000000000000000000, 0.000000000000000000 ) ) ;
#53154 = CARTESIAN_POINT ( 'NONE',  ( 163.1747956065615028, 283.6804097174056665, -3.098853972138146506 ) ) ;
#53156 = CARTESIAN_POINT ( 'NONE',  ( 163.2256942281324541, 247.9317998266098471, -9.780520296312531059 ) ) ;
#53157 = CARTESIAN_POINT ( 'NONE',  ( 40.96864935082037817, 128.0650415295850735, 10.00000000000000888 ) ) ;
#53158 = EDGE_CURVE ( 'NONE', #77633, #70724, #39718, .T. ) ;
#53159 = CARTESIAN_POINT ( 'NONE',  ( 198.4264492142971221, 286.9623037257889564, 17.00126466006521397 ) ) ;
#53160 = CARTESIAN_POINT ( 'NONE',  ( 161.6806056053058853, 263.3655989262382491, -17.06081503136075028 ) ) ;
#53161 = ADVANCED_FACE ( 'NONE', ( #86916 ), #35193, .F. ) ;
#53162 = CARTESIAN_POINT ( 'NONE',  ( 128.5637496887121927, 245.0333772461660544, 9.188101187500095079 ) ) ;
#53163 = CARTESIAN_POINT ( 'NONE',  ( 177.1315819580615027, 269.3555979632168942, 16.09210694347321180 ) ) ;
#53164 = CARTESIAN_POINT ( 'NONE',  ( 195.3624787578944222, 290.3824063481519602, -16.76522224015156226 ) ) ;
#53165 = B_SPLINE_CURVE_WITH_KNOTS ( 'NONE', 3,
 ( #36413, #6022, #45995, #44003 ),
 .UNSPECIFIED., .F., .F.,
 ( 4, 4 ),
 ( 0.04550866176299273036, 0.04887066958154935581 ),
 .UNSPECIFIED. ) ;
#53166 = CARTESIAN_POINT ( 'NONE',  ( 62.52896555438372417, 219.1589784336661637, -6.496448406907675876E-16 ) ) ;
#53167 = ORIENTED_EDGE ( 'NONE', *, *, #30478, .T. ) ;
#53168 = CARTESIAN_POINT ( 'NONE',  ( 173.2130610185342334, 264.9127892606105661, 17.04138321073628148 ) ) ;
#53169 = CARTESIAN_POINT ( 'NONE',  ( 79.37503556926780846, 45.76590238620419626, 12.94519473234442231 ) ) ;
#53170 = VECTOR ( 'NONE', #6865, 1000.000000000000000 ) ;
#53171 = ORIENTED_EDGE ( 'NONE', *, *, #14609, .T. ) ;
#53172 = PLANE ( 'NONE',  #52638 ) ;
#53173 = ORIENTED_EDGE ( 'NONE', *, *, #28011, .F. ) ;
#53174 = ORIENTED_EDGE ( 'NONE', *, *, #34910, .F. ) ;
#53175 = FACE_BOUND ( 'NONE', #85142, .T. ) ;
#53176 = CARTESIAN_POINT ( 'NONE',  ( 66.72442129515968645, 67.86934472784028571, 6.990068089071483470 ) ) ;
#53177 = CARTESIAN_POINT ( 'NONE',  ( 197.8265573649375142, 286.7779075425210635, 16.93047688356437419 ) ) ;
#53178 = CARTESIAN_POINT ( 'NONE',  ( 191.2111338740054975, 299.4595964878050154, -9.718193530796334301 ) ) ;
#53179 = PLANE ( 'NONE',  #9458 ) ;
#53180 = CARTESIAN_POINT ( 'NONE',  ( 155.4186054393023255, 261.4540742680644598, 17.05753227160644769 ) ) ;
#53181 = CARTESIAN_POINT ( 'NONE',  ( 71.53524002805265525, 66.98255073825953332, 10.96953089586062546 ) ) ;
#53182 = VERTEX_POINT ( 'NONE', #81297 ) ;
#53183 = LINE ( 'NONE', #38469, #5838 ) ;
#53184 = CIRCLE ( 'NONE', #37042, 0.1418229129680863287 ) ;
#53185 = ORIENTED_EDGE ( 'NONE', *, *, #35547, .F. ) ;
#53186 = CARTESIAN_POINT ( 'NONE',  ( 76.07519723137014012, 51.47020756999099689, -16.16347409184471573 ) ) ;
#53187 = VECTOR ( 'NONE', #97494, 1000.000000000000114 ) ;
#53188 = DIRECTION ( 'NONE',  ( -0.5372068985985075651, -0.8434505012732950169, 0.000000000000000000 ) ) ;
#53189 = AXIS2_PLACEMENT_3D ( 'NONE', #3962, #35855, #82517 ) ;
#53190 = CARTESIAN_POINT ( 'NONE',  ( 206.3106310032756596, 273.3065002911688453, 10.17860425536756175 ) ) ;
#53191 = CARTESIAN_POINT ( 'NONE',  ( 199.0159380930694226, 281.1150505206304615, 17.25796289221863233 ) ) ;
#53192 = CARTESIAN_POINT ( 'NONE',  ( 162.7773628798197194, 261.4912393770340486, 17.07172388677674491 ) ) ;
#53193 = CARTESIAN_POINT ( 'NONE',  ( 137.8192226437758450, 256.5024278399160949, -9.188101187500093303 ) ) ;
#53194 = ORIENTED_EDGE ( 'NONE', *, *, #83832, .F. ) ;
#53195 = CARTESIAN_POINT ( 'NONE',  ( -19.51267218670369985, 93.08467941069811502, 59.99999999999999289 ) ) ;
#53196 = CARTESIAN_POINT ( 'NONE',  ( 182.1659242776092924, 257.5230415930786876, 6.683065253742526579 ) ) ;
#53197 = CARTESIAN_POINT ( 'NONE',  ( 80.25013155102732298, 44.94815484363307689, -11.26109297976839052 ) ) ;
#53198 = CARTESIAN_POINT ( 'NONE',  ( 201.2949053258274148, 281.9939920013367782, -18.04004790210578335 ) ) ;
#53199 = CARTESIAN_POINT ( 'NONE',  ( 72.87908800440395396, 70.94240749453250316, 7.824389999597036294 ) ) ;
#53200 = CARTESIAN_POINT ( 'NONE',  ( 178.8595466249924755, 265.0989930076032124, -16.03772641351113748 ) ) ;
#53201 = ORIENTED_EDGE ( 'NONE', *, *, #86734, .T. ) ;
#53202 = CARTESIAN_POINT ( 'NONE',  ( 196.0966283236085417, 264.7156248001706444, 5.418721370419348204 ) ) ;
#53203 = AXIS2_PLACEMENT_3D ( 'NONE', #98024, #34707, #50902 ) ;
#53204 = CARTESIAN_POINT ( 'NONE',  ( 181.8578577305817419, 291.4847624314589325, 9.597431263652177691 ) ) ;
#53205 = B_SPLINE_CURVE_WITH_KNOTS ( 'NONE', 3,
 ( #18734, #64834, #27820, #81075 ),
 .UNSPECIFIED., .F., .F.,
 ( 4, 4 ),
 ( 7.943821393640659065E-17, 0.006184891004078511487 ),
 .UNSPECIFIED. ) ;
#53206 = CARTESIAN_POINT ( 'NONE',  ( 87.97782240006738164, 43.76496563450900368, 2.369043524150745927 ) ) ;
#53207 = CARTESIAN_POINT ( 'NONE',  ( 79.88561257828403939, 47.45582108751673189, 13.26507963048562289 ) ) ;
#53208 = CARTESIAN_POINT ( 'NONE',  ( 198.6294664808700077, 266.3094093603824604, 0.8324587486580483642 ) ) ;
#53209 = CARTESIAN_POINT ( 'NONE',  ( 195.5055827311261964, 264.2059424127278930, 0.8350436053642301681 ) ) ;
#53210 = VERTEX_POINT ( 'NONE', #96494 ) ;
#53211 = CARTESIAN_POINT ( 'NONE',  ( 146.7845206192450007, 276.4087478532630939, 4.443586170796542945 ) ) ;
#53212 = CARTESIAN_POINT ( 'NONE',  ( 186.7843925653488668, 282.2516066892422941, 17.48446008842761401 ) ) ;
#53213 = EDGE_CURVE ( 'NONE', #39058, #54972, #25105, .T. ) ;
#53214 = CIRCLE ( 'NONE', #87290, 70.00000000000001421 ) ;
#53215 = LINE ( 'NONE', #85152, #54996 ) ;
#53217 = CARTESIAN_POINT ( 'NONE',  ( 196.4589140796189213, 270.4767738285896712, 11.79566246125468254 ) ) ;
#53216 = CARTESIAN_POINT ( 'NONE',  ( 177.2746010927298812, 264.5551300243030255, -15.37364360889636750 ) ) ;
#53218 = CARTESIAN_POINT ( 'NONE',  ( 30.27384506023333444, 17.28848085856232331, 1.475505719884397138E-15 ) ) ;
#53219 = LINE ( 'NONE', #84170, #24065 ) ;
#53220 = DIRECTION ( 'NONE',  ( 0.4999999999999998890, -0.8660254037844385966, 0.000000000000000000 ) ) ;
#53221 = CARTESIAN_POINT ( 'NONE',  ( 16.60635795911645829, 31.36126292948894445, 6.180339887498949913 ) ) ;
#53222 = CARTESIAN_POINT ( 'NONE',  ( 198.5612432604688991, 286.7288335892616260, 18.30793681285053509 ) ) ;
#53223 = CARTESIAN_POINT ( 'NONE',  ( 147.1562325744354496, 245.7677522451417929, -5.000000000000041744 ) ) ;
#53224 = DIRECTION ( 'NONE',  ( -0.5435407515102096410, 0.8393827800519358950, 0.000000000000000000 ) ) ;
#53225 = VERTEX_POINT ( 'NONE', #26064 ) ;
#53226 = CARTESIAN_POINT ( 'NONE',  ( 66.90909321514121189, 68.17756947893454367, -6.600776075520579766 ) ) ;
#53227 = CARTESIAN_POINT ( 'NONE',  ( 73.09402281141575486, 70.66127457103814891, -7.741035114144303897 ) ) ;
#53228 = CARTESIAN_POINT ( 'NONE',  ( 151.2567985338353935, 268.6625352796243646, -15.71756535662528798 ) ) ;
#53229 = CARTESIAN_POINT ( 'NONE',  ( 8.456677953475336906, 181.8149278399161233, 9.188101187500093303 ) ) ;
#53230 = CARTESIAN_POINT ( 'NONE',  ( 181.5169748047240716, 275.4304238179468598, -16.43353661735662286 ) ) ;
#53231 = CARTESIAN_POINT ( 'NONE',  ( 19.12865694409072503, 32.81751292744056769, -6.180339887498951690 ) ) ;
#53232 = CARTESIAN_POINT ( 'NONE',  ( 76.88190494917691353, 52.40768971240707685, 16.25993826842571366 ) ) ;
#53233 = CARTESIAN_POINT ( 'NONE',  ( 170.3568046055088701, 270.8355684487424924, -16.86163208226229315 ) ) ;
#53234 = CARTESIAN_POINT ( 'NONE',  ( 72.13262339782576760, 71.82946044270117625, -3.914888389595029938 ) ) ;
#53235 = CARTESIAN_POINT ( 'NONE',  ( 130.9362984529373080, 239.7365022471902307, 10.00000000000009948 ) ) ;
#53236 = CARTESIAN_POINT ( 'NONE',  ( 175.5389217430812607, 253.4453625803252521, -3.600109118078927306 ) ) ;
#53237 = CARTESIAN_POINT ( 'NONE',  ( 187.4956075105807827, 259.3323774093973952, -0.7818960507064889320 ) ) ;
#53238 = CARTESIAN_POINT ( 'NONE',  ( 61.50992858288481813, 192.9865022471901739, 1.119607411625061291E-15 ) ) ;
#53239 = DIRECTION ( 'NONE',  ( 0.4999999999999992784, -0.8660254037844390407, 0.000000000000000000 ) ) ;
#53240 = CARTESIAN_POINT ( 'NONE',  ( 148.3707431749605234, 273.6613297946520902, 8.912574527564540716 ) ) ;
#53241 = AXIS2_PLACEMENT_3D ( 'NONE', #87356, #2687, #9276 ) ;
#53242 = CARTESIAN_POINT ( 'NONE',  ( 25.45277359850996390, 179.3768266524160140, -9.188101187500091527 ) ) ;
#53243 = CARTESIAN_POINT ( 'NONE',  ( 67.72263284813347184, 69.74190012044236653, -3.715451582779847328 ) ) ;
#53244 = DIRECTION ( 'NONE',  ( -0.8660254037844384856, -0.5000000000000001110, 0.000000000000000000 ) ) ;
#53245 = CARTESIAN_POINT ( 'NONE',  ( 35.77750112005064409, 38.84336893147759184, -7.433330006724137462 ) ) ;
#53246 = CARTESIAN_POINT ( 'NONE',  ( 202.0995849165119012, 279.2814632178312308, -15.97000401044184414 ) ) ;
#53247 = CARTESIAN_POINT ( 'NONE',  ( 207.2824254892180704, 271.6233028670009162, 6.274396967990798046 ) ) ;
#53248 = CARTESIAN_POINT ( 'NONE',  ( 185.4224844400474126, 266.5931547338063865, 13.20453509119197832 ) ) ;
#53249 = CARTESIAN_POINT ( 'NONE',  ( 162.5249628567144384, 281.0953062916516956, -10.43707322529907877 ) ) ;
#53250 = CARTESIAN_POINT ( 'NONE',  ( 160.3162220307800112, 280.5258973909593010, 9.471671026417038064 ) ) ;
#53251 = ITEM_DEFINED_TRANSFORMATION ( 'NONE', 'NONE', #44547,  #68784 ) ;
#53252 = CARTESIAN_POINT ( 'NONE',  ( 14.52983486323338802, 31.49540643055186706, 3.479690158560446702E-15 ) ) ;
#53253 = CARTESIAN_POINT ( 'NONE',  ( 190.4281805785508084, 300.8157113754859893, -1.233909217199055774 ) ) ;
#53254 = CARTESIAN_POINT ( 'NONE',  ( 72.03620616349491002, 59.26415205210582826, 15.85034427342174901 ) ) ;
#53255 = CARTESIAN_POINT ( 'NONE',  ( 193.9966098916996771, 294.6350105018939871, 13.97117019253516013 ) ) ;
#53256 = ORIENTED_EDGE ( 'NONE', *, *, #82786, .T. ) ;
#53257 = VECTOR ( 'NONE', #20585, 1000.000000000000000 ) ;
#53258 = CARTESIAN_POINT ( 'NONE',  ( 185.5142048876550689, 290.8592545809869421, 12.38599642959644243 ) ) ;
#53259 = CARTESIAN_POINT ( 'NONE',  ( 162.7879170537843834, 283.1953112578214018, -7.983003719734843351 ) ) ;
#53260 = CARTESIAN_POINT ( 'NONE',  ( 81.64803324908639581, 42.02089059119690972, 7.567395689010925075 ) ) ;
#53261 = EDGE_LOOP ( 'NONE', ( #79814, #90626, #95456, #72674 ) ) ;
#53262 = DIRECTION ( 'NONE',  ( -0.000000000000000000, -0.000000000000000000, -1.000000000000000000 ) ) ;
#53263 = CARTESIAN_POINT ( 'NONE',  ( 72.62492194693132319, 71.47378110219968050, -5.675874693310046126 ) ) ;
#53264 = CARTESIAN_POINT ( 'NONE',  ( -19.65312891409030271, 93.06504152958497400, 177.5919119679930134 ) ) ;
#53265 = CARTESIAN_POINT ( 'NONE',  ( 203.5477091018662748, 278.0920214017542662, -16.09930363698006062 ) ) ;
#53266 = EDGE_CURVE ( 'NONE', #48579, #45907, #73663, .T. ) ;
#53267 = EDGE_LOOP ( 'NONE', ( #38120, #14022, #9074, #29116 ) ) ;
#53268 = VECTOR ( 'NONE', #15125, 1000.000000000000000 ) ;
#53269 = ORIENTED_EDGE ( 'NONE', *, *, #33961, .F. ) ;
#53271 = CARTESIAN_POINT ( 'NONE',  ( 150.8581383233440931, 273.8175834856673418, 11.30189666945060623 ) ) ;
#53270 = CARTESIAN_POINT ( 'NONE',  ( 202.1973601604639157, 279.9586468202055016, 15.74103291435646668 ) ) ;
#53272 = EDGE_LOOP ( 'NONE', ( #55059, #62471, #96433, #3602 ) ) ;
#53273 = CARTESIAN_POINT ( 'NONE',  ( 201.4463813434794019, 281.7316278426353620, -17.16864527463587820 ) ) ;
#53274 = CARTESIAN_POINT ( 'NONE',  ( 69.35253854976203058, 63.01665765323906498, 13.58811665770852350 ) ) ;
#53275 = CARTESIAN_POINT ( 'NONE',  ( 81.49862395535369330, 59.56456120573196245, 0.1209609477998291605 ) ) ;
#53276 = CARTESIAN_POINT ( 'NONE',  ( 69.19273132923471792, 69.74333897986481645, -6.091390803950828214 ) ) ;
#53277 = ORIENTED_EDGE ( 'NONE', *, *, #45087, .F. ) ;
#53279 = EDGE_CURVE ( 'NONE', #32899, #48736, #56941, .T. ) ;
#53278 = CARTESIAN_POINT ( 'NONE',  ( 190.3049670482083684, 301.0291234702190764, 0.2225066852051815758 ) ) ;
#53280 = AXIS2_PLACEMENT_3D ( 'NONE', #68680, #53481, #14977 ) ;
#53281 = ORIENTED_EDGE ( 'NONE', *, *, #71482, .F. ) ;
#53282 = CARTESIAN_POINT ( 'NONE',  ( 206.5508451493652444, 272.8904371854448527, 11.05407534521577695 ) ) ;
#53283 = CARTESIAN_POINT ( 'NONE',  ( 75.00226567582841142, 65.52623940974007155, 13.57230656279164727 ) ) ;
#53284 = VERTEX_POINT ( 'NONE', #66546 ) ;
#53285 = CARTESIAN_POINT ( 'NONE',  ( 149.7119746935222793, 271.3382486597900538, 12.05352563709836922 ) ) ;
#53286 = DIRECTION ( 'NONE',  ( 0.5000000000000001110, -0.8660254037844384856, -0.000000000000000000 ) ) ;
#53287 = VERTEX_POINT ( 'NONE', #10366 ) ;
#53288 = CARTESIAN_POINT ( 'NONE',  ( -9.661182929849102763, 72.23920645719188371, 14.90246908070922061 ) ) ;
#53289 = CARTESIAN_POINT ( 'NONE',  ( 36.70787689013189947, 33.14441083166263979, 10.00000000000000533 ) ) ;
#53290 = DIRECTION ( 'NONE',  ( -0.8816062427480089170, -0.4719856276919233706, 0.000000000000000000 ) ) ;
#53291 = CARTESIAN_POINT ( 'NONE',  ( 83.13520543127567919, 52.15262426605146118, 14.79738518802719049 ) ) ;
#53292 = ORIENTED_EDGE ( 'NONE', *, *, #45383, .F. ) ;
#53293 = ORIENTED_EDGE ( 'NONE', *, *, #62968, .F. ) ;
#53294 = CARTESIAN_POINT ( 'NONE',  ( 73.67505968516064740, 69.57270177156178192, 9.668646285131167417 ) ) ;
#53295 = CARTESIAN_POINT ( 'NONE',  ( 146.7879906441258129, 276.4027375938661635, 4.347255311287614887 ) ) ;
#53296 = CARTESIAN_POINT ( 'NONE',  ( 82.31933756389703660, 53.70313499084333841, 15.83617117143144526 ) ) ;
#53297 = CARTESIAN_POINT ( 'NONE',  ( 149.4491471355718772, 271.7934793437897270, 11.43912701239353780 ) ) ;
#53298 = CARTESIAN_POINT ( 'NONE',  ( -19.51633657099221963, 93.10247939160333885, 59.99999999999999289 ) ) ;
#53299 = CARTESIAN_POINT ( 'NONE',  ( 146.7933720846101551, 276.3934166655288891, -0.7715638482002741272 ) ) ;
#53300 = CARTESIAN_POINT ( 'NONE',  ( 147.0721334091522294, 275.9105878882373304, 0.7242168585908188572 ) ) ;
#53301 = CARTESIAN_POINT ( 'NONE',  ( 190.0226014859668453, 301.5181949703289774, 3.835066345245774500 ) ) ;
#53302 = CARTESIAN_POINT ( 'NONE',  ( 69.80658768130543024, 67.27183608565839279, 9.609976433168107235 ) ) ;
#53303 = LINE ( 'NONE', #30507, #27308 ) ;
#53304 = CARTESIAN_POINT ( 'NONE',  ( 167.5734009011913201, 287.5402412053340981, 3.813278936258391205 ) ) ;
#53305 = CARTESIAN_POINT ( 'NONE',  ( 78.02686697169625063, 47.82505017202286979, 14.03973303039792597 ) ) ;
#53306 = VERTEX_POINT ( 'NONE', #81788 ) ;
#53307 = CARTESIAN_POINT ( 'NONE',  ( 149.4340984048157850, 271.8195445100486154, -13.08951326935260617 ) ) ;
#53308 = CARTESIAN_POINT ( 'NONE',  ( 71.69449150190311570, 68.87257317924374433, 9.071537784185924380 ) ) ;
#53309 = CARTESIAN_POINT ( 'NONE',  ( 202.8576051359847838, 278.8876414770759311, 15.11413215307486091 ) ) ;
#53310 = CARTESIAN_POINT ( 'NONE',  ( 79.10360752189127709, 45.94674753059116057, 13.17468094630847375 ) ) ;
#53311 = CARTESIAN_POINT ( 'NONE',  ( 179.8080204723898987, 283.1032712615998435, -15.92647367223843524 ) ) ;
#53312 = CARTESIAN_POINT ( 'NONE',  ( 147.9905646369332999, 274.3198183384625395, -9.173503928458199397 ) ) ;
#53313 = CARTESIAN_POINT ( 'NONE',  ( 168.8622422750650287, 285.9893830644730883, -7.604670509767990083 ) ) ;
#53314 = EDGE_LOOP ( 'NONE', ( #4693, #32877, #80634, #24988 ) ) ;
#53315 = CARTESIAN_POINT ( 'NONE',  ( 208.2912792141756029, 269.8759169579697641, -2.198672330625011995 ) ) ;
#53316 = CARTESIAN_POINT ( 'NONE',  ( -162.0327448629461742, 33.95614270198240803, -21.50000000000000000 ) ) ;
#53317 = CARTESIAN_POINT ( 'NONE',  ( -38.35373792487678202, 26.90998726756845727, -10.00000000000000000 ) ) ;
#53318 = CARTESIAN_POINT ( 'NONE',  ( 40.63510790894940072, 204.2677522451419350, -5.000000000000047962 ) ) ;
#53319 = CARTESIAN_POINT ( 'NONE',  ( 113.9495709998497688, 236.5958772461660544, -9.188101187500095079 ) ) ;
#53320 = CARTESIAN_POINT ( 'NONE',  ( 180.7653681401676238, 294.1091613165833110, -3.018679760699134906 ) ) ;
#53321 = VECTOR ( 'NONE', #25726, 1000.000000000000000 ) ;
#53322 = CARTESIAN_POINT ( 'NONE',  ( -19.65312891409030271, 93.06504152958497400, 10.00000000000000888 ) ) ;
#53323 = DIRECTION ( 'NONE',  ( -0.000000000000000000, -0.000000000000000000, -1.000000000000000000 ) ) ;
#53324 = CARTESIAN_POINT ( 'NONE',  ( 173.1062955787805322, 251.8696176234196855, -3.934703316205188983 ) ) ;
#53325 = CARTESIAN_POINT ( 'NONE',  ( 31.35205101814392847, 201.1589784336661353, -6.496448406907675876E-16 ) ) ;
#53326 = EDGE_CURVE ( 'NONE', #86358, #82234, #84364, .T. ) ;
#53327 = CARTESIAN_POINT ( 'NONE',  ( 162.5148320529283126, 285.2034568178174254, 0.5437328601018158736 ) ) ;
#53328 = AXIS2_PLACEMENT_3D ( 'NONE', #22058, #40236, #8852 ) ;
#53329 = VERTEX_POINT ( 'NONE', #58435 ) ;
#53330 = CARTESIAN_POINT ( 'NONE',  ( 1.158783253108745637, 178.1427522451419350, 10.00000000000009415 ) ) ;
#53331 = CARTESIAN_POINT ( 'NONE',  ( 178.1940240703611380, 265.8106693507822342, 15.39809615566641554 ) ) ;
#53332 = CARTESIAN_POINT ( 'NONE',  ( 74.03799347921402330, 64.05404633756495514, 14.51082138824052414 ) ) ;
#53333 = B_SPLINE_CURVE_WITH_KNOTS ( 'NONE', 3,
 ( #26760, #27761, #43443, #66744 ),
 .UNSPECIFIED., .F., .F.,
 ( 4, 4 ),
 ( 1.588764278728131813E-16, 0.007655728206563773564 ),
 .UNSPECIFIED. ) ;
#53334 = CARTESIAN_POINT ( 'NONE',  ( 190.8683709797118411, 300.0532792356709706, -4.461919767133968762 ) ) ;
#53335 = CARTESIAN_POINT ( 'NONE',  ( 81.89176746338951318, 41.27503766206196190, -5.828951561110701007 ) ) ;
#53336 = EDGE_CURVE ( 'NONE', #24759, #23902, #47851, .T. ) ;
#53337 = FACE_OUTER_BOUND ( 'NONE', #3567, .T. ) ;
#53338 = AXIS2_PLACEMENT_3D ( 'NONE', #30427, #93773, #84666 ) ;
#53339 = CARTESIAN_POINT ( 'NONE',  ( -12.10640029135213247, 60.69888763781672480, -10.00000000000000000 ) ) ;
#53340 = CARTESIAN_POINT ( 'NONE',  ( 102.4837554958880901, 236.6427522451419350, 10.00000000000009237 ) ) ;
#53341 = B_SPLINE_SURFACE_WITH_KNOTS ( 'NONE', 3, 1, ( 
 ( #33069, #88836 ),
 ( #19400, #18381 ),
 ( #64977, #86833 ),
 ( #34563, #87357 ),
 ( #41656, #87842 ),
 ( #72087, #42156 ),
 ( #49767, #25987 ),
 ( #80213, #79716 ),
 ( #17886, #57356 ),
 ( #10781, #94906 ),
 ( #50259, #64474 ),
 ( #73574, #25468 ),
 ( #40653, #73091 ),
 ( #96405, #95920 ),
 ( #3203, #27481 ),
 ( #88332, #26974 ),
 ( #48785, #57856 ),
 ( #10279, #81212 ),
 ( #2688, #72599 ),
 ( #63963, #80723 ),
 ( #11297, #48273 ),
 ( #79219, #11786 ),
 ( #4157, #35052 ),
 ( #65960, #21849 ),
 ( #14254, #44630 ),
 ( #59843, #12275 ),
 ( #20373, #12782 ),
 ( #37533, #60327 ),
 ( #43647, #98873 ),
 ( #44138, #59327 ),
 ( #90307, #29451 ),
 ( #35558, #91283 ),
 ( #36541, #74077 ),
 ( #68438, #99366 ) ),
 .UNSPECIFIED., .T., .F., .F.,
 ( 4, 2, 2, 2, 2, 2, 2, 2, 2, 2, 2, 2, 2, 2, 2, 2, 4 ),
 ( 2, 2 ),
 ( 0.000000000000000000, 0.06250000000000000000, 0.1250000000000000000, 0.1875000000000000000, 0.2500000000000000000, 0.3125000000000000000, 0.3750000000000000000, 0.4375000000000000000, 0.5000000000000000000, 0.5625000000000000000, 0.6250000000000000000, 0.6875000000000000000, 0.7500000000000000000, 0.8125000000000000000, 0.8750000000000000000, 0.9375000000000000000, 1.000000000000000000 ),
 ( 0.000000000000000000, 1.000000000000000000 ),
 .UNSPECIFIED. ) ;
#53342 = DIRECTION ( 'NONE',  ( -0.000000000000000000, -0.000000000000000000, -1.000000000000000000 ) ) ;
#53343 = ORIENTED_EDGE ( 'NONE', *, *, #77658, .F. ) ;
#53344 = EDGE_CURVE ( 'NONE', #80748, #53896, #52699, .T. ) ;
#53345 = CARTESIAN_POINT ( 'NONE',  ( 202.8211298556536804, 279.3504935719197988, 17.07914446815911447 ) ) ;
#53346 = CARTESIAN_POINT ( 'NONE',  ( 153.9000638729780519, 264.8647237507889258, 16.61098735674968907 ) ) ;
#53347 = VECTOR ( 'NONE', #49995, 1000.000000000000000 ) ;
#53348 = CARTESIAN_POINT ( 'NONE',  ( 17.98330449086917682, 175.0643266524160140, -9.188101187500093303 ) ) ;
#53349 = CARTESIAN_POINT ( 'NONE',  ( 12.53574365251957090, 15.43677371833799938, -10.00000000000000355 ) ) ;
#53350 = CARTESIAN_POINT ( 'NONE',  ( 193.5726236920921792, 272.6483137682516258, 14.24630395148186146 ) ) ;
#53351 = CARTESIAN_POINT ( 'NONE',  ( 71.67479916869325507, 58.94068462711909007, -15.88111808811495607 ) ) ;
#53352 = DIRECTION ( 'NONE',  ( -0.9563064286990893281, 0.2923662333936558611, 0.000000000000000000 ) ) ;
#53354 = CARTESIAN_POINT ( 'NONE',  ( 57.65757265809627086, 216.3464784336661353, 1.353441290958777327E-15 ) ) ;
#53353 = CARTESIAN_POINT ( 'NONE',  ( 195.2398765441725743, 275.4993714954396182, -15.53986780429037928 ) ) ;
#53355 = CARTESIAN_POINT ( 'NONE',  ( 164.4915767550571957, 245.7392269735623529, -6.407198159945809657 ) ) ;
#53356 = CIRCLE ( 'NONE', #50111, 49.99999999999999289 ) ;
#53357 = CARTESIAN_POINT ( 'NONE',  ( 74.23329481810236530, 55.36962176604209418, 16.12301265312518339 ) ) ;
#53358 = CARTESIAN_POINT ( 'NONE',  ( -29.41492724108444889, 95.52075410896856056, 44.61813138648138732 ) ) ;
#53359 = CARTESIAN_POINT ( 'NONE',  ( 207.6209998424140792, 271.0368748851258260, 6.610167240481342965 ) ) ;
#53360 = ORIENTED_EDGE ( 'NONE', *, *, #15013, .F. ) ;
#53361 = CARTESIAN_POINT ( 'NONE',  ( 3.558395312976033065, 182.8615022471903444, 5.000000000000046185 ) ) ;
#53362 = CARTESIAN_POINT ( 'NONE',  ( 163.7423057141168385, 247.0370024851108610, -6.909410042141566066 ) ) ;
#53363 = CARTESIAN_POINT ( 'NONE',  ( 132.4608640057421667, 247.2833772461660544, -9.188101187500095079 ) ) ;
#53364 = CARTESIAN_POINT ( 'NONE',  ( 33.66714878060290772, 21.29860640527294180, -2.839279412974138328 ) ) ;
#53365 = CARTESIAN_POINT ( 'NONE',  ( 164.8280002253160319, 260.9906286863443370, -16.15074254659257846 ) ) ;
#53366 = CARTESIAN_POINT ( 'NONE',  ( -76.99869489832862257, 52.47050021824117749, 10.00000000000000000 ) ) ;
#53367 = CARTESIAN_POINT ( 'NONE',  ( 177.3945811460199309, 252.6478776281709315, -0.09019740402004521040 ) ) ;
#53369 = CARTESIAN_POINT ( 'NONE',  ( 47.54560441532652959, 78.55524412553474178, 10.00000000000000000 ) ) ;
#53368 = CARTESIAN_POINT ( 'NONE',  ( 206.9349434189263661, 269.8064106017384916, 1.784245431258210113 ) ) ;
#53370 = CARTESIAN_POINT ( 'NONE',  ( 68.48051572044573732, 64.33975350462213783, 12.32598567578913773 ) ) ;
#53371 = ORIENTED_EDGE ( 'NONE', *, *, #53823, .F. ) ;
#53372 = CARTESIAN_POINT ( 'NONE',  ( 152.7730629122270898, 271.2363297891400293, 14.33490734661111610 ) ) ;
#53373 = CARTESIAN_POINT ( 'NONE',  ( 151.7688189367730445, 268.5115722919948098, -14.80711862932078482 ) ) ;
#53374 = CARTESIAN_POINT ( 'NONE',  ( 196.5882727079285530, 289.1336862968285004, 16.81565452615681977 ) ) ;
#53375 = CARTESIAN_POINT ( 'NONE',  ( 197.3142096324615693, 273.2062379081899053, -13.39448277848560309 ) ) ;
#53376 = ORIENTED_EDGE ( 'NONE', *, *, #64237, .T. ) ;
#53377 = CARTESIAN_POINT ( 'NONE',  ( -28.78056054657191964, 23.66266410781090457, 177.5919119679930134 ) ) ;
#53378 = DIRECTION ( 'NONE',  ( 0.5000000000000003331, -0.8660254037844384856, 0.000000000000000000 ) ) ;
#53379 = EDGE_CURVE ( 'NONE', #74122, #11056, #11869, .T. ) ;
#53380 = EDGE_CURVE ( 'NONE', #7185, #71334, #35141, .T. ) ;
#53381 = LINE ( 'NONE', #44774, #91100 ) ;
#53382 = CARTESIAN_POINT ( 'NONE',  ( 196.2549875969139066, 270.8803193507863512, 12.05863901870844046 ) ) ;
#53383 = DIRECTION ( 'NONE',  ( -0.5840252505817192796, 0.000000000000000000, 0.8117354905897362638 ) ) ;
#53384 = CARTESIAN_POINT ( 'NONE',  ( 66.86954601471772719, 67.94335577711918006, 5.821787759504553073 ) ) ;
#53385 = FACE_OUTER_BOUND ( 'NONE', #61617, .T. ) ;
#53386 = FACE_OUTER_BOUND ( 'NONE', #41463, .T. ) ;
#53387 = PLANE ( 'NONE',  #12655 ) ;
#53388 = ORIENTED_EDGE ( 'NONE', *, *, #45758, .T. ) ;
#53389 = CARTESIAN_POINT ( 'NONE',  ( 190.4163244163388242, 300.8362468508201459, 4.691083071570470331 ) ) ;
#53390 = CARTESIAN_POINT ( 'NONE',  ( 86.55657754374946933, 47.30628205130771136, -10.74852006680811023 ) ) ;
#53391 = CARTESIAN_POINT ( 'NONE',  ( 84.82053053956542499, 45.10610155585538905, -8.666442846737737682 ) ) ;
#53392 = VERTEX_POINT ( 'NONE', #80814 ) ;
#53393 = AXIS2_PLACEMENT_3D ( 'NONE', #57530, #58040, #3850 ) ;
#53395 = ADVANCED_FACE ( 'NONE', ( #35645 ), #18469, .T. ) ;
#53394 = CARTESIAN_POINT ( 'NONE',  ( -55.56624327025929944, 44.99999999999998579, 59.99999999999999289 ) ) ;
#53396 = CARTESIAN_POINT ( 'NONE',  ( 79.38118373144868656, 59.76411540931838573, -16.16477398176405345 ) ) ;
#53397 = CARTESIAN_POINT ( 'NONE',  ( 149.4171629335945681, 271.8488776066536730, -11.42564036194071520 ) ) ;
#53398 = CARTESIAN_POINT ( 'NONE',  ( 75.22798512741415777, 53.64680820920216320, -16.53898548151806835 ) ) ;
#53399 = CARTESIAN_POINT ( 'NONE',  ( 69.95047170429380401, 62.88811978159139215, 13.86734351276082045 ) ) ;
#53400 = VERTEX_POINT ( 'NONE', #97000 ) ;
#53401 = CARTESIAN_POINT ( 'NONE',  ( 98.84807947347611901, 234.0024278399160949, -9.188101187500093303 ) ) ;
#53402 = CARTESIAN_POINT ( 'NONE',  ( 200.1662314894802819, 283.9489124310637180, 17.19420058542677054 ) ) ;
#53403 = CARTESIAN_POINT ( 'NONE',  ( 181.1247500054012392, 271.0610771650950142, -15.98018870080622200 ) ) ;
#53404 = CARTESIAN_POINT ( 'NONE',  ( 81.64670023727850889, 42.65128533460878657, -7.584980231169037523 ) ) ;
#53405 = ORIENTED_EDGE ( 'NONE', *, *, #85928, .T. ) ;
#53406 = ORIENTED_EDGE ( 'NONE', *, *, #58942, .F. ) ;
#53407 = ORIENTED_EDGE ( 'NONE', *, *, #76295, .F. ) ;
#53408 = CARTESIAN_POINT ( 'NONE',  ( 81.98602009217056263, 53.23458893094329625, 15.38303897364004236 ) ) ;
#53409 = ORIENTED_EDGE ( 'NONE', *, *, #98872, .F. ) ;
#53410 = CARTESIAN_POINT ( 'NONE',  ( 69.86600153435685456, 70.48283808624711355, 3.777498432527079064 ) ) ;
#53411 = AXIS2_PLACEMENT_3D ( 'NONE', #81293, #87437, #17970 ) ;
#53412 = ORIENTED_EDGE ( 'NONE', *, *, #24343, .F. ) ;
#53413 = CARTESIAN_POINT ( 'NONE',  ( 207.8302079587528794, 270.6745157982714431, 3.572475529330238153 ) ) ;
#53414 = CARTESIAN_POINT ( 'NONE',  ( 82.36208054384441368, 41.26681451557220015, 3.281558084501622563 ) ) ;
#53415 = DIRECTION ( 'NONE',  ( -0.000000000000000000, -0.000000000000000000, -1.000000000000000000 ) ) ;
#53416 = CARTESIAN_POINT ( 'NONE',  ( -23.57949368289046888, 99.70778085183977169, 45.19941863730353049 ) ) ;
#53417 = CARTESIAN_POINT ( 'NONE',  ( 82.75931229668888989, 53.79267046329768220, -15.79052045153009409 ) ) ;
#53418 = CARTESIAN_POINT ( 'NONE',  ( 204.8008807586744524, 272.7600038595665524, -10.89009281376315741 ) ) ;
#53419 = CARTESIAN_POINT ( 'NONE',  ( 15.78914702631840328, 24.51421378149918695, -9.188101187500004485 ) ) ;
#53420 = CARTESIAN_POINT ( 'NONE',  ( 198.3788960466430069, 277.4004215258680688, -15.34290956586492349 ) ) ;
#53421 = CARTESIAN_POINT ( 'NONE',  ( 189.7493380202622291, 294.8126471784881915, -12.68491631734921299 ) ) ;
#53423 = ORIENTED_EDGE ( 'NONE', *, *, #10509, .F. ) ;
#53422 = DIRECTION ( 'NONE',  ( 0.4999999999999992784, -0.8660254037844390407, 0.000000000000000000 ) ) ;
#53424 = CARTESIAN_POINT ( 'NONE',  ( 162.6937333994314656, 248.8531830095558632, 10.02305144031113926 ) ) ;
#53425 = CARTESIAN_POINT ( 'NONE',  ( 188.2838305778037409, 260.6970239875658990, 2.538272036997531789 ) ) ;
#53426 = DIRECTION ( 'NONE',  ( -0.2805612043866717586, -0.9598361373656965068, 0.000000000000000000 ) ) ;
#53427 =( BOUNDED_CURVE ( )  B_SPLINE_CURVE ( 2, ( #53511, #36822, #22124, #5439, #75853, #98150, #51531, #67732, #83970 ),
 .UNSPECIFIED., .F., .T. ) 
 B_SPLINE_CURVE_WITH_KNOTS ( ( 3, 2, 2, 2, 3 ),
 ( 0.3588709677419354982, 0.3602150537634408733, 0.3629032258064516236, 0.3655913978494623739, 0.3669354838709677491 ),
 .UNSPECIFIED. ) 
 CURVE ( )  GEOMETRIC_REPRESENTATION_ITEM ( )  RATIONAL_B_SPLINE_CURVE ( ( 0.9330127018922194093, 0.9330127018922194093, 1.000000000000000000, 0.8660254037844387076, 1.000000000000000000, 0.8660254037844387076, 1.000000000000000000, 0.9330127018922194093, 0.9330127018922194093 ) ) 
 REPRESENTATION_ITEM ( '' )  );
#53428 = CARTESIAN_POINT ( 'NONE',  ( 81.73013690182854418, 46.02429500294771714, -11.48451531274605486 ) ) ;
#53429 = CARTESIAN_POINT ( 'NONE',  ( 176.3101768776420215, 291.3056225515143183, 7.435599247236559961 ) ) ;
#53430 = CARTESIAN_POINT ( 'NONE',  ( 161.3138715957851161, 283.5633977043666505, 2.146130691252540856 ) ) ;
#53431 = ORIENTED_EDGE ( 'NONE', *, *, #96431, .T. ) ;
#53432 = CARTESIAN_POINT ( 'NONE',  ( 93.60468337831815688, 236.3967562850347122, -4.648177544792955347E-16 ) ) ;
#53433 = FACE_OUTER_BOUND ( 'NONE', #22168, .T. ) ;
#53434 = CARTESIAN_POINT ( 'NONE',  ( 8.231324050681719129, 168.8927522451418213, -10.00000000000009059 ) ) ;
#53435 = CARTESIAN_POINT ( 'NONE',  ( 196.1497905407457836, 269.5260199243853663, -10.84959131364318630 ) ) ;
#53436 = CARTESIAN_POINT ( 'NONE',  ( 172.8824701414635285, 280.2431502589070078, -14.30495993044576331 ) ) ;
#53437 = CARTESIAN_POINT ( 'NONE',  ( 50.26447705663007071, 96.46038765672592774, 177.5919119679930134 ) ) ;
#53438 = CARTESIAN_POINT ( 'NONE',  ( 82.67540033522136866, 44.72113521480816445, -9.646895689004646002 ) ) ;
#53439 = LINE ( 'NONE', #31627, #58111 ) ;
#53441 = CARTESIAN_POINT ( 'NONE',  ( 76.27486002672000609, 65.07516076971148777, 14.62441312286923889 ) ) ;
#53440 = CARTESIAN_POINT ( 'NONE',  ( -10.59588092978231266, 170.8149278399160949, -9.188101187500095079 ) ) ;
#53442 = EDGE_CURVE ( 'NONE', #88529, #45286, #6988, .T. ) ;
#53443 = CARTESIAN_POINT ( 'NONE',  ( 189.0628780359570840, 297.0621672202208856, 8.938274956999553211 ) ) ;
#53444 = EDGE_LOOP ( 'NONE', ( #83965, #37218, #79262, #26241 ) ) ;
#53445 = ORIENTED_EDGE ( 'NONE', *, *, #69772, .F. ) ;
#53446 = CARTESIAN_POINT ( 'NONE',  ( 202.5128468779458331, 267.1751508879428343, 0.8823122286173835649 ) ) ;
#53447 = EDGE_CURVE ( 'NONE', #56117, #37792, #77142, .T. ) ;
#53448 = B_SPLINE_CURVE_WITH_KNOTS ( 'NONE', 3,
 ( #28596, #36687, #98526, #29603 ),
 .UNSPECIFIED., .F., .F.,
 ( 4, 4 ),
 ( 0.01664341470350885061, 0.02552166612420159880 ),
 .UNSPECIFIED. ) ;
#53449 = CARTESIAN_POINT ( 'NONE',  ( -22.42236680055709641, 157.8615022471902591, 0.000000000000000000 ) ) ;
#53450 = CARTESIAN_POINT ( 'NONE',  ( -19.72794058414494245, 93.18552784692582236, 59.99999999999999289 ) ) ;
#53451 = CARTESIAN_POINT ( 'NONE',  ( 163.0339123139343656, 248.2639758459733343, -11.68896797671248322 ) ) ;
#53452 = CARTESIAN_POINT ( 'NONE',  ( 68.61869731438623887, 66.71998516903308030, 10.18785472861651975 ) ) ;
#53453 = CARTESIAN_POINT ( 'NONE',  ( 40.48539884740146277, 126.3902902409112556, 10.00000000000000000 ) ) ;
#53454 = CARTESIAN_POINT ( 'NONE',  ( 29.05227845693028854, 178.3923013555409796, 4.594050593750050204 ) ) ;
#53455 = CARTESIAN_POINT ( 'NONE',  ( 113.0020953926368037, 245.2369531367911009, -4.594050593750048428 ) ) ;
#53456 = PLANE ( 'NONE',  #92052 ) ;
#53457 = DIRECTION ( 'NONE',  ( 0.2471055264905481497, -0.9689885751534065284, 0.000000000000000000 ) ) ;
#53458 = ADVANCED_FACE ( 'NONE', ( #26564 ), #41234, .T. ) ;
#53459 = CYLINDRICAL_SURFACE ( 'NONE', #1208, 16.60714546451156792 ) ;
#53460 = CYLINDRICAL_SURFACE ( 'NONE', #17783, 17.82106496071139645 ) ;
#53461 = CARTESIAN_POINT ( 'NONE',  ( 77.76328872507745871, 54.37645632513159910, -16.02018328028568561 ) ) ;
#53462 = CARTESIAN_POINT ( 'NONE',  ( 157.1135969804030310, 258.5182628004787944, 17.19660297500358226 ) ) ;
#53463 = CARTESIAN_POINT ( 'NONE',  ( 68.54569597095012057, 64.23358675863970291, -12.43730015513902742 ) ) ;
#53464 = CARTESIAN_POINT ( 'NONE',  ( 207.3646600298985447, 271.4808684644054324, -5.284084612275558257 ) ) ;
#53465 = CARTESIAN_POINT ( 'NONE',  ( 189.9640924866416185, 284.8439010332405701, 17.27955391728670165 ) ) ;
#53466 = ADVANCED_FACE ( 'NONE', ( #52824 ), #36627, .F. ) ;
#53467 = CARTESIAN_POINT ( 'NONE',  ( 165.0466594235693094, 249.7004948130006881, -10.73553599785811485 ) ) ;
#53468 = CARTESIAN_POINT ( 'NONE',  ( 66.31795133325435643, 69.20145725284447735, 2.477662600225432055 ) ) ;
#53469 = CARTESIAN_POINT ( 'NONE',  ( 67.91650730281627091, 67.19912629719564734, 8.215611842121816721 ) ) ;
#53470 = CARTESIAN_POINT ( 'NONE',  ( -19.65312891409030271, 93.06504152958497400, 10.00000000000000888 ) ) ;
#53471 = PLANE ( 'NONE',  #15605 ) ;
#53472 = EDGE_CURVE ( 'NONE', #25048, #36314, #65664, .T. ) ;
#53473 = EDGE_LOOP ( 'NONE', ( #48214, #72768 ) ) ;
#53474 = DIRECTION ( 'NONE',  ( 0.2500151307524129951, -0.9682419296822740717, 0.000000000000000000 ) ) ;
#53475 = CIRCLE ( 'NONE', #43786, 2.471954595299370006 ) ;
#53476 = CARTESIAN_POINT ( 'NONE',  ( 207.5408646414791178, 271.1756731246201753, 3.050859480894625886 ) ) ;
#53477 = CARTESIAN_POINT ( 'NONE',  ( 82.30224259357629535, 41.51585266698759824, -5.837696018585297963 ) ) ;
#53478 = CARTESIAN_POINT ( 'NONE',  ( 105.4518702730974979, 225.5643266524160140, 9.188101187500095079 ) ) ;
#53479 = CARTESIAN_POINT ( 'NONE',  ( 13.34262526062736676, 23.10171378149917842, 9.188101187500008038 ) ) ;
#53480 = CARTESIAN_POINT ( 'NONE',  ( 74.83829975255316924, 60.29844347012056005, -16.01251099248637644 ) ) ;
#53481 = DIRECTION ( 'NONE',  ( 0.000000000000000000, 0.000000000000000000, 1.000000000000000000 ) ) ;
#53483 = CARTESIAN_POINT ( 'NONE',  ( 111.2883471010299274, 228.3927522451418213, 10.00000000000009948 ) ) ;
#53482 = CARTESIAN_POINT ( 'NONE',  ( 157.3025066944120454, 258.1910615777721887, 18.21299529665260053 ) ) ;
#53484 = CARTESIAN_POINT ( 'NONE',  ( -63.67680148659454886, 65.89705432001115071, 59.99999999999999289 ) ) ;
#53485 = CARTESIAN_POINT ( 'NONE',  ( 182.8075329105516289, 285.5996758505444291, -15.91971760981349071 ) ) ;
#53486 = CARTESIAN_POINT ( 'NONE',  ( 196.5114383562724072, 290.2791998289336561, -17.87308875047256862 ) ) ;
#53487 = CARTESIAN_POINT ( 'NONE',  ( 35.85928575902275384, 36.10171378149922106, 9.188101187500008038 ) ) ;
#53488 = CARTESIAN_POINT ( 'NONE',  ( 33.05130250568083738, 42.58029201028044497, 1.583844403245397769 ) ) ;
#53489 = LINE ( 'NONE', #75828, #31321 ) ;
#53490 = VERTEX_POINT ( 'NONE', #37130 ) ;
#53491 = CARTESIAN_POINT ( 'NONE',  ( 33.29248241878940462, 22.14754757982091604, -5.678558825948276656 ) ) ;
#53492 = CARTESIAN_POINT ( 'NONE',  ( 77.86555730066851311, 62.20866292688850052, -15.95979438352862090 ) ) ;
#53493 = CARTESIAN_POINT ( 'NONE',  ( 200.3191154286411972, 269.5421802034505276, 8.895171844116440241 ) ) ;
#53494 = CARTESIAN_POINT ( 'NONE',  ( 196.7491951525289835, 289.8673929779723721, -16.35352603081977207 ) ) ;
#53495 = EDGE_CURVE ( 'NONE', #39796, #526, #20460, .T. ) ;
#53496 = ORIENTED_EDGE ( 'NONE', *, *, #68029, .T. ) ;
#53497 = CARTESIAN_POINT ( 'NONE',  ( 84.78071699792324978, 50.02262005461608396, -13.67739062443489750 ) ) ;
#53498 = CARTESIAN_POINT ( 'NONE',  ( 198.3449891235413531, 287.1033967417670283, 16.95540786497457120 ) ) ;
#53499 = CARTESIAN_POINT ( 'NONE',  ( 180.2627280979794193, 263.0731415412748788, -12.84391273256747112 ) ) ;
#53500 = CARTESIAN_POINT ( 'NONE',  ( -19.60272883349852435, 92.93247618524840448, 59.99999999999999289 ) ) ;
#53501 = CARTESIAN_POINT ( 'NONE',  ( 150.7827139563306957, 247.8615022471901739, 5.000000000000051514 ) ) ;
#53502 = EDGE_CURVE ( 'NONE', #861, #74959, #75651, .T. ) ;
#53503 = B_SPLINE_CURVE_WITH_KNOTS ( 'NONE', 3,
 ( #21070, #89982, #59013, #68128 ),
 .UNSPECIFIED., .F., .F.,
 ( 4, 4 ),
 ( 2.189838513871484750E-15, 0.002576580807713663504 ),
 .UNSPECIFIED. ) ;
#53504 = ORIENTED_EDGE ( 'NONE', *, *, #9251, .T. ) ;
#53505 = CARTESIAN_POINT ( 'NONE',  ( 78.41477381122238910, 47.32040575024743134, -14.22103711499937617 ) ) ;
#53506 = CARTESIAN_POINT ( 'NONE',  ( 35.92184506804998279, 29.24335787977765477, -9.188101187500008038 ) ) ;
#53507 = ORIENTED_EDGE ( 'NONE', *, *, #80927, .F. ) ;
#53508 = CARTESIAN_POINT ( 'NONE',  ( -19.65312891409030271, 93.06504152958497400, -10.00000000000000888 ) ) ;
#53509 = CARTESIAN_POINT ( 'NONE',  ( 181.4256177755142403, 290.8855465862295659, -11.11246407318897234 ) ) ;
#53510 = ORIENTED_EDGE ( 'NONE', *, *, #72967, .F. ) ;
#53512 = EDGE_CURVE ( 'NONE', #15461, #12944, #15529, .T. ) ;
#53511 = CARTESIAN_POINT ( 'NONE',  ( 39.04508293989853485, 204.8967562850347122, -4.648177544792955347E-16 ) ) ;
#53513 = CARTESIAN_POINT ( 'NONE',  ( 158.8709510117273567, 255.4744363313390920, 17.58515796180118329 ) ) ;
#53514 = CARTESIAN_POINT ( 'NONE',  ( 84.82554225155547556, 50.21385520134798242, 13.77498508261128407 ) ) ;
#53515 = DIRECTION ( 'NONE',  ( -0.000000000000000000, 0.000000000000000000, -1.000000000000000000 ) ) ;
#53516 = CARTESIAN_POINT ( 'NONE',  ( 153.2283961777204695, 265.2476279883323400, -17.66880461074566000 ) ) ;
#53517 = PLANE ( 'NONE',  #43157 ) ;
#53518 = CARTESIAN_POINT ( 'NONE',  ( 42.37730965384162829, 25.26216523072498532, -2.296566073217252530E-15 ) ) ;
#53519 = CARTESIAN_POINT ( 'NONE',  ( 81.27316195909862984, 55.43468901134095006, -16.33783760952318076 ) ) ;
#53520 = EDGE_CURVE ( 'NONE', #4197, #96323, #37311, .T. ) ;
#53521 = DIRECTION ( 'NONE',  ( -0.5000000000000012212, 0.8660254037844378194, -0.000000000000000000 ) ) ;
#53522 = EDGE_LOOP ( 'NONE', ( #72881, #65000, #58005, #33552, #93596 ) ) ;
#53523 = CYLINDRICAL_SURFACE ( 'NONE', #57816, 17.82106496071139645 ) ;
#53524 = VERTEX_POINT ( 'NONE', #5251 ) ;
#53525 = VERTEX_POINT ( 'NONE', #30535 ) ;
#53526 = CARTESIAN_POINT ( 'NONE',  ( 72.13789110140854177, 72.31505540346954319, -1.296595641072646243 ) ) ;
#53527 = CARTESIAN_POINT ( 'NONE',  ( 170.4004368708347670, 269.6954681395467333, 17.78991379675761664 ) ) ;
#53529 = FACE_OUTER_BOUND ( 'NONE', #50916, .T. ) ;
#53528 = CARTESIAN_POINT ( 'NONE',  ( 164.4761815919938215, 245.7658921781788592, 6.833796894895563412 ) ) ;
#53530 = DIRECTION ( 'NONE',  ( -0.000000000000000000, 0.000000000000000000, -1.000000000000000000 ) ) ;
#53531 = CARTESIAN_POINT ( 'NONE',  ( 197.8594538715673536, 272.3702523096476398, -13.40354871589081398 ) ) ;
#53532 = CARTESIAN_POINT ( 'NONE',  ( 78.40196830515944271, 59.44234872728634400, -16.13643701924537055 ) ) ;
#53533 = CARTESIAN_POINT ( 'NONE',  ( 146.9978162861947908, 276.0393089210717790, -5.134868500856280882 ) ) ;
#53534 = CARTESIAN_POINT ( 'NONE',  ( 183.6422324172568210, 264.5785696717482551, 14.31652553825990104 ) ) ;
#53535 = CARTESIAN_POINT ( 'NONE',  ( 165.8099488291475154, 266.0266196162687038, 17.45967265355124809 ) ) ;
#53536 = CARTESIAN_POINT ( 'NONE',  ( 183.4288137002880319, 284.5585098770374088, -15.07552829229580915 ) ) ;
#53537 = CARTESIAN_POINT ( 'NONE',  ( 108.7534185771431510, 233.5958772461660260, -9.188101187500095079 ) ) ;
#53538 = ORIENTED_EDGE ( 'NONE', *, *, #98732, .F. ) ;
#53539 = DIRECTION ( 'NONE',  ( -1.000000000000000000, 0.000000000000000000, 0.000000000000000000 ) ) ;
#53540 = CARTESIAN_POINT ( 'NONE',  ( 161.1894491815656352, 283.7774907297039135, 2.177303784804435871 ) ) ;
#53541 = CARTESIAN_POINT ( 'NONE',  ( 189.5402112412503186, 274.1870215229640166, 15.72462957861923272 ) ) ;
#53542 = EDGE_LOOP ( 'NONE', ( #70114, #17661, #34263, #23984 ) ) ;
#53543 = ORIENTED_EDGE ( 'NONE', *, *, #48180, .F. ) ;
#53544 = CARTESIAN_POINT ( 'NONE',  ( 74.13858531873714242, 68.40778981217252408, -11.66187469989377767 ) ) ;
#53545 = DIRECTION ( 'NONE',  ( 0.7905172007421661373, 0.000000000000000000, -0.6124398381316893403 ) ) ;
#53546 = DIRECTION ( 'NONE',  ( 1.000000000000000000, 0.000000000000000000, 0.000000000000000000 ) ) ;
#53547 = CARTESIAN_POINT ( 'NONE',  ( 205.8516076510241533, 269.9921726889444926, 5.257599149465654875 ) ) ;
#53548 = CARTESIAN_POINT ( 'NONE',  ( 32.81602777569660390, 24.11029122506295863, -8.090169943749478065 ) ) ;
#53549 = CARTESIAN_POINT ( 'NONE',  ( -29.91485116994501325, 25.08783183303773967, -10.00000000000000000 ) ) ;
#53550 = EDGE_LOOP ( 'NONE', ( #58009, #88271, #100131, #39942 ) ) ;
#53551 = CARTESIAN_POINT ( 'NONE',  ( 194.9041981377178274, 293.0630215474379838, 15.24265665161630956 ) ) ;
#53552 = VECTOR ( 'NONE', #53853, 1000.000000000000114 ) ;
#53553 = EDGE_LOOP ( 'NONE', ( #19547, #58979, #62515 ) ) ;
#53554 = CARTESIAN_POINT ( 'NONE',  ( -72.39633208959961053, 47.04162880533179703, 177.5919119679930134 ) ) ;
#53555 = DIRECTION ( 'NONE',  ( -0.000000000000000000, -0.000000000000000000, -1.000000000000000000 ) ) ;
#53556 = ORIENTED_EDGE ( 'NONE', *, *, #91115, .T. ) ;
#53557 = CARTESIAN_POINT ( 'NONE',  ( 190.9474291326297930, 266.7645650087163745, -12.82661358031884546 ) ) ;
#53558 = CARTESIAN_POINT ( 'NONE',  ( 151.9991393430420601, 267.3767632815465731, -16.97304508723421179 ) ) ;
#53559 = DIRECTION ( 'NONE',  ( -1.000000000000000000, 0.000000000000000000, 0.000000000000000000 ) ) ;
#53560 = LINE ( 'NONE', #68762, #80816 ) ;
#53562 = CARTESIAN_POINT ( 'NONE',  ( 69.92518591997227873, 62.80814789249908614, -13.33122127648681499 ) ) ;
#53561 = CARTESIAN_POINT ( 'NONE',  ( 184.4758362669423093, 288.9580515395709881, -13.18921054981714924 ) ) ;
#53563 = CARTESIAN_POINT ( 'NONE',  ( 201.1388841337167435, 282.2642286331299601, -18.17233400608081340 ) ) ;
#53564 = VERTEX_POINT ( 'NONE', #13360 ) ;
#53565 = CARTESIAN_POINT ( 'NONE',  ( 204.7166734748386716, 272.9112136331068541, -9.669763598799834270 ) ) ;
#53566 = CARTESIAN_POINT ( 'NONE',  ( 72.93513805092823077, 67.35904576704696467, 11.40243080045951629 ) ) ;
#53567 = CARTESIAN_POINT ( 'NONE',  ( 82.26825361666672620, 40.74351925651850337, -3.658449855531767714 ) ) ;
#53568 = DIRECTION ( 'NONE',  ( 0.000000000000000000, 0.000000000000000000, 1.000000000000000000 ) ) ;
#53569 = CARTESIAN_POINT ( 'NONE',  ( 192.6969673322854248, 271.7607060277501887, -14.66458718008113138 ) ) ;
#53570 = CARTESIAN_POINT ( 'NONE',  ( 81.50940192328098988, 59.54589321767952725, 0.1873032967079516220 ) ) ;
#53571 = CARTESIAN_POINT ( 'NONE',  ( 78.14015596324891533, 47.79605781560270117, 14.53813849190288465 ) ) ;
#53572 = CARTESIAN_POINT ( 'NONE',  ( -13.11024591527734628, 27.99999999999999645, 17.00000000000000000 ) ) ;
#53573 = CARTESIAN_POINT ( 'NONE',  ( 191.1479367720956475, 283.2912585338079907, -16.59553443474640133 ) ) ;
#53574 = CARTESIAN_POINT ( 'NONE',  ( 82.39556149134112673, 53.49063599510539291, -15.76428462505607975 ) ) ;
#53575 = CARTESIAN_POINT ( 'NONE',  ( 72.54255783352381570, 218.8149278399160664, -9.188101187500095079 ) ) ;
#53576 = CARTESIAN_POINT ( 'NONE',  ( 147.4047294057049271, 275.3345147238139248, 0.000000000000000000 ) ) ;
#53577 = CARTESIAN_POINT ( 'NONE',  ( 147.4563929227680603, 275.2450308873625886, -3.847749617713808412 ) ) ;
#53578 = DIRECTION ( 'NONE',  ( 0.000000000000000000, 0.000000000000000000, 1.000000000000000000 ) ) ;
#53579 = EDGE_CURVE ( 'NONE', #36145, #43174, #91370, .T. ) ;
#53580 = LINE ( 'NONE', #51602, #15794 ) ;
#53581 = CARTESIAN_POINT ( 'NONE',  ( 161.7412967960748915, 250.5028515975580774, -14.36228887024421041 ) ) ;
#53582 = CARTESIAN_POINT ( 'NONE',  ( 67.63343560358070761, 69.65666620391252195, -0.2166577581527749097 ) ) ;
#53584 = CARTESIAN_POINT ( 'NONE',  ( 76.00333185707168582, 51.30992116068062359, 16.13885810330130255 ) ) ;
#53583 = FACE_OUTER_BOUND ( 'NONE', #81224, .T. ) ;
#53585 = CARTESIAN_POINT ( 'NONE',  ( -36.52772323645827868, 26.41323893245353105, 10.00000000000000000 ) ) ;
#53586 = EDGE_CURVE ( 'NONE', #29851, #16015, #21933, .T. ) ;
#53587 = CARTESIAN_POINT ( 'NONE',  ( 69.42144788871625849, 62.89730317705431872, 13.10748580973936939 ) ) ;
#53588 = CARTESIAN_POINT ( 'NONE',  ( 205.5852664446427411, 274.5628685607306920, -12.83526618994635449 ) ) ;
#53589 = CARTESIAN_POINT ( 'NONE',  ( 196.2609093297512857, 290.7131288316392670, 16.03897268885959448 ) ) ;
#53590 = CARTESIAN_POINT ( 'NONE',  ( 71.94524616390265237, 71.98672967291759051, 2.832588148037977760 ) ) ;
#53591 = EDGE_CURVE ( 'NONE', #86862, #28142, #83779, .T. ) ;
#53592 = CARTESIAN_POINT ( 'NONE',  ( 21.28450569914983248, 195.3464784336661637, 1.353441290958777327E-15 ) ) ;
#53593 = CARTESIAN_POINT ( 'NONE',  ( 48.37494963522306080, 207.9244531367911293, -4.594050593750046652 ) ) ;
#53594 = CARTESIAN_POINT ( 'NONE',  ( 157.4656258344471098, 257.9085309395441641, 18.30485740784190796 ) ) ;
#53595 = CARTESIAN_POINT ( 'NONE',  ( 199.3359313799735162, 277.8054090533971134, 16.38672730308284997 ) ) ;
#53596 = CARTESIAN_POINT ( 'NONE',  ( 82.87264987968924856, 49.76174821331473197, -13.67541387821871446 ) ) ;
#53597 = CARTESIAN_POINT ( 'NONE',  ( 147.1836429658426084, 243.5327760586659451, 1.948934522072303157E-15 ) ) ;
#53598 = CARTESIAN_POINT ( 'NONE',  ( 48.95103868752456577, 97.61288834769685252, -10.00000000000000000 ) ) ;
#53599 = CARTESIAN_POINT ( 'NONE',  ( 26.36427918851389762, 18.14754757982090538, -5.678558825948275768 ) ) ;
#53600 = CARTESIAN_POINT ( 'NONE',  ( 198.5511052797322975, 286.7463930869835167, -17.24711022262289006 ) ) ;
#53601 = CARTESIAN_POINT ( 'NONE',  ( 149.3801359649374092, 271.9130101976182914, -11.41245530317637424 ) ) ;
#53602 = CARTESIAN_POINT ( 'NONE',  ( 6.569006713621681648, 25.83396525600388216, -2.839279412974133887 ) ) ;
#53603 = CARTESIAN_POINT ( 'NONE',  ( 53.67935523340274528, 210.9869531367911009, 4.594050593750046652 ) ) ;
#53604 = CARTESIAN_POINT ( 'NONE',  ( 158.6590954928334440, 256.3327925383782144, -16.23563070158754584 ) ) ;
#53605 = CARTESIAN_POINT ( 'NONE',  ( 194.3162776146270119, 290.4640039533715026, 16.60662885859720816 ) ) ;
#53606 = CARTESIAN_POINT ( 'NONE',  ( 159.6419305724666344, 254.1390605605417079, 16.92015248457581933 ) ) ;
#53607 = CARTESIAN_POINT ( 'NONE',  ( 72.04273812837081437, 59.28583566120335746, 15.34548535902080246 ) ) ;
#53608 = CARTESIAN_POINT ( 'NONE',  ( 153.3155690579966688, 265.0966401306517923, 17.21748418396146363 ) ) ;
#53609 = AXIS2_PLACEMENT_3D ( 'NONE', #32197, #70189, #15487 ) ;
#53610 = LINE ( 'NONE', #54101, #25063 ) ;
#53611 = CARTESIAN_POINT ( 'NONE',  ( 87.70720954677142345, 45.31332896125894649, -6.372777740749068442 ) ) ;
#53612 = CARTESIAN_POINT ( 'NONE',  ( 120.0388121219831277, 230.1115022471901739, -5.000000000000041744 ) ) ;
#53613 = CARTESIAN_POINT ( 'NONE',  ( 200.6129772034685175, 283.1751261563724142, 18.36811917402039640 ) ) ;
#53614 = ADVANCED_FACE ( 'NONE', ( #22435 ), #28534, .F. ) ;
#53615 = CARTESIAN_POINT ( 'NONE',  ( 162.8484966408963714, 268.3243502197477142, -16.55345495915420528 ) ) ;
#53616 = VERTEX_POINT ( 'NONE', #53327 ) ;
#53617 = CARTESIAN_POINT ( 'NONE',  ( 77.07955643721723504, 49.57937043545834399, 15.50364152264906004 ) ) ;
#53618 = ORIENTED_EDGE ( 'NONE', *, *, #59917, .F. ) ;
#53619 = CARTESIAN_POINT ( 'NONE',  ( 159.7132918459648181, 254.0154592091499239, -16.90058287995827158 ) ) ;
#53620 = CARTESIAN_POINT ( 'NONE',  ( 190.3130917849182424, 278.9726400120082417, -16.58120985382013046 ) ) ;
#53621 = CARTESIAN_POINT ( 'NONE',  ( 205.1140127274842655, 272.9918749453946702, -10.94721916815361062 ) ) ;
#53622 = ORIENTED_EDGE ( 'NONE', *, *, #90259, .F. ) ;
#53623 = CARTESIAN_POINT ( 'NONE',  ( 62.37595398666918811, 213.4865022471903444, 10.00000000000009415 ) ) ;
#53625 = EDGE_CURVE ( 'NONE', #43189, #70075, #73573, .T. ) ;
#53624 = CARTESIAN_POINT ( 'NONE',  ( 79.06748585747224922, 46.07688976562260308, -12.67383739758977335 ) ) ;
#53626 = CARTESIAN_POINT ( 'NONE',  ( 148.0637215040603394, 274.1931069276759558, -7.795633835291665648 ) ) ;
#53627 = DIRECTION ( 'NONE',  ( 0.000000000000000000, 0.000000000000000000, -1.000000000000000000 ) ) ;
#53628 = CYLINDRICAL_SURFACE ( 'NONE', #12687, 7.273499999999997634 ) ;
#53629 = ORIENTED_EDGE ( 'NONE', *, *, #59693, .F. ) ;
#53630 = CARTESIAN_POINT ( 'NONE',  ( 24.39888929631063519, 19.80170272979926693, 7.433330006724137462 ) ) ;
#53631 = CARTESIAN_POINT ( 'NONE',  ( -37.96271243472389756, 25.23297040071578223, 10.00000000000000000 ) ) ;
#53632 = DIRECTION ( 'NONE',  ( -0.4803199113995137437, 0.8770933717188629242, 0.000000000000000000 ) ) ;
#53633 = EDGE_CURVE ( 'NONE', #55290, #74173, #27454, .T. ) ;
#53634 = VERTEX_POINT ( 'NONE', #20971 ) ;
#53635 = LINE ( 'NONE', #85084, #7727 ) ;
#53636 = DIRECTION ( 'NONE',  ( -0.5891075386695772131, -0.8080546441192405505, 0.000000000000000000 ) ) ;
#53637 = VERTEX_POINT ( 'NONE', #92375 ) ;
#53638 = CARTESIAN_POINT ( 'NONE',  ( 174.7360925947785972, 286.2149905754307042, 10.56760205176437672 ) ) ;
#53640 = CARTESIAN_POINT ( 'NONE',  ( 67.91983461438699976, 65.33094372862520061, -10.47544803142360337 ) ) ;
#53639 = CARTESIAN_POINT ( 'NONE',  ( 163.2243841140381733, 283.7100838097323958, -3.089421799144727920 ) ) ;
#53641 = CARTESIAN_POINT ( 'NONE',  ( 163.4139553296302267, 247.6057220337265505, -10.31482883765270842 ) ) ;
#53642 = CARTESIAN_POINT ( 'NONE',  ( 204.3951397407346064, 276.6242284793436852, 14.79595971842109137 ) ) ;
#53643 = CARTESIAN_POINT ( 'NONE',  ( 159.5573297132660002, 254.2855935470410031, 16.91607698584599007 ) ) ;
#53644 = CARTESIAN_POINT ( 'NONE',  ( 161.3533544474441612, 263.1708485045204498, -17.19112518918186083 ) ) ;
#53645 = CARTESIAN_POINT ( 'NONE',  ( 164.6623933277139997, 245.4433639909459544, 5.552253915569078657 ) ) ;
#53646 = CARTESIAN_POINT ( 'NONE',  ( 177.6810254821819797, 268.6267531607944079, 17.00611995725074621 ) ) ;
#53647 = CARTESIAN_POINT ( 'NONE',  ( 181.7393891144199642, 260.2674940340181138, 9.489685412558293010 ) ) ;
#53648 = CARTESIAN_POINT ( 'NONE',  ( 66.66973629016931113, 218.4869531367911293, 4.594050593750046652 ) ) ;
#53649 = ORIENTED_EDGE ( 'NONE', *, *, #40629, .F. ) ;
#53650 = CARTESIAN_POINT ( 'NONE',  ( 172.5238994923043947, 264.9055888575895779, 15.91205857390302292 ) ) ;
#53651 = CARTESIAN_POINT ( 'NONE',  ( 163.7226971571442675, 281.6571063072398715, -10.85737102627868467 ) ) ;
#53652 = VERTEX_POINT ( 'NONE', #69529 ) ;
#53653 = CARTESIAN_POINT ( 'NONE',  ( 172.0910100529608258, 260.0785035667472584, 15.53398388876759206 ) ) ;
#53654 = EDGE_LOOP ( 'NONE', ( #87777, #69174, #33131, #7944 ) ) ;
#53655 = FACE_BOUND ( 'NONE', #31941, .T. ) ;
#53656 = CARTESIAN_POINT ( 'NONE',  ( 66.84316555279445993, 67.52164038403083168, 6.631609150140850950 ) ) ;
#53657 = CARTESIAN_POINT ( 'NONE',  ( 195.7585776938734625, 285.5848788086319701, 16.95618921707195170 ) ) ;
#53659 = B_SPLINE_SURFACE_WITH_KNOTS ( 'NONE', 3, 1, ( 
 ( #79057, #56202 ),
 ( #71935, #94258 ),
 ( #78538, #47611 ),
 ( #95278, #8624 ),
 ( #85683, #17731 ),
 ( #2026, #25841 ),
 ( #37632, #39490 ),
 ( #32911, #9125 ),
 ( #63818, #25315 ),
 ( #94753, #56715 ),
 ( #87199, #48634 ),
 ( #68543, #60932 ),
 ( #93255, #47113 ),
 ( #97249, #80565 ),
 ( #82063, #72948 ),
 ( #80062, #26822 ),
 ( #33942, #50117 ),
 ( #12121, #11635 ),
 ( #89187, #74442 ),
 ( #43500, #58690 ),
 ( #10631, #41507 ),
 ( #19736, #96758 ),
 ( #27326, #1417 ),
 ( #71822, #8508 ),
 ( #2421, #71321 ),
 ( #1913, #86562 ),
 ( #47495, #16101 ),
 ( #405, #85036 ),
 ( #93639, #63201 ),
 ( #16598, #93134 ),
 ( #62685, #15584 ),
 ( #48512, #40381 ),
 ( #33299, #78420 ),
 ( #47990, #25194 ) ),
 .UNSPECIFIED., .T., .F., .F.,
 ( 4, 2, 2, 2, 2, 2, 2, 2, 2, 2, 2, 2, 2, 2, 2, 2, 4 ),
 ( 2, 2 ),
 ( 0.000000000000000000, 0.06250000000000000000, 0.1250000000000000000, 0.1875000000000000000, 0.2500000000000000000, 0.3125000000000000000, 0.3750000000000000000, 0.4375000000000000000, 0.5000000000000000000, 0.5625000000000000000, 0.6250000000000000000, 0.6875000000000000000, 0.7500000000000000000, 0.8125000000000000000, 0.8750000000000000000, 0.9375000000000000000, 1.000000000000000000 ),
 ( 0.000000000000000000, 1.000000000000000000 ),
 .UNSPECIFIED. ) ;
#53658 = CARTESIAN_POINT ( 'NONE',  ( 87.20272978483724557, 43.17595422555252327, -1.293722201381849679 ) ) ;
#53660 = CARTESIAN_POINT ( 'NONE',  ( 81.17432035541970947, 55.57579169957366361, 16.36820043613993292 ) ) ;
#53661 = CARTESIAN_POINT ( 'NONE',  ( 155.2419697281468416, 261.7600162942170527, 18.58580762350309357 ) ) ;
#53663 = B_SPLINE_CURVE_WITH_KNOTS ( 'NONE', 3,
 ( #46491, #40388, #94647, #8514, #39383, #94149, #55093, #24702, #911, #56086, #55584, #47996, #24212, #47502, #78940, #17614, #48520, #10021, #40883, #69801, #71832, #25725, #411, #31300, #62188, #79951, #27715, #57592, #42388, #95668, #96648, #97149, #11028, #26712, #56605, #26216, #80964, #57092, #2943, #66693, #3910, #18625, #4401, #97629, #49502, #73321 ),
 .UNSPECIFIED., .F., .F.,
 ( 4, 2, 2, 2, 2, 2, 2, 2, 2, 2, 2, 2, 2, 2, 2, 2, 2, 2, 2, 2, 2, 2, 4 ),
 ( 0.002655933148385926021, 0.003065569018622698195, 0.003270386953741059345, 0.003372795921300235367, 0.003475204888859411822, 0.003680022823977764299, 0.003884840759096116775, 0.004294476629332821295, 0.005113748369806233804, 0.005933020110279646313, 0.006752291850753057954, 0.007571563591226471331, 0.007673972558785656893, 0.007725177042565249674, 0.007776381526344843323, 0.007827586010124435237, 0.007878790493904028885, 0.007981199461463143324, 0.008186017396581375671, 0.008390835331699609753, 0.008595653266817843835, 0.008800471201936079652, 0.009210107072172546080 ),
 .UNSPECIFIED. ) ;
#53662 = CARTESIAN_POINT ( 'NONE',  ( 72.47531805799239635, 69.29348212587751732, 9.109228493206927624 ) ) ;
#53664 = CARTESIAN_POINT ( 'NONE',  ( 86.20995510670323370, 211.3923013555409796, 4.594050593750050204 ) ) ;
#53665 = ORIENTED_EDGE ( 'NONE', *, *, #37494, .T. ) ;
#53666 = FACE_OUTER_BOUND ( 'NONE', #56984, .T. ) ;
#53667 = ORIENTED_EDGE ( 'NONE', *, *, #81114, .T. ) ;
#53668 = ADVANCED_FACE ( 'NONE', ( #41490 ), #40976, .F. ) ;
#53669 = CARTESIAN_POINT ( 'NONE',  ( 163.7627442285549080, 260.9594149212073262, -17.29108549316627119 ) ) ;
#53670 = B_SPLINE_CURVE_WITH_KNOTS ( 'NONE', 3,
 ( #84610, #29381, #37454, #82636, #14676, #60248, #6583, #90226, #13681, #75488, #90729, #6074, #21769, #36967, #37947, #68858 ),
 .UNSPECIFIED., .F., .F.,
 ( 4, 2, 2, 2, 2, 2, 2, 4 ),
 ( 0.000000000000000000, 0.0003786681000628067551, 0.0007573362001256135102, 0.001136004300188420265, 0.001514672400251227020, 0.001893340500314033992, 0.002272008600376840531, 0.003029344800502390290 ),
 .UNSPECIFIED. ) ;
#53671 = CARTESIAN_POINT ( 'NONE',  ( 76.02744352951765450, 65.34233732453844823, -14.42760839744433632 ) ) ;
#53672 = CARTESIAN_POINT ( 'NONE',  ( 206.4229368915142686, 273.1119807867502800, 10.31819530520674810 ) ) ;
#53673 = CARTESIAN_POINT ( 'NONE',  ( 162.0589963607739321, 283.8874982432868705, 0.5155476865025827582 ) ) ;
#53674 = CARTESIAN_POINT ( 'NONE',  ( 194.9499559406243918, 279.5747724307917679, 17.51673600049429780 ) ) ;
#53675 = CARTESIAN_POINT ( 'NONE',  ( 24.55112987542764458, 40.41347472807389352, 10.00000000000000000 ) ) ;
#53676 = ORIENTED_EDGE ( 'NONE', *, *, #99265, .F. ) ;
#53677 = CARTESIAN_POINT ( 'NONE',  ( 87.76435223195018409, 44.22492802364795494, 4.686297260842066770 ) ) ;
#53678 = CARTESIAN_POINT ( 'NONE',  ( 156.6772991465628309, 274.1558122050410020, 13.60064047269150400 ) ) ;
#53679 = CARTESIAN_POINT ( 'NONE',  ( 164.2312669802896892, 282.6376396295875111, -10.04520723185695097 ) ) ;
#53680 = CARTESIAN_POINT ( 'NONE',  ( 201.4463813434794019, 281.7316278426353620, -17.16864527463587820 ) ) ;
#53681 = CARTESIAN_POINT ( 'NONE',  ( 151.3511865740561007, 278.6745403919405248, -1.693856907688049862 ) ) ;
#53682 = DIRECTION ( 'NONE',  ( -0.000000000000000000, -0.000000000000000000, -1.000000000000000000 ) ) ;
#53683 = CARTESIAN_POINT ( 'NONE',  ( 195.9563588169494892, 264.9583988535660524, 5.383380191835067663 ) ) ;
#53684 = CARTESIAN_POINT ( 'NONE',  ( 165.8975677354378035, 271.5909624305264174, 17.28637137770206067 ) ) ;
#53685 = CARTESIAN_POINT ( 'NONE',  ( -21.58168810074490551, 24.33735145887882112, -10.00000000000000000 ) ) ;
#53686 = CARTESIAN_POINT ( 'NONE',  ( 184.6470863607480339, 263.8121736845355940, -12.21359121072102560 ) ) ;
#53687 = CARTESIAN_POINT ( 'NONE',  ( 83.83627951286173641, 51.93148169815736281, 14.52308898787406655 ) ) ;
#53688 = CARTESIAN_POINT ( 'NONE',  ( 195.2218307224750902, 263.8590524788139646, 0.8427596141219795278 ) ) ;
#53689 = ORIENTED_EDGE ( 'NONE', *, *, #81984, .F. ) ;
#53690 = EDGE_CURVE ( 'NONE', #55671, #88888, #72079, .T. ) ;
#53691 = CARTESIAN_POINT ( 'NONE',  ( 190.8545714895799392, 300.0771806536980648, -5.516553996882049837 ) ) ;
#53692 = CARTESIAN_POINT ( 'NONE',  ( -13.83322559834489418, 103.7219465388319577, 43.99456462701717641 ) ) ;
#53693 = CARTESIAN_POINT ( 'NONE',  ( 207.2383675728608239, 271.6996134166075763, 7.873592648726489784 ) ) ;
#53695 = CARTESIAN_POINT ( 'NONE',  ( 74.02137029423680303, 55.08862506472077314, 16.60352351745309107 ) ) ;
#53694 = CARTESIAN_POINT ( 'NONE',  ( 155.6518451030846961, 261.0500913200531841, 17.91778754207898317 ) ) ;
#53696 = ADVANCED_FACE ( 'NONE', ( #11129 ), #63302, .T. ) ;
#53697 = CARTESIAN_POINT ( 'NONE',  ( 25.97889144642132919, 17.12755873383626692, -6.180339887498949025 ) ) ;
#53698 = CARTESIAN_POINT ( 'NONE',  ( -19.65312891409030271, 93.06504152958497400, -20.00000000000000355 ) ) ;
#53699 = CARTESIAN_POINT ( 'NONE',  ( 166.3564281690869677, 285.9358929195967107, -3.185848211132425334 ) ) ;
#53700 = DIRECTION ( 'NONE',  ( 0.4851478631379963491, -0.8403007481384849875, 0.2419218955996714493 ) ) ;
#53701 = CARTESIAN_POINT ( 'NONE',  ( 159.5204760365350012, 254.3494259875849082, 16.90107507090185379 ) ) ;
#53702 = EDGE_CURVE ( 'NONE', #25608, #18420, #40705, .T. ) ;
#53703 =( BOUNDED_CURVE ( )  B_SPLINE_CURVE ( 2, ( #84904, #7879, #70661, #61557, #47357, #76766, #86429, #94008, #23049 ),
 .UNSPECIFIED., .F., .T. ) 
 B_SPLINE_CURVE_WITH_KNOTS ( ( 3, 2, 2, 2, 3 ),
 ( 0.2701612903225806273, 0.2715053763440860024, 0.2741935483870967527, 0.2768817204301075030, 0.2782258064516128782 ),
 .UNSPECIFIED. ) 
 CURVE ( )  GEOMETRIC_REPRESENTATION_ITEM ( )  RATIONAL_B_SPLINE_CURVE ( ( 0.9330127018922194093, 0.9330127018922194093, 1.000000000000000000, 0.8660254037844387076, 1.000000000000000000, 0.8660254037844387076, 1.000000000000000000, 0.9330127018922194093, 0.9330127018922194093 ) ) 
 REPRESENTATION_ITEM ( '' )  );
#53704 = CARTESIAN_POINT ( 'NONE',  ( 147.6614140599763232, 249.3927522451418213, 10.00000000000009592 ) ) ;
#53705 = FACE_OUTER_BOUND ( 'NONE', #36359, .T. ) ;
#53706 = ORIENTED_EDGE ( 'NONE', *, *, #67829, .F. ) ;
#53707 = CARTESIAN_POINT ( 'NONE',  ( 81.30818518503046732, 58.89441083166271085, 0.000000000000000000 ) ) ;
#53708 = CARTESIAN_POINT ( 'NONE',  ( 72.88378191513223214, 70.30562453083473429, -8.123734786539317909 ) ) ;
#53709 = CARTESIAN_POINT ( 'NONE',  ( 138.5626868278036454, 239.2592609112380160, 2.679491924311254714 ) ) ;
#53710 = CARTESIAN_POINT ( 'NONE',  ( 198.7829547491859330, 286.3448180261817129, -18.59838968157616179 ) ) ;
#53711 = CARTESIAN_POINT ( 'NONE',  ( 10.18872876104421366, 182.8149278399160664, -9.188101187500095079 ) ) ;
#53712 = VECTOR ( 'NONE', #27641, 1000.000000000000000 ) ;
#53713 = CARTESIAN_POINT ( 'NONE',  ( 27.28458541428561901, 34.49103043416550918, -8.090169943749479842 ) ) ;
#53714 = CARTESIAN_POINT ( 'NONE',  ( 78.07911708839047549, 58.44437905099346864, 16.56270159866548042 ) ) ;
#53715 = CARTESIAN_POINT ( 'NONE',  ( 171.3229631070106223, 271.3642985138579320, -16.56375429974980662 ) ) ;
#53716 = DIRECTION ( 'NONE',  ( 0.5344452582589497291, -0.8452030915256549815, 0.000000000000000000 ) ) ;
#53717 = CARTESIAN_POINT ( 'NONE',  ( 73.08094384907833785, 54.14441083166272506, 0.000000000000000000 ) ) ;
#53718 = CARTESIAN_POINT ( 'NONE',  ( 187.6248024056100689, 259.1780923452019465, -0.7908679967713718728 ) ) ;
#53719 = CARTESIAN_POINT ( 'NONE',  ( 183.0741553274718001, 295.7116116299331452, 1.042336010579862915 ) ) ;
#53720 = CARTESIAN_POINT ( 'NONE',  ( 66.70608100559137199, 215.9865022471902591, -10.00000000000009415 ) ) ;
#53721 = CARTESIAN_POINT ( 'NONE',  ( 35.06352437372438402, 42.01751292744059185, 6.180339887498949913 ) ) ;
#53722 = EDGE_CURVE ( 'NONE', #64894, #96192, #8071, .T. ) ;
#53723 = CARTESIAN_POINT ( 'NONE',  ( 190.6036479972031259, 300.5117928913073797, -0.6824572005520307405 ) ) ;
#53724 = CARTESIAN_POINT ( 'NONE',  ( 27.18482440607884243, 180.3768266524160140, 9.188101187500098632 ) ) ;
#53725 = CARTESIAN_POINT ( 'NONE',  ( 66.50602851107427682, 67.82027345181231226, 6.844793838059969104 ) ) ;
#53726 =( LENGTH_UNIT ( ) NAMED_UNIT ( * ) SI_UNIT ( .MILLI., .METRE. ) );
#53727 = CARTESIAN_POINT ( 'NONE',  ( 41.60632629512001301, 26.94754757982092741, 5.678558825948272215 ) ) ;
#53728 = CARTESIAN_POINT ( 'NONE',  ( 199.1944722252943905, 285.6320488493591938, -18.17555833707144686 ) ) ;
#53729 = CARTESIAN_POINT ( 'NONE',  ( 207.0200405408487541, 272.0777669287182334, 6.494273599193515878 ) ) ;
#53730 = CARTESIAN_POINT ( 'NONE',  ( 186.1634877655031346, 266.9843438079278144, 13.21246304542636629 ) ) ;
#53731 = CARTESIAN_POINT ( 'NONE',  ( 162.4616894431812284, 280.2021887225156433, -9.893998380673561854 ) ) ;
#53732 = CARTESIAN_POINT ( 'NONE',  ( 162.1586611819999177, 280.6028376852936503, 8.927607144935116423 ) ) ;
#53733 = SHAPE_DEFINITION_REPRESENTATION ( #81570, #94304 ) ;
#53734 = CARTESIAN_POINT ( 'NONE',  ( 19.94606896448370392, 26.91421378149918553, 9.188101187500008038 ) ) ;
#53735 = CARTESIAN_POINT ( 'NONE',  ( 6.588875291771465470, 26.73705186507752174, -3.090169943749475845 ) ) ;
#53736 = CARTESIAN_POINT ( 'NONE',  ( 71.52294418693975331, 59.11029950019791812, 15.31128158434694519 ) ) ;
#53737 = CARTESIAN_POINT ( 'NONE',  ( 194.2321518193436987, 294.2270399159019121, 13.98132384850917020 ) ) ;
#53738 = ORIENTED_EDGE ( 'NONE', *, *, #44824, .T. ) ;
#53739 = CARTESIAN_POINT ( 'NONE',  ( -17.26243516413818924, 24.35187462261283997, -10.00000000000000000 ) ) ;
#53740 = FACE_OUTER_BOUND ( 'NONE', #98417, .T. ) ;
#53741 = CARTESIAN_POINT ( 'NONE',  ( 81.43393898548352183, 42.46093713096067290, 7.472239458194745332 ) ) ;
#53742 = CARTESIAN_POINT ( 'NONE',  ( 153.4232513496498598, 270.1086993216917449, 15.21047082690287588 ) ) ;
#53743 = EDGE_LOOP ( 'NONE', ( #9682, #31975, #17136, #95235 ) ) ;
#53744 = DIRECTION ( 'NONE',  ( 0.2701803667135113662, 0.9628097264997651505, 0.000000000000000000 ) ) ;
#53745 = CARTESIAN_POINT ( 'NONE',  ( 72.35257617177605027, 71.70739429922333841, -5.765621772327581773 ) ) ;
#53746 = CARTESIAN_POINT ( 'NONE',  ( 77.01650215582269254, 63.78770094747507358, 14.95761047872078642 ) ) ;
#53747 = CARTESIAN_POINT ( 'NONE',  ( 181.0230579576209209, 257.1489723966709562, -7.736786952959286978 ) ) ;
#53748 = ORIENTED_EDGE ( 'NONE', *, *, #44937, .F. ) ;
#53749 = ORIENTED_EDGE ( 'NONE', *, *, #58963, .T. ) ;
#53750 = B_SPLINE_CURVE_WITH_KNOTS ( 'NONE', 3,
 ( #12264, #82699, #57344, #35041, #74066, #97864, #50736, #5154, #49756, #35548, #80707, #58339, #96395, #66449, #3191, #4146, #96900, #11770, #13266, #11283, #82201, #59317, #97376, #58824, #27942, #19388, #89315, #50247, #20362, #34074, #12771, #64965, #3673, #36034, #51233, #66934, #42633, #43636, #28435, #74576, #90297, #26468 ),
 .UNSPECIFIED., .F., .F.,
 ( 4, 2, 2, 2, 2, 2, 2, 2, 2, 2, 2, 2, 2, 2, 2, 2, 2, 2, 2, 2, 4 ),
 ( 0.002186794962226318740, 0.002620931419558167677, 0.002837999648224146573, 0.003055067876890125468, 0.003163601991223173246, 0.003272136105556221024, 0.003489204334222307038, 0.003923340791554368913, 0.004791613706218474447, 0.005659886620882579981, 0.006528159535546685516, 0.006962295992878701420, 0.007396432450210717324, 0.007504966564543741683, 0.007559233621710246057, 0.007613500678876752165, 0.007722034793209806014, 0.007830568907542859863, 0.008264705364875214039, 0.008698841822207566479, 0.009132978279539920655 ),
 .UNSPECIFIED. ) ;
#53752 = PLANE ( 'NONE',  #45908 ) ;
#53751 = CARTESIAN_POINT ( 'NONE',  ( 201.8854650512935507, 280.0099856999216854, 16.08627997847975166 ) ) ;
#53753 = ORIENTED_EDGE ( 'NONE', *, *, #7738, .T. ) ;
#53754 = CARTESIAN_POINT ( 'NONE',  ( 201.1755594471486859, 282.2007051268825535, -18.15567516623250910 ) ) ;
#53755 = CARTESIAN_POINT ( 'NONE',  ( 30.82863370761418409, 19.92755873383627119, 6.180339887498953466 ) ) ;
#53756 = CARTESIAN_POINT ( 'NONE',  ( 80.19730562280793151, 57.80653512312768072, 16.60264294324889178 ) ) ;
#53757 = CARTESIAN_POINT ( 'NONE',  ( 54.07885559584777013, 190.4824982072973967, 3.021315404115420679E-15 ) ) ;
#53758 = ORIENTED_EDGE ( 'NONE', *, *, #35961, .T. ) ;
#53759 = CARTESIAN_POINT ( 'NONE',  ( 189.8533352240220893, 301.8113727360248504, -0.2033756396389863053 ) ) ;
#53760 = EDGE_CURVE ( 'NONE', #65497, #27171, #20713, .T. ) ;
#53761 = EDGE_LOOP ( 'NONE', ( #28203, #70634, #92224, #27994 ) ) ;
#53762 = CARTESIAN_POINT ( 'NONE',  ( 74.39841895140679640, 68.21392270468032848, 11.45628786500076579 ) ) ;
#53763 = CARTESIAN_POINT ( 'NONE',  ( -20.01016364259690405, 23.06595206263087050, -10.00000000000000000 ) ) ;
#53764 = ORIENTED_EDGE ( 'NONE', *, *, #15160, .F. ) ;
#53765 = CARTESIAN_POINT ( 'NONE',  ( 190.1751179328237242, 301.2540287353828035, 3.252640783176552475 ) ) ;
#53766 = DIRECTION ( 'NONE',  ( -0.8660254037844379305, -0.5000000000000014433, -0.000000000000000000 ) ) ;
#53767 = EDGE_LOOP ( 'NONE', ( #15237, #80256, #98296, #61720, #41932 ) ) ;
#53768 = CARTESIAN_POINT ( 'NONE',  ( -10.31370568705291291, 72.11042850481820210, 14.81003180042302425 ) ) ;
#53769 = CARTESIAN_POINT ( 'NONE',  ( 190.7779368023172708, 300.2099158256590385, 8.142228434510803581 ) ) ;
#53770 = CARTESIAN_POINT ( 'NONE',  ( 177.5337925685473408, 280.1858537220425092, 16.79564202278857721 ) ) ;
#53771 = CARTESIAN_POINT ( 'NONE',  ( 83.63039906669357038, 52.33209546183138627, 14.75250088251173075 ) ) ;
#53772 = EDGE_LOOP ( 'NONE', ( #53510, #61501, #22655, #13869 ) ) ;
#53773 = ORIENTED_EDGE ( 'NONE', *, *, #80291, .T. ) ;
#53774 = CARTESIAN_POINT ( 'NONE',  ( 87.13197742215592712, 46.34264934104920997, 8.620802749433925882 ) ) ;
#53775 = DIRECTION ( 'NONE',  ( -0.7352104281592295454, 0.6778389383370672094, 0.000000000000000000 ) ) ;
#53776 = CARTESIAN_POINT ( 'NONE',  ( 148.3997536239841679, 273.6110822229926498, 8.713694244701960301 ) ) ;
#53777 = CARTESIAN_POINT ( 'NONE',  ( 149.5633513747893346, 271.5956717990251832, 12.83777201928511325 ) ) ;
#53778 = CARTESIAN_POINT ( 'NONE',  ( 5.871984111234073822, 29.22396284167520619, -10.00000000000000000 ) ) ;
#53779 = CARTESIAN_POINT ( 'NONE',  ( 73.99515186948657686, 54.97541550358009488, -16.60506967685200763 ) ) ;
#53780 = CARTESIAN_POINT ( 'NONE',  ( 147.0276296945837373, 275.9876705829954062, 0.7617065417431535534 ) ) ;
#53781 = CARTESIAN_POINT ( 'NONE',  ( 163.5652124800741944, 257.6669317359933302, 15.50305180493005075 ) ) ;
#53782 = AXIS2_PLACEMENT_3D ( 'NONE', #69773, #380, #66906 ) ;
#53783 = CARTESIAN_POINT ( 'NONE',  ( 69.36291866569143849, 66.30083069348447111, 10.37424756039578710 ) ) ;
#53784 = VECTOR ( 'NONE', #65252, 999.9999999999998863 ) ;
#53785 = LINE ( 'NONE', #52308, #6248 ) ;
#53786 = LINE ( 'NONE', #83247, #91379 ) ;
#53787 = CARTESIAN_POINT ( 'NONE',  ( 69.12385011120056788, 65.62576829796853417, -10.87672581319109000 ) ) ;
#53788 = CARTESIAN_POINT ( 'NONE',  ( 78.61683564465192831, 47.48530518036562142, 14.24614870575583048 ) ) ;
#53789 = VERTEX_POINT ( 'NONE', #50104 ) ;
#53790 = CARTESIAN_POINT ( 'NONE',  ( 206.4044394810958067, 269.6475539527112346, -2.777257397153266361 ) ) ;
#53791 = CARTESIAN_POINT ( 'NONE',  ( 84.58391814946246257, 42.10937633166320637, 0.1196556675772392914 ) ) ;
#53792 = CARTESIAN_POINT ( 'NONE',  ( 87.71554304996901408, 45.29005973903561966, -7.157883044737483047 ) ) ;
#53793 = AXIS2_PLACEMENT_3D ( 'NONE', #29350, #45523, #60214 ) ;
#53794 = CARTESIAN_POINT ( 'NONE',  ( 79.47004366810152476, 45.79327920381835071, 12.92587503265258064 ) ) ;
#53795 = CARTESIAN_POINT ( 'NONE',  ( 179.7730072551474905, 282.8179472056182817, -15.42817071794396000 ) ) ;
#53796 = CARTESIAN_POINT ( 'NONE',  ( 190.7982574810033611, 262.8194055429554510, 8.405793748174573921 ) ) ;
#53797 = CARTESIAN_POINT ( 'NONE',  ( 169.2038551074579402, 285.0728575209601559, -7.946202499671376707 ) ) ;
#53798 = ORIENTED_EDGE ( 'NONE', *, *, #11962, .F. ) ;
#53799 = CARTESIAN_POINT ( 'NONE',  ( 162.6541320028305506, 248.9217746405196294, -10.16950121496441817 ) ) ;
#53800 = CARTESIAN_POINT ( 'NONE',  ( 72.29498584114780613, 71.54824044162640462, 5.047338649552161272 ) ) ;
#53801 = CARTESIAN_POINT ( 'NONE',  ( 47.05812965368398437, 204.6427522451419350, -10.00000000000009415 ) ) ;
#53802 = CARTESIAN_POINT ( 'NONE',  ( 126.9399520566163773, 244.0958772461660544, -9.188101187500095079 ) ) ;
#53803 = CARTESIAN_POINT ( 'NONE',  ( 151.3124059063077311, 268.5662204852269497, -14.45542936000225609 ) ) ;
#53804 = AXIS2_PLACEMENT_3D ( 'NONE', #55409, #40720, #31614 ) ;
#53805 = LINE ( 'NONE', #83268, #64267 ) ;
#53806 = CARTESIAN_POINT ( 'NONE',  ( 187.4521490836430360, 281.3311025107105934, -17.05609064705406297 ) ) ;
#53807 = CARTESIAN_POINT ( 'NONE',  ( 49.09245556086620610, 93.56363653685789927, 10.00000000000000000 ) ) ;
#53808 = CARTESIAN_POINT ( 'NONE',  ( 48.05019010880389629, 207.7369531367911293, -4.594050593750048428 ) ) ;
#53809 = CARTESIAN_POINT ( 'NONE',  ( 178.7939207709925427, 291.7564144783525535, -6.099094555038819365 ) ) ;
#53810 = CARTESIAN_POINT ( 'NONE',  ( 68.52062231897753009, 66.34521348645475314, -9.781991027147515894 ) ) ;
#53811 = VERTEX_POINT ( 'NONE', #42971 ) ;
#53812 = CARTESIAN_POINT ( 'NONE',  ( 72.17391747568852622, 67.01067792759801023, 11.32486803574759904 ) ) ;
#53813 = CARTESIAN_POINT ( 'NONE',  ( 178.9271355275119504, 266.3440916513727643, 15.18250009252006016 ) ) ;
#53814 = ADVANCED_FACE ( 'NONE', ( #36385 ), #2833, .F. ) ;
#53815 = CARTESIAN_POINT ( 'NONE',  ( 72.21491844529387549, 53.64441083166271085, 0.000000000000000000 ) ) ;
#53816 = CARTESIAN_POINT ( 'NONE',  ( 147.5634954182374372, 275.0595239235922236, 4.682022975662822439 ) ) ;
#53817 = CARTESIAN_POINT ( 'NONE',  ( 50.18541494347881837, 88.31343213334855591, 10.00000000000000000 ) ) ;
#53818 = B_SPLINE_CURVE_WITH_KNOTS ( 'NONE', 3,
 ( #71603, #46385, #62084, #68696, #99627, #48797, #15486, #2201, #95448, #79728, #77310, #10291, #94919, #25481, #41163, #97398, #11801, #50272, #3698, #96421, #43151, #97890, #20895, #80739, #73106, #36059, #43662, #74091, #81225, #88851, #27965, #66961, #42169, #3215, #34099, #28464, #34577, #82724, #81717, #66473, #42657, #4684, #49780, #59344 ),
 .UNSPECIFIED., .F., .F.,
 ( 4, 2, 2, 2, 2, 2, 2, 2, 2, 2, 2, 2, 2, 2, 2, 2, 2, 2, 2, 2, 2, 4 ),
 ( 0.0008670981119040801436, 0.001065074094278789692, 0.001164062085466145875, 0.001263050076653502059, 0.001461026059028214426, 0.001659002041402926793, 0.002054954006152456911, 0.002450905970901987030, 0.004034713829900430163, 0.004826617759399616167, 0.005222569724149247333, 0.005420545706524099346, 0.005519533697711450325, 0.005569027693305126682, 0.005618521688898802172, 0.005668015684492478529, 0.005717509680086154886, 0.005816497671273505865, 0.006014473653648208691, 0.006410425618397620415, 0.006806377583147032138, 0.007202329547896444729 ),
 .UNSPECIFIED. ) ;
#53819 = DIRECTION ( 'NONE',  ( 0.000000000000000000, 0.000000000000000000, -1.000000000000000000 ) ) ;
#53820 = ADVANCED_FACE ( 'NONE', ( #54561 ), #38374, .F. ) ;
#53821 = CARTESIAN_POINT ( 'NONE',  ( 181.5591343598143794, 261.9482418225283027, 13.16139462748061284 ) ) ;
#53822 = CARTESIAN_POINT ( 'NONE',  ( 113.3812418268423414, 226.2677522451417929, -5.000000000000041744 ) ) ;
#53823 = EDGE_CURVE ( 'NONE', #81228, #58030, #36890, .T. ) ;
#53824 = DIRECTION ( 'NONE',  ( 0.9995565931350004485, 0.02977611660964677581, 0.000000000000000000 ) ) ;
#53825 = ORIENTED_EDGE ( 'NONE', *, *, #27427, .F. ) ;
#53826 = EDGE_CURVE ( 'NONE', #28514, #74953, #98724, .T. ) ;
#53827 = CARTESIAN_POINT ( 'NONE',  ( 202.9689790241539242, 279.0944113002206564, 15.85114608332523289 ) ) ;
#53828 = CARTESIAN_POINT ( 'NONE',  ( 208.3194307158603067, 269.8271571267425770, -2.120200867047394855 ) ) ;
#53829 = CARTESIAN_POINT ( 'NONE',  ( 24.28913873611587348, 175.6423013555409796, -4.594050593750043987 ) ) ;
#53830 = CARTESIAN_POINT ( 'NONE',  ( 14.46184932687122604, 20.30066082961420904, -10.00000000000000533 ) ) ;
#53831 = CARTESIAN_POINT ( 'NONE',  ( 196.0499355695823169, 273.7105960426958973, 14.77316126107874084 ) ) ;
#53832 = CARTESIAN_POINT ( 'NONE',  ( 31.13482890205414222, 200.3297689869269220, -2.679491924311252493 ) ) ;
#53833 = DIRECTION ( 'NONE',  ( 0.2837547813814350617, 0.9281390619545438758, 0.2409172175609567979 ) ) ;
#53835 = CARTESIAN_POINT ( 'NONE',  ( 64.91088251055593616, 208.2833772461660544, -9.188101187500095079 ) ) ;
#53834 = CARTESIAN_POINT ( 'NONE',  ( 198.2724843312039695, 277.3699619827796710, -15.35028023985861800 ) ) ;
#53836 = CARTESIAN_POINT ( 'NONE',  ( 200.3134965941964651, 283.6938417875134064, 18.29802468362849766 ) ) ;
#53837 = CARTESIAN_POINT ( 'NONE',  ( 72.79159666541453078, 57.09351760226002881, 16.38642577662735533 ) ) ;
#53838 = CARTESIAN_POINT ( 'NONE',  ( 70.90848803616628970, 68.75243874516947074, 9.337650187172339855 ) ) ;
#53839 = CARTESIAN_POINT ( 'NONE',  ( 161.5029716424245407, 251.3413373469583973, -13.00020995489466458 ) ) ;
#53840 = EDGE_LOOP ( 'NONE', ( #13800, #76123, #55886, #71632 ) ) ;
#53841 = CARTESIAN_POINT ( 'NONE',  ( 162.1551341473669652, 267.3145892873122875, 16.48403697670416079 ) ) ;
#53842 = CARTESIAN_POINT ( 'NONE',  ( 9.620573139467140322, 176.3615022471902307, -10.00000000000009592 ) ) ;
#53843 = CARTESIAN_POINT ( 'NONE',  ( 164.3602934812760452, 245.9666162739349318, -7.171958108566009571 ) ) ;
#53844 = CARTESIAN_POINT ( 'NONE',  ( 135.2211464324225858, 255.0024278399160949, -9.188101187500093303 ) ) ;
#53845 = CARTESIAN_POINT ( 'NONE',  ( 33.10845880387886808, 31.06628583063843863, -9.188101187500006262 ) ) ;
#53846 = CARTESIAN_POINT ( 'NONE',  ( 164.5218961637583277, 259.6528873143451506, -16.87288754656431422 ) ) ;
#53847 = CARTESIAN_POINT ( 'NONE',  ( 186.9066306565648858, 261.1604336654457938, 6.359003367118981842 ) ) ;
#53848 = CARTESIAN_POINT ( 'NONE',  ( 206.4768661561222984, 273.0185725604343361, 11.39716120335626925 ) ) ;
#53850 = PLANE ( 'NONE',  #27988 ) ;
#53849 = CARTESIAN_POINT ( 'NONE',  ( 88.48648755238653507, 43.99326657310299282, 1.937087981213223786 ) ) ;
#53851 = CARTESIAN_POINT ( 'NONE',  ( 69.02454561260198318, 64.16955637294137205, 12.06084141314768132 ) ) ;
#53852 = ORIENTED_EDGE ( 'NONE', *, *, #84624, .F. ) ;
#53853 = DIRECTION ( 'NONE',  ( 0.4174706225611763410, 0.9086904199442095154, 0.000000000000000000 ) ) ;
#53854 = CARTESIAN_POINT ( 'NONE',  ( 178.0663898851194062, 286.0990649869549998, 12.90514440047635780 ) ) ;
#53855 = CARTESIAN_POINT ( 'NONE',  ( 156.4379917615520696, 279.8315861724353226, -5.297762579854731868 ) ) ;
#53856 = CARTESIAN_POINT ( 'NONE',  ( 9.022134044517839513, 26.18502408145590010, 5.678558825948276656 ) ) ;
#53857 = ORIENTED_EDGE ( 'NONE', *, *, #47887, .F. ) ;
#53858 = CARTESIAN_POINT ( 'NONE',  ( 206.6530282164287939, 272.7134509216173228, 9.408948237097369827 ) ) ;
#53859 = DIRECTION ( 'NONE',  ( 0.000000000000000000, 0.000000000000000000, 1.000000000000000000 ) ) ;
#53860 = CARTESIAN_POINT ( 'NONE',  ( 157.3661765229227285, 258.0807821998820373, -18.27254492731150748 ) ) ;
#53861 = AXIS2_PLACEMENT_3D ( 'NONE', #66827, #34925, #74465 ) ;
#53862 = CARTESIAN_POINT ( 'NONE',  ( 71.61987371496262256, 72.44464069648769566, 0.9664813023029465988 ) ) ;
#53863 = CARTESIAN_POINT ( 'NONE',  ( 40.08283240419611815, 56.57374221892477095, 177.5919119679930134 ) ) ;
#53864 = CARTESIAN_POINT ( 'NONE',  ( 191.5040086904573684, 295.9693678529874887, 12.56124033758404934 ) ) ;
#53865 = PLANE ( 'NONE',  #67159 ) ;
#53866 = CARTESIAN_POINT ( 'NONE',  ( 207.7625791259561652, 270.7916523727319031, -1.015623356719550063 ) ) ;
#53867 = CARTESIAN_POINT ( 'NONE',  ( 201.0356089830534643, 282.4431064412383989, -18.18835788025466371 ) ) ;
#53868 = ORIENTED_EDGE ( 'NONE', *, *, #16470, .F. ) ;
#53869 = CARTESIAN_POINT ( 'NONE',  ( 190.9414684426061797, 280.9540955606099715, 16.64794557087773796 ) ) ;
#53870 = CARTESIAN_POINT ( 'NONE',  ( 192.6361035247282985, 294.0892689374524593, 14.43747539422717630 ) ) ;
#53871 = EDGE_LOOP ( 'NONE', ( #96380, #65887, #333, #47912 ) ) ;
#53872 = CARTESIAN_POINT ( 'NONE',  ( 148.9232972370683399, 272.7042780851529642, 12.27045554427055940 ) ) ;
#53873 = DIRECTION ( 'NONE',  ( -0.1857746241280658905, 0.9825923819316307872, 0.000000000000000000 ) ) ;
#53874 = CARTESIAN_POINT ( 'NONE',  ( 190.7684124627589313, 298.2021613433544758, 8.215386510820527732 ) ) ;
#53875 = ORIENTED_EDGE ( 'NONE', *, *, #29235, .F. ) ;
#53876 = CARTESIAN_POINT ( 'NONE',  ( 183.8274263638271577, 281.3324037098167310, 17.41033114534894111 ) ) ;
#53877 = CARTESIAN_POINT ( 'NONE',  ( 185.0921216717482025, 263.1328331163757639, -12.61684766275084790 ) ) ;
#53878 = CIRCLE ( 'NONE', #8570, 17.82106496071138224 ) ;
#53879 = CARTESIAN_POINT ( 'NONE',  ( 197.0313051377892748, 289.3787641501790517, -17.15509075150697882 ) ) ;
#53880 = CARTESIAN_POINT ( 'NONE',  ( 74.89047242489884582, 53.29799059985631260, -16.52631573936391618 ) ) ;
#53881 = EDGE_CURVE ( 'NONE', #24841, #83865, #23177, .T. ) ;
#53882 = CARTESIAN_POINT ( 'NONE',  ( 69.44224152808193651, 62.71418222078327176, 13.79865581567335298 ) ) ;
#53883 = ORIENTED_EDGE ( 'NONE', *, *, #83623, .F. ) ;
#53884 = CARTESIAN_POINT ( 'NONE',  ( 104.9102572999672276, 237.5024278399160949, 9.188101187500095079 ) ) ;
#53885 = CARTESIAN_POINT ( 'NONE',  ( 203.1954647288614240, 278.7021265524792852, 16.53270523508054879 ) ) ;
#53886 = CARTESIAN_POINT ( 'NONE',  ( 150.8757650385446993, 269.3225046528533539, 14.31332712971473953 ) ) ;
#53887 = CARTESIAN_POINT ( 'NONE',  ( 81.25434452997238566, 42.43560832920070425, -7.602236268904982275 ) ) ;
#53888 = B_SPLINE_SURFACE_WITH_KNOTS ( 'NONE', 3, 1, ( 
 ( #10840, #19462 ),
 ( #50813, #81762 ),
 ( #12336, #33643 ),
 ( #56915, #43201 ),
 ( #4737, #35621 ),
 ( #41716, #45201 ),
 ( #75623, #5226 ),
 ( #29516, #21906 ),
 ( #99426, #6714 ),
 ( #76140, #29030 ),
 ( #90870, #82275 ),
 ( #20945, #91850 ),
 ( #44693, #12848 ),
 ( #68504, #44200 ),
 ( #76613, #30003 ),
 ( #14804, #97934 ),
 ( #52307, #28509 ),
 ( #83245, #13811 ),
 ( #51828, #37105 ),
 ( #22899, #38083 ),
 ( #92349, #36104 ),
 ( #37593, #7199 ),
 ( #99923, #67009 ),
 ( #59390, #90366 ),
 ( #29401, #20315 ),
 ( #36989, #91725 ),
 ( #74529, #5108 ),
 ( #45574, #45089 ),
 ( #90753, #22290 ),
 ( #97328, #28392 ),
 ( #60270, #76502 ),
 ( #83131, #91226 ),
 ( #51714, #35987 ),
 ( #67899, #13219 ) ),
 .UNSPECIFIED., .T., .F., .F.,
 ( 4, 2, 2, 2, 2, 2, 2, 2, 2, 2, 2, 2, 2, 2, 2, 2, 4 ),
 ( 2, 2 ),
 ( 0.000000000000000000, 0.06250000000000000000, 0.1250000000000000000, 0.1875000000000000000, 0.2500000000000000000, 0.3125000000000000000, 0.3750000000000000000, 0.4375000000000000000, 0.5000000000000000000, 0.5625000000000000000, 0.6250000000000000000, 0.6875000000000000000, 0.7500000000000000000, 0.8125000000000000000, 0.8750000000000000000, 0.9375000000000000000, 1.000000000000000000 ),
 ( 0.000000000000000000, 1.000000000000000000 ),
 .UNSPECIFIED. ) ;
#53889 = VERTEX_POINT ( 'NONE', #38879 ) ;
#53890 = ORIENTED_EDGE ( 'NONE', *, *, #56292, .T. ) ;
#53891 = ORIENTED_EDGE ( 'NONE', *, *, #22660, .T. ) ;
#53892 = CARTESIAN_POINT ( 'NONE',  ( 73.93846185904290280, 63.82218318657452727, 14.12196739231004905 ) ) ;
#53893 = ORIENTED_EDGE ( 'NONE', *, *, #38220, .F. ) ;
#53894 = CARTESIAN_POINT ( 'NONE',  ( 70.00673748363735172, 70.63212956676815679, 3.539627672355045274 ) ) ;
#53895 = CARTESIAN_POINT ( 'NONE',  ( 87.90004739103230236, 45.00901072816739656, 6.408389154966706691 ) ) ;
#53896 = VERTEX_POINT ( 'NONE', #91135 ) ;
#53897 = CARTESIAN_POINT ( 'NONE',  ( 163.7595992360150490, 247.0070492265414828, -6.976205010573520049 ) ) ;
#53898 = CARTESIAN_POINT ( 'NONE',  ( 83.02255207477764998, 48.37928522878374338, 12.76191819685389817 ) ) ;
#53899 = B_SPLINE_CURVE_WITH_KNOTS ( 'NONE', 3,
 ( #85317, #77695, #37173, #14384, #15862, #22475, #61463, #21974, #98995, #6778, #92412, #46246, #177, #7265, #22961, #77170 ),
 .UNSPECIFIED., .F., .F.,
 ( 4, 1, 2, 2, 2, 1, 2, 2, 4 ),
 ( 0.000000000000000000, 0.1249999999999957812, 0.1874999999999948097, 0.2499999999999938383, 0.4999999999999990008, 0.6250000000000004441, 0.6875000000000009992, 0.7500000000000015543, 1.000000000000000000 ),
 .UNSPECIFIED. ) ;
#53901 = EDGE_CURVE ( 'NONE', #93491, #68256, #6987, .T. ) ;
#53900 = CARTESIAN_POINT ( 'NONE',  ( 169.0161032148113236, 281.7934031441919842, 11.67333235455804363 ) ) ;
#53902 = LINE ( 'NONE', #7318, #48499 ) ;
#53903 = CARTESIAN_POINT ( 'NONE',  ( 69.14012651450867963, 68.42618068722562441, -7.476854798959941206 ) ) ;
#53904 = ORIENTED_EDGE ( 'NONE', *, *, #59673, .F. ) ;
#53905 = CARTESIAN_POINT ( 'NONE',  ( 74.66924941948499850, 57.12397588965591666, -16.51158835550184989 ) ) ;
#53906 = CARTESIAN_POINT ( 'NONE',  ( 17.58072690530697813, 12.01110640527291373, 2.839279412974134775 ) ) ;
#53907 = CARTESIAN_POINT ( 'NONE',  ( 44.44844410339183582, 68.22168590943847732, -10.00000000000000000 ) ) ;
#53908 = LINE ( 'NONE', #69622, #9523 ) ;
#53909 = ORIENTED_EDGE ( 'NONE', *, *, #91401, .T. ) ;
#53910 = CARTESIAN_POINT ( 'NONE',  ( 202.8499463704053198, 279.3005819042728604, 17.04674939340617001 ) ) ;
#53911 = CARTESIAN_POINT ( 'NONE',  ( 159.3586121662929713, 254.6297824347537642, -15.50090345830412630 ) ) ;
#53912 = CARTESIAN_POINT ( 'NONE',  ( -22.42236680055709641, 157.8615022471902591, 0.000000000000000000 ) ) ;
#53913 = CARTESIAN_POINT ( 'NONE',  ( 183.8210692855788864, 257.9504670327482927, 6.873620218444065344 ) ) ;
#53914 = CARTESIAN_POINT ( 'NONE',  ( 200.4592688079413847, 283.4413569069752725, 18.39277739746426832 ) ) ;
#53915 = CARTESIAN_POINT ( 'NONE',  ( 157.9042112748594775, 281.1459165152564310, 1.688126963922599755 ) ) ;
#53916 = VERTEX_POINT ( 'NONE', #29308 ) ;
#53917 = CARTESIAN_POINT ( 'NONE',  ( 155.5408495238017395, 261.2423413027869969, -17.06121474717059527 ) ) ;
#53918 = CARTESIAN_POINT ( 'NONE',  ( 74.51634471081780475, 62.42820743237073344, -14.86162480667644736 ) ) ;
#53919 = CARTESIAN_POINT ( 'NONE',  ( 84.99999999999997158, 27.49999999999999645, -59.99999999999999289 ) ) ;
#53920 = CARTESIAN_POINT ( 'NONE',  ( -2.233149578380279721, 169.5177522451418781, -10.00000000000009592 ) ) ;
#53921 = CARTESIAN_POINT ( 'NONE',  ( 192.8989532340791300, 266.9009477387879201, -11.33294346249175000 ) ) ;
#53922 = CARTESIAN_POINT ( 'NONE',  ( 166.7681478528634216, 248.8687067081767452, 8.283836764471310232 ) ) ;
#53923 = CARTESIAN_POINT ( 'NONE',  ( 73.02433024948126672, 69.66517378990661769, 9.714162469163332148 ) ) ;
#53924 = CARTESIAN_POINT ( 'NONE',  ( 72.70196728203136161, 70.94362825444909504, 7.654249537423017280 ) ) ;
#53926 = CARTESIAN_POINT ( 'NONE',  ( 87.97782240006738164, 43.76496563450897526, 2.369043524150738822 ) ) ;
#53925 = CARTESIAN_POINT ( 'NONE',  ( 11.59636713795893925, 171.3768266524160140, 9.188101187500098632 ) ) ;
#53927 = AXIS2_PLACEMENT_3D ( 'NONE', #64219, #19146, #72350 ) ;
#53928 = CARTESIAN_POINT ( 'NONE',  ( 27.21171415029068186, 176.5177522451417929, 5.000000000000051514 ) ) ;
#53929 = ORIENTED_EDGE ( 'NONE', *, *, #80108, .T. ) ;
#53930 = B_SPLINE_CURVE_WITH_KNOTS ( 'NONE', 3,
 ( #44266, #5287, #97033, #28076 ),
 .UNSPECIFIED., .F., .F.,
 ( 4, 4 ),
 ( 0.01837538304589518209, 0.02737905013630983694 ),
 .UNSPECIFIED. ) ;
#53931 = ORIENTED_EDGE ( 'NONE', *, *, #33889, .F. ) ;
#53932 = CARTESIAN_POINT ( 'NONE',  ( 165.4781454232152953, 246.0304399151612245, -2.837517270351797016 ) ) ;
#53933 = CARTESIAN_POINT ( 'NONE',  ( 199.1041333440138317, 265.1832257255362038, 0.2027868546939186056 ) ) ;
#53934 = EDGE_CURVE ( 'NONE', #37554, #312, #82484, .T. ) ;
#53935 = DIRECTION ( 'NONE',  ( -0.8660254037844387076, -0.4999999999999998890, -0.000000000000000000 ) ) ;
#53936 = FACE_OUTER_BOUND ( 'NONE', #78021, .T. ) ;
#53937 = CARTESIAN_POINT ( 'NONE',  ( 162.4213055719747274, 249.3250418481068778, -10.93467306481309187 ) ) ;
#53938 = CARTESIAN_POINT ( 'NONE',  ( -19.65312891409030271, 93.06504152958497400, -10.00000000000000888 ) ) ;
#53939 = CARTESIAN_POINT ( 'NONE',  ( 149.6775418821061123, 277.3372939425368031, 3.097505863387055580 ) ) ;
#53940 = B_SPLINE_CURVE_WITH_KNOTS ( 'NONE', 3,
 ( #5824, #66130, #96582, #74260 ),
 .UNSPECIFIED., .F., .F.,
 ( 4, 4 ),
 ( 0.009217897952540354822, 0.01511262126107456444 ),
 .UNSPECIFIED. ) ;
#53941 = CARTESIAN_POINT ( 'NONE',  ( 12.00188267627663308, 186.9244531367911293, -4.594050593750046652 ) ) ;
#53942 = VECTOR ( 'NONE', #38785, 1000.000000000000000 ) ;
#53943 = CARTESIAN_POINT ( 'NONE',  ( 117.4951228184160783, 229.4548013555409796, -4.594050593750042211 ) ) ;
#53944 = CARTESIAN_POINT ( 'NONE',  ( 178.9323954259722314, 291.8122831636629826, -6.158156483446289187 ) ) ;
#53945 = CARTESIAN_POINT ( 'NONE',  ( 195.8821561183051188, 275.1718881706996171, 15.74945206926084040 ) ) ;
#53946 = DIRECTION ( 'NONE',  ( 0.000000000000000000, -0.6788029332000725669, -0.7343204871709475556 ) ) ;
#53947 = EDGE_CURVE ( 'NONE', #15950, #73688, #54354, .T. ) ;
#53948 = CIRCLE ( 'NONE', #24817, 10.00000000000001066 ) ;
#53949 = CARTESIAN_POINT ( 'NONE',  ( 175.8908519962235459, 273.1107590772576827, -17.81327592954072259 ) ) ;
#53950 = CARTESIAN_POINT ( 'NONE',  ( -5.778093977583854013, 155.2202760586659451, -5.415160957724236172E-17 ) ) ;
#53951 = CARTESIAN_POINT ( 'NONE',  ( 195.7617614321055157, 291.5776783508526364, 16.33009124109666033 ) ) ;
#53952 = CARTESIAN_POINT ( 'NONE',  ( 155.6518451030846961, 261.0500913200531841, 17.91778754207898317 ) ) ;
#53953 = CARTESIAN_POINT ( 'NONE',  ( 161.1061647010182583, 251.6029326557136585, -13.56144933775657613 ) ) ;
#53954 = CARTESIAN_POINT ( 'NONE',  ( 190.1170242653768128, 284.8971620602226267, 17.14187718570638097 ) ) ;
#53955 = CARTESIAN_POINT ( 'NONE',  ( 71.25780773284164127, 62.14891183765285376, 14.64422194484298423 ) ) ;
#53956 = CARTESIAN_POINT ( 'NONE',  ( 171.5938502359046822, 279.8409701536578496, 13.97011670356616975 ) ) ;
#53957 = CARTESIAN_POINT ( 'NONE',  ( 192.5511529533421822, 265.2447470188456009, 7.887563979430734840 ) ) ;
#53958 = CARTESIAN_POINT ( 'NONE',  ( 70.39480543937862933, 70.64432371323627535, 4.229459436019878282 ) ) ;
#53959 = CARTESIAN_POINT ( 'NONE',  ( 190.3691966041315311, 300.9178746160123410, 0.1783449565851275009 ) ) ;
#53960 = CARTESIAN_POINT ( 'NONE',  ( 150.5917955345242376, 274.2788540000528315, 10.61926890178174965 ) ) ;
#53961 = VERTEX_POINT ( 'NONE', #68287 ) ;
#53962 = CARTESIAN_POINT ( 'NONE',  ( 75.08718269694753644, 62.23679730563473811, 15.49738829792160821 ) ) ;
#53963 = CARTESIAN_POINT ( 'NONE',  ( 184.3681170320605247, 268.9686055817056172, 16.19769924168502229 ) ) ;
#53964 = CARTESIAN_POINT ( 'NONE',  ( 100.7430306879021202, 216.7202760586659736, -5.415160957724236172E-17 ) ) ;
#53965 = CARTESIAN_POINT ( 'NONE',  ( 15.07467606819624173, 24.10171378149917842, 9.188101187500008038 ) ) ;
#53966 = CARTESIAN_POINT ( 'NONE',  ( 191.5544531425776427, 298.8649500714207647, 8.366689293739112188 ) ) ;
#53967 = FACE_OUTER_BOUND ( 'NONE', #50914, .T. ) ;
#53969 = CARTESIAN_POINT ( 'NONE',  ( 193.3110229662232484, 278.0645543825088453, 16.34055514812991916 ) ) ;
#53968 = CARTESIAN_POINT ( 'NONE',  ( 66.06006929221051394, 68.60032979153189103, 1.840660791566505861 ) ) ;
#53970 = CARTESIAN_POINT ( 'NONE',  ( 196.3454718165693862, 290.5666623080560385, 17.52957579560619905 ) ) ;
#53971 = CARTESIAN_POINT ( 'NONE',  ( 198.6363782946250183, 286.5986958926748116, -18.50260615857378355 ) ) ;
#53972 = CARTESIAN_POINT ( 'NONE',  ( -16.97593537095525917, 172.5530062829863027, 9.296355089585912665E-16 ) ) ;
#53973 = CARTESIAN_POINT ( 'NONE',  ( 86.26382137438996267, 220.6115022471902591, 10.00000000000009592 ) ) ;
#53974 = CARTESIAN_POINT ( 'NONE',  ( 131.5677753063155251, 236.7677522451417929, -5.000000000000041744 ) ) ;
#53975 = CARTESIAN_POINT ( 'NONE',  ( 66.51358226907667870, 69.48844138931383441, 1.167001339294358120 ) ) ;
#53976 = EDGE_LOOP ( 'NONE', ( #1714, #13968, #89421, #33380 ) ) ;
#53977 = CARTESIAN_POINT ( 'NONE',  ( 27.11724708220625857, 33.84336893147757763, -7.433330006724137462 ) ) ;
#53978 = CARTESIAN_POINT ( 'NONE',  ( 163.2942584940569191, 258.1478583562382028, 16.77787020301746779 ) ) ;
#53979 = CARTESIAN_POINT ( 'NONE',  ( 196.7852062865125902, 267.4955962336644006, 9.737905958038332699 ) ) ;
#53980 = CARTESIAN_POINT ( 'NONE',  ( 197.0313051377892748, 289.3787641501790517, -17.15509075150697882 ) ) ;
#53981 = ORIENTED_EDGE ( 'NONE', *, *, #42302, .T. ) ;
#53982 = DIRECTION ( 'NONE',  ( 0.9834470158338940449, 0.1811959355156967932, 0.000000000000000000 ) ) ;
#53983 = CARTESIAN_POINT ( 'NONE',  ( 78.91121342772640901, 49.10958624234372394, 14.40725116606144240 ) ) ;
#53984 = DIRECTION ( 'NONE',  ( 0.9979227057047517224, -0.06442261589618512863, 0.000000000000000000 ) ) ;
#53985 = CARTESIAN_POINT ( 'NONE',  ( 169.8457105410257668, 251.1523016893514750, -8.510778188974899905 ) ) ;
#53986 = CARTESIAN_POINT ( 'NONE',  ( 75.20389695419315501, 52.88180760346909892, -15.99093876381489032 ) ) ;
#53987 = DIRECTION ( 'NONE',  ( 0.8660254037844393737, 0.4999999999999986677, 0.000000000000000000 ) ) ;
#53988 = ORIENTED_EDGE ( 'NONE', *, *, #93756, .T. ) ;
#53989 = CARTESIAN_POINT ( 'NONE',  ( 188.9081020563885716, 279.7620193737561181, 16.69253326113207336 ) ) ;
#53990 = CARTESIAN_POINT ( 'NONE',  ( 30.86762485498029207, 38.79752408145593989, -5.678558825948271327 ) ) ;
#53991 = EDGE_LOOP ( 'NONE', ( #3176, #41858, #61958, #87676 ) ) ;
#53992 = CARTESIAN_POINT ( 'NONE',  ( -22.42236680055709641, 157.8615022471902591, 0.000000000000000000 ) ) ;
#53993 = DIRECTION ( 'NONE',  ( -0.8660254037844387076, -0.4999999999999998890, -0.000000000000000000 ) ) ;
#53994 = ORIENTED_EDGE ( 'NONE', *, *, #29323, .F. ) ;
#53995 = CARTESIAN_POINT ( 'NONE',  ( 86.31423836152910667, 46.99325454369051869, -10.02800889789844163 ) ) ;
#53996 = CARTESIAN_POINT ( 'NONE',  ( 158.8995732337010054, 255.8553380628405591, 16.02046230101960589 ) ) ;
#53997 = CARTESIAN_POINT ( 'NONE',  ( 190.8429499865819707, 278.0757709512191695, -17.64141544901220371 ) ) ;
#53998 = CARTESIAN_POINT ( 'NONE',  ( 153.6416917630915862, 264.5317790359255810, -18.09859318578890708 ) ) ;
#53999 = CARTESIAN_POINT ( 'NONE',  ( 182.6098810326567445, 277.4798346879709925, 17.79761443238625418 ) ) ;
#54000 = ADVANCED_FACE ( 'NONE', ( #37872 ), #68782, .F. ) ;
#54001 = DIRECTION ( 'NONE',  ( -0.8660254037844379305, -0.5000000000000014433, -0.000000000000000000 ) ) ;
#54002 = CARTESIAN_POINT ( 'NONE',  ( 81.40599722213572420, 56.18777044664494014, -16.43392898140639602 ) ) ;
#54003 = EDGE_CURVE ( 'NONE', #80416, #33600, #83536, .T. ) ;
#54004 = LINE ( 'NONE', #63503, #56236 ) ;
#54006 = ORIENTED_EDGE ( 'NONE', *, *, #10932, .F. ) ;
#54005 =( BOUNDED_CURVE ( )  B_SPLINE_CURVE ( 2, ( #13846, #73668, #58921, #50349, #90899, #51858, #82307, #21449, #12878 ),
 .UNSPECIFIED., .F., .T. ) 
 B_SPLINE_CURVE_WITH_KNOTS ( ( 3, 2, 2, 2, 3 ),
 ( 0.2298387096774193450, 0.2311827956989247201, 0.2338709677419354704, 0.2365591397849462485, 0.2379032258064516236 ),
 .UNSPECIFIED. ) 
 CURVE ( )  GEOMETRIC_REPRESENTATION_ITEM ( )  RATIONAL_B_SPLINE_CURVE ( ( 0.9330127018922194093, 0.9330127018922194093, 1.000000000000000000, 0.8660254037844387076, 1.000000000000000000, 0.8660254037844387076, 1.000000000000000000, 0.9330127018922194093, 0.9330127018922194093 ) ) 
 REPRESENTATION_ITEM ( '' )  );
#54007 = CARTESIAN_POINT ( 'NONE',  ( 207.1609884636329184, 269.8336379652346295, -0.06011041530970540059 ) ) ;
#54008 = EDGE_LOOP ( 'NONE', ( #56621, #49044, #21530, #97449 ) ) ;
#54009 = ORIENTED_EDGE ( 'NONE', *, *, #97551, .F. ) ;
#54010 = CARTESIAN_POINT ( 'NONE',  ( 169.9943822607803838, 269.4584602086645191, 17.68792189269073489 ) ) ;
#54011 = ORIENTED_EDGE ( 'NONE', *, *, #79736, .F. ) ;
#54013 = DIRECTION ( 'NONE',  ( 0.7278481391575631898, -0.6857383512134002101, 0.000000000000000000 ) ) ;
#54012 = DIRECTION ( 'NONE',  ( -0.8660254037844387076, -0.4999999999999998890, -0.000000000000000000 ) ) ;
#54014 = CARTESIAN_POINT ( 'NONE',  ( 197.4972225514353852, 278.9538932286835689, 17.08281588120735606 ) ) ;
#54015 = CARTESIAN_POINT ( 'NONE',  ( 197.5405048943464124, 273.3027842733730495, -13.38352526854320601 ) ) ;
#54016 = CARTESIAN_POINT ( 'NONE',  ( 21.22187778180244422, 61.35672868576827454, 59.99999999999999289 ) ) ;
#54017 = CARTESIAN_POINT ( 'NONE',  ( 192.6946760137320780, 261.4813915186712165, 3.932628284434791966E-12 ) ) ;
#54019 = EDGE_CURVE ( 'NONE', #49232, #93683, #84043, .T. ) ;
#54018 = CARTESIAN_POINT ( 'NONE',  ( 170.1908625819879148, 250.5941916552922351, -5.502416923392919657 ) ) ;
#54020 = CARTESIAN_POINT ( 'NONE',  ( -22.42236680055709641, 157.8615022471902591, 0.000000000000000000 ) ) ;
#54021 = AXIS2_PLACEMENT_3D ( 'NONE', #39785, #33220, #70716 ) ;
#54022 = CARTESIAN_POINT ( 'NONE',  ( 178.5299698652597726, 254.5949104052269263, 5.887118732947904221 ) ) ;
#54023 = CARTESIAN_POINT ( 'NONE',  ( 113.7873647845227225, 230.3768266524160140, -9.188101187500091527 ) ) ;
#54024 = CARTESIAN_POINT ( 'NONE',  ( 70.40687273385728417, 61.02326734534213415, -14.91946605292216610 ) ) ;
#54025 = CARTESIAN_POINT ( 'NONE',  ( 41.82943821127123840, 26.01110640527295814, 2.839279412974134775 ) ) ;
#54026 = CARTESIAN_POINT ( 'NONE',  ( 179.7478462366760539, 290.5198049800060858, -9.475730908087831139 ) ) ;
#54027 = ORIENTED_EDGE ( 'NONE', *, *, #57179, .T. ) ;
#54028 = ORIENTED_EDGE ( 'NONE', *, *, #53520, .F. ) ;
#54029 = CARTESIAN_POINT ( 'NONE',  ( 74.17344901341724039, 68.45477986254626046, -11.63824756869785659 ) ) ;
#54030 = CARTESIAN_POINT ( 'NONE',  ( 74.63372018211819636, 63.10719506861975248, -14.60809168671694636 ) ) ;
#54031 = CARTESIAN_POINT ( 'NONE',  ( 29.12701137275935181, 44.61184105132205957, 10.00000000000000000 ) ) ;
#54032 = CARTESIAN_POINT ( 'NONE',  ( 192.5715242950574009, 297.1033311604131200, 11.04771845794762619 ) ) ;
#54033 = CARTESIAN_POINT ( 'NONE',  ( 73.13649863228465620, 65.99558131849060771, 12.57961139238893189 ) ) ;
#54034 = CARTESIAN_POINT ( 'NONE',  ( 200.8665851640556070, 282.7358642834317948, -16.69422397739980823 ) ) ;
#54035 = CARTESIAN_POINT ( 'NONE',  ( 88.29250555182709093, 233.3297689869268936, -2.679491924311252493 ) ) ;
#54036 = EDGE_CURVE ( 'NONE', #19964, #57005, #47971, .T. ) ;
#54037 = ORIENTED_EDGE ( 'NONE', *, *, #36453, .F. ) ;
#54038 = CARTESIAN_POINT ( 'NONE',  ( 148.1128072303691283, 274.1080879557827643, 10.32046898584627925 ) ) ;
#54039 = ORIENTED_EDGE ( 'NONE', *, *, #84658, .T. ) ;
#54040 = CARTESIAN_POINT ( 'NONE',  ( 194.3442947553755005, 294.0328026529847421, -15.97648891113594871 ) ) ;
#54041 = ORIENTED_EDGE ( 'NONE', *, *, #79193, .T. ) ;
#54042 = CARTESIAN_POINT ( 'NONE',  ( 191.8700694318469289, 267.7572204393412107, -12.41388222293339894 ) ) ;
#54043 = CARTESIAN_POINT ( 'NONE',  ( 159.8863521765906341, 279.1613695579630416, 10.84044400854919843 ) ) ;
#54044 = CARTESIAN_POINT ( 'NONE',  ( 195.5930400684863741, 265.3186233137946033, 4.406227592133483029 ) ) ;
#54045 = LINE ( 'NONE', #83016, #68813 ) ;
#54046 = CARTESIAN_POINT ( 'NONE',  ( 69.34600056039464278, 71.16434039272530754, -0.2959734442564417867 ) ) ;
#54048 = CARTESIAN_POINT ( 'NONE',  ( 69.99185448575823898, 62.80507302648442902, -13.35615040175713375 ) ) ;
#54047 = CARTESIAN_POINT ( 'NONE',  ( 184.3838639634485617, 288.5488729356416115, -13.88906064327808387 ) ) ;
#54049 = CARTESIAN_POINT ( 'NONE',  ( 152.9251141908703175, 265.7729277985770864, -16.20110192949203309 ) ) ;
#54050 = VERTEX_POINT ( 'NONE', #49483 ) ;
#54051 = CARTESIAN_POINT ( 'NONE',  ( 190.9498149295421570, 299.9122141765958531, -5.138500224925297566 ) ) ;
#54052 = CARTESIAN_POINT ( 'NONE',  ( -19.65312891409030271, 93.06504152958497400, -10.00000000000000888 ) ) ;
#54053 = EDGE_CURVE ( 'NONE', #33736, #79982, #34999, .T. ) ;
#54054 = CARTESIAN_POINT ( 'NONE',  ( 186.8270895101041447, 262.8347829455524334, -9.018193060954537543 ) ) ;
#54055 = CARTESIAN_POINT ( 'NONE',  ( 182.2991478702006134, 275.2734891516705034, -17.80812521087705846 ) ) ;
#54056 = CARTESIAN_POINT ( 'NONE',  ( -71.07364842061384991, 47.42355933771584375, -10.00000000000000000 ) ) ;
#54057 = EDGE_CURVE ( 'NONE', #35085, #86588, #64188, .T. ) ;
#54058 = CARTESIAN_POINT ( 'NONE',  ( 189.0215474952646559, 269.9904085317868976, -14.04715979591349040 ) ) ;
#54059 = CARTESIAN_POINT ( 'NONE',  ( 188.1045636728014472, 299.4598449876921791, -3.709602300402848218 ) ) ;
#54060 = CARTESIAN_POINT ( 'NONE',  ( 83.25709734292261999, 43.34571608306740842, 7.235311536896932516 ) ) ;
#54061 = CARTESIAN_POINT ( 'NONE',  ( -19.65312891409030271, 93.06504152958497400, 177.5919119679930134 ) ) ;
#54062 = EDGE_CURVE ( 'NONE', #55615, #19698, #79438, .T. ) ;
#54063 = CARTESIAN_POINT ( 'NONE',  ( 155.4216552449402684, 261.4487918497463284, 18.51722274565528892 ) ) ;
#54064 = CARTESIAN_POINT ( 'NONE',  ( 70.39887500514583962, 61.01293241302482784, -14.92214395283775730 ) ) ;
#54065 = CARTESIAN_POINT ( 'NONE',  ( 82.75425455800102270, 53.83811729049745054, -15.80404254388376550 ) ) ;
#54066 = CARTESIAN_POINT ( 'NONE',  ( 71.86588871287597158, 221.4869531367911293, 4.594050593750046652 ) ) ;
#54067 = CARTESIAN_POINT ( 'NONE',  ( 73.98570270871888965, 68.92876820612470112, -11.10152750440662750 ) ) ;
#54068 = DIRECTION ( 'NONE',  ( -0.5280678506503699854, -0.8492021815265776707, 0.000000000000000000 ) ) ;
#54069 = CARTESIAN_POINT ( 'NONE',  ( 154.9528145190857344, 262.2608478075840708, -17.26679351315302213 ) ) ;
#54070 = ADVANCED_FACE ( 'NONE', ( #10493 ), #47482, .T. ) ;
#54071 = CARTESIAN_POINT ( 'NONE',  ( 161.8807657183444064, 250.2612843381103573, -13.52770735624900311 ) ) ;
#54072 = DIRECTION ( 'NONE',  ( -0.8660254037844387076, -0.4999999999999998890, -0.000000000000000000 ) ) ;
#54073 = CARTESIAN_POINT ( 'NONE',  ( 43.35468487962021555, 120.5828561944265687, -10.00000000000000000 ) ) ;
#54075 = CARTESIAN_POINT ( 'NONE',  ( 76.60151444110638863, 51.30487137736207615, 16.06220798441930953 ) ) ;
#54074 = CARTESIAN_POINT ( 'NONE',  ( 73.71953624722927145, 69.45002187000606853, -9.858408069665332008 ) ) ;
#54076 = EDGE_CURVE ( 'NONE', #25397, #75682, #35870, .T. ) ;
#54077 = CARTESIAN_POINT ( 'NONE',  ( 49.32130651720206771, 81.12656353050643077, 10.00000000000000000 ) ) ;
#54078 = EDGE_CURVE ( 'NONE', #79909, #95521, #16586, .T. ) ;
#54079 = CARTESIAN_POINT ( 'NONE',  ( 167.1283625793575425, 250.6242252090678448, -8.897399544333461918 ) ) ;
#54080 = CARTESIAN_POINT ( 'NONE',  ( 204.8617891913918925, 275.8159679214818425, -13.46007153234462450 ) ) ;
#54081 = CARTESIAN_POINT ( 'NONE',  ( 196.3720681610792553, 290.5205960880691691, 16.18360420724715354 ) ) ;
#54082 = CARTESIAN_POINT ( 'NONE',  ( 147.6095992045671323, 244.4824982072973967, 3.021315404115420679E-15 ) ) ;
#54083 = VECTOR ( 'NONE', #37379, 1000.000000000000114 ) ;
#54084 = CARTESIAN_POINT ( 'NONE',  ( 51.75829523846228852, 194.5643266524159856, -9.188101187500093303 ) ) ;
#54085 = DIRECTION ( 'NONE',  ( -0.000000000000000000, 1.000000000000000000, -0.000000000000000000 ) ) ;
#54086 = CARTESIAN_POINT ( 'NONE',  ( 87.92795318006373861, 43.94156286934877897, 0.4729106731310683265 ) ) ;
#54087 = CARTESIAN_POINT ( 'NONE',  ( 147.8819534105757043, 274.5079385007862811, -9.338341377131436971 ) ) ;
#54088 = CARTESIAN_POINT ( 'NONE',  ( -10.37017993122368154, 171.4865022471902876, 10.00000000000009237 ) ) ;
#54089 = FACE_OUTER_BOUND ( 'NONE', #37742, .T. ) ;
#54090 = CARTESIAN_POINT ( 'NONE',  ( 196.8298363030699250, 269.8487463528495596, -10.82627680366021750 ) ) ;
#54091 = CARTESIAN_POINT ( 'NONE',  ( 21.92109465949963720, 30.84336893147756697, -7.433330006724137462 ) ) ;
#54092 = CARTESIAN_POINT ( 'NONE',  ( 151.0426280674448378, 269.0334894088936153, -15.84467774422408581 ) ) ;
#54093 = CARTESIAN_POINT ( 'NONE',  ( 197.0184425104562820, 289.4010428742387262, -16.90752553128928426 ) ) ;
#54094 = CARTESIAN_POINT ( 'NONE',  ( 10.59179830548347745, 18.06628583063839599, -9.188101187500006262 ) ) ;
#54095 = CARTESIAN_POINT ( 'NONE',  ( 62.93552237999645627, 197.9548013555410080, -4.594050593750042211 ) ) ;
#54096 = CARTESIAN_POINT ( 'NONE',  ( 77.33081447068806824, 63.24619402228064047, 15.57729104808880294 ) ) ;
#54097 = CARTESIAN_POINT ( 'NONE',  ( 202.9490938173916561, 279.1288534886517709, -16.56031645010252973 ) ) ;
#54098 = CARTESIAN_POINT ( 'NONE',  ( 197.9598023461055902, 287.7705598106892921, 18.23120408239484291 ) ) ;
#54099 = CARTESIAN_POINT ( 'NONE',  ( 73.78463575287290155, 65.88767259777996799, 12.89433537800410434 ) ) ;
#54100 = CARTESIAN_POINT ( 'NONE',  ( 149.5435553735961491, 275.3446937576266578, 7.453328770706503015 ) ) ;
#54101 = CARTESIAN_POINT ( 'NONE',  ( -72.30469571560091424, 48.86078274006646183, -10.00000000000000000 ) ) ;
#54102 = CARTESIAN_POINT ( 'NONE',  ( 87.74379322371484591, 45.04902437494477851, -6.671288900681476619 ) ) ;
#54103 = CARTESIAN_POINT ( 'NONE',  ( 106.5432495796755603, 238.9865022471903160, 10.00000000000009237 ) ) ;
#54104 = CARTESIAN_POINT ( 'NONE',  ( 11.60290295393121696, 189.0530062829863027, -4.648177544792955347E-16 ) ) ;
#54105 = CARTESIAN_POINT ( 'NONE',  ( 165.0532575723395041, 244.7663672603923715, -2.144843157699870773 ) ) ;
#54106 = ORIENTED_EDGE ( 'NONE', *, *, #63979, .T. ) ;
#54107 = CARTESIAN_POINT ( 'NONE',  ( -66.76220315631053381, 40.93860057710854505, 10.00000000000000000 ) ) ;
#54108 = CARTESIAN_POINT ( 'NONE',  ( 82.55952364350828532, 54.17540112820317688, 15.56538284540774697 ) ) ;
#54109 = VERTEX_POINT ( 'NONE', #1900 ) ;
#54110 = CARTESIAN_POINT ( 'NONE',  ( 159.4491226731523454, 254.4730136382542582, -15.39140229921534520 ) ) ;
#54111 = CARTESIAN_POINT ( 'NONE',  ( 189.7589793277493868, 278.3644573459904450, -16.50316607585832784 ) ) ;
#54112 = CARTESIAN_POINT ( 'NONE',  ( 70.90260330370475117, 68.90363874238359188, -8.343585586704856283 ) ) ;
#54113 = VERTEX_POINT ( 'NONE', #33287 ) ;
#54114 = ORIENTED_EDGE ( 'NONE', *, *, #7018, .T. ) ;
#54115 = CARTESIAN_POINT ( 'NONE',  ( 66.23755376128818284, 69.21869211729334381, -2.080742945835972968 ) ) ;
#54116 = CARTESIAN_POINT ( 'NONE',  ( 194.2900850603946310, 294.1266965989547657, -15.88613936555681505 ) ) ;
#54117 = DIRECTION ( 'NONE',  ( -0.8718556560469457040, -0.4897629171537489778, 0.000000000000000000 ) ) ;
#54118 = VERTEX_POINT ( 'NONE', #8494 ) ;
#54119 = CARTESIAN_POINT ( 'NONE',  ( 25.58005199048888656, 32.95586893147756768, 7.433330006724141015 ) ) ;
#54120 = DIRECTION ( 'NONE',  ( 0.000000000000000000, 0.000000000000000000, 1.000000000000000000 ) ) ;
#54121 = FACE_OUTER_BOUND ( 'NONE', #40171, .T. ) ;
#54122 = VERTEX_POINT ( 'NONE', #95137 ) ;
#54123 = CARTESIAN_POINT ( 'NONE',  ( 81.97896201599648691, 58.73259127988954731, -0.1545084971874724766 ) ) ;
#54124 = B_SPLINE_CURVE_WITH_KNOTS ( 'NONE', 3,
 ( #41289, #33726, #50895, #28099, #89463, #58970, #90455, #58003, #21024, #19539, #65600, #12928, #89942, #96550, #35704, #51908, #27120, #88985, #43787, #28592, #67091, #81354 ),
 .UNSPECIFIED., .F., .F.,
 ( 4, 2, 2, 2, 2, 2, 2, 2, 2, 2, 4 ),
 ( 0.003530854327582292826, 0.003674460630036895971, 0.003818066932491499116, 0.003961673234946102261, 0.004105279537400705406, 0.004392492142309911696, 0.004679704747219117986, 0.005254129957037643323, 0.005828555166856168659, 0.006977405586493288722, 0.008126256006130408785 ),
 .UNSPECIFIED. ) ;
#54125 = CARTESIAN_POINT ( 'NONE',  ( 189.6666044902458168, 284.7049877867155487, 17.41007887138588117 ) ) ;
#54126 = ORIENTED_EDGE ( 'NONE', *, *, #17228, .F. ) ;
#54127 = CARTESIAN_POINT ( 'NONE',  ( 174.7537062242112995, 286.2005298146486894, 10.60273640048973398 ) ) ;
#54129 = CARTESIAN_POINT ( 'NONE',  ( 68.10110334728497605, 66.09131973784090519, -10.53698601666638979 ) ) ;
#54128 = CARTESIAN_POINT ( 'NONE',  ( 67.80942915694498652, 65.50210952888220106, 10.23305949600108633 ) ) ;
#54130 = CARTESIAN_POINT ( 'NONE',  ( 208.3829315663354862, 269.7171704273955015, -1.768817828503133072 ) ) ;
#54131 = CARTESIAN_POINT ( 'NONE',  ( 163.8040269124969939, 246.9300982336122559, 6.025552750865228013 ) ) ;
#54132 = CARTESIAN_POINT ( 'NONE',  ( 187.7470681246648780, 294.2386427693206201, -10.89872421713186590 ) ) ;
#54133 = CARTESIAN_POINT ( 'NONE',  ( 164.3306481956919924, 265.7257225416949495, -17.70433004990753645 ) ) ;
#54135 = EDGE_CURVE ( 'NONE', #68457, #10970, #25703, .T. ) ;
#54134 = CARTESIAN_POINT ( 'NONE',  ( 140.4172988551291894, 258.0024278399160949, -9.188101187500093303 ) ) ;
#54136 = CARTESIAN_POINT ( 'NONE',  ( 159.8591301300080261, 254.2983864834555447, -15.29415641145932803 ) ) ;
#54137 = CARTESIAN_POINT ( 'NONE',  ( 178.8348794910443758, 257.7124399359195195, 10.03872504014272771 ) ) ;
#54138 = CARTESIAN_POINT ( 'NONE',  ( 76.54827242179186442, 208.8768266524160140, 9.188101187500098632 ) ) ;
#54139 = ORIENTED_EDGE ( 'NONE', *, *, #36778, .T. ) ;
#54140 = CARTESIAN_POINT ( 'NONE',  ( 191.1489696025915919, 299.5672681643093256, 8.892130899335590755 ) ) ;
#54141 = DIRECTION ( 'NONE',  ( 0.000000000000000000, 0.000000000000000000, 1.000000000000000000 ) ) ;
#54142 = VERTEX_POINT ( 'NONE', #2920 ) ;
#54143 = CARTESIAN_POINT ( 'NONE',  ( 185.2824853868734181, 297.7695098558858149, 4.231266468330407093 ) ) ;
#54144 = ORIENTED_EDGE ( 'NONE', *, *, #88067, .F. ) ;
#54145 = CARTESIAN_POINT ( 'NONE',  ( 66.53750495837353185, 67.82509315316526965, 6.869996715873302406 ) ) ;
#54146 = CARTESIAN_POINT ( 'NONE',  ( 34.57290638322662346, 20.36477965099641452, 1.583844403245330712 ) ) ;
#54147 = EDGE_CURVE ( 'NONE', #27723, #40468, #70573, .T. ) ;
#54148 = B_SPLINE_CURVE_WITH_KNOTS ( 'NONE', 3,
 ( #39630, #23948, #54848, #79206, #24457, #1167, #16358, #8758, #32041, #33567, #40137, #64461, #32561, #2174, #55339, #40642, #71077, #2676, #55826, #9780, #71577, #94396, #86315, #94893, #33056, #86820, #87343, #63459, #17875, #87831, #48772, #80203, #79705, #10267, #49266, #41137, #10771, #85829, #57346, #88320, #20363, #42145, #51235, #18875, #12773, #51759 ),
 .UNSPECIFIED., .F., .F.,
 ( 4, 2, 2, 2, 2, 2, 2, 2, 2, 2, 2, 2, 2, 2, 2, 2, 2, 2, 2, 2, 2, 2, 4 ),
 ( 0.0004825194710001968449, 0.001489721961729743209, 0.001993323207094548077, 0.002119223518435738723, 0.002245123829776929369, 0.002371024141118120016, 0.002496924452459310662, 0.002748725075141691954, 0.003000525697824073246, 0.003504126943188788125, 0.004511329433918270793, 0.005518531924647753460, 0.006022133170012418900, 0.006273933792694715190, 0.006525734415377010614, 0.006588684571047504455, 0.006651634726717998297, 0.006714584882388492139, 0.006777535038058985981, 0.007029335660740964817, 0.007532936906104987541, 0.008036538151469010266, 0.008540139396833033858 ),
 .UNSPECIFIED. ) ;
#54149 = CARTESIAN_POINT ( 'NONE',  ( 86.27154027830852101, 42.80277227827716757, -2.586754297940185854 ) ) ;
#54150 = DIRECTION ( 'NONE',  ( 0.4999999999999998890, -0.8660254037844385966, 0.000000000000000000 ) ) ;
#54151 = CARTESIAN_POINT ( 'NONE',  ( 78.64512151719945621, 48.80906647027654088, -14.34982556509240403 ) ) ;
#54152 = CARTESIAN_POINT ( 'NONE',  ( 70.37793518914109825, 63.81744015580922991, 12.87794577580022981 ) ) ;
#54153 = EDGE_CURVE ( 'NONE', #39418, #83741, #45544, .T. ) ;
#54154 = CARTESIAN_POINT ( 'NONE',  ( 81.79837788435251866, 218.0333772461660544, 9.188101187500095079 ) ) ;
#54155 = ORIENTED_EDGE ( 'NONE', *, *, #51770, .T. ) ;
#54156 = VECTOR ( 'NONE', #7201, 1000.000000000000000 ) ;
#54157 = VERTEX_POINT ( 'NONE', #88055 ) ;
#54158 = CARTESIAN_POINT ( 'NONE',  ( 161.3512397267719791, 251.1784502594418598, -12.94313244495258530 ) ) ;
#54159 = ORIENTED_EDGE ( 'NONE', *, *, #44208, .T. ) ;
#54160 = CARTESIAN_POINT ( 'NONE',  ( 83.76771450586321066, 41.67386438877598209, 0.3050775560854859791 ) ) ;
#54161 = VECTOR ( 'NONE', #95315, 1000.000000000000114 ) ;
#54162 = CARTESIAN_POINT ( 'NONE',  ( 184.3861787086252662, 275.3536848780280479, 16.37667645762307700 ) ) ;
#54163 = CARTESIAN_POINT ( 'NONE',  ( 207.1609884636329184, 269.8336379652346295, -0.06011041530970540059 ) ) ;
#54164 = CARTESIAN_POINT ( 'NONE',  ( 207.3562937958418217, 270.9032348272035051, -2.066387192265693340 ) ) ;
#54165 = CARTESIAN_POINT ( 'NONE',  ( 153.2593913506692616, 267.1939427739956727, -16.45456985337825984 ) ) ;
#54166 = VERTEX_POINT ( 'NONE', #18604 ) ;
#54167 = CARTESIAN_POINT ( 'NONE',  ( 158.4333560722609775, 259.8736997123415904, 17.69911652888126952 ) ) ;
#54168 = CARTESIAN_POINT ( 'NONE',  ( 184.9983038504436479, 260.1326763968729097, 6.322520505052498407 ) ) ;
#54169 = CARTESIAN_POINT ( 'NONE',  ( 28.90303340214877181, 40.18528772668521043, -1.583844403245329602 ) ) ;
#54170 = CARTESIAN_POINT ( 'NONE',  ( 200.6583719735737645, 283.0965001081523269, -17.35266956530146132 ) ) ;
#54171 = CARTESIAN_POINT ( 'NONE',  ( 72.64591869506153898, 70.77312924948247996, 7.138500078990828612 ) ) ;
#54172 = CARTESIAN_POINT ( 'NONE',  ( 73.53472180018071924, 66.80482608298828495, -12.17997313596818287 ) ) ;
#54173 = VERTEX_POINT ( 'NONE', #39364 ) ;
#54174 = CARTESIAN_POINT ( 'NONE',  ( 5.968649350820482979, 188.6868197944959320, -37.49999999999994316 ) ) ;
#54175 = EDGE_CURVE ( 'NONE', #76828, #60981, #44293, .T. ) ;
#54176 = LINE ( 'NONE', #30901, #3036 ) ;
#54177 = CARTESIAN_POINT ( 'NONE',  ( 29.55951135474875358, 176.3262482093457777, 3.021315404115420679E-15 ) ) ;
#54178 = CARTESIAN_POINT ( 'NONE',  ( 171.5399254682851051, 251.6352709114593722, 7.166479175369310894 ) ) ;
#54179 = CARTESIAN_POINT ( 'NONE',  ( 198.5359561926482570, 266.1776289375414990, 1.198487561129841339 ) ) ;
#54180 = CARTESIAN_POINT ( 'NONE',  ( 153.2819998794291791, 270.3646030198663084, 13.95166877408641248 ) ) ;
#54181 = EDGE_CURVE ( 'NONE', #86304, #74262, #99941, .T. ) ;
#54182 = ORIENTED_EDGE ( 'NONE', *, *, #28525, .T. ) ;
#54183 = EDGE_CURVE ( 'NONE', #40233, #2331, #98606, .T. ) ;
#54184 = CARTESIAN_POINT ( 'NONE',  ( -14.99731640896322027, 102.3427396610899365, 44.36017770743280408 ) ) ;
#54185 = AXIS2_PLACEMENT_3D ( 'NONE', #27834, #58711, #90684 ) ;
#54186 = EDGE_CURVE ( 'NONE', #85355, #38035, #22073, .T. ) ;
#54187 = CARTESIAN_POINT ( 'NONE',  ( 11.76667899187106059, 31.90941714274742225, -10.00000000000000000 ) ) ;
#54189 = CARTESIAN_POINT ( 'NONE',  ( 73.91518305203547357, 55.21146187366786506, 16.12241119387309496 ) ) ;
#54188 = CARTESIAN_POINT ( 'NONE',  ( 167.9211111253673323, 249.4040118433879627, 8.061254949035708606 ) ) ;
#54190 = CARTESIAN_POINT ( 'NONE',  ( 176.1762632841285381, 285.4164495326317024, -12.05309685415307186 ) ) ;
#54191 = EDGE_CURVE ( 'NONE', #78972, #54142, #77079, .T. ) ;
#54192 = CARTESIAN_POINT ( 'NONE',  ( 28.04762285228751395, 28.14441083166262203, 10.00000000000000533 ) ) ;
#54193 = CARTESIAN_POINT ( 'NONE',  ( 163.0172387208063753, 284.2669704625143368, -4.045436010492660550 ) ) ;
#54194 = CARTESIAN_POINT ( 'NONE',  ( 125.2349645446896886, 253.1115022471903160, -5.000000000000047962 ) ) ;
#54195 = PLANE ( 'NONE',  #88447 ) ;
#54196 = CARTESIAN_POINT ( 'NONE',  ( -5.399381411310668177, 161.5643266524160140, -9.188101187500093303 ) ) ;
#54197 = CARTESIAN_POINT ( 'NONE',  ( 146.7678550509543811, 269.9772791071537199, -2.458545531893916687E-15 ) ) ;
#54198 = ORIENTED_EDGE ( 'NONE', *, *, #25170, .T. ) ;
#54199 = CARTESIAN_POINT ( 'NONE',  ( 160.1603183234873313, 253.8555898246377467, -15.06084538093693936 ) ) ;
#54200 = CARTESIAN_POINT ( 'NONE',  ( 72.51946054628299976, 70.67701989327743206, -7.917356521280768611 ) ) ;
#54201 = CARTESIAN_POINT ( 'NONE',  ( 202.6051175132338926, 273.9538057854381350, -13.19822448684500849 ) ) ;
#54202 = CARTESIAN_POINT ( 'NONE',  ( -132.5954152546898683, 108.6868197944957046, -37.49999999999997868 ) ) ;
#54203 = CARTESIAN_POINT ( 'NONE',  ( 31.75860784375665702, 179.9548013555409796, -4.594050593750042211 ) ) ;
#54204 = CARTESIAN_POINT ( 'NONE',  ( 75.37843707191281339, 53.50823561223473490, 16.04097401286667335 ) ) ;
#54205 = CARTESIAN_POINT ( 'NONE',  ( 181.9103902747559687, 275.6752150453591526, -16.43134084343946455 ) ) ;
#54206 = CARTESIAN_POINT ( 'NONE',  ( 27.78891098193510345, 37.81751292744058190, -6.180339887498951690 ) ) ;
#54207 = CARTESIAN_POINT ( 'NONE',  ( 77.40556785558190711, 54.71814905221435055, 16.53596348862507881 ) ) ;
#54208 = CARTESIAN_POINT ( 'NONE',  ( 205.0994677818405023, 275.4042965269534307, -14.14519517703424789 ) ) ;
#54209 = CARTESIAN_POINT ( 'NONE',  ( 5.723458822437122784, 184.1115022471903160, -5.000000000000047962 ) ) ;
#54210 = CARTESIAN_POINT ( 'NONE',  ( 176.1640045926653499, 252.3529155287689321, -3.563159428949892682 ) ) ;
#54211 = CARTESIAN_POINT ( 'NONE',  ( 166.4153639104449383, 286.7629316800744164, -4.632910421625811459 ) ) ;
#54212 = VECTOR ( 'NONE', #99406, 999.9999999999998863 ) ;
#54213 = CARTESIAN_POINT ( 'NONE',  ( 72.76825883208245216, 219.4865022471902876, 10.00000000000009237 ) ) ;
#54214 = DIRECTION ( 'NONE',  ( 0.4972609476841349796, -0.8612812260087746585, 0.1045284632676570652 ) ) ;
#54215 = DIRECTION ( 'NONE',  ( 0.4999999999999992784, -0.8660254037844390407, 0.000000000000000000 ) ) ;
#54216 = CARTESIAN_POINT ( 'NONE',  ( 29.16053163240333745, 178.4548013555409796, -4.594050593750042211 ) ) ;
#54217 = CARTESIAN_POINT ( 'NONE',  ( 66.63481606961637738, 67.83260985918037989, 6.962306014892454264 ) ) ;
#54218 = EDGE_CURVE ( 'NONE', #79838, #5025, #21583, .T. ) ;
#54219 = CARTESIAN_POINT ( 'NONE',  ( 206.4192790749514188, 271.4707676162397547, -6.632096683787595204 ) ) ;
#54220 = CARTESIAN_POINT ( 'NONE',  ( 151.1451503555562113, 268.8559155969762742, -15.81507177720227553 ) ) ;
#54221 =( GEOMETRIC_REPRESENTATION_CONTEXT ( 3 ) GLOBAL_UNCERTAINTY_ASSIGNED_CONTEXT ( ( #1773 ) ) GLOBAL_UNIT_ASSIGNED_CONTEXT ( ( #86839, #48282, #10787 ) ) REPRESENTATION_CONTEXT ( 'NONE', 'WORKASPACE' ) );
#54222 = CARTESIAN_POINT ( 'NONE',  ( 206.9258336080761183, 272.2409381227055292, 6.776000910836894597 ) ) ;
#54223 = PLANE ( 'NONE',  #58843 ) ;
#54224 = CARTESIAN_POINT ( 'NONE',  ( 159.8766461922783719, 278.4588112948835601, -9.911155033800223890 ) ) ;
#54225 = CARTESIAN_POINT ( 'NONE',  ( 165.8866640751390094, 265.8956478032751534, 17.81115609982314751 ) ) ;
#54226 = ITEM_DEFINED_TRANSFORMATION ( 'NONE', 'NONE', #62326,  #68784 ) ;
#54227 = CARTESIAN_POINT ( 'NONE',  ( 16.80975711337266176, 31.74646525600390135, 2.839279412974139660 ) ) ;
#54228 = CARTESIAN_POINT ( 'NONE',  ( 9.459751770947381289, 21.16454794089040092, -10.00000000000000355 ) ) ;
#54229 = CARTESIAN_POINT ( 'NONE',  ( 22.87549206224920084, 39.05096577487528720, -10.00000000000000000 ) ) ;
#54230 = CARTESIAN_POINT ( 'NONE',  ( 188.4483461232879336, 269.7271065142691668, -14.07674267906546639 ) ) ;
#54231 = ORIENTED_EDGE ( 'NONE', *, *, #1627, .T. ) ;
#54232 = DIRECTION ( 'NONE',  ( -0.9628097264997621529, 0.2701803667135219689, 0.000000000000000000 ) ) ;
#54233 = CARTESIAN_POINT ( 'NONE',  ( 76.68960682072659552, 58.66400703976827202, -16.06550202522544168 ) ) ;
#54234 = CARTESIAN_POINT ( 'NONE',  ( 81.26997250612254220, 42.40853988048920087, 7.543452372214260571 ) ) ;
#54235 = CARTESIAN_POINT ( 'NONE',  ( 18.47929132879751890, 188.1427522451419350, -10.00000000000009592 ) ) ;
#54236 = CARTESIAN_POINT ( 'NONE',  ( 72.63217277574858599, 71.42405857463968744, -5.808642681096034543 ) ) ;
#54237 = CARTESIAN_POINT ( 'NONE',  ( 22.08843299157899764, 31.49103043416549852, -8.090169943749479842 ) ) ;
#54238 = CARTESIAN_POINT ( 'NONE',  ( 180.3524760431470497, 257.5751156092176188, -7.390589067125090672 ) ) ;
#54239 = ORIENTED_EDGE ( 'NONE', *, *, #30478, .F. ) ;
#54241 = CARTESIAN_POINT ( 'NONE',  ( 83.82495796739634386, 42.53198561061005734, -4.832817608612280047 ) ) ;
#54240 = CYLINDRICAL_SURFACE ( 'NONE', #21188, 10.00000000000010658 ) ;
#54242 = ORIENTED_EDGE ( 'NONE', *, *, #62695, .T. ) ;
#54243 = CARTESIAN_POINT ( 'NONE',  ( 191.0900422946452011, 299.6693332556258724, 8.872191398975367349 ) ) ;
#54244 = CARTESIAN_POINT ( 'NONE',  ( -66.76220315631053381, 40.93860057710854505, -10.00000000000000000 ) ) ;
#54245 = FACE_OUTER_BOUND ( 'NONE', #22739, .T. ) ;
#54246 = DIRECTION ( 'NONE',  ( 0.000000000000000000, 0.000000000000000000, 1.000000000000000000 ) ) ;
#54247 = ORIENTED_EDGE ( 'NONE', *, *, #79915, .F. ) ;
#54248 = CARTESIAN_POINT ( 'NONE',  ( 147.7157269441172218, 274.7958511862549926, 8.036290321896261801 ) ) ;
#54249 = EDGE_CURVE ( 'NONE', #213, #74292, #52468, .T. ) ;
#54250 = CARTESIAN_POINT ( 'NONE',  ( 196.4242782546697015, 290.4301655533025155, -16.42402868779123537 ) ) ;
#54251 = CARTESIAN_POINT ( 'NONE',  ( -19.65312891409030271, 93.06504152958497400, 10.00000000000000888 ) ) ;
#54252 = AXIS2_PLACEMENT_3D ( 'NONE', #3521, #26308, #11124 ) ;
#54253 = ORIENTED_EDGE ( 'NONE', *, *, #65131, .F. ) ;
#54254 = CARTESIAN_POINT ( 'NONE',  ( 196.0034224882197975, 291.1591091234520263, 17.53794140922627776 ) ) ;
#54255 = CARTESIAN_POINT ( 'NONE',  ( 162.1392933197202808, 266.6552078212308174, 16.85513656058302345 ) ) ;
#54256 = EDGE_LOOP ( 'NONE', ( #97916, #18407, #45667, #76254 ) ) ;
#54257 = CARTESIAN_POINT ( 'NONE',  ( 30.03287232231581072, 25.84335787977764554, 9.188101187500006262 ) ) ;
#54258 = CARTESIAN_POINT ( 'NONE',  ( 149.2511585606875428, 272.1364056148075292, 11.40684181024752242 ) ) ;
#54259 = CARTESIAN_POINT ( 'NONE',  ( 78.26456671038654633, 47.45118235465228196, -13.78252656109451380 ) ) ;
#54260 = ORIENTED_EDGE ( 'NONE', *, *, #76046, .T. ) ;
#54261 = EDGE_CURVE ( 'NONE', #36219, #13677, #100058, .T. ) ;
#54262 = CARTESIAN_POINT ( 'NONE',  ( -12.28396743053746398, 72.06898478986710188, 14.42833059486102698 ) ) ;
#54263 = DIRECTION ( 'NONE',  ( -1.000000000000000000, 0.000000000000000000, 0.000000000000000000 ) ) ;
#54264 = LINE ( 'NONE', #67493, #3054 ) ;
#54265 = AXIS2_PLACEMENT_3D ( 'NONE', #9593, #55153, #25791 ) ;
#54266 = CARTESIAN_POINT ( 'NONE',  ( 157.4655681218829670, 259.9086309006383431, -17.75190047967350893 ) ) ;
#54267 = ORIENTED_EDGE ( 'NONE', *, *, #89319, .F. ) ;
#54268 = EDGE_CURVE ( 'NONE', #32604, #48299, #32283, .T. ) ;
#54269 = ORIENTED_EDGE ( 'NONE', *, *, #9792, .F. ) ;
#54270 = CARTESIAN_POINT ( 'NONE',  ( 87.10930705799060547, 46.39120889860887331, 8.709784027055659905 ) ) ;
#54271 = CARTESIAN_POINT ( 'NONE',  ( -27.42236680055714260, 166.5217562850347406, 1.224646799147364892E-15 ) ) ;
#54272 = CARTESIAN_POINT ( 'NONE',  ( 68.64455419991973883, 221.9860189848785410, -2.679491924311252493 ) ) ;
#54273 = CARTESIAN_POINT ( 'NONE',  ( 190.2476911738421848, 301.1283281946692796, -1.360079143321618611 ) ) ;
#54274 = VERTEX_POINT ( 'NONE', #68661 ) ;
#54275 = CARTESIAN_POINT ( 'NONE',  ( 148.9230895364621574, 272.7046378331555161, 12.20434325797056019 ) ) ;
#54276 = CARTESIAN_POINT ( 'NONE',  ( 174.0620471294585059, 277.0282672862553000, -15.64145360528607043 ) ) ;
#54277 = CARTESIAN_POINT ( 'NONE',  ( 161.8882824960653579, 250.2482648971885340, -13.83574485983625557 ) ) ;
#54278 = CARTESIAN_POINT ( 'NONE',  ( 147.2567621633200474, 275.5908015054806128, -3.647191014543873955 ) ) ;
#54279 = CARTESIAN_POINT ( 'NONE',  ( 148.9266665119372703, 272.6984423298952152, 12.06339424062075061 ) ) ;
#54280 = CARTESIAN_POINT ( 'NONE',  ( 71.66380185985713069, 70.75815305948317757, 6.002177236114092373 ) ) ;
#54281 = CYLINDRICAL_SURFACE ( 'NONE', #43414, 10.00000000000010658 ) ;
#54282 = CARTESIAN_POINT ( 'NONE',  ( 67.68246526915767447, 66.80505248408825025, 8.573265321495291857 ) ) ;
#54283 = CARTESIAN_POINT ( 'NONE',  ( 154.1288763713144192, 264.1723049937594965, -16.63665840739514579 ) ) ;
#54284 = CARTESIAN_POINT ( 'NONE',  ( 77.94364930070486253, 48.08271769344008817, 14.18973355224276212 ) ) ;
#54285 = CARTESIAN_POINT ( 'NONE',  ( 111.1353355333153843, 222.7202760586659167, -5.415160957724236172E-17 ) ) ;
#54286 = ORIENTED_EDGE ( 'NONE', *, *, #94905, .T. ) ;
#54287 = CARTESIAN_POINT ( 'NONE',  ( 191.6823192895500370, 298.6434794082964572, -8.424208857102787107 ) ) ;
#54288 = CARTESIAN_POINT ( 'NONE',  ( 83.97040189252935249, 41.78422930658946655, -0.6732071361253898489 ) ) ;
#54289 = DIRECTION ( 'NONE',  ( -0.9985601716053730259, 0.05364311403570636710, 0.000000000000000000 ) ) ;
#54290 = CARTESIAN_POINT ( 'NONE',  ( 202.7676489560256528, 279.4431252073101746, -16.04062356091568020 ) ) ;
#54291 = CIRCLE ( 'NONE', #34859, 17.82106496071138224 ) ;
#54292 = FACE_OUTER_BOUND ( 'NONE', #26905, .T. ) ;
#54293 = CARTESIAN_POINT ( 'NONE',  ( 83.79462322672901564, 52.11981396736175043, -14.61821130395286872 ) ) ;
#54294 = CARTESIAN_POINT ( 'NONE',  ( 68.48117590867735771, 65.15193093079356856, -10.98008167408246649 ) ) ;
#54295 = ORIENTED_EDGE ( 'NONE', *, *, #79693, .F. ) ;
#54296 = CARTESIAN_POINT ( 'NONE',  ( 208.0421103033489771, 270.3074901711881353, -2.473242163239977476 ) ) ;
#54297 =( BOUNDED_CURVE ( )  B_SPLINE_CURVE ( 2, ( #71328, #17100, #79456, #95158, #87080, #77922, #78428, #38897, #23688, #70300, #54583, #15590, #63207 ),
 .UNSPECIFIED., .F., .T. ) 
 B_SPLINE_CURVE_WITH_KNOTS ( ( 3, 2, 2, 2, 2, 2, 3 ),
 ( 0.03750000000000000555, 0.04000000000000000083, 0.04499999999999999833, 0.05000000000000000278, 0.05500000000000000028, 0.05999999999999999778, 0.06250000000000000000 ),
 .UNSPECIFIED. ) 
 CURVE ( )  GEOMETRIC_REPRESENTATION_ITEM ( )  RATIONAL_B_SPLINE_CURVE ( ( 0.9755282581475768211, 0.9755282581475768211, 1.000000000000000000, 0.9510565162951535312, 1.000000000000000000, 0.9510565162951535312, 1.000000000000000000, 0.9510565162951535312, 1.000000000000000000, 0.9510565162951535312, 1.000000000000000000, 0.9755282581475768211, 0.9755282581475768211 ) ) 
 REPRESENTATION_ITEM ( '' )  );
#54298 = EDGE_CURVE ( 'NONE', #83576, #27174, #30168, .T. ) ;
#54299 = CARTESIAN_POINT ( 'NONE',  ( 72.19696248574352637, 71.49523067816146238, 5.038491395661391259 ) ) ;
#54300 = CARTESIAN_POINT ( 'NONE',  ( 48.42933654300939139, 198.7677522451418781, 10.00000000000009592 ) ) ;
#54301 = CARTESIAN_POINT ( 'NONE',  ( 133.7059490715647883, 241.8768266524159856, 9.188101187500096856 ) ) ;
#54302 = CARTESIAN_POINT ( 'NONE',  ( 198.4344074287054696, 286.9485196940960918, -17.83642855442570152 ) ) ;
#54303 = CARTESIAN_POINT ( 'NONE',  ( 114.3892930691446850, 248.3967562850347122, -4.648177544792955347E-16 ) ) ;
#54304 = CARTESIAN_POINT ( 'NONE',  ( 187.9181207603909911, 281.6813620558751836, -17.66056584057218259 ) ) ;
#54305 = LINE ( 'NONE', #62925, #43352 ) ;
#54306 = CARTESIAN_POINT ( 'NONE',  ( 44.34243207491050498, 208.6589784336661637, -6.496448406907675876E-16 ) ) ;
#54307 = CARTESIAN_POINT ( 'NONE',  ( 85.72318707267324100, 48.45004672980276439, -11.74706068800014513 ) ) ;
#54308 = VERTEX_POINT ( 'NONE', #84408 ) ;
#54309 = CARTESIAN_POINT ( 'NONE',  ( 70.84135035934207281, 62.78096507068896415, 13.67032215614803370 ) ) ;
#54310 = CARTESIAN_POINT ( 'NONE',  ( -89.11465314115665137, 93.37593066204027537, 37.50000000000002132 ) ) ;
#54311 = EDGE_CURVE ( 'NONE', #17408, #36668, #15400, .T. ) ;
#54312 = CARTESIAN_POINT ( 'NONE',  ( 164.2897805489690768, 249.8104079013010335, 11.36607573508163505 ) ) ;
#54313 = CARTESIAN_POINT ( 'NONE',  ( 190.1813752874636805, 301.2431906792259042, -4.710625539811892359 ) ) ;
#54314 = DIRECTION ( 'NONE',  ( -0.9890802632347809320, 0.1473778574936430164, 0.000000000000000000 ) ) ;
#54315 = CYLINDRICAL_SURFACE ( 'NONE', #55952, 10.00000000000010658 ) ;
#54316 = CARTESIAN_POINT ( 'NONE',  ( 180.6243441928988887, 262.2958008669023116, 12.30780204317005655 ) ) ;
#54317 = CARTESIAN_POINT ( 'NONE',  ( 104.3601438707543565, 244.3927522451419350, 2.944929066748280225E-16 ) ) ;
#54318 = CARTESIAN_POINT ( 'NONE',  ( 41.10245927640360009, 127.8322459559854138, 10.00000000000000000 ) ) ;
#54319 = ORIENTED_EDGE ( 'NONE', *, *, #37222, .T. ) ;
#54320 = CARTESIAN_POINT ( 'NONE',  ( 148.0389988358468827, 274.2359278451201590, 7.783622668412842671 ) ) ;
#54321 = CARTESIAN_POINT ( 'NONE',  ( 20.76088743254790003, 12.39040679176982529, 1.333680081654574804E-15 ) ) ;
#54322 = ADVANCED_FACE ( 'NONE', ( #15960 ), #63064, .T. ) ;
#54323 = AXIS2_PLACEMENT_3D ( 'NONE', #83274, #51338, #13842 ) ;
#54324 = CARTESIAN_POINT ( 'NONE',  ( 36.84650709099022947, 182.8923013555409796, 4.594050593750050204 ) ) ;
#54325 = CARTESIAN_POINT ( 'NONE',  ( 15.99984526765731907, 17.43677371833800649, -10.00000000000000355 ) ) ;
#54326 = CARTESIAN_POINT ( 'NONE',  ( 8.106622824862185439, 30.17147933776455204, -10.00000000000000000 ) ) ;
#54327 = LINE ( 'NONE', #71072, #12539 ) ;
#54328 = LINE ( 'NONE', #29080, #70151 ) ;
#54330 = CARTESIAN_POINT ( 'NONE',  ( 68.04987750350953490, 222.3464784336661637, 1.353441290958777327E-15 ) ) ;
#54329 = CARTESIAN_POINT ( 'NONE',  ( 176.1992339320817962, 287.1978759562800860, 10.54343790665076419 ) ) ;
#54331 = CARTESIAN_POINT ( 'NONE',  ( 200.4116241316243645, 283.5238799070667142, 18.37703770054986663 ) ) ;
#54332 = CARTESIAN_POINT ( 'NONE',  ( 73.10143609569175283, 57.30672121060334945, 15.89779801809523896 ) ) ;
#54333 = CARTESIAN_POINT ( 'NONE',  ( 71.48351530877290827, 69.86829643969724657, 8.246344044914554416 ) ) ;
#54334 = CARTESIAN_POINT ( 'NONE',  ( 13.59582392308679033, 19.80066082961420548, 10.00000000000000533 ) ) ;
#54335 = ORIENTED_EDGE ( 'NONE', *, *, #39709, .F. ) ;
#54336 = VECTOR ( 'NONE', #4453, 1000.000000000000000 ) ;
#54337 = CARTESIAN_POINT ( 'NONE',  ( 36.46736065678477701, 181.8615022471902023, 5.000000000000051514 ) ) ;
#54338 = CARTESIAN_POINT ( 'NONE',  ( 208.2555382576270233, 269.9378221106229034, 3.215405476967123199 ) ) ;
#54339 = CARTESIAN_POINT ( 'NONE',  ( 140.7960114214023974, 264.3464784336661637, 1.353441290958777327E-15 ) ) ;
#54340 = CARTESIAN_POINT ( 'NONE',  ( 28.71100085020356474, 39.68290643055189548, 3.479690158560446702E-15 ) ) ;
#54342 = ADVANCED_FACE ( 'NONE', ( #94503 ), #17464, .T. ) ;
#54341 = CARTESIAN_POINT ( 'NONE',  ( 167.2515702596184042, 262.0622343731731689, -17.21809106051008342 ) ) ;
#54343 = CARTESIAN_POINT ( 'NONE',  ( 187.5228883593873093, 261.4347505834685990, 6.388304628836355192 ) ) ;
#54344 = CARTESIAN_POINT ( 'NONE',  ( 164.7462163020046262, 245.2981783406326599, 1.451255823150352064 ) ) ;
#54345 = PLANE ( 'NONE',  #75997 ) ;
#54346 = CARTESIAN_POINT ( 'NONE',  ( 66.48422118441082773, 68.76807364154430502, 2.317831917423630816 ) ) ;
#54347 = ORIENTED_EDGE ( 'NONE', *, *, #63440, .F. ) ;
#54348 = CARTESIAN_POINT ( 'NONE',  ( 191.0900422946452011, 299.6693332556258724, 8.872191398975367349 ) ) ;
#54349 = CARTESIAN_POINT ( 'NONE',  ( 177.8882589859629491, 286.4065610622367331, 13.19283280512425094 ) ) ;
#54350 = FACE_BOUND ( 'NONE', #67617, .T. ) ;
#54351 = CARTESIAN_POINT ( 'NONE',  ( 10.26584248093601737, 14.43085787977761036, -9.188101187500008038 ) ) ;
#54352 = ORIENTED_EDGE ( 'NONE', *, *, #55697, .F. ) ;
#54353 = CARTESIAN_POINT ( 'NONE',  ( 160.0613190107378614, 253.4126584773486854, 14.75620464716950764 ) ) ;
#54354 = CIRCLE ( 'NONE', #23552, 0.1418229129681522482 ) ;
#54355 = B_SPLINE_CURVE_WITH_KNOTS ( 'NONE', 3,
 ( #72276, #2881, #33778, #64663 ),
 .UNSPECIFIED., .F., .F.,
 ( 4, 4 ),
 ( 0.009427079270958907756, 0.01489411771146553591 ),
 .UNSPECIFIED. ) ;
#54356 = DIRECTION ( 'NONE',  ( 0.000000000000000000, 0.000000000000000000, 1.000000000000000000 ) ) ;
#54357 = CARTESIAN_POINT ( 'NONE',  ( 192.0712386031329686, 297.9698513971258649, 12.12276320360788873 ) ) ;
#54358 = CARTESIAN_POINT ( 'NONE',  ( 163.3740049908953438, 249.6749180501957710, -11.76522313559978627 ) ) ;
#54359 = CARTESIAN_POINT ( 'NONE',  ( 73.76584831522595209, 68.38082682530665579, 10.99424229391075514 ) ) ;
#54360 = CARTESIAN_POINT ( 'NONE',  ( 208.3586375946586315, 269.7592488206576604, -1.970210487958146128 ) ) ;
#54361 = CARTESIAN_POINT ( 'NONE',  ( 153.1627746953036535, 265.3612877299463548, -17.72069958822647351 ) ) ;
#54362 = ORIENTED_EDGE ( 'NONE', *, *, #69340, .T. ) ;
#54363 = ORIENTED_EDGE ( 'NONE', *, *, #55295, .F. ) ;
#54364 = CARTESIAN_POINT ( 'NONE',  ( 190.4780531826553442, 281.5641646806880658, 17.56433427958257454 ) ) ;
#54365 = CARTESIAN_POINT ( 'NONE',  ( 183.1207986101861138, 294.8225010653632694, -8.165837621905515320 ) ) ;
#54366 = ORIENTED_EDGE ( 'NONE', *, *, #91254, .F. ) ;
#54367 = CARTESIAN_POINT ( 'NONE',  ( -66.21217304253431735, 40.79406095866392690, -10.00000000000000000 ) ) ;
#54368 = CARTESIAN_POINT ( 'NONE',  ( 87.27117856089937220, 44.98890866680353895, -6.231534082530021834 ) ) ;
#54369 = ORIENTED_EDGE ( 'NONE', *, *, #32286, .F. ) ;
#54370 = FACE_OUTER_BOUND ( 'NONE', #40140, .T. ) ;
#54371 = CARTESIAN_POINT ( 'NONE',  ( 79.31081143133005185, 59.61002059306027689, -16.52811874246032886 ) ) ;
#54372 = CARTESIAN_POINT ( 'NONE',  ( 204.8762144138505903, 275.7909827032724479, 14.60855957933206817 ) ) ;
#54373 = CARTESIAN_POINT ( 'NONE',  ( 70.01938104327861367, 62.76876530535373178, 13.38671266457854792 ) ) ;
#54374 = EDGE_LOOP ( 'NONE', ( #74415, #25415, #90236, #80230 ) ) ;
#54375 = CARTESIAN_POINT ( 'NONE',  ( 161.3644539559160478, 251.1555625431813894, 12.97746593258196413 ) ) ;
#54376 = CARTESIAN_POINT ( 'NONE',  ( 191.5281967176683509, 298.9104275333885994, 7.715154960566919407 ) ) ;
#54377 = DIRECTION ( 'NONE',  ( 0.8261602328994307465, -0.5634352399127678934, 0.000000000000000000 ) ) ;
#54378 = EDGE_LOOP ( 'NONE', ( #53665, #70991 ) ) ;
#54379 = ORIENTED_EDGE ( 'NONE', *, *, #80546, .T. ) ;
#54380 = EDGE_CURVE ( 'NONE', #49338, #25811, #31807, .T. ) ;
#54381 = VERTEX_POINT ( 'NONE', #37578 ) ;
#54382 = CARTESIAN_POINT ( 'NONE',  ( 160.1863252117574064, 268.8609356850063250, -17.02858764381097956 ) ) ;
#54383 = ORIENTED_EDGE ( 'NONE', *, *, #19669, .T. ) ;
#54384 = EDGE_CURVE ( 'NONE', #27648, #36202, #91523, .T. ) ;
#54385 = CARTESIAN_POINT ( 'NONE',  ( 70.12552833076205161, 70.75604929650035047, 3.338328085167999060 ) ) ;
#54386 = ORIENTED_EDGE ( 'NONE', *, *, #43324, .F. ) ;
#54387 = CARTESIAN_POINT ( 'NONE',  ( 207.8725590214046406, 270.6011616060040410, 1.988011721677743093 ) ) ;
#54388 = CARTESIAN_POINT ( 'NONE',  ( 81.62619352285597074, 44.78313946143589419, 10.36055733450182537 ) ) ;
#54389 = EDGE_CURVE ( 'NONE', #42173, #99081, #22395, .T. ) ;
#54390 = LINE ( 'NONE', #7827, #43062 ) ;
#54391 = EDGE_CURVE ( 'NONE', #16766, #34323, #92825, .T. ) ;
#54392 = CARTESIAN_POINT ( 'NONE',  ( 194.1972774922283236, 294.2874440223457100, -15.09915398317898649 ) ) ;
#54393 = CARTESIAN_POINT ( 'NONE',  ( 82.87565756262195293, 53.54239330764043814, -15.33588095777717086 ) ) ;
#54394 = DIRECTION ( 'NONE',  ( 0.000000000000000000, 0.000000000000000000, 1.000000000000000000 ) ) ;
#54395 = ORIENTED_EDGE ( 'NONE', *, *, #17475, .F. ) ;
#54396 = CARTESIAN_POINT ( 'NONE',  ( 167.0957737472305666, 246.8272050136007749, 1.963998143010642128 ) ) ;
#54397 = CARTESIAN_POINT ( 'NONE',  ( 11.20403028766721398, 24.65586893147754921, -7.433330006724137462 ) ) ;
#54398 = VECTOR ( 'NONE', #79792, 1000.000000000000114 ) ;
#54399 = CARTESIAN_POINT ( 'NONE',  ( 163.4495156451401670, 282.8190555064526279, 8.951327301367555833 ) ) ;
#54400 = CARTESIAN_POINT ( 'NONE',  ( 80.31556117237309422, 57.81632953744806969, 16.60139635717627726 ) ) ;
#54402 = ORIENTED_EDGE ( 'NONE', *, *, #55837, .F. ) ;
#54401 = CARTESIAN_POINT ( 'NONE',  ( 115.4099260042794270, 248.9860189848785126, -2.679491924311252493 ) ) ;
#54403 = CIRCLE ( 'NONE', #34969, 14.99999999999968026 ) ;
#54404 = CARTESIAN_POINT ( 'NONE',  ( 61.92489908531692322, 199.8927522451418213, 10.00000000000009948 ) ) ;
#54405 = CARTESIAN_POINT ( 'NONE',  ( 159.2651917302844993, 254.7915913763855258, -16.53922207549818424 ) ) ;
#54406 = CARTESIAN_POINT ( 'NONE',  ( 165.6682284193261978, 246.6824036188616560, -2.565596566166696846 ) ) ;
#54407 = VECTOR ( 'NONE', #28137, 1000.000000000000000 ) ;
#54408 = CARTESIAN_POINT ( 'NONE',  ( 155.3626990048841492, 275.8588059374729369, -11.87708972044752187 ) ) ;
#54409 = CARTESIAN_POINT ( 'NONE',  ( 171.0910052398126027, 255.4451962542384535, 11.23270455455271133 ) ) ;
#54410 = CARTESIAN_POINT ( 'NONE',  ( 158.0731130136125842, 281.0592270188419093, 2.063127701874739373 ) ) ;
#54411 = ORIENTED_EDGE ( 'NONE', *, *, #15583, .F. ) ;
#54412 = CARTESIAN_POINT ( 'NONE',  ( 194.1719470998206418, 294.3313175489715263, -14.09883309033929599 ) ) ;
#54413 = CARTESIAN_POINT ( 'NONE',  ( 137.2691092145630876, 243.3927522451418497, 10.00000000000009948 ) ) ;
#54414 = DIRECTION ( 'NONE',  ( -0.9184028970038772277, -0.3956464567955659817, 0.000000000000000000 ) ) ;
#54415 = CARTESIAN_POINT ( 'NONE',  ( 4.262040950002970341, 183.2677522451419065, -5.000000000000047962 ) ) ;
#54416 = CARTESIAN_POINT ( 'NONE',  ( 93.00275509369618021, 218.3768266524159856, -9.188101187500093303 ) ) ;
#54417 = CARTESIAN_POINT ( 'NONE',  ( 196.1211713645807890, 269.6255699324162833, -11.03082859017656858 ) ) ;
#54418 = CARTESIAN_POINT ( 'NONE',  ( 30.62489312496363425, 46.16797101519271962, -10.00000000000000000 ) ) ;
#54419 = CARTESIAN_POINT ( 'NONE',  ( 170.2967212533610564, 280.7145836319469367, -13.97955410212758487 ) ) ;
#54420 = CARTESIAN_POINT ( 'NONE',  ( 8.774901663922227257, 164.3262482093457777, 3.021315404115420679E-15 ) ) ;
#54422 = DIRECTION ( 'NONE',  ( -0.8660254037844387076, -0.4999999999999998890, -0.000000000000000000 ) ) ;
#54421 = CARTESIAN_POINT ( 'NONE',  ( 1.284818304444202530, 180.7369531367911293, -4.594050593750048428 ) ) ;
#54423 = CARTESIAN_POINT ( 'NONE',  ( 161.8873598795597388, 250.2498629158519350, 13.90822209621415873 ) ) ;
#54424 = ORIENTED_EDGE ( 'NONE', *, *, #24576, .T. ) ;
#54425 = VECTOR ( 'NONE', #44368, 1000.000000000000227 ) ;
#54426 = VERTEX_POINT ( 'NONE', #54266 ) ;
#54427 = CARTESIAN_POINT ( 'NONE',  ( 42.45923888023187232, 122.5484010731363043, -10.00000000000000000 ) ) ;
#54428 = CARTESIAN_POINT ( 'NONE',  ( 197.6036480476475958, 265.0526450946206865, -2.974152093784073525 ) ) ;
#54429 = CARTESIAN_POINT ( 'NONE',  ( -71.61465314115659453, 63.06504152958490295, 203.6502102582797420 ) ) ;
#54430 = VECTOR ( 'NONE', #17602, 1000.000000000000000 ) ;
#54431 = CARTESIAN_POINT ( 'NONE',  ( 63.31414817410234264, 207.3615022471904012, 5.155647304959626021E-14 ) ) ;
#54432 = CARTESIAN_POINT ( 'NONE',  ( 185.6922465440033250, 286.5916479858942694, 15.93746842189364799 ) ) ;
#54433 = DIRECTION ( 'NONE',  ( 0.8660254037844377084, 0.5000000000000015543, -0.000000000000000000 ) ) ;
#54434 = CARTESIAN_POINT ( 'NONE',  ( 31.29809797828990270, 195.0024278399160949, -9.188101187500093303 ) ) ;
#54435 = CARTESIAN_POINT ( 'NONE',  ( 126.9399520566163773, 244.0958772461660544, -9.188101187500095079 ) ) ;
#54436 = CARTESIAN_POINT ( 'NONE',  ( 199.4166635728208234, 277.5177111250312123, 15.19222490148100846 ) ) ;
#54437 = ORIENTED_EDGE ( 'NONE', *, *, #18434, .T. ) ;
#54438 = CARTESIAN_POINT ( 'NONE',  ( 152.5568709919297987, 273.2141159824016086, -11.74195484041754156 ) ) ;
#54439 = CARTESIAN_POINT ( 'NONE',  ( 175.0472144265203838, 281.5570299394952372, -15.61366602656669400 ) ) ;
#54440 = EDGE_CURVE ( 'NONE', #21181, #99967, #15781, .T. ) ;
#54441 = CARTESIAN_POINT ( 'NONE',  ( 40.41628377845469089, 57.12529113016345406, -10.00000000000000000 ) ) ;
#54442 = CARTESIAN_POINT ( 'NONE',  ( 80.45486823626444561, 57.11063749423583147, -16.22959712110212749 ) ) ;
#54443 = CARTESIAN_POINT ( 'NONE',  ( 194.5051734451974426, 293.7541525883582381, 14.61790433731063921 ) ) ;
#54444 = CARTESIAN_POINT ( 'NONE',  ( 207.4541616930702617, 271.3258470364304458, -6.834942797545373594 ) ) ;
#54445 = CARTESIAN_POINT ( 'NONE',  ( 189.6793199455043464, 284.5195100320480606, 16.64680879193300811 ) ) ;
#54446 = CARTESIAN_POINT ( 'NONE',  ( 194.1789525331299728, 294.3191837825503967, -15.34533909744314961 ) ) ;
#54447 = CARTESIAN_POINT ( 'NONE',  ( 189.3315619462889572, 262.8718067175192914, 7.989062115483674731 ) ) ;
#54448 = CARTESIAN_POINT ( 'NONE',  ( 171.0879638105105585, 279.6763734742275460, 13.89733606482576889 ) ) ;
#54449 = DIRECTION ( 'NONE',  ( 0.4999999999999992784, -0.8660254037844390407, 0.000000000000000000 ) ) ;
#54450 = CARTESIAN_POINT ( 'NONE',  ( 68.14689968819119770, 67.57311714285278015, 7.858381336759803659 ) ) ;
#54451 = CARTESIAN_POINT ( 'NONE',  ( 190.1158090214649405, 301.3567547831981983, -1.340987185199551845 ) ) ;
#54452 = CARTESIAN_POINT ( 'NONE',  ( 30.62489312496363425, 46.16797101519271962, -10.00000000000000000 ) ) ;
#54453 = CARTESIAN_POINT ( 'NONE',  ( 152.3302930170243314, 267.2945999775473638, -15.38153796020247732 ) ) ;
#54454 = CARTESIAN_POINT ( 'NONE',  ( 81.93667712306067585, 41.32900906425540200, -5.893600489608231463 ) ) ;
#54455 = EDGE_CURVE ( 'NONE', #86378, #44968, #21893, .T. ) ;
#54456 = CARTESIAN_POINT ( 'NONE',  ( 116.3314879560220163, 225.7202760586659736, -5.415160957724236172E-17 ) ) ;
#54457 = CARTESIAN_POINT ( 'NONE',  ( 17.70402515066951565, 13.14754757982089295, -5.678558825948276656 ) ) ;
#54458 = B_SPLINE_CURVE_WITH_KNOTS ( 'NONE', 3,
 ( #50827, #66536, #90886, #59407 ),
 .UNSPECIFIED., .F., .F.,
 ( 4, 4 ),
 ( 0.01080040790777650125, 0.01647322660403158570 ),
 .UNSPECIFIED. ) ;
#54459 = CARTESIAN_POINT ( 'NONE',  ( 190.8443993347725325, 300.0947993426467519, 8.522468760355437212 ) ) ;
#54460 = DIRECTION ( 'NONE',  ( 0.5000000000000013323, -0.8660254037844378194, 0.000000000000000000 ) ) ;
#54462 = CARTESIAN_POINT ( 'NONE',  ( 195.6701525283530714, 278.3163088474954634, 17.11539662884900537 ) ) ;
#54461 = CARTESIAN_POINT ( 'NONE',  ( 8.802591199716557568, 28.58029201028040589, 1.583844403245363353 ) ) ;
#54463 = CARTESIAN_POINT ( 'NONE',  ( 191.0207652119315753, 299.7893246826858444, -8.025593426971470379 ) ) ;
#54464 = CARTESIAN_POINT ( 'NONE',  ( 191.1041736655189140, 261.3211040730838590, -4.687602006059129245 ) ) ;
#54465 = CARTESIAN_POINT ( 'NONE',  ( 149.9090183420942424, 271.7417389411527893, -11.59929054339867349 ) ) ;
#54466 = VECTOR ( 'NONE', #29379, 1000.000000000000114 ) ;
#54467 = CARTESIAN_POINT ( 'NONE',  ( 179.5344296421649233, 268.6052087499922436, -17.09315547090865905 ) ) ;
#54468 = CARTESIAN_POINT ( 'NONE',  ( 164.0651280066704771, 248.4778578725967861, 9.975266483072225299 ) ) ;
#54469 = CARTESIAN_POINT ( 'NONE',  ( 67.15292568697987008, 69.89524710907804206, 0.3341031261128851182 ) ) ;
#54470 = ORIENTED_EDGE ( 'NONE', *, *, #67320, .T. ) ;
#54471 = CARTESIAN_POINT ( 'NONE',  ( -19.16796693315586708, 34.39132293302410659, 59.99999999999999289 ) ) ;
#54472 = CARTESIAN_POINT ( 'NONE',  ( 39.80235952159635815, 84.99999999999998579, 10.00000000000000000 ) ) ;
#54473 = AXIS2_PLACEMENT_3D ( 'NONE', #21752, #6053, #29853 ) ;
#54474 = CARTESIAN_POINT ( 'NONE',  ( 81.05125564046635134, 47.50520864145833855, 13.45574471257056359 ) ) ;
#54475 = CARTESIAN_POINT ( 'NONE',  ( 149.6564118588553924, 271.4344863124460971, -11.76165597393390172 ) ) ;
#54476 = ORIENTED_EDGE ( 'NONE', *, *, #4573, .T. ) ;
#54477 = B_SPLINE_SURFACE_WITH_KNOTS ( 'NONE', 3, 1, ( 
 ( #14580, #69262 ),
 ( #45458, #53558 ),
 ( #84510, #15054 ),
 ( #24169, #10991 ),
 ( #9478, #8966 ),
 ( #88037, #63164 ),
 ( #33267, #2901 ),
 ( #40349, #72806 ),
 ( #31744, #71789 ),
 ( #48977, #62648 ),
 ( #94109, #1878 ),
 ( #17568, #95118 ),
 ( #47950, #39836 ),
 ( #41864, #93602 ),
 ( #70766, #87035 ),
 ( #33795, #79913 ),
 ( #48475, #78892 ),
 ( #64679, #24661 ),
 ( #40842, #25160 ),
 ( #25683, #95629 ),
 ( #18585, #80419 ),
 ( #56563, #56043 ),
 ( #55545, #2387 ),
 ( #79417, #9983 ),
 ( #64170, #87549 ),
 ( #18082, #55053 ),
 ( #26177, #86036 ),
 ( #10476, #32262 ),
 ( #41353, #57055 ),
 ( #49464, #72295 ),
 ( #16564, #47460 ),
 ( #78385, #1382 ),
 ( #86529, #17059 ),
 ( #71286, #32760 ) ),
 .UNSPECIFIED., .T., .F., .F.,
 ( 4, 2, 2, 2, 2, 2, 2, 2, 2, 2, 2, 2, 2, 2, 2, 2, 4 ),
 ( 2, 2 ),
 ( 0.000000000000000000, 0.06250000000000000000, 0.1250000000000000000, 0.1875000000000000000, 0.2500000000000000000, 0.3125000000000000000, 0.3750000000000000000, 0.4375000000000000000, 0.5000000000000000000, 0.5625000000000000000, 0.6250000000000000000, 0.6875000000000000000, 0.7500000000000000000, 0.8125000000000000000, 0.8750000000000000000, 0.9375000000000000000, 1.000000000000000000 ),
 ( 0.000000000000000000, 1.000000000000000000 ),
 .UNSPECIFIED. ) ;
#54478 = CARTESIAN_POINT ( 'NONE',  ( 75.75917444283010127, 65.12044684595205979, -14.46054081031674876 ) ) ;
#54479 = CARTESIAN_POINT ( 'NONE',  ( 182.9889844305354245, 264.4095531704369364, -13.10990340061844073 ) ) ;
#54480 = CARTESIAN_POINT ( 'NONE',  ( 165.3207990934748750, 285.3707166551773753, 6.626286169182803221 ) ) ;
#54481 = CARTESIAN_POINT ( 'NONE',  ( -13.19378359325312466, 163.1896272461660544, -10.00000000000009592 ) ) ;
#54482 = AXIS2_PLACEMENT_3D ( 'NONE', #75426, #21710, #52594 ) ;
#54483 = EDGE_LOOP ( 'NONE', ( #73241, #64751, #44679, #1184 ) ) ;
#54484 = CARTESIAN_POINT ( 'NONE',  ( 189.6749581198630210, 280.2046705077256092, 16.64219758661014126 ) ) ;
#54485 = VECTOR ( 'NONE', #36284, 1000.000000000000000 ) ;
#54486 = CARTESIAN_POINT ( 'NONE',  ( 37.11382629638189457, 33.37878583063844218, 9.188101187500006262 ) ) ;
#54487 = ORIENTED_EDGE ( 'NONE', *, *, #53061, .F. ) ;
#54488 = CARTESIAN_POINT ( 'NONE',  ( 176.5752601597114335, 288.5842064133888130, 11.38490813771325350 ) ) ;
#54489 = DIRECTION ( 'NONE',  ( -0.8660254037844387076, -0.4999999999999998890, -0.000000000000000000 ) ) ;
#54490 = VERTEX_POINT ( 'NONE', #83739 ) ;
#54491 = LINE ( 'NONE', #8421, #24756 ) ;
#54492 = DIRECTION ( 'NONE',  ( 0.4999999999999998335, -0.8660254037844389297, 0.000000000000000000 ) ) ;
#54493 = DIRECTION ( 'NONE',  ( -1.000000000000000000, 0.000000000000000000, 0.000000000000000000 ) ) ;
#54494 = FACE_OUTER_BOUND ( 'NONE', #48361, .T. ) ;
#54495 = CYLINDRICAL_SURFACE ( 'NONE', #38854, 16.60714546451156792 ) ;
#54496 = AXIS2_PLACEMENT_3D ( 'NONE', #12467, #43336, #35748 ) ;
#54497 = CARTESIAN_POINT ( 'NONE',  ( 80.29271997359656154, 44.85105216242119042, 11.15187779989279093 ) ) ;
#54498 = CARTESIAN_POINT ( 'NONE',  ( 84.88427240234526039, 50.06337035240281352, -13.24819347122077851 ) ) ;
#54499 = CARTESIAN_POINT ( 'NONE',  ( 81.36199125831662116, 55.41608345602817565, -16.32668456146280889 ) ) ;
#54500 = ORIENTED_EDGE ( 'NONE', *, *, #75963, .F. ) ;
#54501 = CARTESIAN_POINT ( 'NONE',  ( 165.9903072508455466, 286.3044248736204622, 5.270287258096775673 ) ) ;
#54502 = ORIENTED_EDGE ( 'NONE', *, *, #69283, .T. ) ;
#54503 = CARTESIAN_POINT ( 'NONE',  ( 81.29827136372979624, 55.78681482234479461, 16.38844377500790017 ) ) ;
#54504 = VERTEX_POINT ( 'NONE', #44677 ) ;
#54505 = CARTESIAN_POINT ( 'NONE',  ( 169.4836806320240612, 269.1565945087554041, 17.44706958315075340 ) ) ;
#54506 = VERTEX_POINT ( 'NONE', #91834 ) ;
#54507 = CARTESIAN_POINT ( 'NONE',  ( 165.4895756769140007, 275.0579021241501323, -15.80007132412031368 ) ) ;
#54508 = CARTESIAN_POINT ( 'NONE',  ( -50.41871976035449165, 31.58591985673634639, 10.00000000000000000 ) ) ;
#54509 = CARTESIAN_POINT ( 'NONE',  ( 147.2720785848982530, 275.5642726851167481, -7.209059498816540845 ) ) ;
#54510 = CARTESIAN_POINT ( 'NONE',  ( 190.0445576990143195, 301.4801656937889902, 4.140328216824785912 ) ) ;
#54511 = CARTESIAN_POINT ( 'NONE',  ( 147.2658550951450422, 275.5750520855697800, -5.215660180131691526 ) ) ;
#54512 = CARTESIAN_POINT ( 'NONE',  ( 167.8763609878610339, 248.7503499377862681, -4.961192906137089409 ) ) ;
#54513 = EDGE_CURVE ( 'NONE', #28157, #43464, #84243, .T. ) ;
#54514 = CARTESIAN_POINT ( 'NONE',  ( -50.36082798260553517, 30.16005589317048674, 177.5919119679930134 ) ) ;
#54515 = CARTESIAN_POINT ( 'NONE',  ( 178.0456222035626297, 255.4355507755199994, 5.346306856010867747 ) ) ;
#54516 = CARTESIAN_POINT ( 'NONE',  ( 121.2293367285889616, 249.9869531367911293, 4.594050593750046652 ) ) ;
#54517 = CARTESIAN_POINT ( 'NONE',  ( 70.56938734894262666, 60.79602815012135864, -14.52576355119476581 ) ) ;
#54518 = CARTESIAN_POINT ( 'NONE',  ( 160.3128597929971306, 283.6975250075342387, 2.223783518518671176 ) ) ;
#54519 = CARTESIAN_POINT ( 'NONE',  ( 180.5790958426250086, 291.5328203877501210, -9.792797898500380072 ) ) ;
#54520 = ORIENTED_EDGE ( 'NONE', *, *, #86609, .F. ) ;
#54521 = ORIENTED_EDGE ( 'NONE', *, *, #53826, .F. ) ;
#54522 = LINE ( 'NONE', #55038, #85416 ) ;
#54523 = CARTESIAN_POINT ( 'NONE',  ( 177.7757808709156109, 253.3576871789891527, 1.393605394853308699 ) ) ;
#54524 = CARTESIAN_POINT ( 'NONE',  ( 173.9708202189197550, 290.6014801153625626, -4.921738911677555173 ) ) ;
#54525 = CARTESIAN_POINT ( 'NONE',  ( 157.5710319558766344, 257.7259621817996162, 18.28704422422941533 ) ) ;
#54526 = CARTESIAN_POINT ( 'NONE',  ( 72.42579240007300712, 63.30198422945165504, 13.90833229552876738 ) ) ;
#54527 = CARTESIAN_POINT ( 'NONE',  ( 152.8651171364917900, 265.8768457450651113, -16.25664868183201861 ) ) ;
#54528 = CARTESIAN_POINT ( 'NONE',  ( 27.94679880624369162, 69.70277699303075281, 59.99999999999999289 ) ) ;
#54529 = ORIENTED_EDGE ( 'NONE', *, *, #81541, .F. ) ;
#54530 = CARTESIAN_POINT ( 'NONE',  ( 194.7295074538898803, 293.3655946874374081, 16.09945624218667959 ) ) ;
#54531 = CARTESIAN_POINT ( 'NONE',  ( 174.1271922040128572, 253.6654629759184161, -7.526141489418877839 ) ) ;
#54532 = EDGE_LOOP ( 'NONE', ( #18992, #46429, #89760, #72784 ) ) ;
#54533 = CARTESIAN_POINT ( 'NONE',  ( 194.5298665426430489, 293.7113828889860656, -16.13302716640051315 ) ) ;
#54534 = CARTESIAN_POINT ( 'NONE',  ( 65.97662824784276836, 68.66983059223240105, -0.2190663313023521186 ) ) ;
#54535 = ORIENTED_EDGE ( 'NONE', *, *, #99403, .F. ) ;
#54536 = FACE_OUTER_BOUND ( 'NONE', #94675, .T. ) ;
#54537 = CARTESIAN_POINT ( 'NONE',  ( 156.8430461297778891, 276.5937385669784021, 10.19580746110867508 ) ) ;
#54538 = CARTESIAN_POINT ( 'NONE',  ( 195.7544032369005436, 265.2869026655097855, 4.183226695583321941 ) ) ;
#54539 = CARTESIAN_POINT ( 'NONE',  ( 190.0607312434325138, 301.4521522931182176, 3.538147641957853473 ) ) ;
#54540 = AXIS2_PLACEMENT_3D ( 'NONE', #5488, #99194, #59152 ) ;
#54541 = CARTESIAN_POINT ( 'NONE',  ( 160.3733185927383715, 282.5102941377067509, 6.606729549618552078 ) ) ;
#54543 = CARTESIAN_POINT ( 'NONE',  ( 69.85780038398088720, 62.79618712063587793, -13.31498138799742570 ) ) ;
#54542 = CARTESIAN_POINT ( 'NONE',  ( 162.9302848195957267, 282.3798764647056032, -6.613031290533573525 ) ) ;
#54544 = DIRECTION ( 'NONE',  ( -0.9738769792773346312, -0.2270762630343691746, 0.000000000000000000 ) ) ;
#54545 = ORIENTED_EDGE ( 'NONE', *, *, #57496, .F. ) ;
#54546 = AXIS2_PLACEMENT_3D ( 'NONE', #30574, #69064, #44268 ) ;
#54547 = DIRECTION ( 'NONE',  ( -0.9538480676139692305, 0.3002896333693469422, 0.000000000000000000 ) ) ;
#54548 = CARTESIAN_POINT ( 'NONE',  ( 163.9055806673350162, 247.5346603069789921, -7.472254527550087566 ) ) ;
#54549 = CARTESIAN_POINT ( 'NONE',  ( 118.1240276194171770, 250.5530062829863311, -4.648177544792955347E-16 ) ) ;
#54550 = CARTESIAN_POINT ( 'NONE',  ( 24.47725860691335598, 196.4860189848785126, -2.679491924311252493 ) ) ;
#54551 = CARTESIAN_POINT ( 'NONE',  ( 188.2332414194945898, 299.2348910183464454, -3.671804926528876134 ) ) ;
#54552 = CARTESIAN_POINT ( 'NONE',  ( 192.3606619183491091, 297.4685555102766443, 10.99569063633359889 ) ) ;
#54553 = CARTESIAN_POINT ( 'NONE',  ( 50.57404612423096069, 211.5530062829863027, -4.648177544792955347E-16 ) ) ;
#54554 = CIRCLE ( 'NONE', #99852, 9.212605237762131694 ) ;
#54555 = CARTESIAN_POINT ( 'NONE',  ( 154.9683083969241011, 262.2340116239618055, 18.33261662430134109 ) ) ;
#54556 = CARTESIAN_POINT ( 'NONE',  ( 191.3843761966370209, 282.8631020262318430, -17.76976768207862278 ) ) ;
#54557 = CARTESIAN_POINT ( 'NONE',  ( 82.35285118013293015, 53.50770157854819331, -15.77620284334257938 ) ) ;
#54558 = CARTESIAN_POINT ( 'NONE',  ( 90.72909131299699936, 229.3149278399160949, -9.188101187500095079 ) ) ;
#54559 = CARTESIAN_POINT ( 'NONE',  ( 70.70420039156243774, 71.94848598797803163, 6.061257734329015641E-06 ) ) ;
#54560 = CARTESIAN_POINT ( 'NONE',  ( 193.1649355862271591, 296.0755126543221536, -12.21556774862162698 ) ) ;
#54561 = FACE_OUTER_BOUND ( 'NONE', #70033, .T. ) ;
#54562 = CARTESIAN_POINT ( 'NONE',  ( 202.7676489560256528, 279.4431252073101746, -16.04062356091568020 ) ) ;
#54563 = EDGE_CURVE ( 'NONE', #94602, #8880, #42179, .T. ) ;
#54564 = LINE ( 'NONE', #9508, #24742 ) ;
#54565 = FACE_OUTER_BOUND ( 'NONE', #58559, .T. ) ;
#54566 = VECTOR ( 'NONE', #39587, 1000.000000000000000 ) ;
#54567 = CARTESIAN_POINT ( 'NONE',  ( 78.08841283195533833, 61.93109719521473977, 15.70046319500454857 ) ) ;
#54569 = CARTESIAN_POINT ( 'NONE',  ( 75.96574207184018235, 51.41514783579079761, 15.67647344538899645 ) ) ;
#54568 = CARTESIAN_POINT ( 'NONE',  ( 73.14143739346300777, 69.59972439283021117, -9.872010100564622803 ) ) ;
#54570 = CARTESIAN_POINT ( 'NONE',  ( 207.6414258450697616, 271.0014960107308752, 6.436373232459713378 ) ) ;
#54571 = CARTESIAN_POINT ( 'NONE',  ( 166.3640306902089492, 249.9463895289820243, -9.022950769094974177 ) ) ;
#54572 = CARTESIAN_POINT ( 'NONE',  ( 164.7588300145904441, 245.2763307495621632, -4.895387527856912335 ) ) ;
#54573 = CARTESIAN_POINT ( 'NONE',  ( 157.0848929289108469, 258.5679796760466047, 17.57466231005294688 ) ) ;
#54574 = DIRECTION ( 'NONE',  ( -1.000000000000000000, 0.000000000000000000, 0.000000000000000000 ) ) ;
#54575 = EDGE_CURVE ( 'NONE', #45578, #59881, #77614, .T. ) ;
#54576 =( BOUNDED_CURVE ( )  B_SPLINE_CURVE ( 2, ( #5983, #83522, #73900, #42958, #43966, #5002, #67277, #97225, #14085 ),
 .UNSPECIFIED., .F., .T. ) 
 B_SPLINE_CURVE_WITH_KNOTS ( ( 3, 2, 2, 2, 3 ),
 ( 0.4395161290322580627, 0.4408602150537634379, 0.4435483870967741882, 0.4462365591397849385, 0.4475806451612903136 ),
 .UNSPECIFIED. ) 
 CURVE ( )  GEOMETRIC_REPRESENTATION_ITEM ( )  RATIONAL_B_SPLINE_CURVE ( ( 0.9330127018922194093, 0.9330127018922194093, 1.000000000000000000, 0.8660254037844387076, 1.000000000000000000, 0.8660254037844387076, 1.000000000000000000, 0.9330127018922194093, 0.9330127018922194093 ) ) 
 REPRESENTATION_ITEM ( '' )  );
#54577 = CARTESIAN_POINT ( 'NONE',  ( 35.81758128034870481, 200.6744531367911293, 4.594050593750047540 ) ) ;
#54578 = VECTOR ( 'NONE', #57200, 1000.000000000000114 ) ;
#54579 = EDGE_CURVE ( 'NONE', #90499, #54274, #25391, .T. ) ;
#54580 = CARTESIAN_POINT ( 'NONE',  ( 65.42534541587671981, 199.3923013555409796, 4.594050593750050204 ) ) ;
#54581 = DIRECTION ( 'NONE',  ( -1.000000000000000000, 0.000000000000000000, 0.000000000000000000 ) ) ;
#54582 = CARTESIAN_POINT ( 'NONE',  ( 88.54102397196729157, 43.89880672352619229, -0.3772737106920460159 ) ) ;
#54583 = CARTESIAN_POINT ( 'NONE',  ( 4.856824484202590497, 25.73705186507751819, -3.090169943749475845 ) ) ;
#54584 = CARTESIAN_POINT ( 'NONE',  ( -13.76211276271270556, 162.8615022471902591, -10.00000000000009592 ) ) ;
#54585 = CYLINDRICAL_SURFACE ( 'NONE', #91098, 17.82106496071139645 ) ;
#54586 = B_SPLINE_CURVE_WITH_KNOTS ( 'NONE', 3,
 ( #95987, #73642, #51313, #58419 ),
 .UNSPECIFIED., .F., .F.,
 ( 4, 4 ),
 ( 0.009149324415700987867, 0.01512556512898982457 ),
 .UNSPECIFIED. ) ;
#54587 = APPLICATION_CONTEXT ( 'automotive_design' ) ;
#54588 = CARTESIAN_POINT ( 'NONE',  ( 199.9966929353907972, 271.1012207858159400, -11.25541782042054706 ) ) ;
#54589 = CARTESIAN_POINT ( 'NONE',  ( 31.56043161122053320, 21.14754757982091249, -5.678558825948275768 ) ) ;
#54590 = CARTESIAN_POINT ( 'NONE',  ( 130.1965684169901181, 252.6427522451419065, -10.00000000000009592 ) ) ;
#54591 = CARTESIAN_POINT ( 'NONE',  ( 196.6288634187112052, 290.0758136547079289, -16.31544900032282186 ) ) ;
#54592 = CARTESIAN_POINT ( 'NONE',  ( 10.91775413003093931, 21.70171378149917985, -9.188101187500004485 ) ) ;
#54593 = CARTESIAN_POINT ( 'NONE',  ( 62.52896555438372417, 219.1589784336661637, -6.496448406907676862E-16 ) ) ;
#54594 = CARTESIAN_POINT ( 'NONE',  ( 77.31919379202844311, 63.29706486701976331, 15.55867855103717545 ) ) ;
#54595 = CARTESIAN_POINT ( 'NONE',  ( 154.9903553346911735, 262.1958252075976361, -18.39016733948542637 ) ) ;
#54596 = CARTESIAN_POINT ( 'NONE',  ( 197.9552487813401456, 287.7784468162186613, 17.26493623863614602 ) ) ;
#54597 = CARTESIAN_POINT ( 'NONE',  ( 47.97596991287763757, 210.0530062829863027, 1.101618078115930403E-13 ) ) ;
#54598 = CARTESIAN_POINT ( 'NONE',  ( 153.3379181194665080, 265.0579304206846132, 17.59725599559538978 ) ) ;
#54599 =( BOUNDED_CURVE ( )  B_SPLINE_CURVE ( 2, ( #84366, #43824, #21061, #91977, #75250, #37223, #28626, #74764, #13453 ),
 .UNSPECIFIED., .F., .T. ) 
 B_SPLINE_CURVE_WITH_KNOTS ( ( 3, 2, 2, 2, 3 ),
 ( 0.1733870967741935609, 0.1747311827956989361, 0.1774193548387096864, 0.1801075268817204367, 0.1814516129032258118 ),
 .UNSPECIFIED. ) 
 CURVE ( )  GEOMETRIC_REPRESENTATION_ITEM ( )  RATIONAL_B_SPLINE_CURVE ( ( 0.9330127018922194093, 0.9330127018922194093, 1.000000000000000000, 0.8660254037844387076, 1.000000000000000000, 0.8660254037844387076, 1.000000000000000000, 0.9330127018922194093, 0.9330127018922194093 ) ) 
 REPRESENTATION_ITEM ( '' )  );
#54600 = CARTESIAN_POINT ( 'NONE',  ( 75.25638032370783037, 56.77384408695551343, -16.10482308988691358 ) ) ;
#54601 = CARTESIAN_POINT ( 'NONE',  ( 120.5439936075240155, 233.7365022471902307, 10.00000000000009592 ) ) ;
#54602 = CARTESIAN_POINT ( 'NONE',  ( 185.9487007927320974, 279.8905167439364732, -17.76757602008028769 ) ) ;
#54603 = CARTESIAN_POINT ( 'NONE',  ( 165.0387478276132072, 244.7914988754632191, -2.473354058663827626 ) ) ;
#54604 = ORIENTED_EDGE ( 'NONE', *, *, #7786, .F. ) ;
#54605 = LINE ( 'NONE', #68819, #57065 ) ;
#54606 = CIRCLE ( 'NONE', #10987, 15.60714546451148799 ) ;
#54607 = CARTESIAN_POINT ( 'NONE',  ( 82.08557581956762306, 54.06085729471828927, 15.60977446998290574 ) ) ;
#54608 = VERTEX_POINT ( 'NONE', #9196 ) ;
#54609 = CARTESIAN_POINT ( 'NONE',  ( 159.9470087484377814, 253.6106496594791508, -16.54933891566789939 ) ) ;
#54610 = CARTESIAN_POINT ( 'NONE',  ( 190.1660438660940429, 279.2337011502113455, -16.80628667824917954 ) ) ;
#54611 = CARTESIAN_POINT ( 'NONE',  ( -22.42236680055709641, 157.8615022471902591, 0.000000000000000000 ) ) ;
#54612 = VERTEX_POINT ( 'NONE', #24396 ) ;
#54613 = CARTESIAN_POINT ( 'NONE',  ( 173.5665296885054261, 251.8413114671298558, -0.2508721732096706458 ) ) ;
#54614 = ORIENTED_EDGE ( 'NONE', *, *, #78363, .T. ) ;
#54615 = DIRECTION ( 'NONE',  ( -0.4272584830711198545, -0.9041295198387040433, 0.000000000000000000 ) ) ;
#54616 = CARTESIAN_POINT ( 'NONE',  ( 148.2352135776142177, 273.8960739431854563, -9.245976304249309052 ) ) ;
#54617 = CARTESIAN_POINT ( 'NONE',  ( 177.5865089022509551, 268.7852845103913069, 17.37969943402860906 ) ) ;
#54618 = AXIS2_PLACEMENT_3D ( 'NONE', #84164, #68403, #45107 ) ;
#54619 = ORIENTED_EDGE ( 'NONE', *, *, #41038, .T. ) ;
#54620 = AXIS2_PLACEMENT_3D ( 'NONE', #81850, #12424, #74240 ) ;
#54621 = CARTESIAN_POINT ( 'NONE',  ( 21.45803809350889324, 35.49540643055188127, 3.479690158560446702E-15 ) ) ;
#54622 = DIRECTION ( 'NONE',  ( 0.5000000000000001110, -0.8660254037844384856, -0.000000000000000000 ) ) ;
#54623 = CARTESIAN_POINT ( 'NONE',  ( 84.65437100661064562, 50.51450566574431633, -13.57843829959869808 ) ) ;
#54624 = EDGE_CURVE ( 'NONE', #81475, #34164, #72139, .T. ) ;
#54625 = ADVANCED_FACE ( 'NONE', ( #41070 ), #63891, .F. ) ;
#54626 = VERTEX_POINT ( 'NONE', #56279 ) ;
#54627 = CARTESIAN_POINT ( 'NONE',  ( 150.5780525126727980, 271.8381578737140103, 12.98431582152410968 ) ) ;
#54628 = PLANE ( 'NONE',  #49727 ) ;
#54629 = ORIENTED_EDGE ( 'NONE', *, *, #71819, .F. ) ;
#54630 = CARTESIAN_POINT ( 'NONE',  ( 171.7130254469920487, 284.7891961508439067, 10.67702735494407662 ) ) ;
#54631 = VECTOR ( 'NONE', #61184, 1000.000000000000000 ) ;
#54633 = CARTESIAN_POINT ( 'NONE',  ( 67.78035058596742601, 65.61037735967913420, -10.84149385423511802 ) ) ;
#54632 = CARTESIAN_POINT ( 'NONE',  ( 67.63975743122908568, 65.85389184688227715, 10.50638905972799719 ) ) ;
#54634 = CARTESIAN_POINT ( 'NONE',  ( 163.1369207721744772, 248.0855599626920593, -11.24692769914530110 ) ) ;
#54635 = CARTESIAN_POINT ( 'NONE',  ( 164.3330377059402849, 246.0138246616164110, 7.208046019122525294 ) ) ;
#54636 = CARTESIAN_POINT ( 'NONE',  ( 185.3933647707513330, 292.5380661828041866, -10.79500138365868978 ) ) ;
#54637 = CARTESIAN_POINT ( 'NONE',  ( 205.4029933437358295, 274.8785748323546159, -13.50815392427034922 ) ) ;
#54638 = CARTESIAN_POINT ( 'NONE',  ( 139.2268610206906203, 245.0643266524160140, 9.188101187500095079 ) ) ;
#54639 = EDGE_CURVE ( 'NONE', #76018, #53003, #41582, .T. ) ;
#54640 = LINE ( 'NONE', #47060, #42040 ) ;
#54641 = VECTOR ( 'NONE', #12804, 1000.000000000000000 ) ;
#54642 = CARTESIAN_POINT ( 'NONE',  ( 178.9917773741442204, 257.7053463395453150, 10.09848434317354737 ) ) ;
#54643 = CARTESIAN_POINT ( 'NONE',  ( 69.26781250152264136, 219.9869531367911293, 4.594050593750046652 ) ) ;
#54644 = VERTEX_POINT ( 'NONE', #72523 ) ;
#54645 = CARTESIAN_POINT ( 'NONE',  ( 151.0099717111976076, 269.0900518771037468, 15.84752309685681659 ) ) ;
#54646 = CARTESIAN_POINT ( 'NONE',  ( 180.2546767116767228, 254.3082820442907348, 0.6097036191673013139 ) ) ;
#54647 = VERTEX_POINT ( 'NONE', #64902 ) ;
#54648 = FACE_OUTER_BOUND ( 'NONE', #67765, .T. ) ;
#54649 = EDGE_LOOP ( 'NONE', ( #95058, #15543, #88491, #53507 ) ) ;
#54650 = EDGE_LOOP ( 'NONE', ( #87659, #65883, #41713, #93937, #4825 ) ) ;
#54651 = EDGE_CURVE ( 'NONE', #76712, #30963, #10794, .T. ) ;
#54652 = EDGE_CURVE ( 'NONE', #5719, #39984, #52531, .T. ) ;
#54653 = CARTESIAN_POINT ( 'NONE',  ( 66.82165646262005509, 67.51089840573428091, 6.628743624060557060 ) ) ;
#54654 = DIRECTION ( 'NONE',  ( -0.8278489937552534483, 0.5609510170580086497, 0.000000000000000000 ) ) ;
#54655 = CARTESIAN_POINT ( 'NONE',  ( -19.65312891409030271, 93.06504152958497400, -20.00000000000000355 ) ) ;
#54656 = CARTESIAN_POINT ( 'NONE',  ( 56.22356517706937495, 193.2677522451418213, -5.000000000000041744 ) ) ;
#54657 = CARTESIAN_POINT ( 'NONE',  ( 32.18695666311190706, 46.02670049433632471, 177.5919119679930134 ) ) ;
#54658 = CARTESIAN_POINT ( 'NONE',  ( 78.06346978264959091, 222.0024278399160949, -9.188101187500093303 ) ) ;
#54659 = EDGE_LOOP ( 'NONE', ( #1336, #95468, #84425, #51365 ) ) ;
#54660 = AXIS2_PLACEMENT_3D ( 'NONE', #83434, #98627, #68183 ) ;
#54661 = ORIENTED_EDGE ( 'NONE', *, *, #46768, .T. ) ;
#54662 = CARTESIAN_POINT ( 'NONE',  ( 200.3112178831040922, 283.6977886309012433, -17.53557373623702986 ) ) ;
#54663 = ORIENTED_EDGE ( 'NONE', *, *, #92662, .F. ) ;
#54664 = DIRECTION ( 'NONE',  ( 0.000000000000000000, 0.000000000000000000, 1.000000000000000000 ) ) ;
#54665 = CARTESIAN_POINT ( 'NONE',  ( 76.00688113039353766, 65.27918228371470377, -14.45284717766215721 ) ) ;
#54666 = CARTESIAN_POINT ( 'NONE',  ( 202.6051175132338926, 273.9538057854381350, -13.19822448684500849 ) ) ;
#54667 = FACE_OUTER_BOUND ( 'NONE', #93169, .T. ) ;
#54668 = DIRECTION ( 'NONE',  ( -0.000000000000000000, -0.000000000000000000, -1.000000000000000000 ) ) ;
#54669 = ORIENTED_EDGE ( 'NONE', *, *, #35728, .T. ) ;
#54670 = CARTESIAN_POINT ( 'NONE',  ( 84.97959890569808294, 43.76174631704970608, -6.205910672392634275 ) ) ;
#54671 = CARTESIAN_POINT ( 'NONE',  ( 43.23316042107100543, 25.36477965099643583, 1.583844403245330712 ) ) ;
#54672 = CARTESIAN_POINT ( 'NONE',  ( 147.7355616822484023, 275.2941310105550770, -3.966930963970487056 ) ) ;
#54673 = CARTESIAN_POINT ( 'NONE',  ( 200.6985908945154335, 283.0268388936558495, -17.74173253065502820 ) ) ;
#54674 = CARTESIAN_POINT ( 'NONE',  ( 72.54292141210436284, 70.69116050516647931, 7.176139523292191846 ) ) ;
#54675 = CARTESIAN_POINT ( 'NONE',  ( 73.11768136168076637, 66.90819131663745623, -11.89771565002191345 ) ) ;
#54676 = DIRECTION ( 'NONE',  ( 0.4999999999999998890, -0.8660254037844385966, 0.000000000000000000 ) ) ;
#54677 = CARTESIAN_POINT ( 'NONE',  ( 76.55480823776410659, 226.5530062829863027, -4.648177544792955347E-16 ) ) ;
#54678 = CARTESIAN_POINT ( 'NONE',  ( 21.31191609055701974, 193.1115022471903160, -5.000000000000047962 ) ) ;
#54679 = CIRCLE ( 'NONE', #1350, 10.00000000000001066 ) ;
#54680 = CARTESIAN_POINT ( 'NONE',  ( 187.9004646343075819, 266.2528347880879096, -12.82234703419135968 ) ) ;
#54681 = CARTESIAN_POINT ( 'NONE',  ( 83.58343668721781228, 51.99607003748921130, 15.00733587213922604 ) ) ;
#54682 = PLANE ( 'NONE',  #83428 ) ;
#54683 = ORIENTED_EDGE ( 'NONE', *, *, #68900, .F. ) ;
#54684 = CARTESIAN_POINT ( 'NONE',  ( 168.9909194888004436, 268.4774312744898452, 17.82429104036862100 ) ) ;
#54685 = CARTESIAN_POINT ( 'NONE',  ( 162.6937333994314656, 248.8531830095558632, 10.02305144031113926 ) ) ;
#54686 = VECTOR ( 'NONE', #35522, 1000.000000000000114 ) ;
#54687 = EDGE_CURVE ( 'NONE', #23380, #72513, #28695, .T. ) ;
#54688 = AXIS2_PLACEMENT_3D ( 'NONE', #90233, #35483, #44061 ) ;
#54689 = CARTESIAN_POINT ( 'NONE',  ( 164.9586510554008782, 244.9302305544571823, -1.717556444319656039 ) ) ;
#54691 = CARTESIAN_POINT ( 'NONE',  ( 73.80173605198457665, 55.24307582110920833, 16.12032811712526481 ) ) ;
#54690 = CARTESIAN_POINT ( 'NONE',  ( 194.4165969972361552, 293.9075714965812267, 14.23342188338008718 ) ) ;
#54692 = CARTESIAN_POINT ( 'NONE',  ( 176.1647493927595178, 285.2037997243469363, -12.30204738051347668 ) ) ;
#54693 = ADVANCED_FACE ( 'NONE', ( #58767 ), #88257, .F. ) ;
#54694 = CARTESIAN_POINT ( 'NONE',  ( 26.14792707536646432, 33.83478043621389020, -8.090169943749479842 ) ) ;
#54695 = CARTESIAN_POINT ( 'NONE',  ( 171.7482759404909700, 274.6702854657700072, 16.24998979151664713 ) ) ;
#54696 = CARTESIAN_POINT ( 'NONE',  ( 166.3380819770355856, 286.5636595477255923, -3.292484512480813308 ) ) ;
#54697 = CARTESIAN_POINT ( 'NONE',  ( 177.7742028453001240, 274.7292553766789638, -17.79112673411210821 ) ) ;
#54698 = CARTESIAN_POINT ( 'NONE',  ( 191.8959889624703408, 262.3180493352597864, 2.955584705640112997 ) ) ;
#54699 = CARTESIAN_POINT ( 'NONE',  ( 190.7404869014439726, 298.2747809567102308, -9.591077548819823662 ) ) ;
#54700 = VECTOR ( 'NONE', #90424, 1000.000000000000114 ) ;
#54701 = CARTESIAN_POINT ( 'NONE',  ( 3.097972219676621730, 184.8464784336661637, 1.353441290958777327E-15 ) ) ;
#54702 = CARTESIAN_POINT ( 'NONE',  ( 70.96429761875693032, 61.15374941679502996, 14.99935025239130226 ) ) ;
#54703 = VERTEX_POINT ( 'NONE', #36474 ) ;
#54704 = EDGE_CURVE ( 'NONE', #89705, #2785, #62887, .T. ) ;
#54705 = AXIS2_PLACEMENT_3D ( 'NONE', #10338, #63021, #717 ) ;
#54706 = CARTESIAN_POINT ( 'NONE',  ( 175.1487349639535864, 254.8191230408430954, 9.407919966538676348 ) ) ;
#54707 = CARTESIAN_POINT ( 'NONE',  ( 187.4676533354318906, 272.4601757945604845, -16.88503403312462936 ) ) ;
#54708 = CARTESIAN_POINT ( 'NONE',  ( -22.42236680055709641, 157.8615022471902591, 0.000000000000000000 ) ) ;
#54709 = CARTESIAN_POINT ( 'NONE',  ( 18.36166996137734841, 193.6589784336661637, -6.496448406907676862E-16 ) ) ;
#54710 = CARTESIAN_POINT ( 'NONE',  ( 27.45223038363779722, 27.80066082961423035, 10.00000000000000533 ) ) ;
#54711 = CARTESIAN_POINT ( 'NONE',  ( 33.32035334334607057, 27.43677371833803846, -10.00000000000000355 ) ) ;
#54712 = CARTESIAN_POINT ( 'NONE',  ( 84.83247989926988453, 42.35328799155462320, -1.743318450112538942 ) ) ;
#54713 = CARTESIAN_POINT ( 'NONE',  ( 173.6440257905655642, 272.7457858960242447, -16.35518571657235398 ) ) ;
#54714 = LINE ( 'NONE', #47623, #57293 ) ;
#54715 = B_SPLINE_SURFACE_WITH_KNOTS ( 'NONE', 3, 1, ( 
 ( #17385, #72109 ),
 ( #47279, #16882 ),
 ( #94929, #33599 ),
 ( #18406, #41171 ),
 ( #94426, #32074 ),
 ( #9293, #78202 ),
 ( #70581, #2208 ),
 ( #40168, #49296 ),
 ( #1709, #55858 ),
 ( #79242, #48805 ),
 ( #33090, #25489 ),
 ( #55366, #24487 ),
 ( #56878, #1196 ),
 ( #62987, #63488 ),
 ( #40675, #87861 ),
 ( #63986, #86853 ),
 ( #56380, #87378 ),
 ( #17907, #79738 ),
 ( #10298, #2712 ),
 ( #54690, #15699 ),
 ( #31898, #7610 ),
 ( #38996, #69902 ),
 ( #61798, #53694 ),
 ( #47602, #45597 ),
 ( #1017, #46597 ),
 ( #92744, #85153 ),
 ( #77004, #23299 ),
 ( #69414, #62802 ),
 ( #39483, #61304 ),
 ( #47104, #23801 ),
 ( #68903, #92266 ),
 ( #30414, #6625 ),
 ( #38499, #55191 ),
 ( #76528, #14713 ) ),
 .UNSPECIFIED., .T., .F., .F.,
 ( 4, 2, 2, 2, 2, 2, 2, 2, 2, 2, 2, 2, 2, 2, 2, 2, 4 ),
 ( 2, 2 ),
 ( 0.000000000000000000, 0.06250000000000000000, 0.1250000000000000000, 0.1875000000000000000, 0.2500000000000000000, 0.3125000000000000000, 0.3750000000000000000, 0.4375000000000000000, 0.5000000000000000000, 0.5625000000000000000, 0.6250000000000000000, 0.6875000000000000000, 0.7500000000000000000, 0.8125000000000000000, 0.8750000000000000000, 0.9375000000000000000, 1.000000000000000000 ),
 ( 0.000000000000000000, 1.000000000000000000 ),
 .UNSPECIFIED. ) ;
#54716 = CARTESIAN_POINT ( 'NONE',  ( 37.48526053816526371, 54.83666944042810343, -10.00000000000000000 ) ) ;
#54717 = EDGE_CURVE ( 'NONE', #91687, #19465, #76495, .T. ) ;
#54718 = CARTESIAN_POINT ( 'NONE',  ( 187.6689946892134913, 259.7079214702496870, -0.7711235126620424873 ) ) ;
#54719 = EDGE_CURVE ( 'NONE', #25562, #79014, #55160, .T. ) ;
#54720 = CARTESIAN_POINT ( 'NONE',  ( 77.24272341830209143, 208.7365022471902023, -10.00000000000009059 ) ) ;
#54721 = FACE_OUTER_BOUND ( 'NONE', #92456, .T. ) ;
#54722 = AXIS2_PLACEMENT_3D ( 'NONE', #73355, #96683, #27251 ) ;
#54723 = CARTESIAN_POINT ( 'NONE',  ( 203.5193203535926330, 270.1419797252951298, 6.025390116349934821 ) ) ;
#54724 = CARTESIAN_POINT ( 'NONE',  ( 29.78290061743214423, 181.8768266524160140, 9.188101187500098632 ) ) ;
#54725 = CARTESIAN_POINT ( 'NONE',  ( 66.97748580466556234, 68.05911003901715617, 6.908000617270682042 ) ) ;
#54726 = CARTESIAN_POINT ( 'NONE',  ( 124.8976233183423972, 254.4637435831425023, 2.679491924311251605 ) ) ;
#54727 = CARTESIAN_POINT ( 'NONE',  ( 203.0311039195969443, 269.9456838946036328, -6.239233117507705373 ) ) ;
#54728 = CARTESIAN_POINT ( 'NONE',  ( 150.9363692955544991, 269.2175350005573478, -14.27857383982596140 ) ) ;
#54729 = CARTESIAN_POINT ( 'NONE',  ( 3.854092266844447501, 28.45370138451379560, -10.00000000000000000 ) ) ;
#54730 = CARTESIAN_POINT ( 'NONE',  ( -78.94662368502558536, 55.85910816071121587, 10.00000000000000000 ) ) ;
#54731 = CARTESIAN_POINT ( 'NONE',  ( 159.8617658264064119, 278.4604067758004931, -10.61854734195418537 ) ) ;
#54732 = CARTESIAN_POINT ( 'NONE',  ( 207.3988330342936877, 270.8564699888902396, -1.301389719878858875 ) ) ;
#54733 = CARTESIAN_POINT ( 'NONE',  ( 20.98529944902502820, 27.51421378149918695, -9.188101187500004485 ) ) ;
#54734 = CARTESIAN_POINT ( 'NONE',  ( 163.1332433029523372, 248.0919295262283981, 11.24052392390482957 ) ) ;
#54735 = VECTOR ( 'NONE', #50588, 1000.000000000000000 ) ;
#54736 = CARTESIAN_POINT ( 'NONE',  ( 188.7811494455037860, 270.3288468973258887, -14.97842902622537231 ) ) ;
#54737 = ORIENTED_EDGE ( 'NONE', *, *, #27995, .F. ) ;
#54738 = CARTESIAN_POINT ( 'NONE',  ( 9.991594722369004700, 23.95586893147753926, 7.433330006724141015 ) ) ;
#54739 = FACE_OUTER_BOUND ( 'NONE', #40680, .T. ) ;
#54740 = CARTESIAN_POINT ( 'NONE',  ( 75.20199238159069921, 59.20172555882615484, -15.83912561188805590 ) ) ;
#54741 = CYLINDRICAL_SURFACE ( 'NONE', #86135, 7.500000000000000000 ) ;
#54742 = ADVANCED_FACE ( 'NONE', ( #46560 ), #38963, .F. ) ;
#54743 = VERTEX_POINT ( 'NONE', #60752 ) ;
#54744 = CARTESIAN_POINT ( 'NONE',  ( 49.03918259513507394, 79.59780946358316100, -10.00000000000000000 ) ) ;
#54745 = CARTESIAN_POINT ( 'NONE',  ( 72.52145085236621469, 71.52933981707218436, -5.380113948530985013 ) ) ;
#54746 = LINE ( 'NONE', #87741, #22522 ) ;
#54747 = LINE ( 'NONE', #85210, #46850 ) ;
#54748 = ORIENTED_EDGE ( 'NONE', *, *, #57167, .T. ) ;
#54749 = ORIENTED_EDGE ( 'NONE', *, *, #57118, .F. ) ;
#54750 = ADVANCED_FACE ( 'NONE', ( #45566 ), #37958, .F. ) ;
#54752 = CARTESIAN_POINT ( 'NONE',  ( 85.89759834047637810, 43.04820835652777333, -2.464790169128945774 ) ) ;
#54751 = CYLINDRICAL_SURFACE ( 'NONE', #63317, 17.82106496071139645 ) ;
#54753 = VERTEX_POINT ( 'NONE', #49085 ) ;
#54754 = CARTESIAN_POINT ( 'NONE',  ( 153.4495116231415750, 264.8646448025247082, -16.73555355292144498 ) ) ;
#54755 = AXIS2_PLACEMENT_3D ( 'NONE', #18479, #27579, #26574 ) ;
#54756 = CARTESIAN_POINT ( 'NONE',  ( 72.08021828965947009, 72.40975849880194914, -3.082927075499598324 ) ) ;
#54757 = CARTESIAN_POINT ( 'NONE',  ( 72.82235704132158105, 56.84590537091418128, -15.94416503159311027 ) ) ;
#54758 = CARTESIAN_POINT ( 'NONE',  ( 76.88601853014658616, 63.69663891124154276, 15.33692311465240543 ) ) ;
#54759 = CARTESIAN_POINT ( 'NONE',  ( 147.6088797830324779, 274.9809158978982850, 8.531536684623960198 ) ) ;
#54760 = ADVANCED_FACE ( 'NONE', ( #56158 ), #16675, .T. ) ;
#54761 = AXIS2_PLACEMENT_3D ( 'NONE', #84090, #44015, #14140 ) ;
#54762 = EDGE_CURVE ( 'NONE', #8176, #90906, #66128, .T. ) ;
#54763 = AXIS2_PLACEMENT_3D ( 'NONE', #95214, #32857, #26271 ) ;
#54764 = CARTESIAN_POINT ( 'NONE',  ( 180.4468251236610854, 287.2605667330827828, -13.89116134381312584 ) ) ;
#54765 = EDGE_CURVE ( 'NONE', #50442, #77615, #93208, .T. ) ;
#54766 = ORIENTED_EDGE ( 'NONE', *, *, #97037, .T. ) ;
#54767 = CARTESIAN_POINT ( 'NONE',  ( 157.2744851780909414, 258.2395962677452985, 18.17792129701959070 ) ) ;
#54768 = AXIS2_PLACEMENT_3D ( 'NONE', #59098, #90072, #20642 ) ;
#54769 = ADVANCED_FACE ( 'NONE', ( #70371 ), #80518, .F. ) ;
#54770 = CARTESIAN_POINT ( 'NONE',  ( 174.3697573357644899, 277.1653490889620457, -17.12727634137145571 ) ) ;
#54771 = VERTEX_POINT ( 'NONE', #59137 ) ;
#54772 = EDGE_CURVE ( 'NONE', #41280, #79632, #65272, .T. ) ;
#54773 = CARTESIAN_POINT ( 'NONE',  ( 31.05164846989082506, 29.87878583063843507, -9.188101187500006262 ) ) ;
#54774 = CARTESIAN_POINT ( 'NONE',  ( 159.2303255284352304, 254.8519814094557603, 16.39103317446447150 ) ) ;
#54775 = CARTESIAN_POINT ( 'NONE',  ( 191.4282440714642917, 263.9101566603287665, -9.496572910043623139 ) ) ;
#54776 = EDGE_CURVE ( 'NONE', #34725, #83448, #51054, .T. ) ;
#54777 = CARTESIAN_POINT ( 'NONE',  ( 64.91088251055593616, 208.2833772461660544, -9.188101187500095079 ) ) ;
#54778 = ORIENTED_EDGE ( 'NONE', *, *, #62450, .T. ) ;
#54779 = CARTESIAN_POINT ( 'NONE',  ( -17.81096996955940526, 76.60683456116618117, 13.45353793954188681 ) ) ;
#54780 = FACE_BOUND ( 'NONE', #91746, .T. ) ;
#54781 = FACE_OUTER_BOUND ( 'NONE', #56381, .T. ) ;
#54782 = CARTESIAN_POINT ( 'NONE',  ( 102.5559242795368391, 220.0177522451417929, 5.000000000000051514 ) ) ;
#54783 = VERTEX_POINT ( 'NONE', #73387 ) ;
#54784 = ORIENTED_EDGE ( 'NONE', *, *, #24320, .T. ) ;
#54785 = AXIS2_PLACEMENT_3D ( 'NONE', #26717, #17621, #95163 ) ;
#54786 = CARTESIAN_POINT ( 'NONE',  ( 87.13645712923818110, 46.25687745756817293, 8.491008164162357374 ) ) ;
#54787 = LINE ( 'NONE', #62890, #7240 ) ;
#54788 = CARTESIAN_POINT ( 'NONE',  ( 147.7157269441172218, 274.7958511862549926, 8.036290321896261801 ) ) ;
#54789 = ORIENTED_EDGE ( 'NONE', *, *, #19895, .T. ) ;
#54790 = CARTESIAN_POINT ( 'NONE',  ( 149.6700657135140489, 271.4108371424580355, 12.58635654151485284 ) ) ;
#54791 = CARTESIAN_POINT ( 'NONE',  ( 172.7859815943955084, 252.0003099901749692, 7.695973030949746274 ) ) ;
#54792 = CARTESIAN_POINT ( 'NONE',  ( 84.11911179316838627, 207.8262482093457777, 3.021315404115420679E-15 ) ) ;
#54793 = CARTESIAN_POINT ( 'NONE',  ( 193.0065576635309412, 296.3498312632291913, -11.90044991639595295 ) ) ;
#54795 = DIRECTION ( 'NONE',  ( 0.8660254037844385966, 0.5000000000000004441, 0.000000000000000000 ) ) ;
#54794 = B_SPLINE_CURVE_WITH_KNOTS ( 'NONE', 3,
 ( #64906, #62891, #57286, #18312 ),
 .UNSPECIFIED., .F., .F.,
 ( 4, 4 ),
 ( 0.008648408712914583060, 0.01500284571837401729 ),
 .UNSPECIFIED. ) ;
#54796 = B_SPLINE_CURVE_WITH_KNOTS ( 'NONE', 3,
 ( #77112, #30519, #22909, #75147, #127, #38095, #52808, #67520, #98450, #5725, #59912, #30016, #99936, #69006, #68022, #61408 ),
 .UNSPECIFIED., .F., .F.,
 ( 4, 1, 2, 2, 2, 1, 2, 2, 4 ),
 ( 0.000000000000000000, 0.1250000000000056344, 0.1875000000000079103, 0.2500000000000102141, 0.5000000000000087708, 0.6250000000000062172, 0.6875000000000045519, 0.7500000000000028866, 1.000000000000000000 ),
 .UNSPECIFIED. ) ;
#54797 = CARTESIAN_POINT ( 'NONE',  ( 37.48526053816526371, 54.83666944042810343, -10.00000000000000000 ) ) ;
#54798 = AXIS2_PLACEMENT_3D ( 'NONE', #45561, #30377, #91212 ) ;
#54799 = CARTESIAN_POINT ( 'NONE',  ( 184.6885808911535207, 260.6528513612950064, 10.31057805081157852 ) ) ;
#54800 = CARTESIAN_POINT ( 'NONE',  ( 200.3804403721752578, 281.5778917628034606, 17.30444700233937994 ) ) ;
#54801 = CARTESIAN_POINT ( 'NONE',  ( 77.00910850481051284, 63.69207575539577704, -14.97815254220547487 ) ) ;
#54802 = CARTESIAN_POINT ( 'NONE',  ( 78.56719005003022005, 47.98515344134878546, 13.96283253221395881 ) ) ;
#54803 = CARTESIAN_POINT ( 'NONE',  ( 118.9295641673753181, 227.2202760586659736, -5.415160957724236172E-17 ) ) ;
#54804 = ORIENTED_EDGE ( 'NONE', *, *, #75707, .F. ) ;
#54805 = CARTESIAN_POINT ( 'NONE',  ( 147.2405539530007559, 275.6188749492528132, 0.4306668706573002492 ) ) ;
#54806 = CARTESIAN_POINT ( 'NONE',  ( 82.96321432696582576, 41.33265327218170171, -1.885893662060450060 ) ) ;
#54807 = CARTESIAN_POINT ( 'NONE',  ( 87.78256729009754622, 45.12882416216076820, -6.783508070075447982 ) ) ;
#54808 = CARTESIAN_POINT ( 'NONE',  ( 202.8874463667715133, 279.2356300052831557, -15.29930322226033468 ) ) ;
#54809 = CARTESIAN_POINT ( 'NONE',  ( 192.5726205457860942, 296.4466972196345296, 11.71797434446428987 ) ) ;
#54810 = CARTESIAN_POINT ( 'NONE',  ( 83.69613447051490596, 51.47860253839341738, -14.37487551769288352 ) ) ;
#54811 = CARTESIAN_POINT ( 'NONE',  ( 165.3840372259151366, 283.6698659644395093, -8.347863386361117577 ) ) ;
#54812 = ORIENTED_EDGE ( 'NONE', *, *, #5762, .T. ) ;
#54813 = CARTESIAN_POINT ( 'NONE',  ( 162.6257765080958677, 248.9708877980734485, -10.42859054881151160 ) ) ;
#54814 = CARTESIAN_POINT ( 'NONE',  ( 72.35414581608256412, 71.76618622507949397, 5.628474724962970299 ) ) ;
#54815 = CARTESIAN_POINT ( 'NONE',  ( 205.8477028968504783, 272.4695280978870073, 9.472321179085877674 ) ) ;
#54816 = CARTESIAN_POINT ( 'NONE',  ( 151.0801312611820890, 268.9685319718947198, -15.83903210480701240 ) ) ;
#54817 = CARTESIAN_POINT ( 'NONE',  ( 185.8848700110949039, 296.7474278773313472, 4.608973075700647293 ) ) ;
#54818 = CARTESIAN_POINT ( 'NONE',  ( 177.9552638626009298, 260.7378092407702184, -13.94576028113082877 ) ) ;
#54819 = DIRECTION ( 'NONE',  ( -1.000000000000000000, 0.000000000000000000, 0.000000000000000000 ) ) ;
#54820 = CARTESIAN_POINT ( 'NONE',  ( 48.45674693441662129, 186.5327760586659451, 1.948934522072303157E-15 ) ) ;
#54821 = CARTESIAN_POINT ( 'NONE',  ( 164.9335952247126045, 244.9736285262353306, -1.661461410667423255 ) ) ;
#54822 = ORIENTED_EDGE ( 'NONE', *, *, #45199, .F. ) ;
#54823 = CARTESIAN_POINT ( 'NONE',  ( 72.39118694979968893, 67.66586127011399299, 10.85488035418265085 ) ) ;
#54824 = CARTESIAN_POINT ( 'NONE',  ( -19.58090909066553920, 93.18709903958436769, 59.99999999999999289 ) ) ;
#54825 = DIRECTION ( 'NONE',  ( 0.8660254037844379305, 0.5000000000000014433, 0.000000000000000000 ) ) ;
#54826 = CARTESIAN_POINT ( 'NONE',  ( 174.1447466443229359, 262.0166869877857607, 14.36471543667183681 ) ) ;
#54827 = CARTESIAN_POINT ( 'NONE',  ( 36.25628400652970384, 53.06077264917335867, -10.00000000000000000 ) ) ;
#54828 = CARTESIAN_POINT ( 'NONE',  ( 203.1705638993064156, 278.7452560544191442, -15.08126533799095093 ) ) ;
#54829 = CARTESIAN_POINT ( 'NONE',  ( 154.3368938251639406, 269.3942069059096411, -15.13873655495052262 ) ) ;
#54830 = CARTESIAN_POINT ( 'NONE',  ( 102.9889369814290347, 230.2677522451418497, 10.00000000000009592 ) ) ;
#54831 = CARTESIAN_POINT ( 'NONE',  ( 45.60499120716188060, 26.73415679381826138, -6.890680421881970419E-14 ) ) ;
#54832 = ORIENTED_EDGE ( 'NONE', *, *, #31190, .T. ) ;
#54833 = EDGE_CURVE ( 'NONE', #6372, #5348, #64787, .T. ) ;
#54834 = VECTOR ( 'NONE', #87337, 1000.000000000000114 ) ;
#54835 = CARTESIAN_POINT ( 'NONE',  ( 163.0171530587457767, 248.2930037274571191, 9.677214176418313940 ) ) ;
#54836 = CARTESIAN_POINT ( 'NONE',  ( 87.97974684949012669, 44.79880412219662844, 4.785089242980530955 ) ) ;
#54837 = VECTOR ( 'NONE', #57308, 1000.000000000000114 ) ;
#54838 = CARTESIAN_POINT ( 'NONE',  ( 19.17374232530777078, 188.0024278399161233, 9.188101187500095079 ) ) ;
#54839 = VECTOR ( 'NONE', #81284, 1000.000000000000114 ) ;
#54840 = CARTESIAN_POINT ( 'NONE',  ( 15.49551970000783996, 14.11029122506293021, -8.090169943749478065 ) ) ;
#54841 = CARTESIAN_POINT ( 'NONE',  ( 81.90250264543212211, 49.37766992099674468, -14.25890439565079681 ) ) ;
#54842 = CARTESIAN_POINT ( 'NONE',  ( 71.86082717042363299, 59.56791737868546477, -15.73637609511307289 ) ) ;
#54843 = CARTESIAN_POINT ( 'NONE',  ( 74.04309036720468384, 54.83868394417908831, -16.13477068996618513 ) ) ;
#54845 = CARTESIAN_POINT ( 'NONE',  ( 70.26924114858965709, 217.5024278399160664, -9.188101187500093303 ) ) ;
#54844 = DIRECTION ( 'NONE',  ( -1.000000000000000000, 0.000000000000000000, 0.000000000000000000 ) ) ;
#54846 = CARTESIAN_POINT ( 'NONE',  ( 208.1757572214753793, 270.0760069187178374, 2.172546422564154867 ) ) ;
#54847 = CARTESIAN_POINT ( 'NONE',  ( 10.89475974595093000, 11.45404122711131478, -8.090169943749478065 ) ) ;
#54848 = CARTESIAN_POINT ( 'NONE',  ( 184.1672717435397431, 256.7531923835571774, 1.415796120779537093 ) ) ;
#54849 = EDGE_CURVE ( 'NONE', #34337, #29477, #98814, .T. ) ;
#54850 = CARTESIAN_POINT ( 'NONE',  ( -29.54910080626416047, 95.88061498994892418, 44.62839885622795322 ) ) ;
#54851 = CARTESIAN_POINT ( 'NONE',  ( 11.88462290154380874, 22.56454794089039950, 10.00000000000000355 ) ) ;
#54852 = EDGE_LOOP ( 'NONE', ( #49154, #64268, #70241, #38550 ) ) ;
#54853 = ADVANCED_FACE ( 'NONE', ( #72404 ), #20187, .T. ) ;
#54854 = AXIS2_PLACEMENT_3D ( 'NONE', #69943, #560, #62336 ) ;
#54855 = CARTESIAN_POINT ( 'NONE',  ( 165.4802685333492320, 269.3555218720375137, 17.18790657701241642 ) ) ;
#54856 = CARTESIAN_POINT ( 'NONE',  ( 34.30229714732364954, 190.6115022471902591, 10.00000000000009592 ) ) ;
#54857 = DIRECTION ( 'NONE',  ( -1.000000000000000000, 0.000000000000000000, 0.000000000000000000 ) ) ;
#54858 = DIRECTION ( 'NONE',  ( 0.8660254037844382635, 0.5000000000000005551, 0.000000000000000000 ) ) ;
#54859 = CARTESIAN_POINT ( 'NONE',  ( -15.79203335248894469, 167.8149278399160949, -9.188101187500095079 ) ) ;
#54860 = CARTESIAN_POINT ( 'NONE',  ( 35.77386594998528579, 21.44966523072496756, -2.296566073217252530E-15 ) ) ;
#54861 = CARTESIAN_POINT ( 'NONE',  ( 200.3283417415170220, 283.2787895630095250, 16.79050732642456012 ) ) ;
#54862 = CARTESIAN_POINT ( 'NONE',  ( 189.2791439001235290, 261.6176991415632642, 6.688689801143334002 ) ) ;
#54863 = CARTESIAN_POINT ( 'NONE',  ( 164.6869624841032191, 245.4008089637804346, 1.435659848726088317 ) ) ;
#54864 = DIRECTION ( 'NONE',  ( -0.000000000000000000, 1.000000000000000000, -0.000000000000000000 ) ) ;
#54865 = CARTESIAN_POINT ( 'NONE',  ( 66.53410914940803877, 68.80543330372941568, 2.269385016797728305 ) ) ;
#54866 = VERTEX_POINT ( 'NONE', #50561 ) ;
#54867 = DIRECTION ( 'NONE',  ( -0.9538480676139692305, 0.3002896333693469422, 0.000000000000000000 ) ) ;
#54868 = DIRECTION ( 'NONE',  ( -0.000000000000000000, -0.000000000000000000, -1.000000000000000000 ) ) ;
#54869 = CARTESIAN_POINT ( 'NONE',  ( 172.8705364283385961, 268.5860898973321014, -17.62214513231522872 ) ) ;
#54870 = CARTESIAN_POINT ( 'NONE',  ( 9.185703322462064335, 20.70171378149917274, -9.188101187500004485 ) ) ;
#54871 = VECTOR ( 'NONE', #35178, 1000.000000000000000 ) ;
#54872 = CARTESIAN_POINT ( 'NONE',  ( 165.8564336512527291, 246.0288987632202407, -1.146165424362591612 ) ) ;
#54873 = CARTESIAN_POINT ( 'NONE',  ( 88.27455224169976589, 44.26958888746147380, -1.928006731073693469 ) ) ;
#54874 = DIRECTION ( 'NONE',  ( 0.4999999999999992784, -0.8660254037844390407, 0.000000000000000000 ) ) ;
#54875 = DIRECTION ( 'NONE',  ( -0.8660254037844378194, -0.5000000000000013323, -0.000000000000000000 ) ) ;
#54876 = CARTESIAN_POINT ( 'NONE',  ( -13.93676304270635136, 104.6887507934693105, 43.89948692389422291 ) ) ;
#54877 = DIRECTION ( 'NONE',  ( -0.8660254037844387076, -0.4999999999999998890, -0.000000000000000000 ) ) ;
#54878 = CARTESIAN_POINT ( 'NONE',  ( 207.5886452961740076, 271.0929146030698007, -1.661373005306138184 ) ) ;
#54879 = CARTESIAN_POINT ( 'NONE',  ( 152.7729059155601021, 266.0365602647466972, -17.50667083025758686 ) ) ;
#54880 = ORIENTED_EDGE ( 'NONE', *, *, #45815, .T. ) ;
#54881 = EDGE_LOOP ( 'NONE', ( #31594, #21309, #7238, #97552, #6881 ) ) ;
#54882 = ADVANCED_FACE ( 'NONE', ( #20681 ), #51569, .T. ) ;
#54883 = CARTESIAN_POINT ( 'NONE',  ( 130.4311169673963207, 256.1115022471902876, -5.000000000000047962 ) ) ;
#54884 = CARTESIAN_POINT ( 'NONE',  ( 72.77371579809937430, 70.82568240960111439, 7.174012581183236925 ) ) ;
#54885 = ORIENTED_EDGE ( 'NONE', *, *, #74606, .T. ) ;
#54886 = CARTESIAN_POINT ( 'NONE',  ( 70.07366985589914066, 68.21750869337182621, 9.404999606781979438 ) ) ;
#54887 = CARTESIAN_POINT ( 'NONE',  ( 203.4435754520237651, 276.2723861740593634, 14.48166091637323483 ) ) ;
#54888 = VERTEX_POINT ( 'NONE', #80521 ) ;
#54889 = CARTESIAN_POINT ( 'NONE',  ( 68.69988281822412546, 63.95555916913097150, -12.08471377653384771 ) ) ;
#54890 = CARTESIAN_POINT ( 'NONE',  ( 79.42902015582541253, 59.13724458665812023, -16.22739499525147266 ) ) ;
#54891 = EDGE_CURVE ( 'NONE', #41027, #50534, #83652, .T. ) ;
#54892 = CARTESIAN_POINT ( 'NONE',  ( 186.3211539507438772, 284.5818887155355696, -17.00132214566409417 ) ) ;
#54893 = CARTESIAN_POINT ( 'NONE',  ( 69.50649804366692308, 62.68264628211643696, 13.83822202275866786 ) ) ;
#54894 = ORIENTED_EDGE ( 'NONE', *, *, #57248, .F. ) ;
#54895 = CARTESIAN_POINT ( 'NONE',  ( 161.3227470381586102, 251.2278010437646856, 14.45097375514160731 ) ) ;
#54896 = CARTESIAN_POINT ( 'NONE',  ( 9.830230629461709668, 30.95267373526312227, -10.00000000000000000 ) ) ;
#54897 = CARTESIAN_POINT ( 'NONE',  ( 190.8001679306945277, 300.1714103817999444, 7.815449226872675403 ) ) ;
#54898 = CARTESIAN_POINT ( 'NONE',  ( 47.54560441532652959, 78.55524412553472757, -10.00000000000000000 ) ) ;
#54899 = ORIENTED_EDGE ( 'NONE', *, *, #94761, .F. ) ;
#54900 = ADVANCED_FACE ( 'NONE', ( #92596 ), #21671, .T. ) ;
#54901 = VERTEX_POINT ( 'NONE', #14573 ) ;
#54902 = VERTEX_POINT ( 'NONE', #68751 ) ;
#54903 = CARTESIAN_POINT ( 'NONE',  ( 160.3325118702422571, 268.9022058081687874, -16.89581317083065315 ) ) ;
#54904 = ORIENTED_EDGE ( 'NONE', *, *, #9513, .F. ) ;
#54905 = CARTESIAN_POINT ( 'NONE',  ( 71.12899601204873079, 71.68446395904118162, 1.608505432448458894 ) ) ;
#54906 = ORIENTED_EDGE ( 'NONE', *, *, #10419, .F. ) ;
#54907 = CARTESIAN_POINT ( 'NONE',  ( 164.3602934812760452, 245.9666162739349318, -7.171958108566009571 ) ) ;
#54908 =( BOUNDED_CURVE ( )  B_SPLINE_CURVE ( 2, ( #42881, #72846, #66217, #58590, #73817, #11535, #97637, #42395, #50997 ),
 .UNSPECIFIED., .F., .T. ) 
 B_SPLINE_CURVE_WITH_KNOTS ( ( 3, 2, 2, 2, 3 ),
 ( 0.8991935483870967527, 0.9005376344086021279, 0.9032258064516128782, 0.9059139784946236285, 0.9072580645161290036 ),
 .UNSPECIFIED. ) 
 CURVE ( )  GEOMETRIC_REPRESENTATION_ITEM ( )  RATIONAL_B_SPLINE_CURVE ( ( 0.9330127018922194093, 0.9330127018922194093, 1.000000000000000000, 0.8660254037844387076, 1.000000000000000000, 0.8660254037844387076, 1.000000000000000000, 0.9330127018922194093, 0.9330127018922194093 ) ) 
 REPRESENTATION_ITEM ( '' )  );
#54909 = CARTESIAN_POINT ( 'NONE',  ( 82.76870359366968444, 47.59112932736264412, 12.29198334313100105 ) ) ;
#54910 = CARTESIAN_POINT ( 'NONE',  ( 165.2222719793527972, 271.1331909122671959, 17.05175473187279778 ) ) ;
#54911 = CARTESIAN_POINT ( 'NONE',  ( 170.9894191764510083, 283.3192944120900734, 12.01118185074416012 ) ) ;
#54912 = CARTESIAN_POINT ( 'NONE',  ( 194.2389208611690492, 294.2153155915419802, -15.75132567904764791 ) ) ;
#54914 = CARTESIAN_POINT ( 'NONE',  ( 82.48332016352127027, 53.47388482021811740, -15.74481631320922048 ) ) ;
#54913 = AXIS2_PLACEMENT_3D ( 'NONE', #36530, #67431, #6647 ) ;
#54915 = CARTESIAN_POINT ( 'NONE',  ( 159.0092078971553633, 255.2349683812814476, -17.41003440661054213 ) ) ;
#54916 = DIRECTION ( 'NONE',  ( -0.9505498757754612393, 0.3105719460338542959, 0.000000000000000000 ) ) ;
#54917 = CARTESIAN_POINT ( 'NONE',  ( 19.94606896448370392, 26.91421378149918553, 9.188101187500008038 ) ) ;
#54918 = CARTESIAN_POINT ( 'NONE',  ( 198.3474120736350983, 277.3537790377902752, -15.33034485771529098 ) ) ;
#54919 = CARTESIAN_POINT ( 'NONE',  ( 187.6777693585253814, 293.2028220897474853, -13.03854654741220997 ) ) ;
#54920 = AXIS2_PLACEMENT_3D ( 'NONE', #95913, #19392, #34078 ) ;
#54922 = ORIENTED_EDGE ( 'NONE', *, *, #21173, .F. ) ;
#54921 = CARTESIAN_POINT ( 'NONE',  ( 206.9949618004799561, 271.7276603789779870, 5.520981849004880537 ) ) ;
#54923 = CARTESIAN_POINT ( 'NONE',  ( 146.6887764566487533, 276.5745816074078789, -3.628288772073474888 ) ) ;
#54924 = CARTESIAN_POINT ( 'NONE',  ( 179.6160012257981862, 295.0481727651569486, 1.085779272287555663 ) ) ;
#54925 = CARTESIAN_POINT ( 'NONE',  ( 206.0946696452135427, 273.6805563358039421, -10.19627505985792837 ) ) ;
#54926 = CARTESIAN_POINT ( 'NONE',  ( 69.95523204135938045, 62.90150226501648234, 13.86126985460704297 ) ) ;
#54927 = CARTESIAN_POINT ( 'NONE',  ( 84.79359905062281655, 45.64121975909452544, -9.352143619951702291 ) ) ;
#54928 = CARTESIAN_POINT ( 'NONE',  ( 200.1662314894802819, 283.9489124310637180, 17.19420058542677054 ) ) ;
#54929 = CARTESIAN_POINT ( 'NONE',  ( 190.9055077653416674, 262.0587109976776219, -0.7351936343916617433 ) ) ;
#54930 = AXIS2_PLACEMENT_3D ( 'NONE', #73715, #46136, #3816 ) ;
#54931 = ORIENTED_EDGE ( 'NONE', *, *, #33555, .F. ) ;
#54932 = CARTESIAN_POINT ( 'NONE',  ( 194.3072059070401849, 294.0970424226961768, -15.66788609332525617 ) ) ;
#54933 = CARTESIAN_POINT ( 'NONE',  ( 74.87331927037790535, 66.80950769484920215, -13.20416362156882784 ) ) ;
#54935 = EDGE_CURVE ( 'NONE', #35157, #61620, #69252, .T. ) ;
#54934 = CARTESIAN_POINT ( 'NONE',  ( -7.521556465916529710, 24.12430647450515053, -10.00000000000000000 ) ) ;
#54936 = CARTESIAN_POINT ( 'NONE',  ( 19.85049821812286908, 192.2677522451419350, -5.000000000000047962 ) ) ;
#54937 = CARTESIAN_POINT ( 'NONE',  ( 92.13672968991174628, 217.8768266524160140, 9.188101187500096856 ) ) ;
#54938 = CARTESIAN_POINT ( 'NONE',  ( 196.1696074310564200, 269.5488462819374718, -11.79737468409024892 ) ) ;
#54939 = PLANE ( 'NONE',  #97213 ) ;
#54940 = PLANE ( 'NONE',  #75779 ) ;
#54942 = CARTESIAN_POINT ( 'NONE',  ( 75.60565924420463091, 65.54105765176767306, 13.80443174476947732 ) ) ;
#54941 = CARTESIAN_POINT ( 'NONE',  ( 13.92363686274711299, 178.8458772461660544, 9.188101187500095079 ) ) ;
#54943 = AXIS2_PLACEMENT_3D ( 'NONE', #11190, #72992, #46996 ) ;
#54944 = CARTESIAN_POINT ( 'NONE',  ( 161.3644539559160478, 251.1555625431813894, 12.97746593258196413 ) ) ;
#54945 = VERTEX_POINT ( 'NONE', #21186 ) ;
#54946 = ORIENTED_EDGE ( 'NONE', *, *, #24972, .F. ) ;
#54947 = DIRECTION ( 'NONE',  ( 0.2588190451024995897, 0.9659258262890739744, 0.000000000000000000 ) ) ;
#54948 = CARTESIAN_POINT ( 'NONE',  ( 201.1151172693584783, 267.4386146601190717, -3.692085840245449724 ) ) ;
#54949 = CARTESIAN_POINT ( 'NONE',  ( 81.89789973039891890, 46.67758023279904478, -11.97137090468010356 ) ) ;
#54950 = CARTESIAN_POINT ( 'NONE',  ( 22.61461015039527922, 36.55466486950700755, 7.012934429366973338E-14 ) ) ;
#54951 = CARTESIAN_POINT ( 'NONE',  ( 161.1492466472929266, 251.5283125358769212, -13.33353587056634915 ) ) ;
#54952 = LINE ( 'NONE', #17459, #80618 ) ;
#54953 = CARTESIAN_POINT ( 'NONE',  ( 74.09829895435802882, 68.37032454858436381, -11.67432565205426620 ) ) ;
#54954 = CARTESIAN_POINT ( 'NONE',  ( 32.78649236710315762, 198.9244531367911293, -4.594050593750046652 ) ) ;
#54955 = DIRECTION ( 'NONE',  ( -0.5778974349098193741, -0.4186690413702516822, -0.7005360722495063142 ) ) ;
#54956 = VERTEX_POINT ( 'NONE', #23142 ) ;
#54957 = DIRECTION ( 'NONE',  ( -0.06958655048002569676, 0.1205274409548614395, -0.9902680687415721383 ) ) ;
#54958 = CARTESIAN_POINT ( 'NONE',  ( -13.55913805958770624, 162.9786897466781852, -9.594050593750095501 ) ) ;
#54959 = CARTESIAN_POINT ( 'NONE',  ( 29.54281338067077911, 40.55466486950702176, -1.111400068045478839E-16 ) ) ;
#54960 = DIRECTION ( 'NONE',  ( -0.8660254037844387076, -0.4999999999999998890, -0.000000000000000000 ) ) ;
#54961 = CARTESIAN_POINT ( 'NONE',  ( 48.81784752633560487, 86.82484054835779830, -10.00000000000000000 ) ) ;
#54962 = CARTESIAN_POINT ( 'NONE',  ( 189.0920916512246208, 280.9571135833196536, -17.80812859110469404 ) ) ;
#54963 = CARTESIAN_POINT ( 'NONE',  ( 41.51553799054924099, 59.02985107750643579, -10.00000000000000000 ) ) ;
#54964 = CARTESIAN_POINT ( 'NONE',  ( 148.0637215040603394, 274.1931069276759558, -7.795633835291665648 ) ) ;
#54965 = CARTESIAN_POINT ( 'NONE',  ( 191.6817669736708467, 264.6815271297149366, 7.777474833780424923 ) ) ;
#54966 = CARTESIAN_POINT ( 'NONE',  ( 164.7171516385412815, 249.8514189067689131, -10.51224052795927300 ) ) ;
#54967 = CARTESIAN_POINT ( 'NONE',  ( 18.26047324907200675, 192.8967562850347122, -4.648177544792955347E-16 ) ) ;
#54968 = EDGE_CURVE ( 'NONE', #33594, #24915, #45449, .T. ) ;
#54969 = CARTESIAN_POINT ( 'NONE',  ( 147.0660117096331874, 275.9211909828330249, -0.7354350123930680772 ) ) ;
#54970 = CARTESIAN_POINT ( 'NONE',  ( 147.6300909839706321, 274.9441770201837585, 8.328755691084779755 ) ) ;
#54971 = CARTESIAN_POINT ( 'NONE',  ( 181.2305971022323661, 265.9781236237157032, -15.82518789413146010 ) ) ;
#54972 = VERTEX_POINT ( 'NONE', #75894 ) ;
#54973 = B_SPLINE_CURVE_WITH_KNOTS ( 'NONE', 3,
 ( #16398, #54892, #31088, #56766 ),
 .UNSPECIFIED., .F., .F.,
 ( 4, 4 ),
 ( 0.008151151042490834345, 0.01635116468880294660 ),
 .UNSPECIFIED. ) ;
#54974 = CARTESIAN_POINT ( 'NONE',  ( 75.35150063214643978, 63.77177416529143983, 14.96501676786058255 ) ) ;
#54975 = EDGE_CURVE ( 'NONE', #84992, #86705, #94002, .T. ) ;
#54976 = CARTESIAN_POINT ( 'NONE',  ( 161.4289481915915587, 251.7506084730134432, -13.50114579149946259 ) ) ;
#54977 = CARTESIAN_POINT ( 'NONE',  ( 119.9849458542963561, 230.8923013555409796, 4.594050593750050204 ) ) ;
#54978 = CARTESIAN_POINT ( 'NONE',  ( 19.43607595823839418, 14.14754757982089473, -5.678558825948276656 ) ) ;
#54979 = CARTESIAN_POINT ( 'NONE',  ( -11.16403655135938955, 164.3615022471902591, -10.00000000000009592 ) ) ;
#54980 = AXIS2_PLACEMENT_3D ( 'NONE', #12571, #58152, #50544 ) ;
#54982 = CARTESIAN_POINT ( 'NONE',  ( 191.6453933565204295, 276.9075887682292887, 17.07476665461427245 ) ) ;
#54981 = CARTESIAN_POINT ( 'NONE',  ( 49.07456115661582174, 91.13648234292965356, -10.00000000000000000 ) ) ;
#54983 = CARTESIAN_POINT ( 'NONE',  ( 191.2547573475860361, 299.3840384151609442, -6.665042208860675110 ) ) ;
#54984 = CARTESIAN_POINT ( 'NONE',  ( 30.01653393904200584, 17.73415679381823296, -6.890680421881970419E-14 ) ) ;
#54985 = DIRECTION ( 'NONE',  ( -0.9364604334398972663, 0.2023802897980892801, 0.2865031848039413243 ) ) ;
#54986 = CARTESIAN_POINT ( 'NONE',  ( 177.2783070499642406, 266.6479886748795707, -16.91666554439952108 ) ) ;
#54987 = CARTESIAN_POINT ( 'NONE',  ( 146.8574506849497538, 276.2824292740633041, -4.888313306692038118 ) ) ;
#54988 = CARTESIAN_POINT ( 'NONE',  ( -58.00277386063316243, 34.50477571329874138, 177.5919119679930134 ) ) ;
#54989 = ORIENTED_EDGE ( 'NONE', *, *, #7592, .T. ) ;
#54990 = CARTESIAN_POINT ( 'NONE',  ( 192.6608248749084851, 267.1914924341284063, 11.10020417146784588 ) ) ;
#54991 = CARTESIAN_POINT ( 'NONE',  ( 178.7256942771215051, 280.7533503143234270, 16.50221326603510263 ) ) ;
#54992 = CARTESIAN_POINT ( 'NONE',  ( 82.04273294443818543, 51.69458978218974465, 15.23912461881878677 ) ) ;
#54993 = CARTESIAN_POINT ( 'NONE',  ( 179.9209375999747351, 276.5811748711908535, 17.74520275588677265 ) ) ;
#54994 = CARTESIAN_POINT ( 'NONE',  ( 180.4746716150172574, 261.7121554277162545, -13.47270644325290156 ) ) ;
#54995 = CARTESIAN_POINT ( 'NONE',  ( 162.7020145476934090, 284.0983276010327359, 6.051621772638641872 ) ) ;
#54996 = VECTOR ( 'NONE', #84650, 1000.000000000000114 ) ;
#54997 = CARTESIAN_POINT ( 'NONE',  ( 192.1640094933931096, 297.8091675017319062, 12.36911124822534447 ) ) ;
#54998 = ORIENTED_EDGE ( 'NONE', *, *, #18403, .F. ) ;
#54999 = EDGE_CURVE ( 'NONE', #97286, #71770, #96305, .T. ) ;
#55000 = CARTESIAN_POINT ( 'NONE',  ( 73.57121657643290291, 69.82745460598127352, 9.896087309288359890 ) ) ;
#55001 = B_SPLINE_SURFACE_WITH_KNOTS ( 'NONE', 3, 1, ( 
 ( #43166, #67478 ),
 ( #90837, #52275 ),
 ( #98404, #74620 ),
 ( #66976, #97903 ),
 ( #59871, #67980 ),
 ( #59359, #33739 ),
 ( #90335, #48930 ),
 ( #64632, #13309 ),
 ( #5682, #44658 ),
 ( #83215, #57008 ),
 ( #87988, #98900 ),
 ( #95585, #18537 ),
 ( #20912, #13780 ),
 ( #82738, #87503 ),
 ( #29482, #44168 ),
 ( #79868, #49420 ),
 ( #72244, #80366 ),
 ( #4701, #75104 ),
 ( #45656, #46666 ),
 ( #68965, #61365 ),
 ( #1081, #16269 ),
 ( #15253, #76109 ),
 ( #60355, #84713 ),
 ( #6683, #52760 ),
 ( #37559, #69961 ),
 ( #576, #99888 ),
 ( #68468, #92805 ),
 ( #39049, #92321 ),
 ( #54243, #30472 ),
 ( #84, #77067 ),
 ( #69470, #22374 ),
 ( #22869, #46150 ),
 ( #31460, #8675 ),
 ( #7165, #99396 ) ),
 .UNSPECIFIED., .T., .F., .F.,
 ( 4, 2, 2, 2, 2, 2, 2, 2, 2, 2, 2, 2, 2, 2, 2, 2, 4 ),
 ( 2, 2 ),
 ( 0.000000000000000000, 0.06250000000000000000, 0.1250000000000000000, 0.1875000000000000000, 0.2500000000000000000, 0.3125000000000000000, 0.3750000000000000000, 0.4375000000000000000, 0.5000000000000000000, 0.5625000000000000000, 0.6250000000000000000, 0.6875000000000000000, 0.7500000000000000000, 0.8125000000000000000, 0.8750000000000000000, 0.9375000000000000000, 1.000000000000000000 ),
 ( 0.000000000000000000, 1.000000000000000000 ),
 .UNSPECIFIED. ) ;
#55002 = CARTESIAN_POINT ( 'NONE',  ( 34.13026518906141860, 41.74646525600392977, 2.839279412974139660 ) ) ;
#55003 = VERTEX_POINT ( 'NONE', #60637 ) ;
#55004 = CARTESIAN_POINT ( 'NONE',  ( 166.0902728679650693, 248.8705385957478882, 7.015670575385891894 ) ) ;
#55005 = CARTESIAN_POINT ( 'NONE',  ( -110.0000000000000000, 15.00000000000000000, -59.99999999999999289 ) ) ;
#55006 = CARTESIAN_POINT ( 'NONE',  ( 86.74085627840248947, 44.04483152046088179, -5.761820014970100878 ) ) ;
#55007 = ORIENTED_EDGE ( 'NONE', *, *, #27411, .T. ) ;
#55008 = CARTESIAN_POINT ( 'NONE',  ( 86.50129422937833112, 47.15573905589064196, -10.08535824937341374 ) ) ;
#55009 = LINE ( 'NONE', #10937, #26580 ) ;
#55010 = CARTESIAN_POINT ( 'NONE',  ( 163.7010375032499212, 247.1084811230698506, 6.649922295230481950 ) ) ;
#55011 = CARTESIAN_POINT ( 'NONE',  ( 84.95458848507411176, 44.42387911948991075, -8.356648915091495766 ) ) ;
#55012 = CARTESIAN_POINT ( 'NONE',  ( 84.43319883474627829, 44.99437554259058913, -9.553074584682860859 ) ) ;
#55013 = DIRECTION ( 'NONE',  ( -0.000000000000000000, -1.000000000000000000, -0.000000000000000000 ) ) ;
#55014 = ORIENTED_EDGE ( 'NONE', *, *, #30294, .F. ) ;
#55015 = ORIENTED_EDGE ( 'NONE', *, *, #16284, .T. ) ;
#55016 = CARTESIAN_POINT ( 'NONE',  ( 87.10115137904762150, 45.28340438443854055, 6.995308688534716879 ) ) ;
#55017 = VERTEX_POINT ( 'NONE', #45936 ) ;
#55018 = CARTESIAN_POINT ( 'NONE',  ( 77.16396432587895049, 49.58440764469271045, -14.97671560787508405 ) ) ;
#55019 = ORIENTED_EDGE ( 'NONE', *, *, #16168, .F. ) ;
#55020 = CARTESIAN_POINT ( 'NONE',  ( 87.20555836939593064, 45.98127448902955905, -8.722945138008007859 ) ) ;
#55021 = CARTESIAN_POINT ( 'NONE',  ( 78.65113419757746271, 50.64782171794184507, 15.07795987699981666 ) ) ;
#55022 = ORIENTED_EDGE ( 'NONE', *, *, #89571, .F. ) ;
#55023 = CARTESIAN_POINT ( 'NONE',  ( 190.3455805766996605, 300.1776048065829059, -3.435469494870868612 ) ) ;
#55024 = CARTESIAN_POINT ( 'NONE',  ( 164.2960764465929060, 246.0778434407177713, -1.520364048796653877 ) ) ;
#55025 = CARTESIAN_POINT ( 'NONE',  ( 147.5030091739506588, 275.1642891718561259, -5.824350960008994882 ) ) ;
#55026 = CARTESIAN_POINT ( 'NONE',  ( 69.81243019392553606, 62.22010195957141576, -13.63492759933605392 ) ) ;
#55027 = CARTESIAN_POINT ( 'NONE',  ( 82.24318726465129714, 40.84802034143084626, 1.047704164177056585 ) ) ;
#55028 = CARTESIAN_POINT ( 'NONE',  ( 167.6432305260580051, 249.2069326997503538, -5.439418313667148119 ) ) ;
#55029 = CARTESIAN_POINT ( 'NONE',  ( 41.71240375114938814, 62.05720181600818108, 10.00000000000000000 ) ) ;
#55030 = CARTESIAN_POINT ( 'NONE',  ( 157.7427020192611451, 281.4113889458213862, 2.901906572848928167 ) ) ;
#55031 = CARTESIAN_POINT ( 'NONE',  ( 125.3701074643745841, 249.3149278399160949, 9.188101187500093303 ) ) ;
#55032 = CARTESIAN_POINT ( 'NONE',  ( 70.58053732654904877, 60.72247144732425994, -14.55979615259335169 ) ) ;
#55033 = CARTESIAN_POINT ( 'NONE',  ( 35.53452623260358223, 35.91421378149921395, 9.188101187500008038 ) ) ;
#55034 = EDGE_CURVE ( 'NONE', #92904, #20754, #38344, .T. ) ;
#55035 = VERTEX_POINT ( 'NONE', #53056 ) ;
#55037 = ORIENTED_EDGE ( 'NONE', *, *, #19017, .T. ) ;
#55036 = LINE ( 'NONE', #70240, #3996 ) ;
#55038 = CARTESIAN_POINT ( 'NONE',  ( -35.39636583819505233, 63.79609003141229095, -10.00000000000000000 ) ) ;
#55039 = CARTESIAN_POINT ( 'NONE',  ( 178.8222888093016820, 253.5684133990675946, 1.420763099363733906 ) ) ;
#55040 = CARTESIAN_POINT ( 'NONE',  ( 49.09245556086621320, 93.56363653685789927, -10.00000000000000000 ) ) ;
#55041 = CARTESIAN_POINT ( 'NONE',  ( 147.0770520072680654, 275.9020686263983180, 2.568669615083420954 ) ) ;
#55042 = CARTESIAN_POINT ( 'NONE',  ( -19.65312891409030271, 93.06504152958497400, 25.00000000000000000 ) ) ;
#55043 = CARTESIAN_POINT ( 'NONE',  ( 80.71386657632071149, 43.15011696034207489, 9.894852039748123218 ) ) ;
#55044 = CARTESIAN_POINT ( 'NONE',  ( 171.3910097907696013, 265.7400108419894309, -17.48696717007155144 ) ) ;
#55045 = CARTESIAN_POINT ( 'NONE',  ( 174.7976338077968421, 282.4145131704060532, 14.70753238353839265 ) ) ;
#55046 = CARTESIAN_POINT ( 'NONE',  ( 19.98788723728717898, 104.4047874917408336, 22.50000000000002132 ) ) ;
#55047 = ORIENTED_EDGE ( 'NONE', *, *, #5707, .T. ) ;
#55048 = CARTESIAN_POINT ( 'NONE',  ( 200.5783178365889796, 282.7758977645278264, -16.72421819799698639 ) ) ;
#55049 = CARTESIAN_POINT ( 'NONE',  ( 152.8311844419622503, 273.8830713642822730, 12.16002972492639422 ) ) ;
#55050 = ORIENTED_EDGE ( 'NONE', *, *, #48498, .F. ) ;
#55051 = CARTESIAN_POINT ( 'NONE',  ( 81.94845728006144725, 58.78542703240049150, -0.2795964517353725087 ) ) ;
#55052 = CARTESIAN_POINT ( 'NONE',  ( 160.2823167370213184, 279.0841748587739630, 10.63415498209442589 ) ) ;
#55053 = CARTESIAN_POINT ( 'NONE',  ( 151.7203664365511031, 267.8596121193626232, -16.04302167993712658 ) ) ;
#55054 = DIRECTION ( 'NONE',  ( 0.000000000000000000, -0.000000000000000000, 1.000000000000000000 ) ) ;
#55055 = CARTESIAN_POINT ( 'NONE',  ( 199.3359313799735162, 277.8054090533971134, 16.38672730308284997 ) ) ;
#55057 = CARTESIAN_POINT ( 'NONE',  ( 154.7665789146825830, 277.6802373535633137, -9.031277582128581116 ) ) ;
#55056 = CARTESIAN_POINT ( 'NONE',  ( 162.2513340404218241, 281.9508718976948103, -6.600334769067247365 ) ) ;
#55058 = CARTESIAN_POINT ( 'NONE',  ( 48.17894221477870786, 74.75545800895066861, -10.00000000000000000 ) ) ;
#55059 = ORIENTED_EDGE ( 'NONE', *, *, #3900, .F. ) ;
#55060 = CARTESIAN_POINT ( 'NONE',  ( 190.3625087333586521, 300.9294583479858147, -4.271886578030237303 ) ) ;
#55061 = CARTESIAN_POINT ( 'NONE',  ( 163.5341610023646126, 247.8889313856435876, -8.119019177482972083 ) ) ;
#55062 = CARTESIAN_POINT ( 'NONE',  ( 190.2895893073217337, 274.5542638304875140, -15.68163590285366205 ) ) ;
#55063 = CARTESIAN_POINT ( 'NONE',  ( 84.80172950927561715, 50.19486025153374698, 13.34007759942641336 ) ) ;
#55064 = CARTESIAN_POINT ( 'NONE',  ( 168.9579038699606315, 279.3139280689009070, 15.08363371378442608 ) ) ;
#55065 = CARTESIAN_POINT ( 'NONE',  ( 200.1778674013334012, 279.3308388275589778, -16.74461585440090161 ) ) ;
#55066 = CARTESIAN_POINT ( 'NONE',  ( 74.24116255903008721, 68.58322516222325760, 11.55893809163644725 ) ) ;
#55067 = AXIS2_PLACEMENT_3D ( 'NONE', #81168, #35006, #65906 ) ;
#55068 = CARTESIAN_POINT ( 'NONE',  ( 74.13561708490506419, 68.62084109673111243, 10.97025690930964892 ) ) ;
#55069 = FACE_OUTER_BOUND ( 'NONE', #67966, .T. ) ;
#55070 = CARTESIAN_POINT ( 'NONE',  ( -16.57695564860984661, 170.4244531367911293, -4.594050593750046652 ) ) ;
#55071 = CARTESIAN_POINT ( 'NONE',  ( 93.16496130902324069, 224.5958772461660260, -9.188101187500095079 ) ) ;
#55072 = CARTESIAN_POINT ( 'NONE',  ( 203.3684377202211522, 278.4025285431072803, -16.56116267537666076 ) ) ;
#55073 = CARTESIAN_POINT ( 'NONE',  ( 147.0456760057551833, 275.9564134551570760, -3.678503029046952033 ) ) ;
#55074 = CARTESIAN_POINT ( 'NONE',  ( 182.9399940311841135, 294.6164125958089812, -8.120217072990003615 ) ) ;
#55075 = CARTESIAN_POINT ( 'NONE',  ( 155.0453531195792038, 262.1005662498678817, -18.46987289964740953 ) ) ;
#55076 = DIRECTION ( 'NONE',  ( -0.9979398670145503969, -0.06415622980647761597, 0.000000000000000000 ) ) ;
#55077 =( NAMED_UNIT ( * ) SI_UNIT ( $, .STERADIAN. ) SOLID_ANGLE_UNIT ( ) );
#55078 = CARTESIAN_POINT ( 'NONE',  ( 78.31072776954091808, 61.54348912244275027, 15.80414048699106999 ) ) ;
#55080 = CARTESIAN_POINT ( 'NONE',  ( 76.35565666213805969, 51.40178206308662823, 15.62279043926746347 ) ) ;
#55079 = FACE_OUTER_BOUND ( 'NONE', #54649, .T. ) ;
#55081 = CARTESIAN_POINT ( 'NONE',  ( 207.8404471368518216, 270.6567810215766485, 6.233406202017039099 ) ) ;
#55082 = CARTESIAN_POINT ( 'NONE',  ( 166.1201540932435705, 249.6576623637213004, -9.102047968603363515 ) ) ;
#55083 = CARTESIAN_POINT ( 'NONE',  ( 161.3351705126590332, 251.7324723637383670, 13.41138257763892305 ) ) ;
#55084 = EDGE_CURVE ( 'NONE', #81557, #36092, #80713, .T. ) ;
#55085 = CARTESIAN_POINT ( 'NONE',  ( 157.8360072705708603, 257.2670114739976839, 17.12122855844125269 ) ) ;
#55086 = FACE_OUTER_BOUND ( 'NONE', #66640, .T. ) ;
#55087 = EDGE_CURVE ( 'NONE', #70938, #88538, #36357, .T. ) ;
#55088 = CARTESIAN_POINT ( 'NONE',  ( 40.98727782677583065, 182.2202760586659451, -5.415160957724236172E-17 ) ) ;
#55089 = EDGE_CURVE ( 'NONE', #5812, #62259, #67770, .T. ) ;
#55090 = CARTESIAN_POINT ( 'NONE',  ( 64.74867629522887569, 202.0643266524159856, -9.188101187500093303 ) ) ;
#55091 = CARTESIAN_POINT ( 'NONE',  ( 27.81597692694000656, 72.50130484473876891, 59.99999999999999289 ) ) ;
#55092 = CARTESIAN_POINT ( 'NONE',  ( 88.42339661562220954, 43.82656006556687345, 0.1181016345699151954 ) ) ;
#55093 = CARTESIAN_POINT ( 'NONE',  ( 167.2881153130185794, 259.8033680499513594, 16.14645104202834602 ) ) ;
#55094 = CARTESIAN_POINT ( 'NONE',  ( 138.3604885211411499, 256.8149278399160949, 9.188101187500093303 ) ) ;
#55096 = CARTESIAN_POINT ( 'NONE',  ( 70.17810782877538145, 70.93619788462370934, -4.492011057286514841 ) ) ;
#55095 = CARTESIAN_POINT ( 'NONE',  ( 71.99279863978298977, 71.74937481526245620, -3.912420615770861865 ) ) ;
#55097 = CARTESIAN_POINT ( 'NONE',  ( 200.2305960855333353, 271.0184197120956355, -11.41732784617588692 ) ) ;
#55098 = CARTESIAN_POINT ( 'NONE',  ( 28.77833178495667710, 28.56628583063842441, 9.188101187500006262 ) ) ;
#55099 = CARTESIAN_POINT ( 'NONE',  ( 150.9003228897357189, 269.2799692068659283, -14.30003212299500781 ) ) ;
#55100 = CARTESIAN_POINT ( 'NONE',  ( 196.4808189786114951, 290.3322341467384717, -17.84817245450773271 ) ) ;
#55101 = CARTESIAN_POINT ( 'NONE',  ( 9.725772901699041739, 17.56628583063838889, 9.188101187500006262 ) ) ;
#55102 = CARTESIAN_POINT ( 'NONE',  ( 52.13666070897046012, 213.1589784336661637, -6.496448406907676862E-16 ) ) ;
#55103 = CARTESIAN_POINT ( 'NONE',  ( 76.70245435708865500, 63.85979508024991702, 14.86777658481231867 ) ) ;
#55104 = CARTESIAN_POINT ( 'NONE',  ( 155.1601726304954809, 261.9016930232608615, -18.56587418422714464 ) ) ;
#55105 = CARTESIAN_POINT ( 'NONE',  ( 159.9880386575927957, 253.5395837721924863, 15.85893018594752846 ) ) ;
#55106 = CARTESIAN_POINT ( 'NONE',  ( 69.38743239535708085, 62.82953552710814193, -13.71264069967795329 ) ) ;
#55107 = CARTESIAN_POINT ( 'NONE',  ( 201.7940041625137724, 281.1295274581978560, 16.26334312466084953 ) ) ;
#55108 = CARTESIAN_POINT ( 'NONE',  ( 107.0484310652165192, 232.6115022471902307, 10.00000000000009592 ) ) ;
#55109 = FACE_OUTER_BOUND ( 'NONE', #81743, .T. ) ;
#55110 = CARTESIAN_POINT ( 'NONE',  ( 207.6826438088389750, 270.9301044032979462, 7.252082088659585146 ) ) ;
#55111 = ORIENTED_EDGE ( 'NONE', *, *, #5774, .F. ) ;
#55112 = CARTESIAN_POINT ( 'NONE',  ( 77.17192383615090989, 49.30585512036960694, 15.39194763320842441 ) ) ;
#55113 = CARTESIAN_POINT ( 'NONE',  ( 186.9334442694681684, 272.7010231022609332, 15.66575838895225736 ) ) ;
#55114 = ORIENTED_EDGE ( 'NONE', *, *, #88231, .T. ) ;
#55115 = CARTESIAN_POINT ( 'NONE',  ( 159.5221561062548972, 254.3465160214695118, -16.91023001054109542 ) ) ;
#55116 = CARTESIAN_POINT ( 'NONE',  ( 187.1232320155474156, 276.7967530242608518, -16.86548313267018528 ) ) ;
#55117 = CARTESIAN_POINT ( 'NONE',  ( 71.40939848415580116, 68.88699701054706281, -8.787086014537564438 ) ) ;
#55118 = EDGE_LOOP ( 'NONE', ( #61648, #50646, #89354, #77255 ) ) ;
#55119 = CARTESIAN_POINT ( 'NONE',  ( 177.2864851724368123, 253.0591412921742176, -0.2646061339184051509 ) ) ;
#55120 = ORIENTED_EDGE ( 'NONE', *, *, #11455, .T. ) ;
#55121 = CARTESIAN_POINT ( 'NONE',  ( 72.46511837996447980, 71.56249752072032777, 6.234640293157904800 ) ) ;
#55122 = CARTESIAN_POINT ( 'NONE',  ( 194.9819925439454664, 292.9282776833073285, -15.33279721168237586 ) ) ;
#55123 = CARTESIAN_POINT ( 'NONE',  ( 148.6500818154487433, 275.1775010768142238, 7.719411301773694944 ) ) ;
#55124 = ORIENTED_EDGE ( 'NONE', *, *, #73409, .T. ) ;
#55125 = CARTESIAN_POINT ( 'NONE',  ( 30.72569264534336142, 26.24335787977765122, -9.188101187500008038 ) ) ;
#55126 = CARTESIAN_POINT ( 'NONE',  ( 155.4246291545472616, 271.4210554887007447, -15.13027500041984830 ) ) ;
#55127 = CARTESIAN_POINT ( 'NONE',  ( 74.84872400778056090, 66.80276697526576868, -13.19923776164384677 ) ) ;
#55128 = VERTEX_POINT ( 'NONE', #46957 ) ;
#55129 = CARTESIAN_POINT ( 'NONE',  ( 130.8641296692885305, 256.3615022471903444, 5.000000000000046185 ) ) ;
#55130 = CARTESIAN_POINT ( 'NONE',  ( 163.6530677658052753, 285.1143415345633230, 4.800695543634067697 ) ) ;
#55131 = ORIENTED_EDGE ( 'NONE', *, *, #54249, .T. ) ;
#55132 = AXIS2_PLACEMENT_3D ( 'NONE', #89825, #57382, #49788 ) ;
#55133 = DIRECTION ( 'NONE',  ( -1.000000000000000000, 0.000000000000000000, 0.000000000000000000 ) ) ;
#55135 = CARTESIAN_POINT ( 'NONE',  ( 68.04520307338094653, 65.58168358224989447, -10.28824799336666374 ) ) ;
#55134 = CARTESIAN_POINT ( 'NONE',  ( 68.07556148176628597, 65.74332760699670075, 10.87905400252346588 ) ) ;
#55136 = B_SPLINE_CURVE_WITH_KNOTS ( 'NONE', 3,
 ( #91633, #53094, #22200, #98223, #21216, #28294, #14607, #45485, #91140, #4502, #83041, #36895, #29311, #35402, #59169, #60175, #97242, #90144, #21703, #83543, #89657, #82052, #14107, #28805, #13614, #20720, #67805, #98731, #22707, #78413, #47488 ),
 .UNSPECIFIED., .F., .F.,
 ( 4, 3, 3, 3, 3, 3, 3, 3, 3, 3, 4 ),
 ( 0.000000000000000000, 3.357709145156459696E-05, 6.715417940116844182E-05, 0.0001007313198657331928, 0.0001343084960840520677, 0.0001678856156954599166, 0.0002014626747008569686, 0.0002350397637044858380, 0.0002686169264846224240, 0.0003021940916574071827, 0.0003125816342522696090 ),
 .UNSPECIFIED. ) ;
#55137 = CARTESIAN_POINT ( 'NONE',  ( 166.9078262434662747, 265.1710354609668912, -17.73982523066521821 ) ) ;
#55138 = CARTESIAN_POINT ( 'NONE',  ( 193.7901930790854976, 294.9925349088783264, 14.24765323155741115 ) ) ;
#55139 = CARTESIAN_POINT ( 'NONE',  ( 69.93330931759959412, 71.50341667604121199, 8.155205941333377477E-06 ) ) ;
#55140 = CARTESIAN_POINT ( 'NONE',  ( 205.2941531242069857, 275.0670916224857478, -13.92605142593109058 ) ) ;
#55141 = FACE_OUTER_BOUND ( 'NONE', #49346, .T. ) ;
#55142 = CARTESIAN_POINT ( 'NONE',  ( 69.81582973455007846, 63.14295414310246457, -13.67321376818635059 ) ) ;
#55143 = CARTESIAN_POINT ( 'NONE',  ( 182.1143333712344656, 260.2409841647984763, 9.281406274060142181 ) ) ;
#55144 = CARTESIAN_POINT ( 'NONE',  ( 94.11243691623624841, 215.9548013555409796, -4.594050593750042211 ) ) ;
#55145 = ORIENTED_EDGE ( 'NONE', *, *, #92202, .T. ) ;
#55146 = CARTESIAN_POINT ( 'NONE',  ( 191.5694459269389824, 298.8389818071599962, 7.944420692511652504 ) ) ;
#55147 = CARTESIAN_POINT ( 'NONE',  ( 181.4954090331713417, 255.0423029034424189, 0.9094182891644410072 ) ) ;
#55148 = EDGE_CURVE ( 'NONE', #43596, #17546, #78154, .T. ) ;
#55149 = ORIENTED_EDGE ( 'NONE', *, *, #81005, .T. ) ;
#55150 = CARTESIAN_POINT ( 'NONE',  ( 196.0371429460125796, 291.1007035773004645, -15.98343019695849776 ) ) ;
#55151 = VERTEX_POINT ( 'NONE', #39333 ) ;
#55152 = CARTESIAN_POINT ( 'NONE',  ( 79.90892646165700341, 44.66511174005920992, -11.18539793377209257 ) ) ;
#55153 = DIRECTION ( 'NONE',  ( 0.000000000000000000, 0.000000000000000000, 1.000000000000000000 ) ) ;
#55154 = CARTESIAN_POINT ( 'NONE',  ( 25.88687446534342129, 117.6066667404749069, 59.99999999999999289 ) ) ;
#55155 = DIRECTION ( 'NONE',  ( -0.7299047266382376886, 0.6835488936653759673, 0.000000000000000000 ) ) ;
#55156 = CARTESIAN_POINT ( 'NONE',  ( 83.36082971782188622, 47.63437754184118944, -12.10617920438150463 ) ) ;
#55157 = CARTESIAN_POINT ( 'NONE',  ( 162.8493988834005677, 248.5835624823365322, 11.81438570587263470 ) ) ;
#55158 = CARTESIAN_POINT ( 'NONE',  ( 87.26533679362427165, 215.0643266524160140, 9.188101187500095079 ) ) ;
#55159 = VERTEX_POINT ( 'NONE', #54528 ) ;
#55161 = EDGE_CURVE ( 'NONE', #47416, #13304, #10506, .T. ) ;
#55160 = B_SPLINE_CURVE_WITH_KNOTS ( 'NONE', 3,
 ( #99793, #21779, #7073, #91718, #46056, #54152, #15666, #77495, #76972, #61265, #13690, #98810, #68375, #69376, #51061, #83625, #8088, #44564, #60260, #29391, #52171, #6592, #30879, #69869, #14190, #53181, #92234, #45075, #7575, #22785, #21297, #75499, #76014, #61766, #92713, #23263, #37466, #99300, #59771, #53662, #85114, #6083, #84136, #36976, #28894, #29880 ),
 .UNSPECIFIED., .F., .F.,
 ( 4, 1, 1, 1, 2, 2, 1, 1, 1, 2, 2, 1, 1, 2, 2, 1, 1, 2, 2, 1, 1, 2, 2, 1, 2, 2, 1, 2, 2, 4 ),
 ( 0.000000000000000000, 0.06249999999998717692, 0.09374999999998123723, 0.1093749999999801131, 0.1171874999999796552, 0.1249999999999792111, 0.1874999999999961142, 0.2187500000000023037, 0.2343750000000030809, 0.2421875000000033862, 0.2500000000000036637, 0.3125000000000207057, 0.3437500000000268119, 0.3593750000000282552, 0.3750000000000296430, 0.4375000000000286993, 0.4687500000000277001, 0.4843750000000258127, 0.5000000000000238698, 0.5625000000000197620, 0.5937500000000172085, 0.6093750000000150990, 0.6250000000000129896, 0.6875000000000106581, 0.7187500000000082157, 0.7500000000000056621, 0.8125000000000015543, 0.8437500000000018874, 0.8750000000000021094, 1.000000000000000000 ),
 .UNSPECIFIED. ) ;
#55162 = ORIENTED_EDGE ( 'NONE', *, *, #93233, .T. ) ;
#55163 = CARTESIAN_POINT ( 'NONE',  ( 208.3829315663354862, 269.7171704273955015, -1.768817828503133072 ) ) ;
#55164 = EDGE_LOOP ( 'NONE', ( #58998, #52427, #39945, #9295 ) ) ;
#55165 = EDGE_CURVE ( 'NONE', #38435, #39058, #95249, .T. ) ;
#55166 = LINE ( 'NONE', #3388, #62869 ) ;
#55167 = CARTESIAN_POINT ( 'NONE',  ( 183.8037341582430884, 275.4624792557407318, 17.77592483611231700 ) ) ;
#55168 = CARTESIAN_POINT ( 'NONE',  ( 20.07045957425421179, 33.36126292948895866, 6.180339887498949913 ) ) ;
#55169 = CARTESIAN_POINT ( 'NONE',  ( 189.6768609436964539, 274.4077930505946483, -17.07046811116321550 ) ) ;
#55170 = CARTESIAN_POINT ( 'NONE',  ( 84.99999999999997158, 27.49999999999999645, 59.99999999999999289 ) ) ;
#55171 = CARTESIAN_POINT ( 'NONE',  ( 88.02768100692024689, 44.78812371456486119, 4.666884733071423597 ) ) ;
#55172 = ORIENTED_EDGE ( 'NONE', *, *, #48465, .F. ) ;
#55173 = CARTESIAN_POINT ( 'NONE',  ( 157.6466783816650832, 259.5949387289228412, 17.71616314254395519 ) ) ;
#55174 = CARTESIAN_POINT ( 'NONE',  ( 185.0706190396982151, 260.1753711840241863, 6.321521495746559971 ) ) ;
#55175 = CARTESIAN_POINT ( 'NONE',  ( 159.3451320108506764, 254.6531307488737355, -16.72997986213134425 ) ) ;
#55176 = CARTESIAN_POINT ( 'NONE',  ( 148.1295332417885504, 275.8061709343286907, -5.314593380240301812 ) ) ;
#55177 = CARTESIAN_POINT ( 'NONE',  ( 174.7897835487166276, 284.0530019150879184, 13.84973856136962844 ) ) ;
#55178 = CARTESIAN_POINT ( 'NONE',  ( 198.7291624623985058, 284.6509008601083224, -17.69774185455217008 ) ) ;
#55179 = CARTESIAN_POINT ( 'NONE',  ( 73.07159975088246995, 72.16059528448882077, 0.000000000000000000 ) ) ;
#55180 = ORIENTED_EDGE ( 'NONE', *, *, #28094, .F. ) ;
#55181 = CARTESIAN_POINT ( 'NONE',  ( 7.819191540449072164, 28.68125778831126382, 10.00000000000000000 ) ) ;
#55182 =( BOUNDED_CURVE ( )  B_SPLINE_CURVE ( 2, ( #985, #87158, #48591, #32382, #18193, #86148, #9603, #39957, #86641 ),
 .UNSPECIFIED., .F., .T. ) 
 B_SPLINE_CURVE_WITH_KNOTS ( ( 3, 2, 2, 2, 3 ),
 ( 0.8104838709677418818, 0.8118279569892472569, 0.8145161290322581182, 0.8172043010752688685, 0.8185483870967742437 ),
 .UNSPECIFIED. ) 
 CURVE ( )  GEOMETRIC_REPRESENTATION_ITEM ( )  RATIONAL_B_SPLINE_CURVE ( ( 0.9330127018922194093, 0.9330127018922194093, 1.000000000000000000, 0.8660254037844387076, 1.000000000000000000, 0.8660254037844387076, 1.000000000000000000, 0.9330127018922194093, 0.9330127018922194093 ) ) 
 REPRESENTATION_ITEM ( '' )  );
#55183 = CARTESIAN_POINT ( 'NONE',  ( 161.8948331661419218, 250.2369188037922356, 13.64419044796309777 ) ) ;
#55184 = DIRECTION ( 'NONE',  ( -0.8660254037844377084, -0.5000000000000014433, -0.000000000000000000 ) ) ;
#55185 = CARTESIAN_POINT ( 'NONE',  ( 185.8323446419325364, 264.8229110950202880, -11.92140045508744883 ) ) ;
#55186 = CARTESIAN_POINT ( 'NONE',  ( 83.34567255814403097, 52.40788958926237484, 14.85282737495174565 ) ) ;
#55187 = CARTESIAN_POINT ( 'NONE',  ( 156.8397658254749842, 272.7276435997338808, 14.63702169103162731 ) ) ;
#55188 = VERTEX_POINT ( 'NONE', #97939 ) ;
#55189 = LINE ( 'NONE', #62287, #1357 ) ;
#55190 = CARTESIAN_POINT ( 'NONE',  ( 207.2824254892180704, 271.6233028670009162, 6.274396967990798046 ) ) ;
#55192 = CARTESIAN_POINT ( 'NONE',  ( 73.60674897234599712, 55.48729869333283204, 16.10905085971090145 ) ) ;
#55191 = CARTESIAN_POINT ( 'NONE',  ( 154.9910882912764123, 262.1945556895526579, 18.38052604520346023 ) ) ;
#55193 = CARTESIAN_POINT ( 'NONE',  ( 175.7824178399792174, 285.8628427244275372, -13.39878279634721103 ) ) ;
#55194 = EDGE_CURVE ( 'NONE', #59100, #33383, #5230, .T. ) ;
#55195 = CARTESIAN_POINT ( 'NONE',  ( 28.91364825607195144, 28.64441083166262203, -10.00000000000000533 ) ) ;
#55196 = CARTESIAN_POINT ( 'NONE',  ( 164.9031621293093508, 284.7306714147449611, -3.125257715394198055 ) ) ;
#55197 = DIRECTION ( 'NONE',  ( -0.4525327339300165286, 0.8917477921037005872, 0.000000000000000000 ) ) ;
#55198 = AXIS2_PLACEMENT_3D ( 'NONE', #38576, #15775, #69483 ) ;
#55199 = CARTESIAN_POINT ( 'NONE',  ( 189.3293204741634383, 297.6371524027489954, -9.350876801542840511 ) ) ;
#55200 = CARTESIAN_POINT ( 'NONE',  ( -5.751638101304356709, 176.6744531367911293, 4.594050593750047540 ) ) ;
#55201 = LINE ( 'NONE', #61312, #16089 ) ;
#55202 = ORIENTED_EDGE ( 'NONE', *, *, #24676, .F. ) ;
#55203 = EDGE_CURVE ( 'NONE', #86003, #80773, #18574, .T. ) ;
#55204 = EDGE_CURVE ( 'NONE', #14940, #12306, #93244, .T. ) ;
#55205 = CARTESIAN_POINT ( 'NONE',  ( 174.8650114509604521, 255.3214838289419788, 8.489119280892019503 ) ) ;
#55206 = CARTESIAN_POINT ( 'NONE',  ( 183.0423515620436490, 268.5971907196498023, -16.46882057410648414 ) ) ;
#55207 = CARTESIAN_POINT ( 'NONE',  ( 194.5253693406981483, 291.7191722712467481, 16.18900132190417551 ) ) ;
#55208 = CARTESIAN_POINT ( 'NONE',  ( 81.62374368218520715, 41.76230689378203209, 5.959470817902195350 ) ) ;
#55209 = CARTESIAN_POINT ( 'NONE',  ( 20.58103360645747770, 188.8149278399160949, -9.188101187500095079 ) ) ;
#55210 = CYLINDRICAL_SURFACE ( 'NONE', #18410, 16.60714546451156792 ) ;
#55211 = CARTESIAN_POINT ( 'NONE',  ( 32.62753302031853053, 27.03677371833804344, 10.00000000000000533 ) ) ;
#55212 = CARTESIAN_POINT ( 'NONE',  ( 86.04792660047165498, 42.90958022930985294, -0.1400070824457408381 ) ) ;
#55213 = CARTESIAN_POINT ( 'NONE',  ( 146.9456733906991417, 276.1296230653242105, -0.7988785540157754550 ) ) ;
#55214 = CARTESIAN_POINT ( 'NONE',  ( 81.37941775519415444, 56.13859199581248305, 16.08349135110547579 ) ) ;
#55215 = CARTESIAN_POINT ( 'NONE',  ( 87.06060708477828314, 46.38825358833559420, -8.733779054531098041 ) ) ;
#55216 = CARTESIAN_POINT ( 'NONE',  ( 190.9034043754504921, 261.7470625323397826, -1.404837864312324935 ) ) ;
#55217 = CARTESIAN_POINT ( 'NONE',  ( 41.47569090598247499, 209.1868197944957899, 17.47570218321535762 ) ) ;
#55218 = CARTESIAN_POINT ( 'NONE',  ( 59.05618993882879408, 218.2365022471903444, 2.944929066748280225E-16 ) ) ;
#55219 = CARTESIAN_POINT ( 'NONE',  ( 73.62564376992710891, 66.16305478508047599, -12.64589907936473701 ) ) ;
#55220 = LINE ( 'NONE', #1048, #56284 ) ;
#55221 = CARTESIAN_POINT ( 'NONE',  ( 32.46173284068399312, 198.7369531367911293, -4.594050593750048428 ) ) ;
#55222 = CYLINDRICAL_SURFACE ( 'NONE', #63394, 10.00000000000010658 ) ;
#55223 = CARTESIAN_POINT ( 'NONE',  ( 203.5726949774746117, 269.0034548673361883, -6.096665150295551783 ) ) ;
#55224 = CARTESIAN_POINT ( 'NONE',  ( -19.65312891409030271, 93.06504152958497400, 177.5919119679930134 ) ) ;
#55225 = CARTESIAN_POINT ( 'NONE',  ( -78.71521058394759507, 57.86724000996476747, -10.00000000000000000 ) ) ;
#55226 = DIRECTION ( 'NONE',  ( -0.5634352399127678934, -0.8261602328994307465, 0.000000000000000000 ) ) ;
#55227 = CARTESIAN_POINT ( 'NONE',  ( 202.6275056595488593, 279.1946885124775690, -15.35640559527740123 ) ) ;
#55228 = CARTESIAN_POINT ( 'NONE',  ( 205.9961433675841818, 269.8120887608272369, -1.317021689134348250 ) ) ;
#55229 = CARTESIAN_POINT ( 'NONE',  ( 19.86428432551159418, 29.65586893147756342, -7.433330006724137462 ) ) ;
#55230 = CARTESIAN_POINT ( 'NONE',  ( 202.9972156839127990, 279.0455039708822937, 16.77197898838388213 ) ) ;
#55231 = CARTESIAN_POINT ( 'NONE',  ( 196.9098758191317700, 289.5890858996224324, -16.54412079817003800 ) ) ;
#55232 = CARTESIAN_POINT ( 'NONE',  ( 175.3120577001922413, 257.3065038543072660, 11.69806524060765973 ) ) ;
#55233 = VERTEX_POINT ( 'NONE', #51832 ) ;
#55234 = CARTESIAN_POINT ( 'NONE',  ( 14.00658445089738180, 13.80170272979924917, 7.433330006724137462 ) ) ;
#55235 = B_SPLINE_CURVE_WITH_KNOTS ( 'NONE', 3,
 ( #31233, #91578, #91092, #22150, #53041, #83998, #30753, #343, #68739, #37833, #70234, #99662, #60130, #84977, #83490, #46424, #21658, #62119, #52540, #37338, #30248, #68240, #14056, #44936, #99164, #14560, #15523, #76370, #77349, #7956, #16041, #61131, #45435, #22652, #38830, #93067, #53536, #15030, #45922, #69736, #23621, #46943, #39317, #94580, #49439, #64143, #2875, #26152 ),
 .UNSPECIFIED., .F., .F.,
 ( 4, 2, 2, 2, 2, 2, 2, 2, 2, 2, 2, 2, 2, 2, 2, 2, 2, 2, 2, 2, 2, 2, 2, 4 ),
 ( 0.0005391196255988237344, 0.0009791966357432153358, 0.001199235140815413034, 0.001309254393351469165, 0.001419273645887525297, 0.001529292898423581862, 0.001639312150959637993, 0.001859350656031800563, 0.002299427666176084937, 0.003179581686464589500, 0.004059735706753093629, 0.004939889727041598191, 0.005379966737185807105, 0.005600005242257832631, 0.005710024494793798991, 0.005765034121061732297, 0.005820043747329665604, 0.005875053373597598910, 0.005930062999865532217, 0.006040082252401401432, 0.006260120757473031441, 0.006700197767616386871, 0.007140274777759743167, 0.007580351787903099464 ),
 .UNSPECIFIED. ) ;
#55236 = B_SPLINE_CURVE_WITH_KNOTS ( 'NONE', 3,
 ( #34123, #9314, #100159, #30745 ),
 .UNSPECIFIED., .F., .F.,
 ( 4, 4 ),
 ( 0.0003686392678639645488, 0.008300137104892135742 ),
 .UNSPECIFIED. ) ;
#55237 = DIRECTION ( 'NONE',  ( -0.9682419296822741828, -0.2500151307524129951, 0.000000000000000000 ) ) ;
#55238 = CARTESIAN_POINT ( 'NONE',  ( 78.70532132115687318, 57.84908500555658861, -16.23223772817032895 ) ) ;
#55239 = CARTESIAN_POINT ( 'NONE',  ( 71.56491451745446852, 72.38511813685279606, -1.315970478074329764 ) ) ;
#55240 = ORIENTED_EDGE ( 'NONE', *, *, #15635, .T. ) ;
#55241 = CARTESIAN_POINT ( 'NONE',  ( 17.25242200676955306, 190.7677522451419065, -5.000000000000047962 ) ) ;
#55242 = CARTESIAN_POINT ( 'NONE',  ( 169.4692019312130924, 260.3030467232334786, 16.29845513612216479 ) ) ;
#55243 = CARTESIAN_POINT ( 'NONE',  ( 151.2455280670316711, 268.6820563007532314, 14.35914944935941229 ) ) ;
#55244 = DIRECTION ( 'NONE',  ( 0.4924038765061026779, -0.8528685319524446085, -0.1736481776669273058 ) ) ;
#55245 = ORIENTED_EDGE ( 'NONE', *, *, #12679, .F. ) ;
#55246 = VERTEX_POINT ( 'NONE', #12851 ) ;
#55248 = CARTESIAN_POINT ( 'NONE',  ( 85.10720402821901587, 42.81679804039411152, -3.423875221259823132 ) ) ;
#55247 = CARTESIAN_POINT ( 'NONE',  ( -59.87889494062799400, 37.30571521936384016, -10.00000000000000000 ) ) ;
#55249 = EDGE_LOOP ( 'NONE', ( #16644, #32097, #40996 ) ) ;
#55250 = CARTESIAN_POINT ( 'NONE',  ( 200.9061540366740246, 282.6673289856585143, -18.13083321883407351 ) ) ;
#55251 = CARTESIAN_POINT ( 'NONE',  ( 72.01443008256866563, 72.40752555085421704, -2.913864408233449943 ) ) ;
#55252 = CARTESIAN_POINT ( 'NONE',  ( 80.08571567400755953, 57.73203133054578018, 16.60244124437337732 ) ) ;
#55253 = CARTESIAN_POINT ( 'NONE',  ( 2.922271288615635232, 25.18528772668515714, -1.583844403245363130 ) ) ;
#55254 = CARTESIAN_POINT ( 'NONE',  ( 189.9457600613112902, 301.6512882219586800, 0.04117870562599101891 ) ) ;
#55255 = CARTESIAN_POINT ( 'NONE',  ( 183.7220472628443986, 289.6844837637199817, -13.20203550471168441 ) ) ;
#55256 = ADVANCED_FACE ( 'NONE', ( #75627 ), #75139, .T. ) ;
#55257 = VERTEX_POINT ( 'NONE', #97451 ) ;
#55258 = CARTESIAN_POINT ( 'NONE',  ( 176.8860313499903612, 264.3628659159850827, -16.20694568242408806 ) ) ;
#55259 = CARTESIAN_POINT ( 'NONE',  ( 161.8978992285310312, 267.0481668204226366, 16.51610106046594595 ) ) ;
#55260 = VERTEX_POINT ( 'NONE', #89865 ) ;
#55261 = CARTESIAN_POINT ( 'NONE',  ( 23.56475526289127842, 35.64646525600391413, -2.839279412974133887 ) ) ;
#55262 = CARTESIAN_POINT ( 'NONE',  ( 159.5764336135613632, 254.2525046211064819, 15.32981087583629076 ) ) ;
#55263 = CARTESIAN_POINT ( 'NONE',  ( 78.36395837149908061, 47.99321896167455748, -14.02406508485639591 ) ) ;
#55264 = EDGE_CURVE ( 'NONE', #38929, #43160, #37109, .T. ) ;
#55265 = CARTESIAN_POINT ( 'NONE',  ( 59.71473008784930414, 205.2833772461660828, -9.188101187500095079 ) ) ;
#55266 = ORIENTED_EDGE ( 'NONE', *, *, #56721, .F. ) ;
#55267 = CARTESIAN_POINT ( 'NONE',  ( 74.28707621773548908, 68.55768173149772338, 11.60544092197708643 ) ) ;
#55268 = PLANE ( 'NONE',  #95193 ) ;
#55269 = CARTESIAN_POINT ( 'NONE',  ( 150.3737790450080354, 270.1919698983467697, 15.09624067603409969 ) ) ;
#55270 = CARTESIAN_POINT ( 'NONE',  ( 173.4413173480490400, 271.4189269517506204, 16.42543431503443330 ) ) ;
#55271 = VECTOR ( 'NONE', #40165, 1000.000000000000000 ) ;
#55272 = EDGE_LOOP ( 'NONE', ( #94068, #30988, #92452, #12727 ) ) ;
#55273 = CARTESIAN_POINT ( 'NONE',  ( 87.05908908046527017, 46.44005007060783186, 8.820244186435306943 ) ) ;
#55274 = DIRECTION ( 'NONE',  ( -0.5696381972391160176, 0.8218955677251033043, 0.000000000000000000 ) ) ;
#55275 = CARTESIAN_POINT ( 'NONE',  ( 198.2505066714982149, 285.2670451491296149, 0.000000000000000000 ) ) ;
#55276 = ORIENTED_EDGE ( 'NONE', *, *, #31896, .F. ) ;
#55277 = CARTESIAN_POINT ( 'NONE',  ( 171.7283412409539665, 259.5113726030776888, -13.85753488430609615 ) ) ;
#55278 = CARTESIAN_POINT ( 'NONE',  ( -19.65312891409030271, 93.06504152958497400, -10.00000000000000888 ) ) ;
#55279 = EDGE_CURVE ( 'NONE', #11410, #86862, #66524, .T. ) ;
#55280 = CARTESIAN_POINT ( 'NONE',  ( 161.7767236248226084, 250.4414905302161287, -13.15904643207033153 ) ) ;
#55281 = CARTESIAN_POINT ( 'NONE',  ( 192.6247335881259630, 297.0111699613833594, -13.30158778996737290 ) ) ;
#55283 = CYLINDRICAL_SURFACE ( 'NONE', #99569, 17.82106496071139645 ) ;
#55282 = B_SPLINE_CURVE_WITH_KNOTS ( 'NONE', 3,
 ( #96798, #4544, #60216, #28852 ),
 .UNSPECIFIED., .F., .F.,
 ( 4, 4 ),
 ( 0.001595800230172596777, 0.002938264775114524108 ),
 .UNSPECIFIED. ) ;
#55284 = CARTESIAN_POINT ( 'NONE',  ( 179.4583960273904211, 270.4090523040318885, 17.47970616590194837 ) ) ;
#55285 = CARTESIAN_POINT ( 'NONE',  ( 205.7867067512454184, 274.2139637150027056, 10.62737868262404106 ) ) ;
#55286 = CARTESIAN_POINT ( 'NONE',  ( 67.68928581972274117, 66.81561979556911979, 8.564295838791961657 ) ) ;
#55287 = CARTESIAN_POINT ( 'NONE',  ( 72.10195331805068975, 65.17544479578212702, -12.67587372250991073 ) ) ;
#55288 = CARTESIAN_POINT ( 'NONE',  ( 207.6172352878830907, 271.0433952848413810, 3.316653249540578496 ) ) ;
#55289 = CARTESIAN_POINT ( 'NONE',  ( 108.9159718882352479, 227.5643266524159856, -9.188101187500093303 ) ) ;
#55290 = VERTEX_POINT ( 'NONE', #5717 ) ;
#55291 = CARTESIAN_POINT ( 'NONE',  ( 190.2298193533280255, 301.1592830958237528, -4.701752374740866713 ) ) ;
#55292 = CARTESIAN_POINT ( 'NONE',  ( 84.68093819348166562, 42.16537887657799644, 0.2499978311480390847 ) ) ;
#55293 = EDGE_CURVE ( 'NONE', #23145, #68627, #52837, .T. ) ;
#55294 = CARTESIAN_POINT ( 'NONE',  ( 154.9067123643522734, 262.3406990819208886, -18.18534662427576265 ) ) ;
#55295 = EDGE_CURVE ( 'NONE', #9320, #76847, #67512, .T. ) ;
#55296 = CARTESIAN_POINT ( 'NONE',  ( 164.1224127655298730, 246.3786377597482158, 7.356982420601481998 ) ) ;
#55297 = LINE ( 'NONE', #94359, #7806 ) ;
#55298 = FACE_OUTER_BOUND ( 'NONE', #75230, .T. ) ;
#55299 = EDGE_LOOP ( 'NONE', ( #3338, #70083, #20904, #8950 ) ) ;
#55300 = CARTESIAN_POINT ( 'NONE',  ( 207.6050568035884680, 271.0644890383991310, -1.456818755242089702 ) ) ;
#55301 = CARTESIAN_POINT ( 'NONE',  ( 168.4888447738411230, 284.0319032102881351, -11.26574698934179253 ) ) ;
#55302 = CARTESIAN_POINT ( 'NONE',  ( 182.4502886106904214, 259.6876753163259650, 10.69873880494191631 ) ) ;
#55303 = LINE ( 'NONE', #62403, #5585 ) ;
#55304 = CARTESIAN_POINT ( 'NONE',  ( 133.4351425849996531, 247.8458772461660544, 9.188101187500095079 ) ) ;
#55305 = CARTESIAN_POINT ( 'NONE',  ( 150.6626254231123880, 269.6916732958875969, -15.32062296289003811 ) ) ;
#55306 = CARTESIAN_POINT ( 'NONE',  ( 185.7479194277017882, 296.9610668245633178, 4.257868302861396614 ) ) ;
#55307 = CARTESIAN_POINT ( 'NONE',  ( 157.6286460899086137, 257.6261715744221306, 18.25526781158026779 ) ) ;
#55308 = CARTESIAN_POINT ( 'NONE',  ( 38.65784837781280459, 56.65029301956751340, -10.00000000000000000 ) ) ;
#55309 = CARTESIAN_POINT ( 'NONE',  ( 45.10055139898691579, 196.8458772461660544, 9.188101187500095079 ) ) ;
#55310 = VECTOR ( 'NONE', #65358, 999.9999999999998863 ) ;
#55311 = CARTESIAN_POINT ( 'NONE',  ( 85.45699573997251264, 48.32332763657781527, -12.23527099237751692 ) ) ;
#55312 = ORIENTED_EDGE ( 'NONE', *, *, #98662, .T. ) ;
#55313 = CARTESIAN_POINT ( 'NONE',  ( 71.38293444274448518, 64.54152340162306700, 12.82260361281191052 ) ) ;
#55314 = CARTESIAN_POINT ( 'NONE',  ( 88.05520221916579260, 44.74357708579884019, -4.473609059958596035 ) ) ;
#55315 = EDGE_CURVE ( 'NONE', #73229, #81234, #57631, .T. ) ;
#55316 = B_SPLINE_SURFACE_WITH_KNOTS ( 'NONE', 3, 1, ( 
 ( #65893, #58777 ),
 ( #13702, #82153 ),
 ( #59269, #3623 ),
 ( #96848, #74527 ),
 ( #90247, #28909 ),
 ( #34991, #20819 ),
 ( #12725, #75015 ),
 ( #82658, #13217 ),
 ( #73030, #44076 ),
 ( #90751, #21305 ),
 ( #36487, #52181 ),
 ( #83130, #34501 ),
 ( #96344, #26911 ),
 ( #57790, #88769 ),
 ( #50202, #11721 ),
 ( #73516, #61279 ),
 ( #77507, #69878 ),
 ( #85645, #30388 ),
 ( #69387, #15675 ),
 ( #23273, #93218 ),
 ( #85125, #46569 ),
 ( #91224, #8098 ),
 ( #22793, #14199 ),
 ( #91724, #21792 ),
 ( #53190, #44574 ),
 ( #53672, #38474 ),
 ( #492, #31379 ),
 ( #6600, #84626 ),
 ( #52676, #75508 ),
 ( #45088, #68384 ),
 ( #22289, #62264 ),
 ( #23777, #6094 ),
 ( #36988, #76022 ),
 ( #98820, #29400 ) ),
 .UNSPECIFIED., .T., .F., .F.,
 ( 4, 2, 2, 2, 2, 2, 2, 2, 2, 2, 2, 2, 2, 2, 2, 2, 4 ),
 ( 2, 2 ),
 ( 0.000000000000000000, 0.06250000000000000000, 0.1250000000000000000, 0.1875000000000000000, 0.2500000000000000000, 0.3125000000000000000, 0.3750000000000000000, 0.4375000000000000000, 0.5000000000000000000, 0.5625000000000000000, 0.6250000000000000000, 0.6875000000000000000, 0.7500000000000000000, 0.8125000000000000000, 0.8750000000000000000, 0.9375000000000000000, 1.000000000000000000 ),
 ( 0.000000000000000000, 1.000000000000000000 ),
 .UNSPECIFIED. ) ;
#55317 = CARTESIAN_POINT ( 'NONE',  ( 70.35757334106033056, 70.80882110823974074, -3.685191203022120110 ) ) ;
#55318 = CARTESIAN_POINT ( 'NONE',  ( -61.64759997997268925, 36.73658404823907375, -10.00000000000000000 ) ) ;
#55319 = CARTESIAN_POINT ( 'NONE',  ( 82.25840028038837204, 41.50685769110872769, -5.875242208777979869 ) ) ;
#55320 = CARTESIAN_POINT ( 'NONE',  ( 203.3041373168503299, 278.5139001086923827, -16.61929732091214973 ) ) ;
#55321 = CARTESIAN_POINT ( 'NONE',  ( 8.888801338793459905, 187.4860189848785410, -2.679491924311252493 ) ) ;
#55322 = EDGE_CURVE ( 'NONE', #83827, #41296, #28619, .T. ) ;
#55323 = CARTESIAN_POINT ( 'NONE',  ( 121.6806519464431773, 234.3927522451418213, 10.00000000000009592 ) ) ;
#55324 = AXIS2_PLACEMENT_3D ( 'NONE', #72716, #3305, #34185 ) ;
#55325 = CARTESIAN_POINT ( 'NONE',  ( 79.99999999999998579, 9.999999999999985789, 54.99999999999999289 ) ) ;
#55326 = ORIENTED_EDGE ( 'NONE', *, *, #59547, .T. ) ;
#55327 = EDGE_CURVE ( 'NONE', #12886, #77358, #68013, .T. ) ;
#55328 = CARTESIAN_POINT ( 'NONE',  ( 162.9148248802443106, 248.4702413316674381, 9.709394404200100581 ) ) ;
#55329 = CARTESIAN_POINT ( 'NONE',  ( -22.42236680055709641, 157.8615022471902591, 0.000000000000000000 ) ) ;
#55330 = CARTESIAN_POINT ( 'NONE',  ( 33.73396797431614402, 190.2833772461660544, -9.188101187500095079 ) ) ;
#55331 = CARTESIAN_POINT ( 'NONE',  ( 12.72979851930235107, 19.30066082961420548, -10.00000000000000533 ) ) ;
#55332 = DIRECTION ( 'NONE',  ( -1.000000000000000000, 0.000000000000000000, 0.000000000000000000 ) ) ;
#55333 = CARTESIAN_POINT ( 'NONE',  ( 190.1752790837055045, 301.2537496138681945, -5.177773110520776711 ) ) ;
#55334 = CARTESIAN_POINT ( 'NONE',  ( 72.08669722957829151, 72.05604182950044390, 2.885689024754199306 ) ) ;
#55335 = ADVANCED_FACE ( 'NONE', ( #95618 ), #98340, .T. ) ;
#55337 = CARTESIAN_POINT ( 'NONE',  ( 53.12030748017507165, 208.1427522451419350, 10.00000000000009237 ) ) ;
#55336 = CARTESIAN_POINT ( 'NONE',  ( 4.150881819241740267, 21.13478043621385538, 8.090169943749478065 ) ) ;
#55338 = CARTESIAN_POINT ( 'NONE',  ( 128.2864073861747727, 233.3262482093457493, 3.021315404115420679E-15 ) ) ;
#55339 = CARTESIAN_POINT ( 'NONE',  ( 184.4818116536155514, 257.8287756997602287, 1.353309037794695024 ) ) ;
#55340 = CARTESIAN_POINT ( 'NONE',  ( 157.2104826425669728, 258.3504519110855995, -16.92635148710569482 ) ) ;
#55341 = CARTESIAN_POINT ( 'NONE',  ( 162.2080922643726240, 251.7946761793016321, -12.96017575965868396 ) ) ;
#55342 = ORIENTED_EDGE ( 'NONE', *, *, #38969, .F. ) ;
#55343 = CARTESIAN_POINT ( 'NONE',  ( 21.31191609055706593, 183.1115022471902591, 10.00000000000009592 ) ) ;
#55344 = LINE ( 'NONE', #55831, #45766 ) ;
#55345 = LINE ( 'NONE', #39636, #85490 ) ;
#55346 = CARTESIAN_POINT ( 'NONE',  ( 143.8814004702669536, 260.0024278399161517, 9.188101187500095079 ) ) ;
#55347 = CARTESIAN_POINT ( 'NONE',  ( 33.29248241878940462, 22.14754757982091604, -5.678558825948276656 ) ) ;
#55348 = CARTESIAN_POINT ( 'NONE',  ( 170.0801020929759204, 263.5121983774269552, 15.83860714571988915 ) ) ;
#55349 = CARTESIAN_POINT ( 'NONE',  ( 185.3894397174689175, 260.3747351616150354, 6.351723045801915823 ) ) ;
#55350 = CARTESIAN_POINT ( 'NONE',  ( 74.86346528667428402, 202.4824982072973967, 3.021315404115420679E-15 ) ) ;
#55351 = CARTESIAN_POINT ( 'NONE',  ( 183.5770085761344887, 258.0265213594843772, -2.300074763849718540 ) ) ;
#55352 = CARTESIAN_POINT ( 'NONE',  ( 66.05783656691208705, 68.59385915743264661, 1.875286379491093447 ) ) ;
#55353 = EDGE_LOOP ( 'NONE', ( #96678, #92415, #70096 ) ) ;
#55354 = B_SPLINE_CURVE_WITH_KNOTS ( 'NONE', 3,
 ( #32625, #63523, #48843, #10340 ),
 .UNSPECIFIED., .F., .F.,
 ( 4, 4 ),
 ( 0.008727764669621856930, 0.01504605018596882372 ),
 .UNSPECIFIED. ) ;
#55355 = B_SPLINE_CURVE_WITH_KNOTS ( 'NONE', 3,
 ( #61836, #17245, #10164, #63849 ),
 .UNSPECIFIED., .F., .F.,
 ( 4, 4 ),
 ( 0.04383130453832326245, 0.04887120950165268346 ),
 .UNSPECIFIED. ) ;
#55356 = CARTESIAN_POINT ( 'NONE',  ( 179.8738126827349788, 255.7374587583702237, -7.018155654023178869 ) ) ;
#55357 = CARTESIAN_POINT ( 'NONE',  ( 2.780145572064765425, 23.64646525600387506, -2.839279412974133887 ) ) ;
#55358 = CARTESIAN_POINT ( 'NONE',  ( 153.2539470794098122, 277.7226751097910551, -5.798683309584624190 ) ) ;
#55359 = CARTESIAN_POINT ( 'NONE',  ( 14.76917458061509514, 17.03085787977761711, 9.188101187500006262 ) ) ;
#55360 = CARTESIAN_POINT ( 'NONE',  ( 206.1062572280473546, 273.6604860535989587, -9.773577984388410300 ) ) ;
#55361 = DIRECTION ( 'NONE',  ( -1.000000000000000000, 0.000000000000000000, 0.000000000000000000 ) ) ;
#55362 = CARTESIAN_POINT ( 'NONE',  ( -52.32156893544652121, 31.15564784356141814, 177.5919119679930134 ) ) ;
#55363 = CARTESIAN_POINT ( 'NONE',  ( -19.15453390681661716, 24.31945705462846163, 10.00000000000000000 ) ) ;
#55364 = CARTESIAN_POINT ( 'NONE',  ( 93.60468337831815688, 236.3967562850347122, -4.648177544792955347E-16 ) ) ;
#55365 = CARTESIAN_POINT ( 'NONE',  ( 87.89296955652562815, 44.95200477618787716, 6.297572492595286953 ) ) ;
#55366 = CARTESIAN_POINT ( 'NONE',  ( 193.9401685343300699, 294.7327698005063326, 14.01047396938887069 ) ) ;
#55367 = ORIENTED_EDGE ( 'NONE', *, *, #427, .F. ) ;
#55368 = ORIENTED_EDGE ( 'NONE', *, *, #33051, .F. ) ;
#55369 = CARTESIAN_POINT ( 'NONE',  ( 19.98788723728717898, 104.4047874917408336, -22.49999999999983302 ) ) ;
#55370 = CARTESIAN_POINT ( 'NONE',  ( 72.85632693199180210, 70.83663663905541341, 7.234987929808680995 ) ) ;
#55371 = ORIENTED_EDGE ( 'NONE', *, *, #44100, .T. ) ;
#55372 = CARTESIAN_POINT ( 'NONE',  ( 160.0581542544236697, 283.4287238101934463, 3.385839116031148510 ) ) ;
#55373 = DIRECTION ( 'NONE',  ( 0.000000000000000000, 0.000000000000000000, -1.000000000000000000 ) ) ;
#55374 = ORIENTED_EDGE ( 'NONE', *, *, #72185, .T. ) ;
#55375 = CYLINDRICAL_SURFACE ( 'NONE', #57208, 10.00000000000010658 ) ;
#55376 = CARTESIAN_POINT ( 'NONE',  ( 85.04793144752864009, 49.76842598555754194, 13.42690168825989439 ) ) ;
#55378 = AXIS2_PLACEMENT_3D ( 'NONE', #1309, #85449, #60200 ) ;
#55377 = CARTESIAN_POINT ( 'NONE',  ( 11.41020553640983692, 28.36126292948894800, 6.180339887498949913 ) ) ;
#55379 = ORIENTED_EDGE ( 'NONE', *, *, #10883, .F. ) ;
#55380 = CARTESIAN_POINT ( 'NONE',  ( 155.5508027672438516, 261.2251017794452537, 18.53492801382433797 ) ) ;
#55381 = B_SPLINE_CURVE_WITH_KNOTS ( 'NONE', 3,
 ( #61616, #76356, #92571, #39794, #70218, #1338, #30234, #24621, #825, #62609, #93053, #32223, #63126, #9943, #58027, #3836, #41309, #72253, #64128, #95078, #11458, #79380, #56001, #88493, #72765, #73243, #96075, #47910, #2858, #95591, #42314, #48432, #34721, #56523, #87511, #32723, #94563, #33749, #19055, #64641, #26137, #40805, #9433, #25642, #78851, #49929, #57016, #18044 ),
 .UNSPECIFIED., .F., .F.,
 ( 4, 2, 2, 2, 2, 2, 2, 2, 2, 2, 2, 2, 2, 2, 2, 2, 2, 2, 2, 2, 2, 2, 2, 4 ),
 ( 0.0002339713884637640586, 0.0007176085954676936045, 0.001201245802471623096, 0.001443064405973626656, 0.001563973707724620630, 0.001684883009475614604, 0.001805792311226608578, 0.001926701612977602552, 0.002168520216479427436, 0.002652157423483079805, 0.003135794630486731741, 0.004103069044493933698, 0.005070343458501136956, 0.005553980665504702589, 0.005795799269006407343, 0.005916708570757258853, 0.006037617872508110363, 0.006098072523383518337, 0.006158527174258925443, 0.006279436476009738789, 0.006521255079511365481, 0.007004892286514617997, 0.007488529493517870513, 0.007972166700521123028 ),
 .UNSPECIFIED. ) ;
#55382 = CARTESIAN_POINT ( 'NONE',  ( 151.4384131719918685, 268.3479694989391078, 14.98299707687648841 ) ) ;
#55383 = CARTESIAN_POINT ( 'NONE',  ( 39.48888774545857672, 24.92755873383629250, 6.180339887498953466 ) ) ;
#55384 = ORIENTED_EDGE ( 'NONE', *, *, #25704, .T. ) ;
#55385 = VERTEX_POINT ( 'NONE', #47201 ) ;
#55386 = B_SPLINE_CURVE_WITH_KNOTS ( 'NONE', 3,
 ( #50542, #33885, #4451, #88124, #49553, #80506, #34358, #41956, #3483, #96200, #26761, #90632, #76394, #61160, #99687, #28779, #52074, #45948, #36873, #46450, #44462, #22682, #61660, #77381, #53561, #59660, #14583, #67779, #36366, #6970, #92129, #37854, #68763, #67271, #30270, #45461, #84513, #30779, #92609, #15057, #54047, #37362, #76865, #23156, #98198, #7463 ),
 .UNSPECIFIED., .F., .F.,
 ( 4, 2, 2, 2, 2, 2, 2, 2, 2, 2, 2, 2, 2, 2, 2, 2, 2, 2, 2, 2, 2, 2, 4 ),
 ( 0.0007152033892065767741, 0.0009241115395241573677, 0.001133019689841737853, 0.001237473765000528421, 0.001341927840159318555, 0.001550835990476795608, 0.001968652291111705043, 0.002386468591746614912, 0.003222101193016370033, 0.004057733794286125587, 0.004893366395555881140, 0.005311182696190713814, 0.005520090846508093722, 0.005624544921666784110, 0.005676771959246130171, 0.005728998996825474498, 0.005833453071984298459, 0.005937907147143122420, 0.006146815297460746924, 0.006355723447778373163, 0.006564631598095997667, 0.006982447898731253613, 0.007400264199366509560 ),
 .UNSPECIFIED. ) ;
#55387 = VERTEX_POINT ( 'NONE', #70503 ) ;
#55388 = CARTESIAN_POINT ( 'NONE',  ( 73.70413300610479723, 62.75607992594843410, 14.52880401046331649 ) ) ;
#55389 = ORIENTED_EDGE ( 'NONE', *, *, #76724, .T. ) ;
#55390 = DIRECTION ( 'NONE',  ( 0.4493970231495826861, -0.7783784768652872721, -0.4383711467890751834 ) ) ;
#55391 = EDGE_LOOP ( 'NONE', ( #49950, #64362, #33877, #37255 ) ) ;
#55392 = CARTESIAN_POINT ( 'NONE',  ( 82.39459624707119190, 46.56163555380788210, 11.63221967415142011 ) ) ;
#55393 = CARTESIAN_POINT ( 'NONE',  ( 88.74573251350186354, 44.01220097505220963, 0.000000000000000000 ) ) ;
#55394 = CARTESIAN_POINT ( 'NONE',  ( 148.4083960970861256, 273.5961130204771052, -8.574185186226726429 ) ) ;
#55395 = EDGE_CURVE ( 'NONE', #469, #4764, #87912, .T. ) ;
#55396 = CARTESIAN_POINT ( 'NONE',  ( -19.65312891409030271, 93.06504152958497400, 177.5919119679930134 ) ) ;
#55397 = DIRECTION ( 'NONE',  ( 0.5000000000000013323, -0.8660254037844378194, 0.000000000000000000 ) ) ;
#55398 = VECTOR ( 'NONE', #12139, 1000.000000000000000 ) ;
#55399 = FACE_OUTER_BOUND ( 'NONE', #77837, .T. ) ;
#55400 = CARTESIAN_POINT ( 'NONE',  ( 18.36860284018464995, 32.64646525600389992, -2.839279412974133887 ) ) ;
#55401 = CARTESIAN_POINT ( 'NONE',  ( 201.8642752310742026, 279.1281314597073901, -15.91742344199423975 ) ) ;
#55402 = CARTESIAN_POINT ( 'NONE',  ( 191.4715169758341631, 298.5146068092147402, -8.393071345078833900 ) ) ;
#55404 = EDGE_LOOP ( 'NONE', ( #8813, #62447, #34129 ) ) ;
#55403 = CARTESIAN_POINT ( 'NONE',  ( 197.9598023461055902, 287.7705598106892921, 18.23120408239484291 ) ) ;
#55405 = DIRECTION ( 'NONE',  ( 1.804112415015878984E-15, -1.000000000000000000, 0.000000000000000000 ) ) ;
#55406 = CARTESIAN_POINT ( 'NONE',  ( 168.2950000418480840, 257.1262184943008151, -14.43479976811267207 ) ) ;
#55407 = CARTESIAN_POINT ( 'NONE',  ( 159.6288139302610887, 254.1617792512662675, -15.32287760493869477 ) ) ;
#55408 = EDGE_CURVE ( 'NONE', #45021, #11459, #52799, .T. ) ;
#55409 = CARTESIAN_POINT ( 'NONE',  ( -11.40312891409031693, 78.77562236714182120, 59.99999999999999289 ) ) ;
#55410 = EDGE_CURVE ( 'NONE', #40696, #28346, #4350, .T. ) ;
#55411 = CARTESIAN_POINT ( 'NONE',  ( 161.5056331467593225, 250.9110330116698435, 14.52719814064025528 ) ) ;
#55412 = CARTESIAN_POINT ( 'NONE',  ( 50.32263495959776378, 94.90690751109829648, -10.00000000000000000 ) ) ;
#55413 = VERTEX_POINT ( 'NONE', #33517 ) ;
#55414 = CARTESIAN_POINT ( 'NONE',  ( 194.1856896721330941, 294.3075147154997353, -15.68532121655275091 ) ) ;
#55415 = CARTESIAN_POINT ( 'NONE',  ( 136.3309150271299757, 239.5177522451417929, 5.000000000000051514 ) ) ;
#55416 = DIRECTION ( 'NONE',  ( 0.000000000000000000, -1.000000000000000000, 0.000000000000000000 ) ) ;
#55417 = CARTESIAN_POINT ( 'NONE',  ( 12.05626958406296367, 177.7677522451418497, 10.00000000000009592 ) ) ;
#55418 = CARTESIAN_POINT ( 'NONE',  ( 82.93486267893706554, 224.8149278399160664, -9.188101187500095079 ) ) ;
#55419 = CARTESIAN_POINT ( 'NONE',  ( 196.2856740628847660, 269.3488336749823020, -11.99430192484340729 ) ) ;
#55420 = CARTESIAN_POINT ( 'NONE',  ( 10.05514423959709625, 21.50829794293879260, -10.00000000000000355 ) ) ;
#55421 = CARTESIAN_POINT ( 'NONE',  ( 170.2399687990647976, 280.5198609568276424, -13.78404537617314141 ) ) ;
#55423 = CARTESIAN_POINT ( 'NONE',  ( -19.65312891409032403, 93.06504152958505927, 0.000000000000000000 ) ) ;
#55422 = CARTESIAN_POINT ( 'NONE',  ( 4.315907217689738395, 182.4869531367911293, 4.594050593750046652 ) ) ;
#55424 = CARTESIAN_POINT ( 'NONE',  ( 200.1385401540174769, 283.9968752310148830, 17.30012534137638625 ) ) ;
#55425 = ORIENTED_EDGE ( 'NONE', *, *, #75166, .T. ) ;
#55427 = EDGE_LOOP ( 'NONE', ( #75177, #40953, #12986, #75031 ) ) ;
#55426 = UNCERTAINTY_MEASURE_WITH_UNIT (LENGTH_MEASURE( 1.000000000000000082E-05 ), #56367, 'distance_accuracy_value', 'NONE');
#55428 = CARTESIAN_POINT ( 'NONE',  ( 169.1311965936330353, 247.8770103324328034, 7.134965090537657859E-13 ) ) ;
#55429 = CARTESIAN_POINT ( 'NONE',  ( 188.8744765375133454, 261.5075027424167615, -6.011881065006100755 ) ) ;
#55430 = CARTESIAN_POINT ( 'NONE',  ( 68.04221563692973973, 69.62749528806014609, 2.672723919121051228 ) ) ;
#55431 = CARTESIAN_POINT ( 'NONE',  ( 31.15975419450677819, 23.15404122711134960, 8.090169943749479842 ) ) ;
#55432 = CARTESIAN_POINT ( 'NONE',  ( 207.8844858873204657, 270.5805036682629066, -6.251308616122969397 ) ) ;
#55433 = CARTESIAN_POINT ( 'NONE',  ( 142.4863040978925142, 267.5053245118543828, -2.761272660171010366E-15 ) ) ;
#55434 = CARTESIAN_POINT ( 'NONE',  ( 74.18796447308154995, 68.76651203251665834, -11.36463150814737766 ) ) ;
#55435 = EDGE_CURVE ( 'NONE', #48842, #98408, #86268, .T. ) ;
#55436 = CARTESIAN_POINT ( 'NONE',  ( 38.38920161542251464, 180.7202760586659451, -5.415160957724236172E-17 ) ) ;
#55437 = CARTESIAN_POINT ( 'NONE',  ( 77.00817486789587463, 215.2677522451418497, 10.00000000000009592 ) ) ;
#55438 = CARTESIAN_POINT ( 'NONE',  ( 199.4869826154170482, 277.5167049526704091, 15.17882519192913726 ) ) ;
#55439 = EDGE_LOOP ( 'NONE', ( #73479, #52416, #33478, #73154 ) ) ;
#55440 = DIRECTION ( 'NONE',  ( -0.8660254037844379305, -0.5000000000000014433, -0.000000000000000000 ) ) ;
#55441 = EDGE_CURVE ( 'NONE', #3474, #81396, #39892, .T. ) ;
#55442 = ADVANCED_FACE ( 'NONE', ( #40593 ), #80659, .T. ) ;
#55443 = CARTESIAN_POINT ( 'NONE',  ( 175.2553799847831897, 281.2052230826317327, -14.44794444881370943 ) ) ;
#55444 = VECTOR ( 'NONE', #59796, 1000.000000000000000 ) ;
#55445 = DIRECTION ( 'NONE',  ( -0.000000000000000000, 1.000000000000000000, -0.000000000000000000 ) ) ;
#55446 = CARTESIAN_POINT ( 'NONE',  ( 157.0957870390718369, 258.5491105237443321, 17.69218919045495397 ) ) ;
#55447 = CARTESIAN_POINT ( 'NONE',  ( 155.4917600441137324, 261.3273667757233056, 17.14261720787171939 ) ) ;
#55448 = CARTESIAN_POINT ( 'NONE',  ( 207.6357208050208101, 271.0113774299547913, -6.790259683043212036 ) ) ;
#55449 = CARTESIAN_POINT ( 'NONE',  ( -34.73454462704830803, 165.1868197944959036, 8.171888229646977204E-14 ) ) ;
#55450 = CARTESIAN_POINT ( 'NONE',  ( 194.6310785344323904, 293.5360785768717165, -14.54510914272505495 ) ) ;
#55451 = EDGE_CURVE ( 'NONE', #63738, #11479, #9186, .T. ) ;
#55452 = ADVANCED_FACE ( 'NONE', ( #80156 ), #10222, .F. ) ;
#55453 = CARTESIAN_POINT ( 'NONE',  ( 72.95338987351841809, 67.58086510047205309, 11.78688422015949477 ) ) ;
#55454 = CARTESIAN_POINT ( 'NONE',  ( 163.8147431267737204, 246.9115372060205118, 7.125417796469586840 ) ) ;
#55455 = CARTESIAN_POINT ( 'NONE',  ( 175.9532122701685921, 256.5273912432038514, -11.06277192129556042 ) ) ;
#55456 = CARTESIAN_POINT ( 'NONE',  ( 191.5324528500417216, 298.9030556958743432, -8.286652526617016790 ) ) ;
#55457 = CARTESIAN_POINT ( 'NONE',  ( 148.1672759425158290, 274.0137453789218398, 7.847779094015780110 ) ) ;
#55458 = ORIENTED_EDGE ( 'NONE', *, *, #28389, .F. ) ;
#55459 = CARTESIAN_POINT ( 'NONE',  ( 74.57284120713386244, 59.58620412426768809, 16.13232198448460863 ) ) ;
#55460 = CARTESIAN_POINT ( 'NONE',  ( 135.0578773561867649, 260.3297689869269220, -2.679491924311252493 ) ) ;
#55461 = CARTESIAN_POINT ( 'NONE',  ( 110.1064097226738312, 240.5024278399161233, 9.188101187500095079 ) ) ;
#55462 = CARTESIAN_POINT ( 'NONE',  ( 18.45335787429653607, 11.44966523072493558, -2.296566073217252530E-15 ) ) ;
#55463 = CARTESIAN_POINT ( 'NONE',  ( 191.5694459269389824, 298.8389818071599962, 7.944420692511652504 ) ) ;
#55464 = DIRECTION ( 'NONE',  ( 0.05364311403570637404, 0.9985601716053731369, 0.000000000000000000 ) ) ;
#55465 = AXIS2_PLACEMENT_3D ( 'NONE', #82494, #91555, #59608 ) ;
#55467 = CARTESIAN_POINT ( 'NONE',  ( 102.5355703512972809, 241.5530062829863027, -4.648177544792955347E-16 ) ) ;
#55466 = FACE_OUTER_BOUND ( 'NONE', #10113, .T. ) ;
#55468 = B_SPLINE_CURVE_WITH_KNOTS ( 'NONE', 3,
 ( #55121, #32832, #86107, #1948, #2458, #16634, #63742, #78458, #1457, #55616, #48547, #94676, #25234, #79487, #97177, #65235, #58613, #89112, #81973, #18655, #64752, #2975, #27744, #18148, #19661, #12550, #58130, #66240, #11059, #65722, #96679 ),
 .UNSPECIFIED., .F., .F.,
 ( 4, 3, 3, 3, 3, 3, 3, 3, 3, 3, 4 ),
 ( 0.000000000000000000, 0.1333490885032316831, 0.3007194338854232707, 0.4699862290244899432, 0.5844252810809152932, 0.6686540514502595789, 0.7354980260655316071, 0.8028463152565562533, 0.8633854507756971719, 0.9437142632666813968, 1.000000000000000000 ),
 .UNSPECIFIED. ) ;
#55469 = CARTESIAN_POINT ( 'NONE',  ( 190.9252692466827455, 299.9547285464148558, -6.441337159356977260 ) ) ;
#55470 = CARTESIAN_POINT ( 'NONE',  ( 189.7671801472840514, 261.0678685170981339, -4.565022058661969417 ) ) ;
#55471 = CARTESIAN_POINT ( 'NONE',  ( 196.6800254274587019, 289.9871984561398222, -17.90749311895638129 ) ) ;
#55472 = CARTESIAN_POINT ( 'NONE',  ( 89.36707907128423756, 215.7365022471902023, 10.00000000000009948 ) ) ;
#55473 = CARTESIAN_POINT ( 'NONE',  ( 173.7827001204449004, 290.0886546788046303, -1.066826985794086191 ) ) ;
#55474 = CARTESIAN_POINT ( 'NONE',  ( 65.88310562893973099, 69.02589174555536999, 1.996831191813060347 ) ) ;
#55475 = ORIENTED_EDGE ( 'NONE', *, *, #52182, .T. ) ;
#55476 = CARTESIAN_POINT ( 'NONE',  ( 132.7946446283434625, 254.1427522451419065, -10.00000000000009592 ) ) ;
#55477 = CARTESIAN_POINT ( 'NONE',  ( -59.82327302696292293, 35.73826312759339174, 10.00000000000000000 ) ) ;
#55478 = CARTESIAN_POINT ( 'NONE',  ( 199.8507473897895750, 270.1007356502280459, 9.248113246699395162 ) ) ;
#55479 = ORIENTED_EDGE ( 'NONE', *, *, #93249, .T. ) ;
#55480 = CARTESIAN_POINT ( 'NONE',  ( 75.86452061248199641, 65.14283366293828692, -14.47928019947265277 ) ) ;
#55481 = CARTESIAN_POINT ( 'NONE',  ( 187.5689534105982261, 259.0063497273899884, 3.853393514624363636 ) ) ;
#55482 = LINE ( 'NONE', #69702, #4864 ) ;
#55483 = CARTESIAN_POINT ( 'NONE',  ( 152.8522706834672533, 265.8990964544007056, 17.63080661522264947 ) ) ;
#55484 =( BOUNDED_SURFACE ( )  B_SPLINE_SURFACE ( 1, 2, ( 
 ( #16958, #62546, #93508, #23052, #86432, #47847, #78786, #269, #64073, #53950, #40750, #9373, #40252, #9893, #71192, #1786, #25064, #32668, #63567, #86938, #17469, #48380, #71699, #2293, #84906, #15448, #2801, #49869, #10384, #12383, #95018, #18995, #33687, #41253, #87457, #48883, #72193, #4262, #49372, #35161, #3298, #73188, #79817, #11400, #18487, #73679, #26583, #80832, #42254, #80315, #42745, #74193, #97018, #27588, #66070, #58453, #3782, #34664, #96020, #65566, #57456, #19505, #56466, #11887, #50857, #26082, #89426, #64582, #19980, #95534, #43249, #96512, #81808, #25580, #4783, #87943, #27082, #17989, #56956, #10885, #41761, #72708, #57964, #34177, #65071, #88949, #50361, #81316, #35664, #52847, #97977, #68547, #13377, #13858, #52349, #44244, #84298, #75182, #44736, #75670, #6255, #37153, #68052, #67552, #36150, #98975, #22453, #5756, #74692, #98484, #99472, #36646, #89902, #37636, #29076, #76655, #82809, #14846, #60433, #20990, #59941, #66565, #5270, #90912, #67054, #12891, #7243, #97492, #45732, #29559, #21461, #53348, #83294, #14360, #30048, #76183, #91389, #21953, #83797, #43748, #45247, #6758, #60938, #20481, #28553, #91898, #82322, #28059, #58932, #51354, #59435, #90416, #51871, #92393, #53829, #47732, #92881, #78666, #46747, #16349, #22940, #54838, #61929, #16842, #70037, #93387, #62426, #23435, #86307, #17343, #40129, #71068, #9257, #1670, #23939, #85820, #39123, #47243, #650, #32553, #86811, #55818, #85295, #84789, #15330, #78163, #69042, #63451, #46225, #8750, #94387, #24940, #77147, #38643, #48251, #8258, #39621, #79197, #70543, #7751, #1159, #38125, #32033, #62944, #99972, #69549, #31537, #30557, #61441, #154, #31042, #93895, #54324, #15839, #24449, #77674, #55330, #50239, #63944, #26460, #33045, #81193, #40633, #18361, #19861, #72577, #80699, #41127, #25445, #3665, #88310, #41633, #49746, #64957, #64451, #11274, #42625, #42136, #96891, #95902, #4138, #57833, #50728, #96386, #34543, #80191, #94883, #73067, #57336, #3182, #18864, #72065, #56335, #73554, #49254, #65937, #10258, #65441, #35033, #87333, #11762, #33556, #71568, #2164, #26950, #10759, #88814, #19379, #27460, #95410, #58331, #48763, #25967, #89307, #17865, #9771, #79696, #2665, #56837, #87822, #45493, #84059, #51225, #74058, #29808, #27935, #85038, #54084, #15587, #14615, #4647, #61194, #81683, #7494, #30811, #82193, #89779, #37886, #53104, #22713, #36027, #38392, #53593, #15090, #91640, #12764, #76427, #74568, #84550, #7000, #68795, #43114, #92163, #68299, #61690, #46488, #69303, #22207, #45979, #99723, #30309, #5146, #76896, #20355, #99222, #100225, #35539, #92643, #58817, #93136, #23191, #77421, #8022, #38894, #43629, #66442, #60681, #69798, #407, #31297, #62183, #23685, #97369, #12256, #54580, #79453, #2426, #55090, #62688, #9524, #24699, #94643, #9004, #10018, #25199, #87077, #63204, #24209, #55581, #47498, #56082, #86565, #17095, #16106, #32803, #39876, #33303, #25722, #40880, #63707, #79948, #10514, #93644, #86076, #41391, #47993, #17609, #64205, #1916, #16600, #71325, #64716, #48517, #71829, #95154, #78423, #78936, #72334, #56601, #70813, #87587, #40385, #1419, #32302, #18112, #8511, #94146, #49015, #39379, #2939, #77919, #33827, #85561, #95665, #47005, #70296, #907, #31786, #41897, #20116, #4398, #58097, #66206, #50488, #80961, #97147, #59067, #27713, #13023, #81443, #20611, #74328, #36289, #12514, #50986, #96645, #11025, #58581, #42871, #89080, #35295, #88570, #72836, #90037, #34788, #82461, #26708, #12014, #51492, #3429, #28191, #50005, #88073, #18621, #81936, #89553, #19630, #65691, #34304, #43386, #42386, #27215, #49499, #65204, #73804, #96145, #43886, #26213, #4917, #57589, #19132, #80454, #11525, #73316, #35797, #3907, #66691, #97627, #74825, #5405, #67188, #57090, #76786, #29692, #52986, #22088, #52483, #45861, #77291, #100109, #30693, #7379, #38268, #83934, #14498, #99109, #45380, #60568, #69179, #46362, #15467, #44876, #13514, #51997, #76311, #28696, #61573, #44382, #22588, #59574, #14974, #53964, #29205, #92524, #36786, #23070, #67695, #7899, #68677, #84921, #90549, #38774, #91035, #91524, #21121, #98623, #83431, #5895, #82940, #6885, #6400, #13997, #30186, #60073, #75315, #98112, #84429, #21603, #75816, #37285, #37775, #99608, #68180, #61072, #92043, #53478, #78801, #16973, #9389, #40265, #70680, #39259, #71205, #25594, #78301, #77808, #1294, #2305, #47376, #93011, #40762, #32179, #79829, #85955, #18003, #63581, #24081, #39751, #69680, #8391, #94027, #70171, #15984, #10397, #284, #87468, #1797, #8883, #56480, #63082, #17483, #71713, #79334, #54456, #32681, #86448, #24578, #94523, #31665, #46883, #33186, #55461, #48895, #778, #47864, #95030, #62561, #64086, #93524, #31172, #62062, #25075, #55955, #86950, #48391, #9904, #54977, #23565, #16482, #85435, #11414, #64595, #80844, #18500, #51369, #73201, #49885, #3796, #42268, #10899, #33702, #88452, #87955, #43263, #12397, #74208, #34677, #95547, #19517, #41266, #66085, #89438, #41775, #49386, #96527, #65579, #81330, #96034, #97031, #11901, #73691, #27097, #72721, #57980, #34191, #42759, #88963, #50377, #2813, #4275, #26595, #19994, #4798, #27600, #35174, #66580, #97504, #80331, #3312, #28074, #58466, #50872, #81822, #35679, #65083, #58946, #82337, #89917, #20497, #72209, #57469, #26096, #56970, #19011, #75196, #84313, #98990, #44264, #98500, #99488, #67067, #21478, #53363, #97991, #29573, #36164, #14860, #43764, #52366, #22955, #75687, #83812, #5771, #28570, #6773, #91404, #44754, #52862, #37168, #67567, #14379, #45747, #45263, #99988, #68066, #7259, #60955, #53844, #30066, #37652, #83311, #91914, #6273, #60451, #21969, #29090, #22469, #92407, #76672, #38142, #69059, #30572, #76197, #68563, #13873, #61457, #12905, #74708, #5285, #59450, #59956, #90431, #21003, #51884, #82825, #13393, #36660, #90928, #46240, #1686, #40649, #15857, #55833, #23449, #63467, #54339, #2182, #55346, #32571, #15344, #94403, #77690, #78179, #7768, #85311 ),
 ( #46764, #54859, #8273, #86323, #85837, #16367, #77166, #62962, #39138, #24957, #86828, #40146, #93912, #9789, #71587, #92896, #70051, #33065, #47258, #16860, #17361, #32050, #666, #1176, #94901, #24466, #47747, #48268, #31551, #8768, #63959, #79215, #62440, #25464, #70559, #93407, #23956, #71087, #38661, #39637, #84804, #69564, #78684, #171, #31055, #61944, #9273, #66457, #18884, #26971, #87839, #72083, #50256, #34560, #88329, #96402, #80719, #10778, #57853, #89323, #88833, #43133, #11293, #50747, #58347, #19877, #4153, #35050, #42152, #73087, #57353, #3681, #49764, #96908, #4665, #74075, #3200, #2684, #10275, #65460, #87353, #81700, #33575, #81209, #17882, #73571, #12273, #18378, #27479, #95430, #65957, #25983, #35556, #19397, #97382, #48780, #56353, #49273, #11781, #79712, #56853, #41653, #64470, #41145, #42641, #64974, #72595, #80210, #34084, #95917, #26477, #14252, #59325, #29943, #75070, #75561, #13747, #5649, #45625, #36539, #6149, #37043, #67952, #98870, #29449, #28962, #97872, #60325, #84197, #67445, #36041, #59840, #60818, #98374, #51242, #99364, #90803, #38020, #44136, #76554, #21847, #82707, #21358, #27949, #66942, #52243, #28445, #74583, #68931, #58831, #7133, #91281, #83187, #14744, #44627, #76079, #91780, #37530, #52729, #83691, #45139, #5162, #6655, #68435, #22345, #82209, #90305, #53242, #43645, #89796, #20371, #12780, #20875, #51765, #13274, #53724, #15223, #9147, #54216, #40021, #8148, #78055, #84683, #16241, #23329, #78561, #31429, #54724, #23830, #85183, #47630, #79085, #39021, #7640, #547, #32447, #77559, #22840, #70961, #62320, #9667, #15730, #48141, #93787, #46634, #69929, #99856, #38532, #85705, #69438, #46118, #40528, #30441, #17234, #1049, #93273, #86700, #47132, #1562, #63343, #94281, #8644, #39514, #70439, #77034, #31927, #62831, #24347, #55, #30939, #55221, #61824, #61330, #92290, #86202, #92775, #16741, #24836, #55710, #87222, #81094, #25862, #11660, #80087, #49634, #25338, #88204, #95306, #50140, #3077, #26352, #95799, #56738, #19274, #50627, #73456, #4039, #42522, #34928, #57228, #18755, #72473, #80591, #33967, #65824, #19759, #89211, #18256, #17756, #56229, #11168, #2054, #96789, #48657, #96279, #32936, #88704, #27349, #2562, #58230, #10154, #81581, #41020, #12150, #42036, #71463, #63840, #94778, #64342, #64852, #79590, #71958, #87720, #33445, #49152, #72971, #10654, #41530, #3562, #34442, #65341, #26849, #57724, #74468, #45022, #90180, #90689, #28843, #20755, #60704, #51643, #21246, #52123, #83074, #13644, #44517, #44011, #12660, #75448, #99248, #5538, #6032, #5048, #89692, #75966, #82592, #29832, #43529, #59723, #68322, #20251, #6541, #66830, #4536, #35436, #67840, #13157, #36927, #98760, #74954, #97758, #29343, #82088, #28328, #36422, #66339, #67330, #51126, #53129, #98254, #60208, #91169, #21733, #35928, #97272, #52617, #59205, #37416, #14136, #91665, #83575, #27839, #22228, #43012, #84086, #73950, #58716, #52653, #99774, #14671, #84604, #99284, #100281, #15142, #76956, #53166, #14174, #45549, #37449, #46039, #76482, #7059, #6066, #22771, #29866, #23250, #15647, #30867, #53648, #69855, #468, #83606, #45059, #31357, #37941, #7556, #92700, #92219, #76000, #61250, #54643, #38448, #69362, #54138, #6577, #68853, #62240, #85100, #68359, #46545, #30367, #60737, #91699, #61750, #98794, #84120, #77480, #29375, #8077, #67873, #38950, #75483, #93194, #85620, #23747, #44549, #22262, #60243, #36960, #91202, #21763, #56142, #40448, #70874, #87141, #49073, #17672, #3000, #71383, #10574, #64263, #26272, #2481, #10073, #86623, #968, #48572, #32858, #95216, #57148, #33363, #40938, #17157, #31845, #79511, #63765, #78998, #25259, #78481, #62748, #80005, #24758, #72390, #16660, #1971, #41449, #93704, #18171, #39935, #77975, #8572, #71882, #48055, #25783, #94697, #9584, #1480, #56659, #55144, #32363, #87644, #39437, #33890, #24267, #16164, #64775, #95723, #47062, #70356, #86130, #47554, #63262, #9068, #94203, #59125, #51555, #19685, #11085, #66265, #88130, #12573, #35856, #88624, #96204, #42929, #58154, #27766, #42440, #43450, #89615, #20176, #96702, #57648, #89134, #81021, #51043, #50547, #12071, #49557, #97199, #73376, #66749, #90098, #74391, #82001, #13079, #43940, #26767, #19193, #5463, #73868, #4974, #97685, #35355, #50063, #4457, #98178, #28251, #82518, #36346, #11583, #67249, #28757, #18676, #3963, #80510, #41960, #34845, #65749, #72897, #3487, #27271, #34362, #65260, #76371, #82994, #30754, #90609, #68241, #69737, #22152, #30249, #91093, #75374, #53537, #37834, #91579, #99663, #84000, #14057, #61132, #23128, #92107, #46425, #14561, #54023, #75882, #99165, #13572, #67757, #45436, #5957, #77350, #59637, #6942, #98682, #36849, #52056, #44442, #29262, #69239, #44938, #100169, #29753, #68740, #60132, #22654, #83491, #38331, #53042, #84488, #15031, #6460, #7438, #38831, #61633, #84978, #15524, #7957, #45923, #76841, #60625, #345, #21176, #21659, #52541, #37339, #78364, #46944, #85494, #78867, #62120, #64144, #77862, #56018, #93068, #48449, #87528, #62624, #2364, #70235, #9961, #839, #48955, #1856, #79394, #23622, #40819, #24146, #24639, #54516, #31720, #16539, #39319, #16043, #9452, #39811, #86013, #63643, #93579, #8448, #71766, #17542, #55031, #33242, #8944, #40324, #17036, #70743, #79889, #1355, #71263, #32738, #94581, #25135, #87013, #32240, #47435, #95095, #18059, #63140, #94085, #55519, #25659, #86507, #47927, #56538, #10453, #41327, #72270, #31234, #50436, #65144, #49946, #2876, #10964, #3852, #41836, #18561, #4857, #33768, #74273, #81390, #19071, #43327, #34735, #35238, #89499, #97088, #27156, #65636, #80904, #80394, #11957, #64655, #11476, #72782, #49440, #58043, #26153, #20057, #3373, #73748, #57030, #66141, #95605, #26651, #81880, #96092, #50930, #57532, #88013, #12456, #34247, #88508, #42329, #4342, #73257, #89024, #27657, #58525, #42818, #19575, #96592, #1684, #47745, #25461, #62960, #16365, #10273, #79710, #24464, #95428, #40143, #40647 ) ),
 .UNSPECIFIED., .F., .F., .T. ) 
 B_SPLINE_SURFACE_WITH_KNOTS ( ( 2, 2 ),
 ( 3, 2, 2, 2, 2, 2, 2, 2, 2, 2, 2, 2, 2, 2, 2, 2, 2, 2, 2, 2, 2, 2, 2, 2, 2, 2, 2, 2, 2, 2, 2, 2, 2, 2, 2, 2, 2, 2, 2, 2, 2, 2, 2, 2, 2, 2, 2, 2, 2, 2, 2, 2, 2, 2, 2, 2, 2, 2, 2, 2, 2, 2, 2, 2, 2, 2, 2, 2, 2, 2, 2, 2, 2, 2, 2, 2, 2, 2, 2, 2, 2, 2, 2, 2, 2, 2, 2, 2, 2, 2, 2, 2, 2, 2, 2, 2, 2, 2, 2, 2, 2, 2, 2, 2, 2, 2, 2, 2, 2, 2, 2, 2, 2, 2, 2, 2, 2, 2, 2, 2, 2, 2, 2, 2, 2, 2, 2, 2, 2, 2, 2, 2, 2, 2, 2, 2, 2, 2, 2, 2, 2, 2, 2, 2, 2, 2, 2, 2, 2, 2, 2, 2, 2, 2, 2, 2, 2, 2, 2, 2, 2, 2, 2, 2, 2, 2, 2, 2, 2, 2, 2, 2, 2, 2, 2, 2, 2, 2, 2, 2, 2, 2, 2, 2, 2, 2, 2, 2, 2, 2, 2, 2, 2, 2, 2, 2, 2, 2, 2, 2, 2, 2, 2, 2, 2, 2, 2, 2, 2, 2, 2, 2, 2, 2, 2, 2, 2, 2, 2, 2, 2, 2, 2, 2, 2, 2, 2, 2, 2, 2, 2, 2, 2, 2, 2, 2, 2, 2, 2, 2, 2, 2, 2, 2, 2, 2, 2, 2, 2, 2, 2, 2, 2, 2, 2, 2, 2, 2, 2, 2, 2, 2, 2, 2, 2, 2, 2, 2, 2, 2, 2, 2, 2, 2, 2, 2, 2, 2, 2, 2, 2, 2, 2, 2, 2, 2, 2, 2, 2, 2, 2, 2, 2, 2, 2, 2, 2, 2, 2, 2, 2, 2, 2, 2, 2, 2, 2, 2, 2, 2, 2, 2, 2, 2, 2, 2, 2, 2, 2, 2, 2, 2, 2, 2, 2, 2, 2, 2, 2, 2, 2, 2, 2, 2, 2, 2, 2, 2, 2, 2, 2, 2, 2, 2, 2, 2, 2, 2, 2, 2, 2, 2, 2, 2, 2, 2, 2, 2, 2, 2, 2, 2, 2, 2, 2, 2, 2, 2, 2, 2, 2, 2, 3 ),
 ( 0.000000000000000000, 1.000000000000000000 ),
 ( 0.000000000000000000, 0.002688172043010752903, 0.005376344086021505805, 0.008064516129032257841, 0.01075268817204301161, 0.01344086021505376365, 0.01612903225806451568, 0.01881720430107526945, 0.02150537634408602322, 0.02419354838709677352, 0.02688172043010752729, 0.02956989247311828106, 0.03225806451612903136, 0.03494623655913978166, 0.03763440860215053890, 0.04032258064516128920, 0.04301075268817204644, 0.04569892473118279674, 0.04838709677419354704, 0.05107526881720430428, 0.05376344086021505458, 0.05645161290322580488, 0.05913978494623656212, 0.06182795698924731242, 0.06451612903225806273, 0.06720430107526881303, 0.06989247311827956333, 0.07258064516129032751, 0.07526881720430107781, 0.07795698924731182811, 0.08064516129032257841, 0.08333333333333332871, 0.08602150537634409289, 0.08870967741935484319, 0.09139784946236559349, 0.09408602150537634379, 0.09677419354838709409, 0.09946236559139784439, 0.1021505376344086086, 0.1048387096774193589, 0.1075268817204301092, 0.1102150537634408595, 0.1129032258064516098, 0.1155913978494623601, 0.1182795698924731242, 0.1209677419354838745, 0.1236559139784946248, 0.1263440860215053752, 0.1290322580645161255, 0.1317204301075268758, 0.1344086021505376261, 0.1370967741935483764, 0.1397849462365591267, 0.1424731182795699047, 0.1451612903225806550, 0.1478494623655914053, 0.1505376344086021556, 0.1532258064516129059, 0.1559139784946236562, 0.1586021505376344065, 0.1612903225806451568, 0.1639784946236559071, 0.1666666666666666574, 0.1693548387096774077, 0.1720430107526881858, 0.1747311827956989361, 0.1774193548387096864, 0.1801075268817204367, 0.1827956989247311870, 0.1854838709677419373, 0.1881720430107526876, 0.1908602150537634379, 0.1935483870967741882, 0.1962365591397849385, 0.1989247311827956888, 0.2016129032258064391, 0.2043010752688172171, 0.2069892473118279674, 0.2096774193548387177, 0.2123655913978494680, 0.2150537634408602183, 0.2177419354838709686, 0.2204301075268817189, 0.2231182795698924692, 0.2258064516129032195, 0.2284946236559139698, 0.2311827956989247201, 0.2338709677419354704, 0.2365591397849462485, 0.2392473118279569988, 0.2419354838709677491, 0.2446236559139784994, 0.2473118279569892497, 0.2500000000000000000, 0.2526881720430107503, 0.2553763440860215006, 0.2580645161290322509, 0.2607526881720430012, 0.2634408602150537515, 0.2661290322580645018, 0.2688172043010752521, 0.2715053763440860024, 0.2741935483870967527, 0.2768817204301075030, 0.2795698924731182533, 0.2822580645161290591, 0.2849462365591398094, 0.2876344086021505597, 0.2903225806451613100, 0.2930107526881720603, 0.2956989247311828106, 0.2983870967741935609, 0.3010752688172043112, 0.3037634408602150615, 0.3064516129032258118, 0.3091397849462365621, 0.3118279569892473124, 0.3145161290322580627, 0.3172043010752688130, 0.3198924731182795633, 0.3225806451612903136, 0.3252688172043010639, 0.3279569892473118142, 0.3306451612903225645, 0.3333333333333333148, 0.3360215053763440651, 0.3387096774193548154, 0.3413978494623655657, 0.3440860215053763715, 0.3467741935483871218, 0.3494623655913978721, 0.3521505376344086224, 0.3548387096774193727, 0.3575268817204301230, 0.3602150537634408733, 0.3629032258064516236, 0.3655913978494623739, 0.3682795698924731242, 0.3709677419354838745, 0.3736559139784946248, 0.3763440860215053752, 0.3790322580645161255, 0.3817204301075268758, 0.3844086021505376261, 0.3870967741935483764, 0.3897849462365591267, 0.3924731182795698770, 0.3951612903225806273, 0.3978494623655913776, 0.4005376344086021279, 0.4032258064516128782, 0.4059139784946236285, 0.4086021505376344343, 0.4112903225806451846, 0.4139784946236559349, 0.4166666666666666852, 0.4193548387096774355, 0.4220430107526881858, 0.4247311827956989361, 0.4274193548387096864, 0.4301075268817204367, 0.4327956989247311870, 0.4354838709677419373, 0.4381720430107526876, 0.4408602150537634379, 0.4435483870967741882, 0.4462365591397849385, 0.4489247311827956888, 0.4516129032258064391, 0.4543010752688171894, 0.4569892473118279397, 0.4596774193548386900, 0.4623655913978494403, 0.4650537634408601906, 0.4677419354838709409, 0.4704301075268817467, 0.4731182795698924970, 0.4758064516129032473, 0.4784946236559139976, 0.4811827956989247479, 0.4838709677419354982, 0.4865591397849462485, 0.4892473118279569988, 0.4919354838709677491, 0.4946236559139784994, 0.4973118279569892497, 0.5000000000000000000, 0.5026881720430107503, 0.5053763440860215006, 0.5080645161290322509, 0.5107526881720430012, 0.5134408602150537515, 0.5161290322580645018, 0.5188172043010752521, 0.5215053763440860024, 0.5241935483870967527, 0.5268817204301075030, 0.5295698924731182533, 0.5322580645161290036, 0.5349462365591397539, 0.5376344086021505042, 0.5403225806451612545, 0.5430107526881720048, 0.5456989247311827551, 0.5483870967741935054, 0.5510752688172042557, 0.5537634408602150060, 0.5564516129032257563, 0.5591397849462365066, 0.5618279569892472569, 0.5645161290322581182, 0.5672043010752688685, 0.5698924731182796188, 0.5725806451612903691, 0.5752688172043011194, 0.5779569892473118697, 0.5806451612903226200, 0.5833333333333333703, 0.5860215053763441206, 0.5887096774193548709, 0.5913978494623656212, 0.5940860215053763715, 0.5967741935483871218, 0.5994623655913978721, 0.6021505376344086224, 0.6048387096774193727, 0.6075268817204301230, 0.6102150537634408733, 0.6129032258064516236, 0.6155913978494623739, 0.6182795698924731242, 0.6209677419354838745, 0.6236559139784946248, 0.6263440860215053752, 0.6290322580645161255, 0.6317204301075268758, 0.6344086021505376261, 0.6370967741935483764, 0.6397849462365591267, 0.6424731182795698770, 0.6451612903225806273, 0.6478494623655913776, 0.6505376344086021279, 0.6532258064516128782, 0.6559139784946236285, 0.6586021505376343788, 0.6612903225806451291, 0.6639784946236558794, 0.6666666666666666297, 0.6693548387096773800, 0.6720430107526881303, 0.6747311827956988806, 0.6774193548387096309, 0.6801075268817203812, 0.6827956989247311315, 0.6854838709677418818, 0.6881720430107527431, 0.6908602150537634934, 0.6935483870967742437, 0.6962365591397849940, 0.6989247311827957443, 0.7016129032258064946, 0.7043010752688172449, 0.7069892473118279952, 0.7096774193548387455, 0.7123655913978494958, 0.7150537634408602461, 0.7177419354838709964, 0.7204301075268817467, 0.7231182795698924970, 0.7258064516129032473, 0.7284946236559139976, 0.7311827956989247479, 0.7338709677419354982, 0.7365591397849462485, 0.7392473118279569988, 0.7419354838709677491, 0.7446236559139784994, 0.7473118279569892497, 0.7500000000000000000, 0.7526881720430107503, 0.7553763440860215006, 0.7580645161290322509, 0.7607526881720430012, 0.7634408602150537515, 0.7661290322580645018, 0.7688172043010752521, 0.7715053763440860024, 0.7741935483870967527, 0.7768817204301075030, 0.7795698924731182533, 0.7822580645161290036, 0.7849462365591397539, 0.7876344086021505042, 0.7903225806451612545, 0.7930107526881720048, 0.7956989247311827551, 0.7983870967741935054, 0.8010752688172042557, 0.8037634408602150060, 0.8064516129032257563, 0.8091397849462365066, 0.8118279569892472569, 0.8145161290322581182, 0.8172043010752688685, 0.8198924731182796188, 0.8225806451612903691, 0.8252688172043011194, 0.8279569892473118697, 0.8306451612903226200, 0.8333333333333333703, 0.8360215053763441206, 0.8387096774193548709, 0.8413978494623656212, 0.8440860215053763715, 0.8467741935483871218, 0.8494623655913978721, 0.8521505376344086224, 0.8548387096774193727, 0.8575268817204301230, 0.8602150537634408733, 0.8629032258064516236, 0.8655913978494623739, 0.8682795698924731242, 0.8709677419354838745, 0.8736559139784946248, 0.8763440860215053752, 0.8790322580645161255, 0.8817204301075268758, 0.8844086021505376261, 0.8870967741935483764, 0.8897849462365591267, 0.8924731182795698770, 0.8951612903225806273, 0.8978494623655913776, 0.9005376344086021279, 0.9032258064516128782, 0.9059139784946236285, 0.9086021505376343788, 0.9112903225806451291, 0.9139784946236558794, 0.9166666666666666297, 0.9193548387096773800, 0.9220430107526881303, 0.9247311827956988806, 0.9274193548387096309, 0.9301075268817203812, 0.9327956989247311315, 0.9354838709677418818, 0.9381720430107527431, 0.9408602150537634934, 0.9435483870967742437, 0.9462365591397849940, 0.9489247311827957443, 0.9516129032258064946, 0.9543010752688172449, 0.9569892473118279952, 0.9596774193548387455, 0.9623655913978494958, 0.9650537634408602461, 0.9677419354838709964, 0.9704301075268817467, 0.9731182795698924970, 0.9758064516129032473, 0.9784946236559139976, 0.9811827956989247479, 0.9838709677419354982, 0.9865591397849462485, 0.9892473118279569988, 0.9919354838709677491, 0.9946236559139784994, 0.9973118279569892497, 1.000000000000000000 ),
 .UNSPECIFIED. ) 
 GEOMETRIC_REPRESENTATION_ITEM ( )  RATIONAL_B_SPLINE_SURFACE ( (
 ( 1.000000000000000000, 0.8660254037844387076, 1.000000000000000000, 0.8660254037844387076, 1.000000000000000000, 0.8660254037844387076, 1.000000000000000000, 0.8660254037844387076, 1.000000000000000000, 0.8660254037844387076, 1.000000000000000000, 0.8660254037844387076, 1.000000000000000000, 0.8660254037844387076, 1.000000000000000000, 0.8660254037844387076, 1.000000000000000000, 0.8660254037844387076, 1.000000000000000000, 0.8660254037844387076, 1.000000000000000000, 0.8660254037844387076, 1.000000000000000000, 0.8660254037844387076, 1.000000000000000000, 0.8660254037844387076, 1.000000000000000000, 0.8660254037844387076, 1.000000000000000000, 0.8660254037844387076, 1.000000000000000000, 0.8660254037844387076, 1.000000000000000000, 0.8660254037844387076, 1.000000000000000000, 0.8660254037844387076, 1.000000000000000000, 0.8660254037844387076, 1.000000000000000000, 0.8660254037844387076, 1.000000000000000000, 0.8660254037844387076, 1.000000000000000000, 0.8660254037844387076, 1.000000000000000000, 0.8660254037844387076, 1.000000000000000000, 0.8660254037844387076, 1.000000000000000000, 0.8660254037844387076, 1.000000000000000000, 0.8660254037844387076, 1.000000000000000000, 0.8660254037844387076, 1.000000000000000000, 0.8660254037844387076, 1.000000000000000000, 0.8660254037844387076, 1.000000000000000000, 0.8660254037844387076, 1.000000000000000000, 0.8660254037844387076, 1.000000000000000000, 0.8660254037844387076, 1.000000000000000000, 0.8660254037844387076, 1.000000000000000000, 0.8660254037844387076, 1.000000000000000000, 0.8660254037844387076, 1.000000000000000000, 0.8660254037844387076, 1.000000000000000000, 0.8660254037844387076, 1.000000000000000000, 0.8660254037844387076, 1.000000000000000000, 0.8660254037844387076, 1.000000000000000000, 0.8660254037844387076, 1.000000000000000000, 0.8660254037844387076, 1.000000000000000000, 0.8660254037844387076, 1.000000000000000000, 0.8660254037844387076, 1.000000000000000000, 0.8660254037844387076, 1.000000000000000000, 0.8660254037844387076, 1.000000000000000000, 0.8660254037844387076, 1.000000000000000000, 0.8660254037844387076, 1.000000000000000000, 0.8660254037844387076, 1.000000000000000000, 0.8660254037844387076, 1.000000000000000000, 0.8660254037844387076, 1.000000000000000000, 0.8660254037844387076, 1.000000000000000000, 0.8660254037844387076, 1.000000000000000000, 0.8660254037844387076, 1.000000000000000000, 0.8660254037844387076, 1.000000000000000000, 0.8660254037844387076, 1.000000000000000000, 0.8660254037844387076, 1.000000000000000000, 0.8660254037844387076, 1.000000000000000000, 0.8660254037844387076, 1.000000000000000000, 0.8660254037844387076, 1.000000000000000000, 0.8660254037844387076, 1.000000000000000000, 0.8660254037844387076, 1.000000000000000000, 0.8660254037844387076, 1.000000000000000000, 0.8660254037844387076, 1.000000000000000000, 0.8660254037844387076, 1.000000000000000000, 0.8660254037844387076, 1.000000000000000000, 0.8660254037844387076, 1.000000000000000000, 0.8660254037844387076, 1.000000000000000000, 0.8660254037844387076, 1.000000000000000000, 0.8660254037844387076, 1.000000000000000000, 0.8660254037844387076, 1.000000000000000000, 0.8660254037844387076, 1.000000000000000000, 0.8660254037844387076, 1.000000000000000000, 0.8660254037844387076, 1.000000000000000000, 0.8660254037844387076, 1.000000000000000000, 0.8660254037844387076, 1.000000000000000000, 0.8660254037844387076, 1.000000000000000000, 0.8660254037844387076, 1.000000000000000000, 0.8660254037844387076, 1.000000000000000000, 0.8660254037844387076, 1.000000000000000000, 0.8660254037844387076, 1.000000000000000000, 0.8660254037844387076, 1.000000000000000000, 0.8660254037844387076, 1.000000000000000000, 0.8660254037844387076, 1.000000000000000000, 0.8660254037844387076, 1.000000000000000000, 0.8660254037844387076, 1.000000000000000000, 0.8660254037844387076, 1.000000000000000000, 0.8660254037844387076, 1.000000000000000000, 0.8660254037844387076, 1.000000000000000000, 0.8660254037844387076, 1.000000000000000000, 0.8660254037844387076, 1.000000000000000000, 0.8660254037844387076, 1.000000000000000000, 0.8660254037844387076, 1.000000000000000000, 0.8660254037844387076, 1.000000000000000000, 0.8660254037844387076, 1.000000000000000000, 0.8660254037844387076, 1.000000000000000000, 0.8660254037844387076, 1.000000000000000000, 0.8660254037844387076, 1.000000000000000000, 0.8660254037844387076, 1.000000000000000000, 0.8660254037844387076, 1.000000000000000000, 0.8660254037844387076, 1.000000000000000000, 0.8660254037844387076, 1.000000000000000000, 0.8660254037844387076, 1.000000000000000000, 0.8660254037844387076, 1.000000000000000000, 0.8660254037844387076, 1.000000000000000000, 0.8660254037844387076, 1.000000000000000000, 0.8660254037844387076, 1.000000000000000000, 0.8660254037844387076, 1.000000000000000000, 0.8660254037844387076, 1.000000000000000000, 0.8660254037844387076, 1.000000000000000000, 0.8660254037844387076, 1.000000000000000000, 0.8660254037844387076, 1.000000000000000000, 0.8660254037844387076, 1.000000000000000000, 0.8660254037844387076, 1.000000000000000000, 0.8660254037844387076, 1.000000000000000000, 0.8660254037844387076, 1.000000000000000000, 0.8660254037844387076, 1.000000000000000000, 0.8660254037844387076, 1.000000000000000000, 0.8660254037844387076, 1.000000000000000000, 0.8660254037844387076, 1.000000000000000000, 0.8660254037844387076, 1.000000000000000000, 0.8660254037844387076, 1.000000000000000000, 0.8660254037844387076, 1.000000000000000000, 0.8660254037844387076, 1.000000000000000000, 0.8660254037844387076, 1.000000000000000000, 0.8660254037844387076, 1.000000000000000000, 0.8660254037844387076, 1.000000000000000000, 0.8660254037844387076, 1.000000000000000000, 0.8660254037844387076, 1.000000000000000000, 0.8660254037844387076, 1.000000000000000000, 0.8660254037844387076, 1.000000000000000000, 0.8660254037844387076, 1.000000000000000000, 0.8660254037844387076, 1.000000000000000000, 0.8660254037844387076, 1.000000000000000000, 0.8660254037844387076, 1.000000000000000000, 0.8660254037844387076, 1.000000000000000000, 0.8660254037844387076, 1.000000000000000000, 0.8660254037844387076, 1.000000000000000000, 0.8660254037844387076, 1.000000000000000000, 0.8660254037844387076, 1.000000000000000000, 0.8660254037844387076, 1.000000000000000000, 0.8660254037844387076, 1.000000000000000000, 0.8660254037844387076, 1.000000000000000000, 0.8660254037844387076, 1.000000000000000000, 0.8660254037844387076, 1.000000000000000000, 0.8660254037844387076, 1.000000000000000000, 0.8660254037844387076, 1.000000000000000000, 0.8660254037844387076, 1.000000000000000000, 0.8660254037844387076, 1.000000000000000000, 0.8660254037844387076, 1.000000000000000000, 0.8660254037844387076, 1.000000000000000000, 0.8660254037844387076, 1.000000000000000000, 0.8660254037844387076, 1.000000000000000000, 0.8660254037844387076, 1.000000000000000000, 0.8660254037844387076, 1.000000000000000000, 0.8660254037844387076, 1.000000000000000000, 0.8660254037844387076, 1.000000000000000000, 0.8660254037844387076, 1.000000000000000000, 0.8660254037844387076, 1.000000000000000000, 0.8660254037844387076, 1.000000000000000000, 0.8660254037844387076, 1.000000000000000000, 0.8660254037844387076, 1.000000000000000000, 0.8660254037844387076, 1.000000000000000000, 0.8660254037844387076, 1.000000000000000000, 0.8660254037844387076, 1.000000000000000000, 0.8660254037844387076, 1.000000000000000000, 0.8660254037844387076, 1.000000000000000000, 0.8660254037844387076, 1.000000000000000000, 0.8660254037844387076, 1.000000000000000000, 0.8660254037844387076, 1.000000000000000000, 0.8660254037844387076, 1.000000000000000000, 0.8660254037844387076, 1.000000000000000000, 0.8660254037844387076, 1.000000000000000000, 0.8660254037844387076, 1.000000000000000000, 0.8660254037844387076, 1.000000000000000000, 0.8660254037844387076, 1.000000000000000000, 0.8660254037844387076, 1.000000000000000000, 0.8660254037844387076, 1.000000000000000000, 0.8660254037844387076, 1.000000000000000000, 0.8660254037844387076, 1.000000000000000000, 0.8660254037844387076, 1.000000000000000000, 0.8660254037844387076, 1.000000000000000000, 0.8660254037844387076, 1.000000000000000000, 0.8660254037844387076, 1.000000000000000000, 0.8660254037844387076, 1.000000000000000000, 0.8660254037844387076, 1.000000000000000000, 0.8660254037844387076, 1.000000000000000000, 0.8660254037844387076, 1.000000000000000000, 0.8660254037844387076, 1.000000000000000000, 0.8660254037844387076, 1.000000000000000000, 0.8660254037844387076, 1.000000000000000000, 0.8660254037844387076, 1.000000000000000000, 0.8660254037844387076, 1.000000000000000000, 0.8660254037844387076, 1.000000000000000000, 0.8660254037844387076, 1.000000000000000000, 0.8660254037844387076, 1.000000000000000000, 0.8660254037844387076, 1.000000000000000000, 0.8660254037844387076, 1.000000000000000000, 0.8660254037844387076, 1.000000000000000000, 0.8660254037844387076, 1.000000000000000000, 0.8660254037844387076, 1.000000000000000000, 0.8660254037844387076, 1.000000000000000000, 0.8660254037844387076, 1.000000000000000000, 0.8660254037844387076, 1.000000000000000000, 0.8660254037844387076, 1.000000000000000000, 0.8660254037844387076, 1.000000000000000000, 0.8660254037844387076, 1.000000000000000000, 0.8660254037844387076, 1.000000000000000000, 0.8660254037844387076, 1.000000000000000000, 0.8660254037844387076, 1.000000000000000000, 0.8660254037844387076, 1.000000000000000000, 0.8660254037844387076, 1.000000000000000000, 0.8660254037844387076, 1.000000000000000000, 0.8660254037844387076, 1.000000000000000000, 0.8660254037844387076, 1.000000000000000000, 0.8660254037844387076, 1.000000000000000000, 0.8660254037844387076, 1.000000000000000000, 0.8660254037844387076, 1.000000000000000000, 0.8660254037844387076, 1.000000000000000000, 0.8660254037844387076, 1.000000000000000000, 0.8660254037844387076, 1.000000000000000000, 0.8660254037844387076, 1.000000000000000000, 0.8660254037844387076, 1.000000000000000000, 0.8660254037844387076, 1.000000000000000000, 0.8660254037844387076, 1.000000000000000000, 0.8660254037844387076, 1.000000000000000000, 0.8660254037844387076, 1.000000000000000000, 0.8660254037844387076, 1.000000000000000000, 0.8660254037844387076, 1.000000000000000000, 0.8660254037844387076, 1.000000000000000000, 0.8660254037844387076, 1.000000000000000000, 0.8660254037844387076, 1.000000000000000000, 0.8660254037844387076, 1.000000000000000000, 0.8660254037844387076, 1.000000000000000000, 0.8660254037844387076, 1.000000000000000000, 0.8660254037844387076, 1.000000000000000000, 0.8660254037844387076, 1.000000000000000000, 0.8660254037844387076, 1.000000000000000000, 0.8660254037844387076, 1.000000000000000000, 0.8660254037844387076, 1.000000000000000000, 0.8660254037844387076, 1.000000000000000000, 0.8660254037844387076, 1.000000000000000000, 0.8660254037844387076, 1.000000000000000000, 0.8660254037844387076, 1.000000000000000000, 0.8660254037844387076, 1.000000000000000000, 0.8660254037844387076, 1.000000000000000000, 0.8660254037844387076, 1.000000000000000000, 0.8660254037844387076, 1.000000000000000000, 0.8660254037844387076, 1.000000000000000000, 0.8660254037844387076, 1.000000000000000000, 0.8660254037844387076, 1.000000000000000000, 0.8660254037844387076, 1.000000000000000000, 0.8660254037844387076, 1.000000000000000000, 0.8660254037844387076, 1.000000000000000000, 0.8660254037844387076, 1.000000000000000000, 0.8660254037844387076, 1.000000000000000000, 0.8660254037844387076, 1.000000000000000000, 0.8660254037844387076, 1.000000000000000000, 0.8660254037844387076, 1.000000000000000000, 0.8660254037844387076, 1.000000000000000000, 0.8660254037844387076, 1.000000000000000000, 0.8660254037844387076, 1.000000000000000000, 0.8660254037844387076, 1.000000000000000000, 0.8660254037844387076, 1.000000000000000000, 0.8660254037844387076, 1.000000000000000000, 0.8660254037844387076, 1.000000000000000000, 0.8660254037844387076, 1.000000000000000000, 0.8660254037844387076, 1.000000000000000000, 0.8660254037844387076, 1.000000000000000000, 0.8660254037844387076, 1.000000000000000000, 0.8660254037844387076, 1.000000000000000000, 0.8660254037844387076, 1.000000000000000000, 0.8660254037844387076, 1.000000000000000000, 0.8660254037844387076, 1.000000000000000000, 0.8660254037844387076, 1.000000000000000000, 0.8660254037844387076, 1.000000000000000000, 0.8660254037844387076, 1.000000000000000000, 0.8660254037844387076, 1.000000000000000000, 0.8660254037844387076, 1.000000000000000000, 0.8660254037844387076, 1.000000000000000000, 0.8660254037844387076, 1.000000000000000000, 0.8660254037844387076, 1.000000000000000000, 0.8660254037844387076, 1.000000000000000000, 0.8660254037844387076, 1.000000000000000000, 0.8660254037844387076, 1.000000000000000000, 0.8660254037844387076, 1.000000000000000000, 0.8660254037844387076, 1.000000000000000000, 0.8660254037844387076, 1.000000000000000000, 0.8660254037844387076, 1.000000000000000000, 0.8660254037844387076, 1.000000000000000000, 0.8660254037844387076, 1.000000000000000000, 0.8660254037844387076, 1.000000000000000000, 0.8660254037844387076, 1.000000000000000000, 0.8660254037844387076, 1.000000000000000000, 0.8660254037844387076, 1.000000000000000000, 0.8660254037844387076, 1.000000000000000000, 0.8660254037844387076, 1.000000000000000000, 0.8660254037844387076, 1.000000000000000000, 0.8660254037844387076, 1.000000000000000000, 0.8660254037844387076, 1.000000000000000000, 0.8660254037844387076, 1.000000000000000000, 0.8660254037844387076, 1.000000000000000000, 0.8660254037844387076, 1.000000000000000000, 0.8660254037844387076, 1.000000000000000000, 0.8660254037844387076, 1.000000000000000000, 0.8660254037844387076, 1.000000000000000000, 0.8660254037844387076, 1.000000000000000000, 0.8660254037844387076, 1.000000000000000000, 0.8660254037844387076, 1.000000000000000000, 0.8660254037844387076, 1.000000000000000000, 0.8660254037844387076, 1.000000000000000000, 0.8660254037844387076, 1.000000000000000000, 0.8660254037844387076, 1.000000000000000000, 0.8660254037844387076, 1.000000000000000000, 0.8660254037844387076, 1.000000000000000000, 0.8660254037844387076, 1.000000000000000000, 0.8660254037844387076, 1.000000000000000000, 0.8660254037844387076, 1.000000000000000000, 0.8660254037844387076, 1.000000000000000000, 0.8660254037844387076, 1.000000000000000000, 0.8660254037844387076, 1.000000000000000000, 0.8660254037844387076, 1.000000000000000000, 0.8660254037844387076, 1.000000000000000000, 0.8660254037844387076, 1.000000000000000000, 0.8660254037844387076, 1.000000000000000000, 0.8660254037844387076, 1.000000000000000000, 0.8660254037844387076, 1.000000000000000000, 0.8660254037844387076, 1.000000000000000000, 0.8660254037844387076, 1.000000000000000000, 0.8660254037844387076, 1.000000000000000000, 0.8660254037844387076, 1.000000000000000000, 0.8660254037844387076, 1.000000000000000000, 0.8660254037844387076, 1.000000000000000000, 0.8660254037844387076, 1.000000000000000000, 0.8660254037844387076, 1.000000000000000000, 0.8660254037844387076, 1.000000000000000000, 0.8660254037844387076, 1.000000000000000000, 0.8660254037844387076, 1.000000000000000000, 0.8660254037844387076, 1.000000000000000000, 0.8660254037844387076, 1.000000000000000000, 0.8660254037844387076, 1.000000000000000000, 0.8660254037844387076, 1.000000000000000000, 0.8660254037844387076, 1.000000000000000000, 0.8660254037844387076, 1.000000000000000000, 0.8660254037844387076, 1.000000000000000000, 0.8660254037844387076, 1.000000000000000000, 0.8660254037844387076, 1.000000000000000000, 0.8660254037844387076, 1.000000000000000000, 0.8660254037844387076, 1.000000000000000000, 0.8660254037844387076, 1.000000000000000000, 0.8660254037844387076, 1.000000000000000000, 0.8660254037844387076, 1.000000000000000000, 0.8660254037844387076, 1.000000000000000000, 0.8660254037844387076, 1.000000000000000000, 0.8660254037844387076, 1.000000000000000000, 0.8660254037844387076, 1.000000000000000000, 0.8660254037844387076, 1.000000000000000000, 0.8660254037844387076, 1.000000000000000000, 0.8660254037844387076, 1.000000000000000000, 0.8660254037844387076, 1.000000000000000000, 0.8660254037844387076, 1.000000000000000000, 0.8660254037844387076, 1.000000000000000000, 0.8660254037844387076, 1.000000000000000000, 0.8660254037844387076, 1.000000000000000000, 0.8660254037844387076, 1.000000000000000000, 0.8660254037844387076, 1.000000000000000000, 0.8660254037844387076, 1.000000000000000000, 0.8660254037844387076, 1.000000000000000000, 0.8660254037844387076, 1.000000000000000000, 0.8660254037844387076, 1.000000000000000000, 0.8660254037844387076, 1.000000000000000000, 0.8660254037844387076, 1.000000000000000000, 0.8660254037844387076, 1.000000000000000000),
 ( 1.000000000000000000, 0.8660254037844387076, 1.000000000000000000, 0.8660254037844387076, 1.000000000000000000, 0.8660254037844387076, 1.000000000000000000, 0.8660254037844387076, 1.000000000000000000, 0.8660254037844387076, 1.000000000000000000, 0.8660254037844387076, 1.000000000000000000, 0.8660254037844387076, 1.000000000000000000, 0.8660254037844387076, 1.000000000000000000, 0.8660254037844387076, 1.000000000000000000, 0.8660254037844387076, 1.000000000000000000, 0.8660254037844387076, 1.000000000000000000, 0.8660254037844387076, 1.000000000000000000, 0.8660254037844387076, 1.000000000000000000, 0.8660254037844387076, 1.000000000000000000, 0.8660254037844387076, 1.000000000000000000, 0.8660254037844387076, 1.000000000000000000, 0.8660254037844387076, 1.000000000000000000, 0.8660254037844387076, 1.000000000000000000, 0.8660254037844387076, 1.000000000000000000, 0.8660254037844387076, 1.000000000000000000, 0.8660254037844387076, 1.000000000000000000, 0.8660254037844387076, 1.000000000000000000, 0.8660254037844387076, 1.000000000000000000, 0.8660254037844387076, 1.000000000000000000, 0.8660254037844387076, 1.000000000000000000, 0.8660254037844387076, 1.000000000000000000, 0.8660254037844387076, 1.000000000000000000, 0.8660254037844387076, 1.000000000000000000, 0.8660254037844387076, 1.000000000000000000, 0.8660254037844387076, 1.000000000000000000, 0.8660254037844387076, 1.000000000000000000, 0.8660254037844387076, 1.000000000000000000, 0.8660254037844387076, 1.000000000000000000, 0.8660254037844387076, 1.000000000000000000, 0.8660254037844387076, 1.000000000000000000, 0.8660254037844387076, 1.000000000000000000, 0.8660254037844387076, 1.000000000000000000, 0.8660254037844387076, 1.000000000000000000, 0.8660254037844387076, 1.000000000000000000, 0.8660254037844387076, 1.000000000000000000, 0.8660254037844387076, 1.000000000000000000, 0.8660254037844387076, 1.000000000000000000, 0.8660254037844387076, 1.000000000000000000, 0.8660254037844387076, 1.000000000000000000, 0.8660254037844387076, 1.000000000000000000, 0.8660254037844387076, 1.000000000000000000, 0.8660254037844387076, 1.000000000000000000, 0.8660254037844387076, 1.000000000000000000, 0.8660254037844387076, 1.000000000000000000, 0.8660254037844387076, 1.000000000000000000, 0.8660254037844387076, 1.000000000000000000, 0.8660254037844387076, 1.000000000000000000, 0.8660254037844387076, 1.000000000000000000, 0.8660254037844387076, 1.000000000000000000, 0.8660254037844387076, 1.000000000000000000, 0.8660254037844387076, 1.000000000000000000, 0.8660254037844387076, 1.000000000000000000, 0.8660254037844387076, 1.000000000000000000, 0.8660254037844387076, 1.000000000000000000, 0.8660254037844387076, 1.000000000000000000, 0.8660254037844387076, 1.000000000000000000, 0.8660254037844387076, 1.000000000000000000, 0.8660254037844387076, 1.000000000000000000, 0.8660254037844387076, 1.000000000000000000, 0.8660254037844387076, 1.000000000000000000, 0.8660254037844387076, 1.000000000000000000, 0.8660254037844387076, 1.000000000000000000, 0.8660254037844387076, 1.000000000000000000, 0.8660254037844387076, 1.000000000000000000, 0.8660254037844387076, 1.000000000000000000, 0.8660254037844387076, 1.000000000000000000, 0.8660254037844387076, 1.000000000000000000, 0.8660254037844387076, 1.000000000000000000, 0.8660254037844387076, 1.000000000000000000, 0.8660254037844387076, 1.000000000000000000, 0.8660254037844387076, 1.000000000000000000, 0.8660254037844387076, 1.000000000000000000, 0.8660254037844387076, 1.000000000000000000, 0.8660254037844387076, 1.000000000000000000, 0.8660254037844387076, 1.000000000000000000, 0.8660254037844387076, 1.000000000000000000, 0.8660254037844387076, 1.000000000000000000, 0.8660254037844387076, 1.000000000000000000, 0.8660254037844387076, 1.000000000000000000, 0.8660254037844387076, 1.000000000000000000, 0.8660254037844387076, 1.000000000000000000, 0.8660254037844387076, 1.000000000000000000, 0.8660254037844387076, 1.000000000000000000, 0.8660254037844387076, 1.000000000000000000, 0.8660254037844387076, 1.000000000000000000, 0.8660254037844387076, 1.000000000000000000, 0.8660254037844387076, 1.000000000000000000, 0.8660254037844387076, 1.000000000000000000, 0.8660254037844387076, 1.000000000000000000, 0.8660254037844387076, 1.000000000000000000, 0.8660254037844387076, 1.000000000000000000, 0.8660254037844387076, 1.000000000000000000, 0.8660254037844387076, 1.000000000000000000, 0.8660254037844387076, 1.000000000000000000, 0.8660254037844387076, 1.000000000000000000, 0.8660254037844387076, 1.000000000000000000, 0.8660254037844387076, 1.000000000000000000, 0.8660254037844387076, 1.000000000000000000, 0.8660254037844387076, 1.000000000000000000, 0.8660254037844387076, 1.000000000000000000, 0.8660254037844387076, 1.000000000000000000, 0.8660254037844387076, 1.000000000000000000, 0.8660254037844387076, 1.000000000000000000, 0.8660254037844387076, 1.000000000000000000, 0.8660254037844387076, 1.000000000000000000, 0.8660254037844387076, 1.000000000000000000, 0.8660254037844387076, 1.000000000000000000, 0.8660254037844387076, 1.000000000000000000, 0.8660254037844387076, 1.000000000000000000, 0.8660254037844387076, 1.000000000000000000, 0.8660254037844387076, 1.000000000000000000, 0.8660254037844387076, 1.000000000000000000, 0.8660254037844387076, 1.000000000000000000, 0.8660254037844387076, 1.000000000000000000, 0.8660254037844387076, 1.000000000000000000, 0.8660254037844387076, 1.000000000000000000, 0.8660254037844387076, 1.000000000000000000, 0.8660254037844387076, 1.000000000000000000, 0.8660254037844387076, 1.000000000000000000, 0.8660254037844387076, 1.000000000000000000, 0.8660254037844387076, 1.000000000000000000, 0.8660254037844387076, 1.000000000000000000, 0.8660254037844387076, 1.000000000000000000, 0.8660254037844387076, 1.000000000000000000, 0.8660254037844387076, 1.000000000000000000, 0.8660254037844387076, 1.000000000000000000, 0.8660254037844387076, 1.000000000000000000, 0.8660254037844387076, 1.000000000000000000, 0.8660254037844387076, 1.000000000000000000, 0.8660254037844387076, 1.000000000000000000, 0.8660254037844387076, 1.000000000000000000, 0.8660254037844387076, 1.000000000000000000, 0.8660254037844387076, 1.000000000000000000, 0.8660254037844387076, 1.000000000000000000, 0.8660254037844387076, 1.000000000000000000, 0.8660254037844387076, 1.000000000000000000, 0.8660254037844387076, 1.000000000000000000, 0.8660254037844387076, 1.000000000000000000, 0.8660254037844387076, 1.000000000000000000, 0.8660254037844387076, 1.000000000000000000, 0.8660254037844387076, 1.000000000000000000, 0.8660254037844387076, 1.000000000000000000, 0.8660254037844387076, 1.000000000000000000, 0.8660254037844387076, 1.000000000000000000, 0.8660254037844387076, 1.000000000000000000, 0.8660254037844387076, 1.000000000000000000, 0.8660254037844387076, 1.000000000000000000, 0.8660254037844387076, 1.000000000000000000, 0.8660254037844387076, 1.000000000000000000, 0.8660254037844387076, 1.000000000000000000, 0.8660254037844387076, 1.000000000000000000, 0.8660254037844387076, 1.000000000000000000, 0.8660254037844387076, 1.000000000000000000, 0.8660254037844387076, 1.000000000000000000, 0.8660254037844387076, 1.000000000000000000, 0.8660254037844387076, 1.000000000000000000, 0.8660254037844387076, 1.000000000000000000, 0.8660254037844387076, 1.000000000000000000, 0.8660254037844387076, 1.000000000000000000, 0.8660254037844387076, 1.000000000000000000, 0.8660254037844387076, 1.000000000000000000, 0.8660254037844387076, 1.000000000000000000, 0.8660254037844387076, 1.000000000000000000, 0.8660254037844387076, 1.000000000000000000, 0.8660254037844387076, 1.000000000000000000, 0.8660254037844387076, 1.000000000000000000, 0.8660254037844387076, 1.000000000000000000, 0.8660254037844387076, 1.000000000000000000, 0.8660254037844387076, 1.000000000000000000, 0.8660254037844387076, 1.000000000000000000, 0.8660254037844387076, 1.000000000000000000, 0.8660254037844387076, 1.000000000000000000, 0.8660254037844387076, 1.000000000000000000, 0.8660254037844387076, 1.000000000000000000, 0.8660254037844387076, 1.000000000000000000, 0.8660254037844387076, 1.000000000000000000, 0.8660254037844387076, 1.000000000000000000, 0.8660254037844387076, 1.000000000000000000, 0.8660254037844387076, 1.000000000000000000, 0.8660254037844387076, 1.000000000000000000, 0.8660254037844387076, 1.000000000000000000, 0.8660254037844387076, 1.000000000000000000, 0.8660254037844387076, 1.000000000000000000, 0.8660254037844387076, 1.000000000000000000, 0.8660254037844387076, 1.000000000000000000, 0.8660254037844387076, 1.000000000000000000, 0.8660254037844387076, 1.000000000000000000, 0.8660254037844387076, 1.000000000000000000, 0.8660254037844387076, 1.000000000000000000, 0.8660254037844387076, 1.000000000000000000, 0.8660254037844387076, 1.000000000000000000, 0.8660254037844387076, 1.000000000000000000, 0.8660254037844387076, 1.000000000000000000, 0.8660254037844387076, 1.000000000000000000, 0.8660254037844387076, 1.000000000000000000, 0.8660254037844387076, 1.000000000000000000, 0.8660254037844387076, 1.000000000000000000, 0.8660254037844387076, 1.000000000000000000, 0.8660254037844387076, 1.000000000000000000, 0.8660254037844387076, 1.000000000000000000, 0.8660254037844387076, 1.000000000000000000, 0.8660254037844387076, 1.000000000000000000, 0.8660254037844387076, 1.000000000000000000, 0.8660254037844387076, 1.000000000000000000, 0.8660254037844387076, 1.000000000000000000, 0.8660254037844387076, 1.000000000000000000, 0.8660254037844387076, 1.000000000000000000, 0.8660254037844387076, 1.000000000000000000, 0.8660254037844387076, 1.000000000000000000, 0.8660254037844387076, 1.000000000000000000, 0.8660254037844387076, 1.000000000000000000, 0.8660254037844387076, 1.000000000000000000, 0.8660254037844387076, 1.000000000000000000, 0.8660254037844387076, 1.000000000000000000, 0.8660254037844387076, 1.000000000000000000, 0.8660254037844387076, 1.000000000000000000, 0.8660254037844387076, 1.000000000000000000, 0.8660254037844387076, 1.000000000000000000, 0.8660254037844387076, 1.000000000000000000, 0.8660254037844387076, 1.000000000000000000, 0.8660254037844387076, 1.000000000000000000, 0.8660254037844387076, 1.000000000000000000, 0.8660254037844387076, 1.000000000000000000, 0.8660254037844387076, 1.000000000000000000, 0.8660254037844387076, 1.000000000000000000, 0.8660254037844387076, 1.000000000000000000, 0.8660254037844387076, 1.000000000000000000, 0.8660254037844387076, 1.000000000000000000, 0.8660254037844387076, 1.000000000000000000, 0.8660254037844387076, 1.000000000000000000, 0.8660254037844387076, 1.000000000000000000, 0.8660254037844387076, 1.000000000000000000, 0.8660254037844387076, 1.000000000000000000, 0.8660254037844387076, 1.000000000000000000, 0.8660254037844387076, 1.000000000000000000, 0.8660254037844387076, 1.000000000000000000, 0.8660254037844387076, 1.000000000000000000, 0.8660254037844387076, 1.000000000000000000, 0.8660254037844387076, 1.000000000000000000, 0.8660254037844387076, 1.000000000000000000, 0.8660254037844387076, 1.000000000000000000, 0.8660254037844387076, 1.000000000000000000, 0.8660254037844387076, 1.000000000000000000, 0.8660254037844387076, 1.000000000000000000, 0.8660254037844387076, 1.000000000000000000, 0.8660254037844387076, 1.000000000000000000, 0.8660254037844387076, 1.000000000000000000, 0.8660254037844387076, 1.000000000000000000, 0.8660254037844387076, 1.000000000000000000, 0.8660254037844387076, 1.000000000000000000, 0.8660254037844387076, 1.000000000000000000, 0.8660254037844387076, 1.000000000000000000, 0.8660254037844387076, 1.000000000000000000, 0.8660254037844387076, 1.000000000000000000, 0.8660254037844387076, 1.000000000000000000, 0.8660254037844387076, 1.000000000000000000, 0.8660254037844387076, 1.000000000000000000, 0.8660254037844387076, 1.000000000000000000, 0.8660254037844387076, 1.000000000000000000, 0.8660254037844387076, 1.000000000000000000, 0.8660254037844387076, 1.000000000000000000, 0.8660254037844387076, 1.000000000000000000, 0.8660254037844387076, 1.000000000000000000, 0.8660254037844387076, 1.000000000000000000, 0.8660254037844387076, 1.000000000000000000, 0.8660254037844387076, 1.000000000000000000, 0.8660254037844387076, 1.000000000000000000, 0.8660254037844387076, 1.000000000000000000, 0.8660254037844387076, 1.000000000000000000, 0.8660254037844387076, 1.000000000000000000, 0.8660254037844387076, 1.000000000000000000, 0.8660254037844387076, 1.000000000000000000, 0.8660254037844387076, 1.000000000000000000, 0.8660254037844387076, 1.000000000000000000, 0.8660254037844387076, 1.000000000000000000, 0.8660254037844387076, 1.000000000000000000, 0.8660254037844387076, 1.000000000000000000, 0.8660254037844387076, 1.000000000000000000, 0.8660254037844387076, 1.000000000000000000, 0.8660254037844387076, 1.000000000000000000, 0.8660254037844387076, 1.000000000000000000, 0.8660254037844387076, 1.000000000000000000, 0.8660254037844387076, 1.000000000000000000, 0.8660254037844387076, 1.000000000000000000, 0.8660254037844387076, 1.000000000000000000, 0.8660254037844387076, 1.000000000000000000, 0.8660254037844387076, 1.000000000000000000, 0.8660254037844387076, 1.000000000000000000, 0.8660254037844387076, 1.000000000000000000, 0.8660254037844387076, 1.000000000000000000, 0.8660254037844387076, 1.000000000000000000, 0.8660254037844387076, 1.000000000000000000, 0.8660254037844387076, 1.000000000000000000, 0.8660254037844387076, 1.000000000000000000, 0.8660254037844387076, 1.000000000000000000, 0.8660254037844387076, 1.000000000000000000, 0.8660254037844387076, 1.000000000000000000, 0.8660254037844387076, 1.000000000000000000, 0.8660254037844387076, 1.000000000000000000, 0.8660254037844387076, 1.000000000000000000, 0.8660254037844387076, 1.000000000000000000, 0.8660254037844387076, 1.000000000000000000, 0.8660254037844387076, 1.000000000000000000, 0.8660254037844387076, 1.000000000000000000, 0.8660254037844387076, 1.000000000000000000, 0.8660254037844387076, 1.000000000000000000, 0.8660254037844387076, 1.000000000000000000, 0.8660254037844387076, 1.000000000000000000, 0.8660254037844387076, 1.000000000000000000, 0.8660254037844387076, 1.000000000000000000, 0.8660254037844387076, 1.000000000000000000, 0.8660254037844387076, 1.000000000000000000, 0.8660254037844387076, 1.000000000000000000, 0.8660254037844387076, 1.000000000000000000, 0.8660254037844387076, 1.000000000000000000, 0.8660254037844387076, 1.000000000000000000, 0.8660254037844387076, 1.000000000000000000, 0.8660254037844387076, 1.000000000000000000, 0.8660254037844387076, 1.000000000000000000, 0.8660254037844387076, 1.000000000000000000, 0.8660254037844387076, 1.000000000000000000, 0.8660254037844387076, 1.000000000000000000, 0.8660254037844387076, 1.000000000000000000, 0.8660254037844387076, 1.000000000000000000, 0.8660254037844387076, 1.000000000000000000, 0.8660254037844387076, 1.000000000000000000, 0.8660254037844387076, 1.000000000000000000, 0.8660254037844387076, 1.000000000000000000, 0.8660254037844387076, 1.000000000000000000, 0.8660254037844387076, 1.000000000000000000, 0.8660254037844387076, 1.000000000000000000, 0.8660254037844387076, 1.000000000000000000, 0.8660254037844387076, 1.000000000000000000, 0.8660254037844387076, 1.000000000000000000, 0.8660254037844387076, 1.000000000000000000, 0.8660254037844387076, 1.000000000000000000, 0.8660254037844387076, 1.000000000000000000, 0.8660254037844387076, 1.000000000000000000, 0.8660254037844387076, 1.000000000000000000, 0.8660254037844387076, 1.000000000000000000, 0.8660254037844387076, 1.000000000000000000, 0.8660254037844387076, 1.000000000000000000, 0.8660254037844387076, 1.000000000000000000, 0.8660254037844387076, 1.000000000000000000, 0.8660254037844387076, 1.000000000000000000, 0.8660254037844387076, 1.000000000000000000, 0.8660254037844387076, 1.000000000000000000, 0.8660254037844387076, 1.000000000000000000, 0.8660254037844387076, 1.000000000000000000, 0.8660254037844387076, 1.000000000000000000, 0.8660254037844387076, 1.000000000000000000, 0.8660254037844387076, 1.000000000000000000, 0.8660254037844387076, 1.000000000000000000, 0.8660254037844387076, 1.000000000000000000, 0.8660254037844387076, 1.000000000000000000, 0.8660254037844387076, 1.000000000000000000, 0.8660254037844387076, 1.000000000000000000, 0.8660254037844387076, 1.000000000000000000, 0.8660254037844387076, 1.000000000000000000, 0.8660254037844387076, 1.000000000000000000, 0.8660254037844387076, 1.000000000000000000, 0.8660254037844387076, 1.000000000000000000, 0.8660254037844387076, 1.000000000000000000, 0.8660254037844387076, 1.000000000000000000, 0.8660254037844387076, 1.000000000000000000, 0.8660254037844387076, 1.000000000000000000, 0.8660254037844387076, 1.000000000000000000) ) ) 
 REPRESENTATION_ITEM ( '' )  SURFACE ( )  );
#55485 = VERTEX_POINT ( 'NONE', #87294 ) ;
#55486 = CARTESIAN_POINT ( 'NONE',  ( 190.8222259996342700, 280.8384348826126597, 16.64285960788097896 ) ) ;
#55487 = CARTESIAN_POINT ( 'NONE',  ( 34.84170590957603508, 35.51421378149921537, -9.188101187500004485 ) ) ;
#55488 = DIRECTION ( 'NONE',  ( 0.3984034379158949979, -0.9172102815913020235, 0.000000000000000000 ) ) ;
#55489 = ORIENTED_EDGE ( 'NONE', *, *, #54135, .F. ) ;
#55490 = CARTESIAN_POINT ( 'NONE',  ( 164.2656921623427593, 279.4100564649723992, 11.98912045511763047 ) ) ;
#55491 = ADVANCED_FACE ( 'NONE', ( #17825 ), #72026, .T. ) ;
#55492 = CARTESIAN_POINT ( 'NONE',  ( 194.3708539535661259, 293.9868007723104029, -16.01585187499628304 ) ) ;
#55493 = CARTESIAN_POINT ( 'NONE',  ( 84.07632125876401119, 43.96420502296712840, -8.427032882940022063 ) ) ;
#55494 = ORIENTED_EDGE ( 'NONE', *, *, #71138, .T. ) ;
#55495 = CARTESIAN_POINT ( 'NONE',  ( 86.20597319207941212, 46.97128461232403396, -10.07072581233441610 ) ) ;
#55496 = LINE ( 'NONE', #10429, #11980 ) ;
#55497 = CARTESIAN_POINT ( 'NONE',  ( 61.08237637342866577, 217.6199935810940644, 2.679491924311251605 ) ) ;
#55498 = DIRECTION ( 'NONE',  ( -0.4055404667435467125, 0.9140770918436946779, 0.000000000000000000 ) ) ;
#55499 = DIRECTION ( 'NONE',  ( 0.5000000000000014433, -0.8660254037844378194, 0.000000000000000000 ) ) ;
#55500 = DIRECTION ( 'NONE',  ( -0.6201213960746324583, 0.7845058662179964504, 0.000000000000000000 ) ) ;
#55501 = VERTEX_POINT ( 'NONE', #41090 ) ;
#55502 = ORIENTED_EDGE ( 'NONE', *, *, #5138, .T. ) ;
#55503 = CARTESIAN_POINT ( 'NONE',  ( 194.9471474500919896, 290.9886311562445371, 16.55118206508679890 ) ) ;
#55504 = ORIENTED_EDGE ( 'NONE', *, *, #84999, .F. ) ;
#55505 = FACE_OUTER_BOUND ( 'NONE', #72847, .T. ) ;
#55506 = ORIENTED_EDGE ( 'NONE', *, *, #57133, .T. ) ;
#55507 = CARTESIAN_POINT ( 'NONE',  ( -10.54235908185773418, 24.92402704602492847, -10.00000000000000000 ) ) ;
#55508 = CARTESIAN_POINT ( 'NONE',  ( 78.31895580137157253, 49.37400206353071752, 14.66798886358647813 ) ) ;
#55509 = EDGE_LOOP ( 'NONE', ( #66993, #76826, #9545, #33750 ) ) ;
#55510 = CARTESIAN_POINT ( 'NONE',  ( 182.7187161720513870, 280.2422681844545309, -16.11425770197665130 ) ) ;
#55511 = CARTESIAN_POINT ( 'NONE',  ( 206.7074763235984562, 272.6191440336236838, -10.69202547607624609 ) ) ;
#55512 = CARTESIAN_POINT ( 'NONE',  ( 147.7698481346699566, 274.7021105344513217, -7.287563475572640392 ) ) ;
#55513 = CARTESIAN_POINT ( 'NONE',  ( 198.7408816115379864, 285.9624092822338071, -17.04496721243561197 ) ) ;
#55514 = CARTESIAN_POINT ( 'NONE',  ( 66.90909321525143127, 68.17756947874360662, -6.600776075497400974 ) ) ;
#55515 = DIRECTION ( 'NONE',  ( -0.8660254037844378194, -0.5000000000000014433, -0.000000000000000000 ) ) ;
#55516 = CARTESIAN_POINT ( 'NONE',  ( -58.11485369836745463, 56.56539583079995737, 59.99999999999999289 ) ) ;
#55517 = ADVANCED_FACE ( 'NONE', ( #64413 ), #91102, .F. ) ;
#55518 = PLANE ( 'NONE',  #66146 ) ;
#55519 = CARTESIAN_POINT ( 'NONE',  ( 132.1361044793229951, 247.0958772461660544, -9.188101187500095079 ) ) ;
#55520 = CARTESIAN_POINT ( 'NONE',  ( 186.4053619253457157, 262.6073444215381301, -9.037681140890068576 ) ) ;
#55521 = CARTESIAN_POINT ( 'NONE',  ( 38.02916716989017942, 40.14336893147758900, 7.433330006724141015 ) ) ;
#55522 = ORIENTED_EDGE ( 'NONE', *, *, #63690, .T. ) ;
#55523 = AXIS2_PLACEMENT_3D ( 'NONE', #15482, #23581, #8897 ) ;
#55525 = VERTEX_POINT ( 'NONE', #27900 ) ;
#55524 = CARTESIAN_POINT ( 'NONE',  ( 156.6168467568483891, 276.9391697405689001, 11.51099842983860633 ) ) ;
#55526 = LINE ( 'NONE', #93585, #9372 ) ;
#55527 = CARTESIAN_POINT ( 'NONE',  ( 178.6718079657368605, 253.5168414102466556, 1.418467519481931172 ) ) ;
#55528 = CARTESIAN_POINT ( 'NONE',  ( 174.0958964869310819, 290.5965046355827326, -4.902034896575071521 ) ) ;
#55529 = CARTESIAN_POINT ( 'NONE',  ( 190.3035812936891205, 300.3508029452809751, 2.075471296006329514 ) ) ;
#55530 = CARTESIAN_POINT ( 'NONE',  ( 72.76527857391883458, 64.58864651986012007, 13.32453080016684588 ) ) ;
#55531 = EDGE_CURVE ( 'NONE', #10673, #49297, #97824, .T. ) ;
#55532 = CARTESIAN_POINT ( 'NONE',  ( 152.7295469705997277, 266.1116601603806657, -17.40211458100010589 ) ) ;
#55533 = CARTESIAN_POINT ( 'NONE',  ( 78.96239046496309300, 54.80267053941222599, 16.44022611344569285 ) ) ;
#55534 = CARTESIAN_POINT ( 'NONE',  ( -19.65312891409028850, 79.99999999999991473, -54.99999999999999289 ) ) ;
#55535 = ADVANCED_FACE ( 'NONE', ( #66404 ), #51187, .T. ) ;
#55536 = CARTESIAN_POINT ( 'NONE',  ( 177.5477342733873058, 255.5783683057051974, -8.395856749569729160 ) ) ;
#55537 = ORIENTED_EDGE ( 'NONE', *, *, #47040, .T. ) ;
#55538 = CARTESIAN_POINT ( 'NONE',  ( 147.7785919239399846, 274.6869658471848652, -7.924750738206837397 ) ) ;
#55539 = LINE ( 'NONE', #32258, #81945 ) ;
#55540 = AXIS2_PLACEMENT_3D ( 'NONE', #68687, #20621, #92055 ) ;
#55541 = ORIENTED_EDGE ( 'NONE', *, *, #94392, .F. ) ;
#55542 = CARTESIAN_POINT ( 'NONE',  ( 188.2574254122442028, 265.6453801167639313, -11.59643318832059222 ) ) ;
#55543 = VECTOR ( 'NONE', #43297, 1000.000000000000000 ) ;
#55544 = CARTESIAN_POINT ( 'NONE',  ( 191.0385514471091142, 283.4162394903332256, -16.57259208637104564 ) ) ;
#55545 = CARTESIAN_POINT ( 'NONE',  ( 191.5041680634890326, 298.9520463832649284, -9.652406396186668402 ) ) ;
#55546 = CARTESIAN_POINT ( 'NONE',  ( 185.2824853868734181, 297.7695098558858149, 4.231266468330407093 ) ) ;
#55547 = CARTESIAN_POINT ( 'NONE',  ( 163.1332433029523372, 248.0919295262283981, 11.24052392390482957 ) ) ;
#55549 = CARTESIAN_POINT ( 'NONE',  ( 154.5748677679694651, 277.6768200149726908, -9.086954252033812907 ) ) ;
#55548 = CARTESIAN_POINT ( 'NONE',  ( 153.3453455745885776, 270.2083751330562791, 14.04681399919192764 ) ) ;
#55550 = CARTESIAN_POINT ( 'NONE',  ( 200.3729394803074797, 267.3312977064779830, 6.351288650702686667 ) ) ;
#55551 = ORIENTED_EDGE ( 'NONE', *, *, #99606, .T. ) ;
#55552 = CARTESIAN_POINT ( 'NONE',  ( 204.6993599598945650, 272.9423004453971089, -9.711292078056779076 ) ) ;
#55553 = B_SPLINE_SURFACE_WITH_KNOTS ( 'NONE', 3, 1, ( 
 ( #42875, #59578 ),
 ( #90554, #20615 ),
 ( #73808, #28702 ),
 ( #43890, #74829 ),
 ( #66694, #58584 ),
 ( #20119, #73322 ),
 ( #51496, #50990 ),
 ( #11530, #60077 ),
 ( #4402, #82466 ),
 ( #98116, #65695 ),
 ( #27219, #12019 ),
 ( #52001, #21124 ),
 ( #35299, #97150 ),
 ( #67700, #91040 ),
 ( #66211, #5898 ),
 ( #13027, #81940 ),
 ( #75320, #5409 ),
 ( #21607, #27716 ),
 ( #34792, #98628 ),
 ( #28195, #82944 ),
 ( #19633, #29208 ),
 ( #13517, #52487 ),
 ( #96649, #12518 ),
 ( #44385, #42389 ),
 ( #3911, #43390 ),
 ( #74333, #58102 ),
 ( #89084, #50493 ),
 ( #81447, #4921 ),
 ( #35800, #59071 ),
 ( #90042, #36292 ),
 ( #67193, #38272 ),
 ( #62565, #22092 ),
 ( #70175, #53482 ),
 ( #6889, #52990 ) ),
 .UNSPECIFIED., .T., .F., .F.,
 ( 4, 2, 2, 2, 2, 2, 2, 2, 2, 2, 2, 2, 2, 2, 2, 2, 4 ),
 ( 2, 2 ),
 ( 0.000000000000000000, 0.06250000000000000000, 0.1250000000000000000, 0.1875000000000000000, 0.2500000000000000000, 0.3125000000000000000, 0.3750000000000000000, 0.4375000000000000000, 0.5000000000000000000, 0.5625000000000000000, 0.6250000000000000000, 0.6875000000000000000, 0.7500000000000000000, 0.8125000000000000000, 0.8750000000000000000, 0.9375000000000000000, 1.000000000000000000 ),
 ( 0.000000000000000000, 1.000000000000000000 ),
 .UNSPECIFIED. ) ;
#55554 = CARTESIAN_POINT ( 'NONE',  ( 186.9700126462538776, 262.9196008017059398, -9.025915536625742419 ) ) ;
#55555 = CARTESIAN_POINT ( 'NONE',  ( 154.2351116723865232, 278.9542530893276648, 6.640610626432363439 ) ) ;
#55556 = CARTESIAN_POINT ( 'NONE',  ( 170.3290958195750022, 289.6815776661216546, -1.151831906498994140 ) ) ;
#55557 = CARTESIAN_POINT ( 'NONE',  ( 152.6757560589063303, 266.2048287524194166, 16.73757896668104195 ) ) ;
#55558 = CARTESIAN_POINT ( 'NONE',  ( 74.39896838111268096, 68.39356553035000275, 11.80479640254015195 ) ) ;
#55559 = CARTESIAN_POINT ( 'NONE',  ( 194.4889937320412230, 293.7821766735966662, 14.99892588346621380 ) ) ;
#55560 = CYLINDRICAL_SURFACE ( 'NONE', #22305, 17.82106496071139645 ) ;
#55561 = EDGE_CURVE ( 'NONE', #23462, #42521, #14375, .T. ) ;
#55562 = LINE ( 'NONE', #25699, #80303 ) ;
#55563 = CARTESIAN_POINT ( 'NONE',  ( 87.96880888631662287, 221.5958772461660544, -9.188101187500095079 ) ) ;
#55564 = CARTESIAN_POINT ( 'NONE',  ( -167.0327448629461742, 42.61639673982675447, 30.52142883766498116 ) ) ;
#55565 = CARTESIAN_POINT ( 'NONE',  ( -19.79482558122098013, 93.07102426866003952, 59.99999999999999289 ) ) ;
#55566 = DIRECTION ( 'NONE',  ( -0.4330127018922173554, -0.2499999999999980016, 0.8660254037844402619 ) ) ;
#55567 = CARTESIAN_POINT ( 'NONE',  ( 72.04834849415195208, 72.28436413801230742, -0.8995985284803106330 ) ) ;
#55568 = CARTESIAN_POINT ( 'NONE',  ( -35.23882338977090001, 123.3422401859822344, -12.33162903191226789 ) ) ;
#55569 = CARTESIAN_POINT ( 'NONE',  ( 125.9182562534771677, 255.0530062829863311, -4.648177544792955347E-16 ) ) ;
#55570 = DIRECTION ( 'NONE',  ( 0.4145187862775202015, -0.7179675985244525771, -0.5591929034707450175 ) ) ;
#55572 = CARTESIAN_POINT ( 'NONE',  ( 76.22210074466102014, 51.34659161545482675, 15.62784121295812767 ) ) ;
#55571 = CARTESIAN_POINT ( 'NONE',  ( 190.2138197578740630, 300.4348890635282601, -1.218754932262906321 ) ) ;
#55573 = CARTESIAN_POINT ( 'NONE',  ( 207.5768482435486817, 271.1133476975963390, 4.854912217663986951 ) ) ;
#55574 = EDGE_CURVE ( 'NONE', #61794, #7924, #96348, .T. ) ;
#55575 = CARTESIAN_POINT ( 'NONE',  ( 166.5514548696166628, 250.1203565289131916, -8.987830393236849957 ) ) ;
#55576 = CYLINDRICAL_SURFACE ( 'NONE', #1292, 17.82106496071139645 ) ;
#55577 = CARTESIAN_POINT ( 'NONE',  ( 196.3519702320103590, 290.5554067223432639, 17.39042812051341969 ) ) ;
#55578 = CARTESIAN_POINT ( 'NONE',  ( 190.0398248856338057, 298.8169614316505545, -8.166243001185458539 ) ) ;
#55579 = CARTESIAN_POINT ( 'NONE',  ( 22.87549206224920084, 39.05096577487528720, 10.00000000000000000 ) ) ;
#55580 = CARTESIAN_POINT ( 'NONE',  ( 40.58072100116311276, 203.4244531367911293, -4.594050593750046652 ) ) ;
#55581 = CARTESIAN_POINT ( 'NONE',  ( 68.45643432912224569, 201.1423013555409796, -4.594050593750043987 ) ) ;
#55582 = DIRECTION ( 'NONE',  ( -0.5000000000000001110, 0.8660254037844385966, 0.000000000000000000 ) ) ;
#55583 = CARTESIAN_POINT ( 'NONE',  ( 88.17984709959166878, 44.08761100535731714, 0.5351384936683012405 ) ) ;
#55584 = CARTESIAN_POINT ( 'NONE',  ( 167.1156311472931861, 259.7982583194432777, 15.94551010330511787 ) ) ;
#55586 = CARTESIAN_POINT ( 'NONE',  ( 202.6833006059332263, 277.5892208352050829, 15.45935665133711900 ) ) ;
#55585 = CARTESIAN_POINT ( 'NONE',  ( 198.6196860892239897, 286.2322653470183127, -17.00643444671568716 ) ) ;
#55587 = EDGE_CURVE ( 'NONE', #32613, #82087, #60005, .T. ) ;
#55588 = CARTESIAN_POINT ( 'NONE',  ( 199.8052201840724820, 271.0811423415471495, -11.18866198556676927 ) ) ;
#55589 = CARTESIAN_POINT ( 'NONE',  ( 26.89353023359722883, 24.03085787977764198, 9.188101187500006262 ) ) ;
#55590 = CARTESIAN_POINT ( 'NONE',  ( 198.7829547491859330, 286.3448180261817129, -18.59838968157616179 ) ) ;
#55591 = CARTESIAN_POINT ( 'NONE',  ( 80.73658319580380294, 47.53320970514121768, -13.02157490326441902 ) ) ;
#55592 = CARTESIAN_POINT ( 'NONE',  ( 15.22926075146606273, 30.83396525600389637, -2.839279412974133887 ) ) ;
#55593 = CARTESIAN_POINT ( 'NONE',  ( 66.66973629016931113, 218.4869531367911293, 4.594050593750046652 ) ) ;
#55594 = DIRECTION ( 'NONE',  ( -0.5000000000000013323, 0.8660254037844379305, 0.000000000000000000 ) ) ;
#55595 = DIRECTION ( 'NONE',  ( 0.8660254037844378194, 0.5000000000000015543, -0.000000000000000000 ) ) ;
#55596 = CARTESIAN_POINT ( 'NONE',  ( 198.5558597050348908, 286.7381581807989051, 17.16554469393394200 ) ) ;
#55597 = DIRECTION ( 'NONE',  ( 0.000000000000000000, 1.000000000000000000, 0.000000000000000000 ) ) ;
#55598 = CARTESIAN_POINT ( 'NONE',  ( 201.6857638146347256, 281.3170052401528665, 17.84391605515014945 ) ) ;
#55599 = AXIS2_PLACEMENT_3D ( 'NONE', #73981, #43556, #4565 ) ;
#55600 = CARTESIAN_POINT ( 'NONE',  ( 109.2134945746776538, 223.8615022471902023, 5.000000000000051514 ) ) ;
#55601 = CARTESIAN_POINT ( 'NONE',  ( 161.8016137473484548, 250.3983795733946636, 14.25000412375400316 ) ) ;
#55602 = CARTESIAN_POINT ( 'NONE',  ( 164.5416088356626290, 245.6525688679454618, -1.463507744092769292 ) ) ;
#55603 = ORIENTED_EDGE ( 'NONE', *, *, #94471, .T. ) ;
#55604 = AXIS2_PLACEMENT_3D ( 'NONE', #31064, #30581, #76683 ) ;
#55605 = CARTESIAN_POINT ( 'NONE',  ( 77.69869663927875081, 49.40449606496737545, 15.31866489331840420 ) ) ;
#55606 = CARTESIAN_POINT ( 'NONE',  ( 186.0400780920065529, 271.7087950812899066, 16.90619359840448510 ) ) ;
#55607 = ORIENTED_EDGE ( 'NONE', *, *, #59099, .F. ) ;
#55608 = CARTESIAN_POINT ( 'NONE',  ( 159.2102594322688844, 254.8867369075254885, -16.13039487917589199 ) ) ;
#55609 = CARTESIAN_POINT ( 'NONE',  ( 181.8774662184618194, 285.1120569720015965, 15.89814067624403116 ) ) ;
#55610 = B_SPLINE_CURVE_WITH_KNOTS ( 'NONE', 3,
 ( #29821, #61209, #13633, #59712, #75436, #91653, #30824, #91156, #90678, #67828, #15102, #98750, #60695, #29330, #22219, #13144 ),
 .UNSPECIFIED., .F., .F.,
 ( 4, 1, 2, 2, 2, 1, 2, 2, 4 ),
 ( 0.000000000000000000, 0.1249999999999974465, 0.1874999999999963918, 0.2499999999999953371, 0.4999999999999977796, 0.6249999999999976685, 0.6874999999999975575, 0.7499999999999975575, 1.000000000000000000 ),
 .UNSPECIFIED. ) ;
#55611 = CARTESIAN_POINT ( 'NONE',  ( 7.864685750751951865, 30.05722773587472929, -10.00000000000000000 ) ) ;
#55612 = ORIENTED_EDGE ( 'NONE', *, *, #91616, .F. ) ;
#55613 = CARTESIAN_POINT ( 'NONE',  ( 177.0706589053032474, 253.3103952305708617, -0.2596013527085206940 ) ) ;
#55615 = VERTEX_POINT ( 'NONE', #50206 ) ;
#55614 = VECTOR ( 'NONE', #71744, 1000.000000000000114 ) ;
#55616 = CARTESIAN_POINT ( 'NONE',  ( 72.40589440182066028, 71.76200285602328677, 5.709577571112511407 ) ) ;
#55617 = CARTESIAN_POINT ( 'NONE',  ( 42.72800263476181470, 202.1427522451419350, 10.00000000000009415 ) ) ;
#55618 = LINE ( 'NONE', #48549, #75745 ) ;
#55619 = ORIENTED_EDGE ( 'NONE', *, *, #91858, .T. ) ;
#55620 = CARTESIAN_POINT ( 'NONE',  ( 22.20737081713590655, 33.79752408145593279, -5.678558825948271327 ) ) ;
#55621 = CARTESIAN_POINT ( 'NONE',  ( 79.78566621355244592, 44.75865846334889397, 11.33384506647717416 ) ) ;
#55622 = CARTESIAN_POINT ( 'NONE',  ( 75.21677898156802655, 66.43306031420556224, -13.15226642884186070 ) ) ;
#55623 = LINE ( 'NONE', #86606, #39679 ) ;
#55624 = ORIENTED_EDGE ( 'NONE', *, *, #52802, .T. ) ;
#55625 = DIRECTION ( 'NONE',  ( -0.5840252505817139506, 0.000000000000000000, -0.8117354905897402606 ) ) ;
#55626 = CARTESIAN_POINT ( 'NONE',  ( 48.74043828842092552, 100.0309547576005258, -10.00000000000000000 ) ) ;
#55627 = ORIENTED_EDGE ( 'NONE', *, *, #77498, .F. ) ;
#55628 = CARTESIAN_POINT ( 'NONE',  ( 186.0541232522963639, 298.0217281582578721, 1.045760341051833908 ) ) ;
#55630 = CARTESIAN_POINT ( 'NONE',  ( 148.4042165687623083, 273.6033521758856750, -8.709765892313745539 ) ) ;
#55629 = CARTESIAN_POINT ( 'NONE',  ( 163.1340607412760448, 284.0498969924611856, -2.585094881414993218 ) ) ;
#55631 = CARTESIAN_POINT ( 'NONE',  ( 163.3020905273760093, 247.7994775548095845, -11.05431316445765155 ) ) ;
#55632 = CARTESIAN_POINT ( 'NONE',  ( 193.7118145980225279, 295.1282904202991517, 14.61271143546694162 ) ) ;
#55633 = CARTESIAN_POINT ( 'NONE',  ( 185.9342682518984020, 292.9530047715350634, -10.72693318328547818 ) ) ;
#55634 = CARTESIAN_POINT ( 'NONE',  ( 157.8820657059571033, 257.1872359237914338, -17.60412210594719440 ) ) ;
#55635 = CARTESIAN_POINT ( 'NONE',  ( 146.3987206697217403, 246.1423013555409796, -4.594050593750043987 ) ) ;
#55636 = DIRECTION ( 'NONE',  ( -0.8660254037844387076, -0.4999999999999998890, -0.000000000000000000 ) ) ;
#55637 = CARTESIAN_POINT ( 'NONE',  ( 173.8665542827094725, 250.6399523573830095, -0.9454928766311748722 ) ) ;
#55638 = VERTEX_POINT ( 'NONE', #68877 ) ;
#55639 = CARTESIAN_POINT ( 'NONE',  ( 151.3589047706063582, 268.4856820897672378, 14.56544807350869419 ) ) ;
#55640 = CARTESIAN_POINT ( 'NONE',  ( 78.10947740687990404, 61.47724562959768946, -16.15800848020992930 ) ) ;
#55641 = EDGE_LOOP ( 'NONE', ( #60595, #55737, #72910, #98297 ) ) ;
#55642 = CARTESIAN_POINT ( 'NONE',  ( 157.1606728774482065, 258.4367249549846974, -18.41782236529479633 ) ) ;
#55643 = ORIENTED_EDGE ( 'NONE', *, *, #57001, .T. ) ;
#55644 = VERTEX_POINT ( 'NONE', #7587 ) ;
#55645 = FACE_OUTER_BOUND ( 'NONE', #57537, .T. ) ;
#55646 = CARTESIAN_POINT ( 'NONE',  ( 153.0305350670531936, 277.3750776671890890, 8.290292975357761662 ) ) ;
#55647 = DIRECTION ( 'NONE',  ( 0.1473778574936323582, 0.9890802632347824863, 0.000000000000000000 ) ) ;
#55648 = FACE_OUTER_BOUND ( 'NONE', #60963, .T. ) ;
#55649 = EDGE_CURVE ( 'NONE', #45951, #86106, #18959, .T. ) ;
#55650 = DIRECTION ( 'NONE',  ( -0.8660254037844387076, -0.4999999999999998890, -0.000000000000000000 ) ) ;
#55651 = CARTESIAN_POINT ( 'NONE',  ( 73.24602992621615272, 225.3464784336661353, 1.353441290958777327E-15 ) ) ;
#55652 = VERTEX_POINT ( 'NONE', #93222 ) ;
#55653 = EDGE_CURVE ( 'NONE', #46249, #79661, #3361, .T. ) ;
#55654 = VERTEX_POINT ( 'NONE', #53675 ) ;
#55656 = EDGE_CURVE ( 'NONE', #40825, #14428, #46573, .T. ) ;
#55655 = CARTESIAN_POINT ( 'NONE',  ( 208.3764315856425640, 269.7284287242038658, -1.833640725398759441 ) ) ;
#55657 = ORIENTED_EDGE ( 'NONE', *, *, #30852, .F. ) ;
#55658 = EDGE_CURVE ( 'NONE', #79781, #98426, #83640, .T. ) ;
#55659 = CARTESIAN_POINT ( 'NONE',  ( 28.71959338928917305, 24.78052372038641593, -10.00000000000000355 ) ) ;
#55660 = CARTESIAN_POINT ( 'NONE',  ( 164.0466959984708808, 284.5713585264927588, 0.5044889840302336781 ) ) ;
#55661 = CARTESIAN_POINT ( 'NONE',  ( -15.31269525828471068, 104.2312461070085021, 36.50000000000000000 ) ) ;
#55662 = CARTESIAN_POINT ( 'NONE',  ( 88.27143343078938642, 44.36575123808635368, 4.213746458969101383 ) ) ;
#55663 = ORIENTED_EDGE ( 'NONE', *, *, #8783, .T. ) ;
#55664 = CARTESIAN_POINT ( 'NONE',  ( 85.82643298209987393, 43.85229891390187618, -5.345846949436618090 ) ) ;
#55665 = LINE ( 'NONE', #63289, #6072 ) ;
#55666 = CARTESIAN_POINT ( 'NONE',  ( 206.6912923161529818, 272.6471755567893638, -9.325620632947922317 ) ) ;
#55667 = CARTESIAN_POINT ( 'NONE',  ( -71.07364842061382149, 47.42355933771584375, -10.00000000000000000 ) ) ;
#55668 = CARTESIAN_POINT ( 'NONE',  ( 175.1469972352321633, 284.3759121112690309, 13.98116163681930146 ) ) ;
#55669 = CARTESIAN_POINT ( 'NONE',  ( 72.58249898592296745, 70.72798385450705894, 7.152797386299237559 ) ) ;
#55670 = CARTESIAN_POINT ( 'NONE',  ( 93.96857342517719758, 10.00000000000001243, 0.000000000000000000 ) ) ;
#55671 = VERTEX_POINT ( 'NONE', #68387 ) ;
#55672 = FACE_OUTER_BOUND ( 'NONE', #89373, .T. ) ;
#55673 = CARTESIAN_POINT ( 'NONE',  ( 200.8432122835317841, 282.7763473000181307, 17.15137370990203891 ) ) ;
#55674 = CARTESIAN_POINT ( 'NONE',  ( 86.31701533123542447, 45.73308513344992576, 8.415584269618911151 ) ) ;
#55675 = CARTESIAN_POINT ( 'NONE',  ( 184.8630750434761296, 264.0504083588372168, -12.11215620985133512 ) ) ;
#55676 = CARTESIAN_POINT ( 'NONE',  ( 83.55704177478077099, 51.98730140788478593, 15.00998877770038042 ) ) ;
#55677 = CARTESIAN_POINT ( 'NONE',  ( 203.9648368022151601, 269.0477214045654364, 5.644613064108824574 ) ) ;
#55678 = FACE_BOUND ( 'NONE', #22670, .T. ) ;
#55679 = ORIENTED_EDGE ( 'NONE', *, *, #55946, .F. ) ;
#55680 = VECTOR ( 'NONE', #19565, 1000.000000000000341 ) ;
#55681 = CARTESIAN_POINT ( 'NONE',  ( 72.91325260937172459, 64.33234797326966259, -13.52415029394816770 ) ) ;
#55683 = CARTESIAN_POINT ( 'NONE',  ( 73.80042137613033049, 55.16559329544060120, 16.59890288620815824 ) ) ;
#55682 = CARTESIAN_POINT ( 'NONE',  ( 180.5897091146829609, 267.0577128828192031, -14.91057311322558476 ) ) ;
#55684 = CARTESIAN_POINT ( 'NONE',  ( 175.9417783262450712, 285.5840353934577251, -13.36389416340276171 ) ) ;
#55685 = CARTESIAN_POINT ( 'NONE',  ( 26.33642183074453058, 30.90829794293881960, 10.00000000000000355 ) ) ;
#55686 = CARTESIAN_POINT ( 'NONE',  ( 180.4105609632205756, 272.9652835783806495, 17.11323411940207606 ) ) ;
#55687 = CARTESIAN_POINT ( 'NONE',  ( 181.7815785431583038, 276.1505370498239813, -17.81783396216490445 ) ) ;
#55688 = CARTESIAN_POINT ( 'NONE',  ( 191.6505299071077104, 262.2872231605458069, 2.938842163976925104 ) ) ;
#55689 = CARTESIAN_POINT ( 'NONE',  ( 188.5010067632256607, 276.1349817662086252, -17.56847558694355982 ) ) ;
#55690 = CARTESIAN_POINT ( 'NONE',  ( -3.586574591843265658, 177.9244531367911577, -4.594050593750046652 ) ) ;
#55691 = LINE ( 'NONE', #72950, #37131 ) ;
#55692 = ORIENTED_EDGE ( 'NONE', *, *, #36398, .F. ) ;
#55693 = CARTESIAN_POINT ( 'NONE',  ( 175.3514250190609687, 255.5038543308169494, 8.239661746456338420 ) ) ;
#55694 = CARTESIAN_POINT ( 'NONE',  ( 85.72375369157853697, 153.9044130683316212, 0.000000000000000000 ) ) ;
#55695 = CARTESIAN_POINT ( 'NONE',  ( 82.07978327023018039, 41.81623142779876900, 5.466382998867931775 ) ) ;
#55696 = CARTESIAN_POINT ( 'NONE',  ( 22.06942799527072907, 192.7369531367911293, -4.594050593750048428 ) ) ;
#55697 = EDGE_CURVE ( 'NONE', #61969, #58437, #6001, .T. ) ;
#55698 = CARTESIAN_POINT ( 'NONE',  ( 71.12873073640183463, 200.3262482093457777, 3.021315404115420679E-15 ) ) ;
#55699 = CARTESIAN_POINT ( 'NONE',  ( 37.92328063009087202, 22.86426979415092475, -3.090169943749474069 ) ) ;
#55700 = CARTESIAN_POINT ( 'NONE',  ( 178.4923177964227250, 291.6910058127210164, 5.905753715927121839 ) ) ;
#55701 = CARTESIAN_POINT ( 'NONE',  ( 147.2784190576484491, 275.5532906641692534, 0.2793038414862047958 ) ) ;
#55702 = PLANE ( 'NONE',  #10451 ) ;
#55703 = CARTESIAN_POINT ( 'NONE',  ( 187.6909010698966540, 296.4604880036308714, -7.720386555275442042 ) ) ;
#55704 = CARTESIAN_POINT ( 'NONE',  ( 83.44503355366286712, 51.91352208420826031, 15.00625484349790106 ) ) ;
#55705 = CARTESIAN_POINT ( 'NONE',  ( 193.0502745353014689, 295.6857625178031412, -12.56346185710428998 ) ) ;
#55706 = CARTESIAN_POINT ( 'NONE',  ( 61.50992858288472576, 212.9865022471903444, -10.00000000000009415 ) ) ;
#55707 = CARTESIAN_POINT ( 'NONE',  ( 69.94880244668077296, 66.76424936624940187, -10.23932032170969997 ) ) ;
#55708 = CARTESIAN_POINT ( 'NONE',  ( 185.6631735345632706, 277.8091931743529699, -17.25901495274653286 ) ) ;
#55709 = CARTESIAN_POINT ( 'NONE',  ( 203.6925490392534925, 269.5270927311577793, 7.084861529579629114 ) ) ;
#55710 = CARTESIAN_POINT ( 'NONE',  ( 42.15091268916992817, 185.9548013555409796, -4.594050593750042211 ) ) ;
#55711 = CARTESIAN_POINT ( 'NONE',  ( 197.8977219949227049, 287.8780861330898801, 17.48564646125164046 ) ) ;
#55712 = EDGE_CURVE ( 'NONE', #16775, #76974, #84147, .T. ) ;
#55713 = CARTESIAN_POINT ( 'NONE',  ( 73.27344031762343946, 203.1115022471901739, -5.000000000000041744 ) ) ;
#55714 = B_SPLINE_CURVE_WITH_KNOTS ( 'NONE', 3,
 ( #56310, #100071, #48740, #52951, #37736, #6850, #84887, #62526, #69643, #30658, #10234, #14936, #91488, #22051, #87306, #53924, #15427, #84390, #60535, #99566, #46847, #46325, #743, #17839, #83901, #45345, #30149, #79672, #15944, #41103, #77250 ),
 .UNSPECIFIED., .F., .F.,
 ( 4, 3, 3, 3, 3, 3, 3, 3, 3, 3, 4 ),
 ( 0.000000000000000000, 0.1333490885032278528, 0.3007194338854267679, 0.4699862290245069296, 0.5844252810809245080, 0.6686540514502667953, 0.7354980260655522573, 0.8028463152565803451, 0.8633854507757331431, 0.9437142632667367970, 1.000000000000000000 ),
 .UNSPECIFIED. ) ;
#55715 = LINE ( 'NONE', #61335, #44945 ) ;
#55716 = DIRECTION ( 'NONE',  ( 0.1237105541964823863, -0.9923183454821336014, 0.000000000000000000 ) ) ;
#55717 = ORIENTED_EDGE ( 'NONE', *, *, #89156, .F. ) ;
#55718 = DIRECTION ( 'NONE',  ( 0.5895128895116616974, 0.8077589696806909414, 0.000000000000000000 ) ) ;
#55719 = CARTESIAN_POINT ( 'NONE',  ( 168.1103729947156751, 282.0138679452536508, -10.93130146384492996 ) ) ;
#55720 = CARTESIAN_POINT ( 'NONE',  ( 49.17298586869600996, 105.8308522718264584, 10.00000000000000000 ) ) ;
#55721 = CARTESIAN_POINT ( 'NONE',  ( 160.8398227522241370, 262.6459064758317936, 17.80292298429472098 ) ) ;
#55722 = CARTESIAN_POINT ( 'NONE',  ( 21.45803809350889679, 35.49540643055188127, 3.479690158560446702E-15 ) ) ;
#55723 = CARTESIAN_POINT ( 'NONE',  ( 163.4004183463084416, 247.6291687766210146, 10.19167732382099345 ) ) ;
#55724 = CARTESIAN_POINT ( 'NONE',  ( 196.9431415128477170, 289.5314680279574304, -16.61413060656005669 ) ) ;
#55725 = CARTESIAN_POINT ( 'NONE',  ( 187.6748237365926286, 269.2623419302518073, -14.09746843418098905 ) ) ;
#55726 = ORIENTED_EDGE ( 'NONE', *, *, #38803, .T. ) ;
#55727 = CARTESIAN_POINT ( 'NONE',  ( 4.137530017820133743, 25.49540643055185285, 3.479690158560446702E-15 ) ) ;
#55728 = CARTESIAN_POINT ( 'NONE',  ( 189.2844570553383790, 299.8432624979336651, 4.996325856711115954 ) ) ;
#55729 = CARTESIAN_POINT ( 'NONE',  ( 77.85254210321063795, 58.20651666130322610, -16.18224212962651265 ) ) ;
#55730 = CARTESIAN_POINT ( 'NONE',  ( 71.49023828022640714, 72.34911387847559183, -1.236132173619994168 ) ) ;
#55731 = EDGE_LOOP ( 'NONE', ( #35822, #86858, #26394, #79732 ) ) ;
#55732 = CARTESIAN_POINT ( 'NONE',  ( 32.47331203838563596, 45.95596728736418868, 10.00000000000000000 ) ) ;
#55733 = DIRECTION ( 'NONE',  ( 1.000000000000000000, 0.000000000000000000, 0.000000000000000000 ) ) ;
#55734 = DIRECTION ( 'NONE',  ( -0.8660254037844379305, -0.5000000000000014433, -0.000000000000000000 ) ) ;
#55735 = CARTESIAN_POINT ( 'NONE',  ( 177.7080561073729257, 256.3275381662501786, -7.267023968690817348 ) ) ;
#55736 = CARTESIAN_POINT ( 'NONE',  ( 190.0550686570564949, 301.4619601804237732, 4.203010638620038542 ) ) ;
#55737 = ORIENTED_EDGE ( 'NONE', *, *, #62855, .T. ) ;
#55738 = ORIENTED_EDGE ( 'NONE', *, *, #68616, .T. ) ;
#55740 = FILL_AREA_STYLE ('',( #94313 ) ) ;
#55739 = CARTESIAN_POINT ( 'NONE',  ( 189.2635003502843745, 273.9792018228808956, -15.65845025130167478 ) ) ;
#55741 = ORIENTED_EDGE ( 'NONE', *, *, #34705, .F. ) ;
#55742 = CARTESIAN_POINT ( 'NONE',  ( 34.78335331324970525, 43.58029201028044497, 1.583844403245397769 ) ) ;
#55743 = CARTESIAN_POINT ( 'NONE',  ( 187.9019955452718023, 260.0457317612239194, -6.306085470763082235 ) ) ;
#55744 = CARTESIAN_POINT ( 'NONE',  ( 72.71379711463576712, 57.17174861646414996, -15.88508012487434939 ) ) ;
#55745 = CARTESIAN_POINT ( 'NONE',  ( 77.33081447068806824, 63.24619402228064047, 15.57729104808880294 ) ) ;
#55746 = CARTESIAN_POINT ( 'NONE',  ( 204.6475128369918082, 276.1871054541632020, -13.72068618491070779 ) ) ;
#55748 = CARTESIAN_POINT ( 'NONE',  ( 106.9945647975297760, 223.3923013555410080, 4.594050593750050204 ) ) ;
#55747 = VECTOR ( 'NONE', #85766, 1000.000000000000000 ) ;
#55749 = CARTESIAN_POINT ( 'NONE',  ( 148.9831146496684084, 272.6006712873522133, -12.63706091291043343 ) ) ;
#55750 = CARTESIAN_POINT ( 'NONE',  ( 180.6772252457255377, 287.0457239474706057, -13.49698767722689752 ) ) ;
#55751 = EDGE_LOOP ( 'NONE', ( #49317, #53667, #35966, #13921, #67730, #58546, #19045, #29380, #2365, #88406, #86728, #25060, #79986, #12938, #66234, #32638, #69560, #91218, #38464, #68709 ) ) ;
#55752 = CARTESIAN_POINT ( 'NONE',  ( 164.3890147726454813, 245.9168695380243435, -6.010262808998044548 ) ) ;
#55753 = EDGE_LOOP ( 'NONE', ( #41482, #6947, #77304, #89832 ) ) ;
#55754 = CARTESIAN_POINT ( 'NONE',  ( 30.72569264534336142, 26.24335787977765122, -9.188101187500008038 ) ) ;
#55755 = ADVANCED_FACE ( 'NONE', ( #30391 ), #60272, .T. ) ;
#55756 = CARTESIAN_POINT ( 'NONE',  ( 157.1649673255039943, 259.2653790051248279, 17.12562605537966220 ) ) ;
#55757 = CARTESIAN_POINT ( 'NONE',  ( 78.39811245026406539, 48.00393270933970058, -14.01973118892057357 ) ) ;
#55758 = CARTESIAN_POINT ( 'NONE',  ( 56.16917826928300883, 212.4244531367911577, -4.594050593750046652 ) ) ;
#55759 = CARTESIAN_POINT ( 'NONE',  ( 74.41008358870023187, 68.25813196090381041, 11.42500230979621634 ) ) ;
#55760 = FACE_OUTER_BOUND ( 'NONE', #78470, .T. ) ;
#55761 = DIRECTION ( 'NONE',  ( 1.000000000000000000, 0.000000000000000000, -0.000000000000000000 ) ) ;
#55762 = DIRECTION ( 'NONE',  ( -0.8660254037844387076, -0.4999999999999998890, -0.000000000000000000 ) ) ;
#55763 = ORIENTED_EDGE ( 'NONE', *, *, #16681, .F. ) ;
#55764 =( BOUNDED_CURVE ( )  B_SPLINE_CURVE ( 2, ( #65672, #4896, #51474, #74806, #50472, #81425, #72818, #4379, #35279 ),
 .UNSPECIFIED., .F., .T. ) 
 B_SPLINE_CURVE_WITH_KNOTS ( ( 3, 2, 2, 2, 3 ),
 ( 0.3750000000000000000, 0.3763440860215053752, 0.3790322580645161255, 0.3817204301075268758, 0.3830645161290322509 ),
 .UNSPECIFIED. ) 
 CURVE ( )  GEOMETRIC_REPRESENTATION_ITEM ( )  RATIONAL_B_SPLINE_CURVE ( ( 0.9330127018922194093, 0.9330127018922194093, 1.000000000000000000, 0.8660254037844387076, 1.000000000000000000, 0.8660254037844387076, 1.000000000000000000, 0.9330127018922194093, 0.9330127018922194093 ) ) 
 REPRESENTATION_ITEM ( '' )  );
#55765 = CARTESIAN_POINT ( 'NONE',  ( 72.02976470237955198, 59.30830629416842470, -15.33705471575644808 ) ) ;
#55766 = LINE ( 'NONE', #64400, #37966 ) ;
#55767 = CARTESIAN_POINT ( 'NONE',  ( 78.86219776201926379, 59.55369065033505649, 16.50996775951927020 ) ) ;
#55768 = ORIENTED_EDGE ( 'NONE', *, *, #17831, .F. ) ;
#55769 = CARTESIAN_POINT ( 'NONE',  ( 171.7744858013287228, 259.2587365160856621, -13.76106460065646253 ) ) ;
#55770 = CARTESIAN_POINT ( 'NONE',  ( 69.94473186773970497, 69.73739167999330846, -5.878840642600716038 ) ) ;
#55771 = CARTESIAN_POINT ( 'NONE',  ( 207.8575108622103755, 270.6272257822888037, -6.381720258959569847 ) ) ;
#55772 = ADVANCED_FACE ( 'NONE', ( #8102 ), #30891, .F. ) ;
#55773 = CARTESIAN_POINT ( 'NONE',  ( 192.6679047218190135, 296.9363953644068488, -13.34486378385621386 ) ) ;
#55774 = CARTESIAN_POINT ( 'NONE',  ( 190.8072577185990610, 300.1591305089344814, 3.698484652594827171 ) ) ;
#55775 = LINE ( 'NONE', #17821, #85058 ) ;
#55776 = CIRCLE ( 'NONE', #81738, 0.1418229129681591871 ) ;
#55777 = CARTESIAN_POINT ( 'NONE',  ( 86.87502629904909668, 43.20941739936903758, -2.818466721968422739 ) ) ;
#55778 = LINE ( 'NONE', #86769, #44401 ) ;
#55779 = CARTESIAN_POINT ( 'NONE',  ( 154.3285155289529769, 264.0917920393945337, -16.81000869023829125 ) ) ;
#55780 = CARTESIAN_POINT ( 'NONE',  ( 75.48012123268173923, 53.33211347945791658, 16.49774674168797972 ) ) ;
#55781 = CARTESIAN_POINT ( 'NONE',  ( 105.5326262849960131, 240.9244531367911293, -4.594050593750046652 ) ) ;
#55782 = ORIENTED_EDGE ( 'NONE', *, *, #33686, .F. ) ;
#55783 = CARTESIAN_POINT ( 'NONE',  ( 191.8232488616404225, 298.3993822291468518, -9.342381338555176384 ) ) ;
#55784 = CARTESIAN_POINT ( 'NONE',  ( 83.32494336655207690, 41.48408949819171454, -1.461985904981788487 ) ) ;
#55785 = CARTESIAN_POINT ( 'NONE',  ( 203.3205561747472814, 278.4854618126124706, -15.14439614831292147 ) ) ;
#55786 = CARTESIAN_POINT ( 'NONE',  ( 163.8147431267737204, 246.9115372060205118, 7.125417796469586840 ) ) ;
#55787 = CARTESIAN_POINT ( 'NONE',  ( 83.90615881913062424, 51.69600214455904563, -14.41633884075334393 ) ) ;
#55788 = CARTESIAN_POINT ( 'NONE',  ( 178.1484433634098536, 255.2371399336910827, 4.532319796120597211 ) ) ;
#55789 = ORIENTED_EDGE ( 'NONE', *, *, #4440, .T. ) ;
#55790 = CARTESIAN_POINT ( 'NONE',  ( 80.64870151538644905, 57.33808369813028349, -16.23392458231729307 ) ) ;
#55791 = CARTESIAN_POINT ( 'NONE',  ( 154.6130741698598854, 273.3603101155351851, -13.17814745200596427 ) ) ;
#55792 = CARTESIAN_POINT ( 'NONE',  ( 182.0067218172421235, 260.4949756789683306, 9.583730042554169160 ) ) ;
#55793 = CARTESIAN_POINT ( 'NONE',  ( 206.1569797555946195, 273.5726320587986038, -9.753408447412784454 ) ) ;
#55794 = CARTESIAN_POINT ( 'NONE',  ( 133.1643360984345463, 253.8149278399160949, 9.188101187500093303 ) ) ;
#55795 = B_SPLINE_CURVE_WITH_KNOTS ( 'NONE', 3,
 ( #67542, #21452, #13849, #94379 ),
 .UNSPECIFIED., .F., .F.,
 ( 4, 4 ),
 ( 0.04033338801658184480, 0.04875068421467537716 ),
 .UNSPECIFIED. ) ;
#55796 = CARTESIAN_POINT ( 'NONE',  ( 198.4427928769277969, 286.9339956717308837, -17.97122743692687763 ) ) ;
#55797 = DIRECTION ( 'NONE',  ( -0.5000000000000002220, 0.8660254037844384856, 0.000000000000000000 ) ) ;
#55798 = CARTESIAN_POINT ( 'NONE',  ( 189.6721586819687957, 282.5493231147508482, -16.58139960728656703 ) ) ;
#55799 = DIRECTION ( 'NONE',  ( 0.4755282581475757664, -0.8236391035463335175, -0.3090169943749448977 ) ) ;
#55800 = CARTESIAN_POINT ( 'NONE',  ( 48.48320281069610616, 207.9869531367911009, 4.594050593750046652 ) ) ;
#55801 = CARTESIAN_POINT ( 'NONE',  ( 78.92023586790456591, 59.45316570216661489, -16.52216786098995982 ) ) ;
#55802 = LINE ( 'NONE', #23926, #35065 ) ;
#55803 = CARTESIAN_POINT ( 'NONE',  ( 70.93180422968134735, 70.94319162518513622, -4.401341846138759450 ) ) ;
#55804 = CARTESIAN_POINT ( 'NONE',  ( 174.4129540281212201, 262.1633850759363895, 14.35098408255141322 ) ) ;
#55805 = CARTESIAN_POINT ( 'NONE',  ( 82.30224259366366368, 41.51585266683629527, -5.837696018721792335 ) ) ;
#55806 = CARTESIAN_POINT ( 'NONE',  ( 178.8786119934938483, 291.7246583498065320, -6.365583027218077561 ) ) ;
#55807 = VECTOR ( 'NONE', #49805, 1000.000000000000000 ) ;
#55808 = CARTESIAN_POINT ( 'NONE',  ( 203.3684377202211522, 278.4025285431072803, -16.56116267537666076 ) ) ;
#55809 = CARTESIAN_POINT ( 'NONE',  ( 153.6066505450084492, 269.2403879892464715, -15.56648601798310239 ) ) ;
#55810 = CARTESIAN_POINT ( 'NONE',  ( 121.1754704609022468, 240.7677522451418497, 10.00000000000009592 ) ) ;
#55811 = B_SPLINE_SURFACE_WITH_KNOTS ( 'NONE', 3, 1, ( 
 ( #13383, #66571 ),
 ( #68059, #89909 ),
 ( #91396, #97983 ),
 ( #81814, #51877 ),
 ( #29083, #27593 ),
 ( #83805, #51360 ),
 ( #44253, #58938 ),
 ( #13865, #12390 ),
 ( #28561, #28065 ),
 ( #14369, #29566 ),
 ( #59441, #68554 ),
 ( #82815, #97497 ),
 ( #45255, #19984 ),
 ( #21961, #60440 ),
 ( #52854, #20996 ),
 ( #44745, #75188 ),
 ( #43753, #50864 ),
 ( #74698, #58457 ),
 ( #5763, #5277 ),
 ( #36652, #67559 ),
 ( #43255, #98491 ),
 ( #59948, #90919 ),
 ( #75678, #21468 ),
 ( #52356, #37160 ),
 ( #76190, #6765 ),
 ( #89431, #74200 ),
 ( #4789, #79577 ),
 ( #54846, #7758 ),
 ( #69556, #33432 ),
 ( #22461, #85827 ),
 ( #22947, #92400 ),
 ( #39131, #53355 ),
 ( #92888, #657 ),
 ( #60947, #56725 ) ),
 .UNSPECIFIED., .T., .F., .F.,
 ( 4, 2, 2, 2, 2, 2, 2, 2, 2, 2, 2, 2, 2, 2, 2, 2, 4 ),
 ( 2, 2 ),
 ( 0.000000000000000000, 0.06250000000000000000, 0.1250000000000000000, 0.1875000000000000000, 0.2500000000000000000, 0.3125000000000000000, 0.3750000000000000000, 0.4375000000000000000, 0.5000000000000000000, 0.5625000000000000000, 0.6250000000000000000, 0.6875000000000000000, 0.7500000000000000000, 0.8125000000000000000, 0.8750000000000000000, 0.9375000000000000000, 1.000000000000000000 ),
 ( 0.000000000000000000, 1.000000000000000000 ),
 .UNSPECIFIED. ) ;
#55812 = CARTESIAN_POINT ( 'NONE',  ( 76.26004098100119677, 53.26552314622699669, -15.96572022850413219 ) ) ;
#55813 = VERTEX_POINT ( 'NONE', #91228 ) ;
#55814 = AXIS2_PLACEMENT_3D ( 'NONE', #44389, #4926, #35805 ) ;
#55815 = CARTESIAN_POINT ( 'NONE',  ( 163.3543347837650686, 247.7089878483399730, 10.92686688779373405 ) ) ;
#55816 = CARTESIAN_POINT ( 'NONE',  ( 87.92709505194216035, 44.79768224621495420, 4.873456775040940769 ) ) ;
#55817 = EDGE_CURVE ( 'NONE', #78871, #20189, #47989, .T. ) ;
#55818 = CARTESIAN_POINT ( 'NONE',  ( 23.50386934422995822, 190.5024278399160949, -9.188101187500093303 ) ) ;
#55819 = CARTESIAN_POINT ( 'NONE',  ( 10.22618198766610575, 28.83705186507752671, 3.090169943749475401 ) ) ;
#55820 = CARTESIAN_POINT ( 'NONE',  ( 192.3060925962972476, 271.9899639347428888, 15.52435667988647516 ) ) ;
#55821 = CARTESIAN_POINT ( 'NONE',  ( 149.2678550509543811, 265.6471520882315076, -1.519623991172852856E-15 ) ) ;
#55822 = CARTESIAN_POINT ( 'NONE',  ( 74.08065690531799419, 54.82731643721707826, -16.13522336645903721 ) ) ;
#55824 = CARTESIAN_POINT ( 'NONE',  ( 65.24466313315730304, 195.1427522451417644, 1.119607411625061291E-15 ) ) ;
#55823 = CARTESIAN_POINT ( 'NONE',  ( 192.7686961758011250, 263.9209412561240811, -8.347089341778378468 ) ) ;
#55825 = CARTESIAN_POINT ( 'NONE',  ( 171.7216141583608930, 286.8318612379766819, 7.460387380223108877 ) ) ;
#55826 = CARTESIAN_POINT ( 'NONE',  ( 183.8250474427275094, 257.7038322492317093, 1.335502332953788729 ) ) ;
#55827 = CARTESIAN_POINT ( 'NONE',  ( -2.524136441754524451, 180.8967562850347406, 2.649461200531984646E-14 ) ) ;
#55828 = CARTESIAN_POINT ( 'NONE',  ( 66.36217872752992264, 68.78091108627523909, -4.321716179073264996 ) ) ;
#55829 = ORIENTED_EDGE ( 'NONE', *, *, #95552, .T. ) ;
#55830 = CARTESIAN_POINT ( 'NONE',  ( 26.50806851326365532, 196.1115022471903160, -5.000000000000047962 ) ) ;
#55831 = CARTESIAN_POINT ( 'NONE',  ( -19.59030177132946449, 93.19218903752455674, 59.99999999999999289 ) ) ;
#55832 = LINE ( 'NONE', #9788, #7767 ) ;
#55833 = CARTESIAN_POINT ( 'NONE',  ( 145.4512450625087467, 254.7833772461660544, -9.188101187500095079 ) ) ;
#55834 = CARTESIAN_POINT ( 'NONE',  ( 39.23796756512304995, 23.44966523072497822, -2.296566073217252530E-15 ) ) ;
#55837 = EDGE_CURVE ( 'NONE', #42053, #46017, #72650, .T. ) ;
#55836 = CARTESIAN_POINT ( 'NONE',  ( 200.4194242942598407, 282.7622742240619687, 16.88461573361379564 ) ) ;
#55835 = CARTESIAN_POINT ( 'NONE',  ( 163.9100659486979907, 252.4955106033718835, 13.24059601348467297 ) ) ;
#55838 = CARTESIAN_POINT ( 'NONE',  ( 185.4274225405056882, 260.0935088849925592, 7.264075338455358910 ) ) ;
#55839 = CARTESIAN_POINT ( 'NONE',  ( 25.38519627463738715, 32.84336893147757053, -7.433330006724137462 ) ) ;
#55840 = CARTESIAN_POINT ( 'NONE',  ( 205.8030308266901898, 274.1856895869457844, 10.55961490432110317 ) ) ;
#55841 = CARTESIAN_POINT ( 'NONE',  ( 186.8289980366191685, 258.5750005707243417, -2.467696023248564074 ) ) ;
#55842 = CARTESIAN_POINT ( 'NONE',  ( 66.25952267273640928, 69.15726288014950285, 2.537017490915350670 ) ) ;
#55843 = ORIENTED_EDGE ( 'NONE', *, *, #83815, .F. ) ;
#55844 = CARTESIAN_POINT ( 'NONE',  ( 55.65417314315315878, 214.4860189848785694, -2.679491924311252493 ) ) ;
#55845 = CARTESIAN_POINT ( 'NONE',  ( 180.5920144538960699, 286.8105750589551235, 13.18251988290063004 ) ) ;
#55846 = CARTESIAN_POINT ( 'NONE',  ( 168.7075216304318417, 287.6756853637114659, 0.5128971772568799992 ) ) ;
#55847 = CARTESIAN_POINT ( 'NONE',  ( 8.859747497914600700, 17.06628583063839599, -9.188101187500006262 ) ) ;
#55848 = CARTESIAN_POINT ( 'NONE',  ( 207.1531864936216607, 271.8471513736934071, 8.161497146364244060 ) ) ;
#55849 = VECTOR ( 'NONE', #44075, 1000.000000000000114 ) ;
#55850 = CARTESIAN_POINT ( 'NONE',  ( 84.81351086726648703, 50.35522970061591508, -13.86072692636569670 ) ) ;
#55851 = CARTESIAN_POINT ( 'NONE',  ( 206.1408608592916494, 273.6005508061571732, -10.42739367433323494 ) ) ;
#55852 = ADVANCED_FACE ( 'NONE', ( #4208 ), #56411, .T. ) ;
#55853 = CARTESIAN_POINT ( 'NONE',  ( 192.3606619183491091, 297.4685555102766443, 10.99569063633359889 ) ) ;
#55854 = CARTESIAN_POINT ( 'NONE',  ( 164.8251969117060298, 245.1613799118173063, -1.508678420156898348 ) ) ;
#55855 = AXIS2_PLACEMENT_3D ( 'NONE', #18083, #17060, #87550 ) ;
#55856 = CARTESIAN_POINT ( 'NONE',  ( 191.3843761966370209, 282.8631020262318430, -17.76976768207862278 ) ) ;
#55857 = CARTESIAN_POINT ( 'NONE',  ( 87.88245627177123254, 44.92329797532170943, 6.249457923817309357 ) ) ;
#55858 = CARTESIAN_POINT ( 'NONE',  ( 154.9344967692067598, 262.2925750810547356, 17.30210568643136781 ) ) ;
#55859 = ORIENTED_EDGE ( 'NONE', *, *, #27783, .T. ) ;
#55860 = ORIENTED_EDGE ( 'NONE', *, *, #41272, .F. ) ;
#55861 = CARTESIAN_POINT ( 'NONE',  ( 155.9060408714371988, 277.3267832574535419, -10.46950353421899038 ) ) ;
#55862 = CARTESIAN_POINT ( 'NONE',  ( 86.72740319991413571, 46.97082492543196963, 10.28929863393111610 ) ) ;
#55863 = EDGE_LOOP ( 'NONE', ( #61841, #82956, #87509, #27354 ) ) ;
#55864 = LINE ( 'NONE', #31578, #75871 ) ;
#55865 = ORIENTED_EDGE ( 'NONE', *, *, #71380, .F. ) ;
#55866 = CARTESIAN_POINT ( 'NONE',  ( -44.74834796241764678, 29.05375577536863929, -10.00000000000000000 ) ) ;
#55867 = CARTESIAN_POINT ( 'NONE',  ( 84.55218960391981398, 48.55517814912271746, -12.33429493815133782 ) ) ;
#55868 = CARTESIAN_POINT ( 'NONE',  ( 20.78273902371470072, 14.12755873383625804, -6.180339887498949025 ) ) ;
#55869 = VERTEX_POINT ( 'NONE', #35104 ) ;
#55870 = CARTESIAN_POINT ( 'NONE',  ( 173.9119411810186193, 267.2826965128863890, 17.13893503472135649 ) ) ;
#55871 = PLANE ( 'NONE',  #91876 ) ;
#55872 = CARTESIAN_POINT ( 'NONE',  ( 175.0125019719911847, 292.0719086349095051, 3.303583340955516423 ) ) ;
#55873 = VECTOR ( 'NONE', #81596, 1000.000000000000000 ) ;
#55874 = CARTESIAN_POINT ( 'NONE',  ( 190.8264243556038195, 300.1259329198319961, 8.466983560044813117 ) ) ;
#55875 = CARTESIAN_POINT ( 'NONE',  ( 151.3777100552970580, 274.9574019808734420, -8.625823521072360833 ) ) ;
#55876 = VERTEX_POINT ( 'NONE', #87889 ) ;
#55877 = EDGE_CURVE ( 'NONE', #57299, #83821, #66015, .T. ) ;
#55878 = EDGE_CURVE ( 'NONE', #24506, #3124, #89374, .T. ) ;
#55879 = CARTESIAN_POINT ( 'NONE',  ( -19.65312891409030271, 93.06504152958497400, 10.00000000000000888 ) ) ;
#55880 = ORIENTED_EDGE ( 'NONE', *, *, #72773, .F. ) ;
#55881 = VERTEX_POINT ( 'NONE', #81751 ) ;
#55882 = CARTESIAN_POINT ( 'NONE',  ( 73.73726724665601751, 62.90511275149663106, 14.47564044095566160 ) ) ;
#55883 = VECTOR ( 'NONE', #27750, 1000.000000000000227 ) ;
#55884 = ORIENTED_EDGE ( 'NONE', *, *, #43187, .F. ) ;
#55885 = CARTESIAN_POINT ( 'NONE',  ( 160.7087992090237663, 271.0393196853082145, 16.56332265730499387 ) ) ;
#55886 = ORIENTED_EDGE ( 'NONE', *, *, #3580, .T. ) ;
#55887 = EDGE_CURVE ( 'NONE', #14510, #57901, #12326, .T. ) ;
#55888 = CARTESIAN_POINT ( 'NONE',  ( 197.2484515917759609, 283.9560669716739199, 17.81188092217798769 ) ) ;
#55889 = CARTESIAN_POINT ( 'NONE',  ( 71.26320768968655273, 69.07654504452045785, 8.407160263220744056 ) ) ;
#55890 = CARTESIAN_POINT ( 'NONE',  ( 147.6884207308302450, 274.8431469350302336, -8.096293592099874203 ) ) ;
#55891 = CARTESIAN_POINT ( 'NONE',  ( 82.51639823017981712, 53.47659673923356394, -15.74004163755323482 ) ) ;
#55892 = EDGE_CURVE ( 'NONE', #40803, #54888, #85357, .T. ) ;
#55893 = DIRECTION ( 'NONE',  ( -1.850371707708595795E-16, -7.401486830834383181E-16, 1.000000000000000000 ) ) ;
#55894 = ORIENTED_EDGE ( 'NONE', *, *, #99337, .F. ) ;
#55895 = CARTESIAN_POINT ( 'NONE',  ( 96.49374645304573050, 226.5177522451418781, -10.00000000000009592 ) ) ;
#55896 = CARTESIAN_POINT ( 'NONE',  ( 20.38389956778225809, 29.95586893147755703, 7.433330006724141015 ) ) ;
#55897 = CARTESIAN_POINT ( 'NONE',  ( 164.4494343874829099, 245.8122196953522121, 2.922779519406129456 ) ) ;
#55898 = CARTESIAN_POINT ( 'NONE',  ( 191.5513189742059978, 298.4536868043492746, -8.478051802322086772 ) ) ;
#55900 = ORIENTED_EDGE ( 'NONE', *, *, #91995, .T. ) ;
#55899 = CARTESIAN_POINT ( 'NONE',  ( 159.4285914931787431, 254.5085746851079023, 15.41072477910873673 ) ) ;
#55901 = EDGE_CURVE ( 'NONE', #1717, #21251, #70782, .T. ) ;
#55902 = CARTESIAN_POINT ( 'NONE',  ( 81.49499594866964003, 59.57084509763894431, -0.08682408883347023099 ) ) ;
#55903 = CARTESIAN_POINT ( 'NONE',  ( 168.8244094625508751, 257.0541383169796745, -14.93690306707719628 ) ) ;
#55904 = EDGE_CURVE ( 'NONE', #53182, #26719, #81772, .T. ) ;
#55905 = CARTESIAN_POINT ( 'NONE',  ( 206.1798448551755598, 273.5330285446045195, -10.53862763475382813 ) ) ;
#55906 = CYLINDRICAL_SURFACE ( 'NONE', #26292, 17.82106496071139645 ) ;
#55907 = CARTESIAN_POINT ( 'NONE',  ( 200.8769374536528858, 282.7179335918746688, 17.26928237494566787 ) ) ;
#55908 = CARTESIAN_POINT ( 'NONE',  ( -19.65312891409030271, 93.06504152958497400, 59.99999999999999289 ) ) ;
#55909 = EDGE_LOOP ( 'NONE', ( #28579, #5825, #18937, #43271 ) ) ;
#55910 = CARTESIAN_POINT ( 'NONE',  ( 155.0691674984522308, 262.0593185357093944, -17.32141920768173904 ) ) ;
#55911 = CARTESIAN_POINT ( 'NONE',  ( -52.42927860546615904, 87.56549226992709123, -10.00000000000000000 ) ) ;
#55912 = CARTESIAN_POINT ( 'NONE',  ( 74.94692089407371327, 66.84572622250871632, -13.20830831734917687 ) ) ;
#55913 = CARTESIAN_POINT ( 'NONE',  ( 207.5686001603237116, 271.1276337968068333, 7.659944433763431704 ) ) ;
#55914 = CARTESIAN_POINT ( 'NONE',  ( 14.14916430987532792, 185.6427522451419065, 10.00000000000009237 ) ) ;
#55916 = CARTESIAN_POINT ( 'NONE',  ( 97.82019495012963262, 215.0327760586659736, 1.948934522072302763E-15 ) ) ;
#55915 = B_SPLINE_CURVE_WITH_KNOTS ( 'NONE', 3,
 ( #36605, #30509, #14317, #99429, #60392, #5229, #52797, #59394, #7202, #74652, #67511, #75626, #60890, #6213, #5716, #13338, #82278, #98442, #76143, #52310, #51307, #61400, #44695, #83248, #90370, #45689, #12850, #51831, #29033, #38086, #76616, #45204, #29519, #91348, #21909, #82771, #6717, #37596, #68507, #30006, #91853, #59904, #36108, #68998, #22412, #99925, #67013, #90873, #53304, #84259 ),
 .UNSPECIFIED., .F., .F.,
 ( 4, 2, 2, 2, 2, 2, 2, 2, 2, 2, 2, 2, 2, 2, 2, 2, 2, 2, 2, 2, 2, 2, 2, 2, 4 ),
 ( 0.0001608434559496862688, 0.001169039375235548118, 0.001673137334878438886, 0.001925186314699919290, 0.002051210804610674454, 0.002177235294521429401, 0.002303259784432184782, 0.002429284274342939729, 0.002681333254164449623, 0.003185431213807470279, 0.004193627133093571872, 0.005201823052379673032, 0.005705921012022679810, 0.005957969991844181898, 0.006210018971665684853, 0.006273031216621136053, 0.006336043461576586384, 0.006399055706532036716, 0.006462067951487487916, 0.006714116931309142659, 0.006966165911130798270, 0.007218214890952453014, 0.007470263870774108625, 0.007722312850595764236, 0.008226410810239198623 ),
 .UNSPECIFIED. ) ;
#55917 = CARTESIAN_POINT ( 'NONE',  ( 82.29815274954648885, 40.89485058540869034, -1.228882935992447578 ) ) ;
#55918 = CARTESIAN_POINT ( 'NONE',  ( 174.5401493766550516, 282.4217946544197275, -14.57910214582674691 ) ) ;
#55919 = CARTESIAN_POINT ( 'NONE',  ( 167.0407061306596290, 278.0018592765986227, -13.72108455681485317 ) ) ;
#55921 = DIRECTION ( 'NONE',  ( 0.5000000000000001110, -0.8660254037844387076, -0.000000000000000000 ) ) ;
#55920 = CARTESIAN_POINT ( 'NONE',  ( 12.08367997547019002, 165.5327760586659451, 1.948934522072303157E-15 ) ) ;
#55922 = VECTOR ( 'NONE', #94618, 1000.000000000000000 ) ;
#55923 = CARTESIAN_POINT ( 'NONE',  ( 188.8544700204132880, 297.4231428397746413, 9.261439979758030461 ) ) ;
#55924 = VERTEX_POINT ( 'NONE', #74133 ) ;
#55925 = EDGE_LOOP ( 'NONE', ( #38509, #90227, #96795, #66364 ) ) ;
#55926 = CARTESIAN_POINT ( 'NONE',  ( 200.8035035346175619, 267.7285506604447392, -2.858260968050738704 ) ) ;
#55927 = CARTESIAN_POINT ( 'NONE',  ( 87.94702792923476409, 43.95278803585774341, 0.4997626018594838460 ) ) ;
#55928 = AXIS2_PLACEMENT_3D ( 'NONE', #714, #53415, #93963 ) ;
#55929 = CARTESIAN_POINT ( 'NONE',  ( 83.58440307966948524, 42.98227934588280874, 6.232988767175322131 ) ) ;
#55930 = CARTESIAN_POINT ( 'NONE',  ( 35.52916646935157274, 197.9865022471903160, -10.00000000000009592 ) ) ;
#55931 = CARTESIAN_POINT ( 'NONE',  ( 59.27500801855438795, 193.4824982072973683, 3.021315404115420679E-15 ) ) ;
#55932 = LINE ( 'NONE', #9886, #98478 ) ;
#55933 = CARTESIAN_POINT ( 'NONE',  ( 23.88258191050314494, 196.8464784336661637, 1.353441290958777525E-15 ) ) ;
#55934 = CARTESIAN_POINT ( 'NONE',  ( 77.00817486789581778, 225.2677522451419350, -5.000000000000047962 ) ) ;
#55935 = DIRECTION ( 'NONE',  ( -0.000000000000000000, -0.000000000000000000, -1.000000000000000000 ) ) ;
#55936 = ORIENTED_EDGE ( 'NONE', *, *, #89456, .T. ) ;
#55937 = CARTESIAN_POINT ( 'NONE',  ( 84.19046594057184052, 47.86424601814110247, 11.90803564236390422 ) ) ;
#55938 = CARTESIAN_POINT ( 'NONE',  ( 178.9714194486930694, 253.6239517424200187, 1.422777586239305059 ) ) ;
#55939 = EDGE_CURVE ( 'NONE', #92701, #50903, #90204, .T. ) ;
#55940 = CARTESIAN_POINT ( 'NONE',  ( 31.34407949807308569, 36.83478043621390441, -8.090169943749479842 ) ) ;
#55941 = CARTESIAN_POINT ( 'NONE',  ( 68.88995186411204941, 64.71362435216896358, -12.21736274004632783 ) ) ;
#55942 = CARTESIAN_POINT ( 'NONE',  ( 57.34764182315618797, 215.4637435831425307, 2.679491924311251605 ) ) ;
#55943 = VECTOR ( 'NONE', #39841, 1000.000000000000000 ) ;
#55944 = CARTESIAN_POINT ( 'NONE',  ( 186.6671973743490582, 282.6820187201159342, 16.18259547852653313 ) ) ;
#55945 = CARTESIAN_POINT ( 'NONE',  ( 194.4032909867620447, 293.9306181827685123, -16.05392006271526384 ) ) ;
#55946 = EDGE_CURVE ( 'NONE', #98647, #59479, #8201, .T. ) ;
#55947 = CARTESIAN_POINT ( 'NONE',  ( 67.72512177463541150, 68.26770340457413511, -7.327815147115877004 ) ) ;
#55948 = CARTESIAN_POINT ( 'NONE',  ( 171.7403546589055452, 279.6099264174512200, 14.56001095287713021 ) ) ;
#55949 = CARTESIAN_POINT ( 'NONE',  ( 146.7434471017767521, 276.4798892723637209, 0.7354350123930684102 ) ) ;
#55950 = CARTESIAN_POINT ( 'NONE',  ( 148.4016473149517594, 273.6078022540229426, 8.470066617688926769 ) ) ;
#55951 = ORIENTED_EDGE ( 'NONE', *, *, #36707, .F. ) ;
#55952 = AXIS2_PLACEMENT_3D ( 'NONE', #90902, #37139, #6244 ) ;
#55953 = CARTESIAN_POINT ( 'NONE',  ( 207.8725590214046406, 270.6011616060040410, 1.988011721677743093 ) ) ;
#55954 = CARTESIAN_POINT ( 'NONE',  ( 181.1274570500190464, 268.2429819168116296, 15.60512382003630982 ) ) ;
#55955 = CARTESIAN_POINT ( 'NONE',  ( 111.1617914095948692, 244.1744531367911293, 4.594050593750047540 ) ) ;
#55956 = CARTESIAN_POINT ( 'NONE',  ( 18.38602693954342371, 22.56628583063840310, 9.188101187500006262 ) ) ;
#55958 = EDGE_CURVE ( 'NONE', #91009, #47559, #77093, .T. ) ;
#55957 = CARTESIAN_POINT ( 'NONE',  ( 74.66874582000750138, 67.11449834074296916, 12.47724195657757029 ) ) ;
#55959 = CARTESIAN_POINT ( 'NONE',  ( 82.44310520575160695, 54.28011738120408580, -15.96781897959229113 ) ) ;
#55961 = DIRECTION ( 'NONE',  ( -0.000000000000000000, -0.000000000000000000, -1.000000000000000000 ) ) ;
#55960 = CARTESIAN_POINT ( 'NONE',  ( -52.31886624268647523, 30.86069821571189919, -10.00000000000000000 ) ) ;
#55962 = CARTESIAN_POINT ( 'NONE',  ( 150.9165176611652157, 269.2519190399329432, -13.92901968401340262 ) ) ;
#55963 = CYLINDRICAL_SURFACE ( 'NONE', #94101, 17.82106496071139645 ) ;
#55964 = CARTESIAN_POINT ( 'NONE',  ( 149.7200635338602410, 271.3242383773507527, -12.12223662813266500 ) ) ;
#55965 = CARTESIAN_POINT ( 'NONE',  ( 81.50068165357551209, 227.8615022471903160, 5.000000000000046185 ) ) ;
#55966 = CARTESIAN_POINT ( 'NONE',  ( 172.7682828100511188, 290.3836512414355298, -1.901510031099399978 ) ) ;
#55967 = CARTESIAN_POINT ( 'NONE',  ( -17.42236680055705023, 149.2012482093457777, 0.000000000000000000 ) ) ;
#55968 = ORIENTED_EDGE ( 'NONE', *, *, #61510, .T. ) ;
#55969 = CARTESIAN_POINT ( 'NONE',  ( 43.33680334696484948, 124.1889737374328462, -10.00000000000000000 ) ) ;
#55970 = CARTESIAN_POINT ( 'NONE',  ( 175.5198215696162265, 278.6707974891042454, 15.42220655511384564 ) ) ;
#55971 = CARTESIAN_POINT ( 'NONE',  ( 165.5298684834693574, 269.3554679133272884, -17.63324793928101997 ) ) ;
#55973 = VERTEX_POINT ( 'NONE', #39071 ) ;
#55972 = EDGE_CURVE ( 'NONE', #13906, #57617, #79265, .T. ) ;
#55974 = CARTESIAN_POINT ( 'NONE',  ( 72.11864215578678738, 72.30468452837580173, 1.217881537791027702 ) ) ;
#55975 = ADVANCED_FACE ( 'NONE', ( #61876 ), #16293, .T. ) ;
#55976 = CYLINDRICAL_SURFACE ( 'NONE', #53609, 14.82106496071141066 ) ;
#55977 = CARTESIAN_POINT ( 'NONE',  ( 155.8723835780803881, 261.2467561593892356, 17.10610717069041797 ) ) ;
#55978 = CARTESIAN_POINT ( 'NONE',  ( -19.65312891409030271, 93.06504152958497400, -10.00000000000000888 ) ) ;
#55979 = CARTESIAN_POINT ( 'NONE',  ( 192.1883190596398094, 297.7670620978826150, 12.41391288785556668 ) ) ;
#55980 = ORIENTED_EDGE ( 'NONE', *, *, #82033, .T. ) ;
#55981 = CARTESIAN_POINT ( 'NONE',  ( 191.2104420009116836, 280.2857515794617598, 17.80337293751487593 ) ) ;
#55982 = CARTESIAN_POINT ( 'NONE',  ( 32.59967566254915994, 39.79752408145595410, -5.678558825948271327 ) ) ;
#55983 = CARTESIAN_POINT ( 'NONE',  ( 188.7308569474326134, 285.6752924799993707, 17.07521345989996320 ) ) ;
#55984 = VERTEX_POINT ( 'NONE', #46692 ) ;
#55985 = CARTESIAN_POINT ( 'NONE',  ( 166.1807419043942673, 280.1926019274495161, 11.70936788950543495 ) ) ;
#55986 = CARTESIAN_POINT ( 'NONE',  ( -41.22173478680166880, 38.49732326316120634, 59.99999999999999289 ) ) ;
#55987 = CARTESIAN_POINT ( 'NONE',  ( 164.6558840558436714, 246.1165554557707082, -1.230166818256332117 ) ) ;
#55988 = ORIENTED_EDGE ( 'NONE', *, *, #41699, .F. ) ;
#55989 = CARTESIAN_POINT ( 'NONE',  ( 86.29029894244921195, 46.98537786981302844, -10.03429304951027490 ) ) ;
#55990 = CARTESIAN_POINT ( 'NONE',  ( 188.7753597038515920, 293.7201965824127115, 12.88945448372762570 ) ) ;
#55991 = B_SPLINE_CURVE_WITH_KNOTS ( 'NONE', 3,
 ( #46898, #22605, #69195, #53978 ),
 .UNSPECIFIED., .F., .F.,
 ( 4, 4 ),
 ( 0.000000000000000000, 0.004243563290278051271 ),
 .UNSPECIFIED. ) ;
#55992 = DIRECTION ( 'NONE',  ( -0.3535533905932733423, 0.6123724356957830350, 0.7071067811865577868 ) ) ;
#55993 = FACE_OUTER_BOUND ( 'NONE', #19589, .T. ) ;
#55994 = AXIS2_PLACEMENT_3D ( 'NONE', #49348, #96484, #27053 ) ;
#55995 = CARTESIAN_POINT ( 'NONE',  ( 45.29353982640898835, 28.01110640527296525, 2.839279412974134775 ) ) ;
#55996 = VECTOR ( 'NONE', #58053, 1000.000000000000000 ) ;
#55997 = CARTESIAN_POINT ( 'NONE',  ( 203.5629025532486196, 278.0657055720176913, -15.85226727704602823 ) ) ;
#55998 = EDGE_LOOP ( 'NONE', ( #94804, #25938, #95001, #28154 ) ) ;
#55999 = EDGE_CURVE ( 'NONE', #12449, #42468, #78614, .T. ) ;
#56000 = ORIENTED_EDGE ( 'NONE', *, *, #20158, .F. ) ;
#56002 = VECTOR ( 'NONE', #66632, 1000.000000000000000 ) ;
#56001 = CARTESIAN_POINT ( 'NONE',  ( 176.4420281119471952, 259.8590673950340033, 12.32580266317428652 ) ) ;
#56003 = ORIENTED_EDGE ( 'NONE', *, *, #38388, .T. ) ;
#56004 = CARTESIAN_POINT ( 'NONE',  ( 77.14924902310487198, 49.32506698715211257, -14.89041676429049232 ) ) ;
#56005 = ORIENTED_EDGE ( 'NONE', *, *, #83531, .F. ) ;
#56006 = CARTESIAN_POINT ( 'NONE',  ( 173.3310713462738306, 270.5831704705003631, 16.79086624453662679 ) ) ;
#56007 = CARTESIAN_POINT ( 'NONE',  ( 203.3041373168503299, 278.5139001086923827, -16.61929732091214973 ) ) ;
#56008 = ORIENTED_EDGE ( 'NONE', *, *, #4528, .F. ) ;
#56009 = EDGE_CURVE ( 'NONE', #53637, #13224, #98620, .T. ) ;
#56010 = CARTESIAN_POINT ( 'NONE',  ( 164.3231499090067302, 246.0309508282801971, -1.360008376207661573 ) ) ;
#56011 = CARTESIAN_POINT ( 'NONE',  ( 190.0953138929461375, 301.3922533871005385, 3.399835324073681608 ) ) ;
#56012 = DIRECTION ( 'NONE',  ( -0.03004293549037828290, -0.9995486091367047354, 0.000000000000000000 ) ) ;
#56013 = CARTESIAN_POINT ( 'NONE',  ( 192.8607783413999073, 296.6023284558532396, -11.80574095728561446 ) ) ;
#56014 = CARTESIAN_POINT ( 'NONE',  ( 153.0444155045374544, 265.5662918618958201, -16.15173036748435109 ) ) ;
#56015 = DIRECTION ( 'NONE',  ( -0.000000000000000000, -1.000000000000000000, -0.000000000000000000 ) ) ;
#56016 = CARTESIAN_POINT ( 'NONE',  ( 157.7016178275996481, 280.8566103467931043, 2.084903823814490131 ) ) ;
#56017 = EDGE_CURVE ( 'NONE', #9204, #66666, #34533, .T. ) ;
#56018 = CARTESIAN_POINT ( 'NONE',  ( 121.7437996339097310, 241.0958772461660544, -9.188101187500095079 ) ) ;
#56019 = ORIENTED_EDGE ( 'NONE', *, *, #7343, .F. ) ;
#56020 = CARTESIAN_POINT ( 'NONE',  ( 75.65485643130637072, 54.67754446188314432, 16.11849813384655050 ) ) ;
#56021 = VERTEX_POINT ( 'NONE', #34492 ) ;
#56022 = ADVANCED_FACE ( 'NONE', ( #95850 ), #41585, .F. ) ;
#56024 = VERTEX_POINT ( 'NONE', #34982 ) ;
#56023 = PLANE ( 'NONE',  #29882 ) ;
#56025 = AXIS2_PLACEMENT_3D ( 'NONE', #94828, #49207, #72008 ) ;
#56026 = CARTESIAN_POINT ( 'NONE',  ( 201.6144114969290229, 275.0453523290713065, 13.34253202614237033 ) ) ;
#56027 = CARTESIAN_POINT ( 'NONE',  ( 23.46864935082055581, 158.3759306620404743, -30.52142883766493853 ) ) ;
#56028 = CARTESIAN_POINT ( 'NONE',  ( 174.2958066453992103, 290.3206272445223135, -4.802435633763557199 ) ) ;
#56029 = CARTESIAN_POINT ( 'NONE',  ( 146.6773087776009277, 276.5944442101636582, 3.546544321270581612 ) ) ;
#56030 = CARTESIAN_POINT ( 'NONE',  ( 71.12465364093185372, 72.19127489105424900, 0.5914781838053912999 ) ) ;
#56031 = CARTESIAN_POINT ( 'NONE',  ( 80.81823777232595774, 43.03079984276644154, 9.681521901304016353 ) ) ;
#56032 = CARTESIAN_POINT ( 'NONE',  ( 173.9326749925096465, 287.2443000551036221, -9.522606441215669903 ) ) ;
#56033 = VECTOR ( 'NONE', #37033, 1000.000000000000000 ) ;
#56034 = DIRECTION ( 'NONE',  ( 1.000000000000000000, 0.000000000000000000, 0.000000000000000000 ) ) ;
#56035 = CARTESIAN_POINT ( 'NONE',  ( -11.38800805193611154, 34.97435025094601713, 59.99999999999999289 ) ) ;
#56036 = VERTEX_POINT ( 'NONE', #65884 ) ;
#56037 = CARTESIAN_POINT ( 'NONE',  ( 147.6512387128590262, 274.9075480792844246, -8.209968531507987777 ) ) ;
#56038 = CARTESIAN_POINT ( 'NONE',  ( 152.8861948602045402, 273.8046404715449853, 12.06949787893822013 ) ) ;
#56039 = ORIENTED_EDGE ( 'NONE', *, *, #37565, .T. ) ;
#56040 = CARTESIAN_POINT ( 'NONE',  ( 162.9254136962317148, 277.9293967287522946, 13.77390558128574760 ) ) ;
#56041 = B_SPLINE_CURVE_WITH_KNOTS ( 'NONE', 3,
 ( #70297, #77422, #40386, #408 ),
 .UNSPECIFIED., .F., .F.,
 ( 4, 4 ),
 ( 0.01598569196496549966, 0.02481275599104538002 ),
 .UNSPECIFIED. ) ;
#56042 = CARTESIAN_POINT ( 'NONE',  ( 159.8161384505802971, 279.1487373509320946, 10.85936962484722201 ) ) ;
#56043 = CARTESIAN_POINT ( 'NONE',  ( 151.9574818334562565, 267.4489162046660340, -15.47372068035671155 ) ) ;
#56044 = DIRECTION ( 'NONE',  ( -0.4851478631379979034, 0.8403007481384877631, 0.2419218955996582654 ) ) ;
#56045 = CARTESIAN_POINT ( 'NONE',  ( 163.3706531435203146, 247.6807236201477735, 10.06957846017757241 ) ) ;
#56047 = CARTESIAN_POINT ( 'NONE',  ( 154.4362440790400797, 276.8969399611219160, -8.726023671585549479 ) ) ;
#56046 = CARTESIAN_POINT ( 'NONE',  ( 164.7244464148843690, 284.0693728551247546, -6.859052662106053688 ) ) ;
#56048 = CARTESIAN_POINT ( 'NONE',  ( 200.4385098325799675, 267.3393730264926376, 6.361263591900818248 ) ) ;
#56049 = ORIENTED_EDGE ( 'NONE', *, *, #55877, .F. ) ;
#56050 = CARTESIAN_POINT ( 'NONE',  ( 167.1454213690836639, 281.4972382487084133, -10.93374221028199322 ) ) ;
#56051 = CARTESIAN_POINT ( 'NONE',  ( 163.5491121955337803, 247.7522377084982281, -7.761536679276979989 ) ) ;
#56052 = DIRECTION ( 'NONE',  ( -0.4999999999999987788, 0.8660254037844392627, 0.000000000000000000 ) ) ;
#56053 = CARTESIAN_POINT ( 'NONE',  ( 85.25577013208754806, 208.4824982072973967, 3.021315404115420679E-15 ) ) ;
#56054 = CARTESIAN_POINT ( 'NONE',  ( 188.6013203369844575, 298.5946043969738639, -4.227064913786014344 ) ) ;
#56055 = CARTESIAN_POINT ( 'NONE',  ( 188.5612436805310779, 268.6432733723845558, 15.05044350854306323 ) ) ;
#56056 = DIRECTION ( 'NONE',  ( 1.000000000000000000, -1.784287003861858500E-15, 0.000000000000000000 ) ) ;
#56057 = CARTESIAN_POINT ( 'NONE',  ( -12.91644128716779072, 174.8967562850347406, 1.347971487989956912E-14 ) ) ;
#56058 = CARTESIAN_POINT ( 'NONE',  ( 69.88429420325151398, 70.97642176483110177, -1.039711900314023829 ) ) ;
#56059 = CARTESIAN_POINT ( 'NONE',  ( -9.892408837089959661, 177.3464784336661637, 1.353441290958777525E-15 ) ) ;
#56060 = CARTESIAN_POINT ( 'NONE',  ( 83.80088808272151368, 225.3149278399160949, 9.188101187500093303 ) ) ;
#56061 = CARTESIAN_POINT ( 'NONE',  ( 67.59152061837809811, 66.69868789956184685, 8.645681936733796036 ) ) ;
#56062 = CARTESIAN_POINT ( 'NONE',  ( 88.03469742524457331, 44.28626028149027860, -4.397723919905312862 ) ) ;
#56063 = CARTESIAN_POINT ( 'NONE',  ( 182.8053931574769422, 294.3809610745131522, -8.049654163022442077 ) ) ;
#56064 = DIRECTION ( 'NONE',  ( -0.8660254037844379305, -0.5000000000000014433, 0.000000000000000000 ) ) ;
#56065 = CIRCLE ( 'NONE', #35114, 17.82106496071138935 ) ;
#56066 = DIRECTION ( 'NONE',  ( -0.8660254037844387076, -0.4999999999999998890, -0.000000000000000000 ) ) ;
#56067 = CARTESIAN_POINT ( 'NONE',  ( 84.87428755225029420, 50.22423732196602941, -13.34510061061973829 ) ) ;
#56068 = AXIS2_PLACEMENT_3D ( 'NONE', #2994, #72384, #81015 ) ;
#56069 = CARTESIAN_POINT ( 'NONE',  ( 77.59444824636439364, 61.81028894563407050, 15.66474382954858413 ) ) ;
#56071 = CARTESIAN_POINT ( 'NONE',  ( 208.1303168694798273, 270.1547119170880364, -0.9257663487928086132 ) ) ;
#56070 = DIRECTION ( 'NONE',  ( 0.8944271909999157444, 0.000000000000000000, -0.4472135954999582608 ) ) ;
#56072 = CARTESIAN_POINT ( 'NONE',  ( 161.4650976420346637, 250.9812425653634023, 12.76171476511797565 ) ) ;
#56073 = CARTESIAN_POINT ( 'NONE',  ( 168.8088173946568702, 251.8078635755704511, -8.785532002324718093 ) ) ;
#56074 =( BOUNDED_CURVE ( )  B_SPLINE_CURVE ( 2, ( #76965, #99293, #29874, #59764, #67882, #90733, #98803, #7566, #60746 ),
 .UNSPECIFIED., .F., .T. ) 
 B_SPLINE_CURVE_WITH_KNOTS ( ( 3, 2, 2, 2, 3 ),
 ( 0.6008064516129032473, 0.6021505376344086224, 0.6048387096774193727, 0.6075268817204301230, 0.6088709677419354982 ),
 .UNSPECIFIED. ) 
 CURVE ( )  GEOMETRIC_REPRESENTATION_ITEM ( )  RATIONAL_B_SPLINE_CURVE ( ( 0.9330127018922194093, 0.9330127018922194093, 1.000000000000000000, 0.8660254037844387076, 1.000000000000000000, 0.8660254037844387076, 1.000000000000000000, 0.9330127018922194093, 0.9330127018922194093 ) ) 
 REPRESENTATION_ITEM ( '' )  );
#56075 = DIRECTION ( 'NONE',  ( 0.7548338719222560389, -0.6559160203858837024, 0.000000000000000000 ) ) ;
#56076 = VECTOR ( 'NONE', #87646, 1000.000000000000227 ) ;
#56077 = CARTESIAN_POINT ( 'NONE',  ( -54.21831688459418785, 33.63902229265146104, -10.00000000000000000 ) ) ;
#56078 = CARTESIAN_POINT ( 'NONE',  ( 80.01979875032591849, 57.54866692369600401, 16.59896302490741604 ) ) ;
#56079 = CARTESIAN_POINT ( 'NONE',  ( 73.43248428410468875, 69.89844921070914552, 9.717079046730820124 ) ) ;
#56080 = CARTESIAN_POINT ( 'NONE',  ( 45.42531092540608029, 197.0333772461660828, 9.188101187500095079 ) ) ;
#56081 = CARTESIAN_POINT ( 'NONE',  ( 76.83812372118222811, 63.31165668814058023, -15.46182035231785079 ) ) ;
#56082 = CARTESIAN_POINT ( 'NONE',  ( 64.91088251055593616, 208.2833772461660544, -9.188101187500095079 ) ) ;
#56083 = LINE ( 'NONE', #24700, #70939 ) ;
#56085 = EDGE_CURVE ( 'NONE', #45306, #61384, #41073, .T. ) ;
#56084 = CARTESIAN_POINT ( 'NONE',  ( 88.36916805580219147, 44.19665079577453071, 0.1927284833306444622 ) ) ;
#56086 = CARTESIAN_POINT ( 'NONE',  ( 167.1743255730581552, 259.8161784781199231, 15.97983238844050824 ) ) ;
#56088 = LINE ( 'NONE', #58103, #3718 ) ;
#56087 = CARTESIAN_POINT ( 'NONE',  ( 198.6959030336114438, 286.1027943447343205, -17.01025293640724811 ) ) ;
#56089 = DIRECTION ( 'NONE',  ( -0.8769651246872975925, 0.4805540241036304061, 0.000000000000000000 ) ) ;
#56090 = CARTESIAN_POINT ( 'NONE',  ( 25.79477067763620468, 36.93396525600391556, 2.839279412974139660 ) ) ;
#56091 = AXIS2_PLACEMENT_3D ( 'NONE', #36757, #61547, #30666 ) ;
#56092 = FACE_OUTER_BOUND ( 'NONE', #77106, .T. ) ;
#56093 = CARTESIAN_POINT ( 'NONE',  ( 196.4242782546697015, 290.4301655533025155, -16.42402868779123537 ) ) ;
#56094 = ORIENTED_EDGE ( 'NONE', *, *, #35429, .T. ) ;
#56095 = CARTESIAN_POINT ( 'NONE',  ( 13.67041502465407277, 29.93396525600389424, 2.839279412974139660 ) ) ;
#56096 = CARTESIAN_POINT ( 'NONE',  ( 74.46396492422927338, 222.9869531367911293, 4.594050593750046652 ) ) ;
#56097 = CARTESIAN_POINT ( 'NONE',  ( 76.57610849078304227, 63.76548037954881920, 14.87549170960290645 ) ) ;
#56098 = DIRECTION ( 'NONE',  ( -0.9991767892008870389, -0.04056776950001317328, 0.000000000000000000 ) ) ;
#56099 = VECTOR ( 'NONE', #2124, 1000.000000000000000 ) ;
#56100 = CARTESIAN_POINT ( 'NONE',  ( 172.7227978551848651, 290.4444241243636498, -0.3282510524908365257 ) ) ;
#56101 = CARTESIAN_POINT ( 'NONE',  ( 156.6812872898450735, 261.2670451491295012, 0.000000000000000000 ) ) ;
#56102 = CARTESIAN_POINT ( 'NONE',  ( 201.9631990782953892, 280.8364732676815834, 16.42174701891640964 ) ) ;
#56103 = EDGE_CURVE ( 'NONE', #75148, #60835, #2783, .T. ) ;
#56104 = AXIS2_PLACEMENT_3D ( 'NONE', #82498, #36327, #60110 ) ;
#56105 = EDGE_CURVE ( 'NONE', #55035, #8715, #3135, .T. ) ;
#56106 = DIRECTION ( 'NONE',  ( 0.5000000000000001110, -0.8660254037844384856, -0.000000000000000000 ) ) ;
#56107 = CARTESIAN_POINT ( 'NONE',  ( 193.4977959244270096, 288.4670934838076164, 16.06266015785881507 ) ) ;
#56108 = CARTESIAN_POINT ( 'NONE',  ( 134.2560625007776878, 234.9865022471901455, 1.119607411625061291E-15 ) ) ;
#56109 = LINE ( 'NONE', #39900, #31242 ) ;
#56110 = CARTESIAN_POINT ( 'NONE',  ( 164.2672861321391053, 246.1277097281173667, -2.417001679502223777 ) ) ;
#56111 = EDGE_LOOP ( 'NONE', ( #7816, #63510 ) ) ;
#56112 = CARTESIAN_POINT ( 'NONE',  ( 188.4697100348334402, 272.9738383098946315, 15.64619135176044118 ) ) ;
#56113 = ORIENTED_EDGE ( 'NONE', *, *, #82460, .T. ) ;
#56114 = CARTESIAN_POINT ( 'NONE',  ( 202.6551236945213361, 279.6380246773706517, 15.55476940527561425 ) ) ;
#56115 = CARTESIAN_POINT ( 'NONE',  ( 39.20103187901341357, 54.69033006916458106, 10.00000000000000000 ) ) ;
#56116 = CARTESIAN_POINT ( 'NONE',  ( 73.24164692391426001, 68.69381212440423212, -10.32746940148697234 ) ) ;
#56117 = VERTEX_POINT ( 'NONE', #57781 ) ;
#56118 = DIRECTION ( 'NONE',  ( 0.9862134920484671996, 0.1654779384134575648, 0.000000000000000000 ) ) ;
#56119 = ORIENTED_EDGE ( 'NONE', *, *, #67984, .F. ) ;
#56120 = DIRECTION ( 'NONE',  ( -0.9997716407803077798, 0.02136975178731310987, 0.000000000000000000 ) ) ;
#56121 = CARTESIAN_POINT ( 'NONE',  ( 170.8439429942262962, 250.1382644172885250, 2.884658875547349677 ) ) ;
#56122 = LINE ( 'NONE', #47039, #19207 ) ;
#56123 = ORIENTED_EDGE ( 'NONE', *, *, #7869, .F. ) ;
#56124 = CARTESIAN_POINT ( 'NONE',  ( 23.32838594064934767, 31.65586893147757408, -7.433330006724137462 ) ) ;
#56125 = CARTESIAN_POINT ( 'NONE',  ( 84.73244144816675316, 50.45694327749722419, -13.52220349883642569 ) ) ;
#56126 = LINE ( 'NONE', #63750, #99601 ) ;
#56127 = PLANE ( 'NONE',  #98354 ) ;
#56128 = CARTESIAN_POINT ( 'NONE',  ( 51.26196130476894552, 193.7365022471901739, -10.00000000000009237 ) ) ;
#56129 = ORIENTED_EDGE ( 'NONE', *, *, #68249, .T. ) ;
#56130 = ORIENTED_EDGE ( 'NONE', *, *, #10976, .T. ) ;
#56131 = DIRECTION ( 'NONE',  ( -3.977257660627182967E-15, 7.954515321254365934E-15, 1.000000000000000000 ) ) ;
#56132 = ADVANCED_FACE ( 'NONE', ( #19330 ), #50192, .F. ) ;
#56134 = CARTESIAN_POINT ( 'NONE',  ( 180.7942833579522812, 266.7097690628117448, -16.23795806611159520 ) ) ;
#56133 = CARTESIAN_POINT ( 'NONE',  ( 67.69820113011998330, 65.71482418403419956, 10.68697367106847196 ) ) ;
#56135 = CARTESIAN_POINT ( 'NONE',  ( 81.78067039160912088, 55.44360204288782512, -15.94198801934737908 ) ) ;
#56136 = CARTESIAN_POINT ( 'NONE',  ( 194.2669918475045279, 294.1666952169902629, 14.00965265288584050 ) ) ;
#56137 = CARTESIAN_POINT ( 'NONE',  ( 185.5198499209504064, 292.6877627818749374, -10.71450089700853070 ) ) ;
#56138 = CARTESIAN_POINT ( 'NONE',  ( 157.0877926458200307, 258.5629572190321710, -17.40668770468195703 ) ) ;
#56139 = CARTESIAN_POINT ( 'NONE',  ( 164.1007040320689612, 246.4162383890708270, 4.419515984332184289 ) ) ;
#56140 = CARTESIAN_POINT ( 'NONE',  ( 76.43459130371124388, 61.29278126438280339, -15.98275306604615054 ) ) ;
#56141 = PLANE ( 'NONE',  #90415 ) ;
#56142 = CARTESIAN_POINT ( 'NONE',  ( 82.61045024828291616, 212.3768266524159856, -9.188101187500091527 ) ) ;
#56143 = ORIENTED_EDGE ( 'NONE', *, *, #5384, .T. ) ;
#56144 = CARTESIAN_POINT ( 'NONE',  ( 191.0816511748900268, 299.6838671013740623, 7.311127128005925790 ) ) ;
#56145 = CARTESIAN_POINT ( 'NONE',  ( 164.7364331287320738, 247.3151232938002693, -7.618980141130590411 ) ) ;
#56146 = VECTOR ( 'NONE', #76162, 1000.000000000000114 ) ;
#56147 = VERTEX_POINT ( 'NONE', #44067 ) ;
#56148 = CARTESIAN_POINT ( 'NONE',  ( 156.7071728003359965, 259.2222101297794552, -17.92398391197042073 ) ) ;
#56149 = AXIS2_PLACEMENT_3D ( 'NONE', #88114, #18664, #49544 ) ;
#56150 = ORIENTED_EDGE ( 'NONE', *, *, #47729, .F. ) ;
#56151 = CARTESIAN_POINT ( 'NONE',  ( 79.99398376985880077, 44.81349857560560679, -11.27244585305868085 ) ) ;
#56152 = ADVANCED_FACE ( 'NONE', ( #5587 ), #43584, .T. ) ;
#56153 = CARTESIAN_POINT ( 'NONE',  ( -63.30067564770008914, 39.94154026010144065, -10.00000000000000000 ) ) ;
#56155 = B_SPLINE_SURFACE_WITH_KNOTS ( 'NONE', 3, 1, ( 
 ( #99929, #21426 ),
 ( #6721, #59907 ),
 ( #30010, #45208 ),
 ( #84751, #46190 ),
 ( #91857, #52313 ),
 ( #37600, #44699 ),
 ( #22416, #53307 ),
 ( #15291, #52801 ),
 ( #76147, #44205 ),
 ( #84262, #77107 ),
 ( #38089, #68015 ),
 ( #14809, #45692 ),
 ( #76620, #7711 ),
 ( #7205, #75630 ),
 ( #30512, #6216 ),
 ( #83251, #37112 ),
 ( #98445, #61403 ),
 ( #22904, #92356 ),
 ( #29522, #13817 ),
 ( #38603, #97941 ),
 ( #75141, #28515 ),
 ( #59398, #90374 ),
 ( #20952, #51834 ),
 ( #82775, #5720 ),
 ( #36608, #60395 ),
 ( #14321, #67515 ),
 ( #91351, #48729 ),
 ( #69507, #87297 ),
 ( #616, #79160 ),
 ( #93860, #24415 ),
 ( #9217, #46708 ),
 ( #70507, #40092 ),
 ( #55291, #39088 ),
 ( #39586, #122 ) ),
 .UNSPECIFIED., .T., .F., .F.,
 ( 4, 2, 2, 2, 2, 2, 2, 2, 2, 2, 2, 2, 2, 2, 2, 2, 4 ),
 ( 2, 2 ),
 ( 0.000000000000000000, 0.06250000000000000000, 0.1250000000000000000, 0.1875000000000000000, 0.2500000000000000000, 0.3125000000000000000, 0.3750000000000000000, 0.4375000000000000000, 0.5000000000000000000, 0.5625000000000000000, 0.6250000000000000000, 0.6875000000000000000, 0.7500000000000000000, 0.8125000000000000000, 0.8750000000000000000, 0.9375000000000000000, 1.000000000000000000 ),
 ( 0.000000000000000000, 1.000000000000000000 ),
 .UNSPECIFIED. ) ;
#56154 = CARTESIAN_POINT ( 'NONE',  ( 191.4082244002820516, 299.1182256826033949, -8.271837126846561361 ) ) ;
#56156 = CARTESIAN_POINT ( 'NONE',  ( 83.37551210837683868, 41.64352063595823239, -2.325603929493660793 ) ) ;
#56157 = CARTESIAN_POINT ( 'NONE',  ( 84.30219332075782290, 47.40784315339518429, -11.50221644715631442 ) ) ;
#56158 = FACE_OUTER_BOUND ( 'NONE', #99525, .T. ) ;
#56159 = CARTESIAN_POINT ( 'NONE',  ( 99.20033616346982797, 218.8923013555410080, 4.594050593750050204 ) ) ;
#56160 = B_SPLINE_CURVE_WITH_KNOTS ( 'NONE', 3,
 ( #63402, #63898, #26907, #64909, #57786, #2621, #18811, #95368, #25921, #79648, #41079, #49695, #56793, #87779, #94340, #19335, #49215, #11716, #17297, #80147, #71524, #80649, #88762, #41589, #24895, #55770, #50197, #34022, #86763, #73025, #81149, #42577, #73510, #48200, #79147, #9729, #40583, #59779, #13698, #27410, #58289, #28902, #44071, #82654, #5591, #59264 ),
 .UNSPECIFIED., .F., .F.,
 ( 4, 1, 1, 1, 2, 2, 1, 1, 1, 2, 2, 1, 1, 2, 2, 1, 1, 2, 2, 1, 1, 2, 2, 1, 2, 2, 1, 2, 2, 4 ),
 ( 0.000000000000000000, 0.06249999999997057909, 0.09374999999995715927, 0.1093749999999491240, 0.1171874999999468620, 0.1249999999999445999, 0.1874999999999323874, 0.2187499999999275579, 0.2343749999999261702, 0.2421874999999250877, 0.2499999999999240052, 0.3124999999999299449, 0.3437499999999344968, 0.3593749999999367728, 0.3749999999999391043, 0.4374999999999454880, 0.4687499999999472089, 0.4843749999999496514, 0.4999999999999521494, 0.5624999999999568123, 0.5937499999999590328, 0.6093749999999601430, 0.6249999999999612532, 0.6874999999999653610, 0.7187499999999689138, 0.7499999999999725775, 0.8124999999999800160, 0.8437499999999837907, 0.8749999999999876765, 1.000000000000000000 ),
 .UNSPECIFIED. ) ;
#56161 = ORIENTED_EDGE ( 'NONE', *, *, #23778, .T. ) ;
#56162 = ORIENTED_EDGE ( 'NONE', *, *, #17619, .F. ) ;
#56163 = CARTESIAN_POINT ( 'NONE',  ( 207.7625791259561652, 270.7916523727319031, -1.015623356719550063 ) ) ;
#56164 = EDGE_LOOP ( 'NONE', ( #47146, #43049, #24721, #70197 ) ) ;
#56165 = DIRECTION ( 'NONE',  ( 0.4999999999999998890, -0.8660254037844385966, 0.000000000000000000 ) ) ;
#56166 = CARTESIAN_POINT ( 'NONE',  ( 164.9101359252495627, 286.5608941336866451, 1.040025780022917790 ) ) ;
#56167 = DIRECTION ( 'NONE',  ( -0.4999999999999998890, 0.8660254037844385966, 0.000000000000000000 ) ) ;
#56168 = FACE_OUTER_BOUND ( 'NONE', #18647, .T. ) ;
#56169 = EDGE_LOOP ( 'NONE', ( #38559, #27350, #33092, #52997 ) ) ;
#56170 = AXIS2_PLACEMENT_3D ( 'NONE', #95499, #12342, #18452 ) ;
#56171 = CARTESIAN_POINT ( 'NONE',  ( 204.4345574087956550, 276.5559550755466489, 14.49589339982634861 ) ) ;
#56172 = CARTESIAN_POINT ( 'NONE',  ( 80.94948737998437593, 46.40359012725748755, 12.14654003525263271 ) ) ;
#56173 = CARTESIAN_POINT ( 'NONE',  ( 206.0930919633010774, 273.6832889610345774, -9.866500005465628220 ) ) ;
#56174 = CARTESIAN_POINT ( 'NONE',  ( 84.99999999999998579, 14.99999999999999467, -2.106367960268910711 ) ) ;
#56175 = CARTESIAN_POINT ( 'NONE',  ( 71.71174882302005926, 58.93038559421764688, -15.88944412480316259 ) ) ;
#56176 = B_SPLINE_CURVE_WITH_KNOTS ( 'NONE', 3,
 ( #18006, #10903, #3316, #72212, #71716, #27603, #42762, #64089, #41778, #81825, #34196, #73205, #2816, #48898 ),
 .UNSPECIFIED., .F., .F.,
 ( 4, 2, 2, 2, 2, 2, 4 ),
 ( 0.000000000000000000, 0.0004778436358628718899, 0.0007167654537943066693, 0.0009556872717257413946, 0.001194609089657176337, 0.001433530907588610953, 0.001911374543451394101 ),
 .UNSPECIFIED. ) ;
#56177 = CARTESIAN_POINT ( 'NONE',  ( 19.12011368430507829, 34.47266676343468106, -10.00000000000000000 ) ) ;
#56178 = EDGE_CURVE ( 'NONE', #36317, #61038, #20808, .T. ) ;
#56179 = DIRECTION ( 'NONE',  ( 0.000000000000000000, 0.000000000000000000, 1.000000000000000000 ) ) ;
#56180 = ORIENTED_EDGE ( 'NONE', *, *, #15402, .T. ) ;
#56181 = CARTESIAN_POINT ( 'NONE',  ( 203.5600082621025138, 276.7824627000144915, -14.31784352948871586 ) ) ;
#56182 = CARTESIAN_POINT ( 'NONE',  ( 200.5438717407500917, 283.2948203288816558, 18.39667691545567152 ) ) ;
#56183 = AXIS2_PLACEMENT_3D ( 'NONE', #12152, #18757, #49155 ) ;
#56184 = FACE_OUTER_BOUND ( 'NONE', #53767, .T. ) ;
#56185 = CARTESIAN_POINT ( 'NONE',  ( 170.8523262845096156, 251.5461551665960656, 7.045273212770799987 ) ) ;
#56186 = CARTESIAN_POINT ( 'NONE',  ( 83.48272809759448876, 51.94771123612188291, 15.01134753452855186 ) ) ;
#56187 = CARTESIAN_POINT ( 'NONE',  ( 175.3650005030352190, 290.1543442456702451, -6.274446597477803422 ) ) ;
#56188 = EDGE_CURVE ( 'NONE', #54274, #22323, #45426, .T. ) ;
#56189 = LINE ( 'NONE', #77526, #47794 ) ;
#56190 = ORIENTED_EDGE ( 'NONE', *, *, #35314, .F. ) ;
#56191 = CARTESIAN_POINT ( 'NONE',  ( 185.9406580756425171, 265.4572926502605128, 14.02042132963198817 ) ) ;
#56192 = CARTESIAN_POINT ( 'NONE',  ( 207.6826438088389750, 270.9301044032979462, 7.252082088659585146 ) ) ;
#56194 = CARTESIAN_POINT ( 'NONE',  ( 74.31898897143159388, 55.32162592116677047, 16.60231691840947477 ) ) ;
#56193 = CARTESIAN_POINT ( 'NONE',  ( 180.4105437470794868, 266.7128773822078074, -14.76931904508903770 ) ) ;
#56195 = CARTESIAN_POINT ( 'NONE',  ( 199.5752298111263769, 281.0719457017619902, -17.16897691529692693 ) ) ;
#56196 = CARTESIAN_POINT ( 'NONE',  ( 31.59046986846508887, 19.20801979619930222, -3.090169943749474069 ) ) ;
#56197 = CARTESIAN_POINT ( 'NONE',  ( 82.85336985908988083, 152.2760637034261890, 0.000000000000000000 ) ) ;
#56198 = CARTESIAN_POINT ( 'NONE',  ( 172.2871986639351292, 275.0669045666151646, 16.54537181790850653 ) ) ;
#56199 = CARTESIAN_POINT ( 'NONE',  ( 27.80861752939100029, 41.25950758903265836, -10.00000000000000000 ) ) ;
#56200 = CARTESIAN_POINT ( 'NONE',  ( -60.01996847620949183, 50.48172571078520576, 59.99999999999999289 ) ) ;
#56201 = CARTESIAN_POINT ( 'NONE',  ( 189.0439077586675580, 261.2591905183114704, 2.867651556594005058 ) ) ;
#56202 = CARTESIAN_POINT ( 'NONE',  ( 161.8882824960653579, 250.2482648971885340, -13.83574485983625557 ) ) ;
#56203 = CARTESIAN_POINT ( 'NONE',  ( -3.938137090306929711, 168.5333772461660828, 9.188101187500095079 ) ) ;
#56204 = B_SPLINE_CURVE_WITH_KNOTS ( 'NONE', 3,
 ( #82683, #91257, #60299, #91755, #30419, #20850, #21330, #13250, #52706, #52214, #83160, #82181, #98848, #75046, #99341, #22318 ),
 .UNSPECIFIED., .F., .F.,
 ( 4, 1, 2, 2, 2, 1, 2, 2, 4 ),
 ( 0.000000000000000000, 0.1249999999999995004, 0.1874999999999981126, 0.2499999999999967248, 0.4999999999999920619, 0.6249999999999913403, 0.6874999999999925615, 0.7499999999999938938, 1.000000000000000000 ),
 .UNSPECIFIED. ) ;
#56205 = DIRECTION ( 'NONE',  ( -0.8660254037844387076, -0.4999999999999998890, -0.000000000000000000 ) ) ;
#56206 = ORIENTED_EDGE ( 'NONE', *, *, #11368, .T. ) ;
#56207 = CARTESIAN_POINT ( 'NONE',  ( 174.9515149362974000, 255.1616608167260267, 9.153033967938712934 ) ) ;
#56208 = DIRECTION ( 'NONE',  ( 0.4330127018922168558, -0.7499999999999987788, 0.5000000000000039968 ) ) ;
#56209 = CARTESIAN_POINT ( 'NONE',  ( 82.10624035338234705, 41.84472205286013491, 5.498941269084485661 ) ) ;
#56210 = CARTESIAN_POINT ( 'NONE',  ( 19.90436448580963713, 191.4869531367911293, 4.594050593750046652 ) ) ;
#56211 = CARTESIAN_POINT ( 'NONE',  ( 32.88524308553003550, 19.39040679176984838, -6.890680421881970419E-14 ) ) ;
#56212 = CARTESIAN_POINT ( 'NONE',  ( 39.55573625059402332, 31.03677371833804699, 10.00000000000000533 ) ) ;
#56213 = CARTESIAN_POINT ( 'NONE',  ( 181.5751262769139771, 294.5022803070306736, 6.467137775781628406 ) ) ;
#56214 = CARTESIAN_POINT ( 'NONE',  ( 191.5521510896938935, 298.8689373439769952, -9.847378829740700112 ) ) ;
#56215 = CARTESIAN_POINT ( 'NONE',  ( 149.0195931398871494, 272.5374886889096047, 11.89322657225677560 ) ) ;
#56216 = CARTESIAN_POINT ( 'NONE',  ( 141.9600801517288460, 242.7677522451417929, -5.000000000000041744 ) ) ;
#56217 = CARTESIAN_POINT ( 'NONE',  ( 4.698709606056801213, 26.21091486745858390, -1.111400068045478839E-16 ) ) ;
#56218 = CARTESIAN_POINT ( 'NONE',  ( 189.6629915901594075, 298.0196469402222874, -7.906960439105454874 ) ) ;
#56219 = DIRECTION ( 'NONE',  ( -0.3177184104407422272, 0.9481851146622204407, 0.000000000000000000 ) ) ;
#56220 = EDGE_CURVE ( 'NONE', #99079, #96205, #40623, .T. ) ;
#56221 = B_SPLINE_CURVE_WITH_KNOTS ( 'NONE', 3,
 ( #35628, #66033, #58417, #89393, #66527, #50819, #81768, #97455, #28023, #58898, #17952, #79783, #72155, #99930, #36609, #44206, #60895, #7206, #83252, #13819, #76148, #44700, #14810, #51835, #98446, #75631, #29037, #20953, #90375, #6722, #21914, #43713, #82776, #99434, #45209, #29523, #59908, #90878, #30514, #21427, #6217, #52314, #30011, #91859, #52803, #98941 ),
 .UNSPECIFIED., .F., .F.,
 ( 4, 1, 2, 2, 1, 2, 2, 1, 1, 2, 2, 1, 1, 2, 2, 1, 1, 2, 2, 1, 1, 1, 2, 2, 1, 1, 1, 2, 2, 4 ),
 ( 0.000000000000000000, 0.06249999999999610034, 0.09374999999999414357, 0.1249999999999922007, 0.1874999999999881484, 0.2187499999999878986, 0.2499999999999876765, 0.3124999999999863998, 0.3437499999999856781, 0.3593749999999852340, 0.3749999999999847899, 0.4374999999999796274, 0.4687499999999789613, 0.4843749999999789613, 0.4999999999999789058, 0.5624999999999704681, 0.5937499999999658051, 0.6093749999999658051, 0.6249999999999656941, 0.6874999999999559241, 0.7187499999999531486, 0.7343749999999520384, 0.7421874999999514833, 0.7499999999999509281, 0.8124999999999613642, 0.8437499999999666933, 0.8593749999999676925, 0.8671874999999703570, 0.8749999999999729106, 1.000000000000000000 ),
 .UNSPECIFIED. ) ;
#56222 = EDGE_CURVE ( 'NONE', #61618, #5477, #62316, .T. ) ;
#56223 = VECTOR ( 'NONE', #11875, 1000.000000000000114 ) ;
#56224 = CARTESIAN_POINT ( 'NONE',  ( 77.17055463465335663, 215.3615022471902591, -10.00000000000009592 ) ) ;
#56225 = CARTESIAN_POINT ( 'NONE',  ( 69.16499752431022330, 66.81492530410388042, -9.669340448346357419 ) ) ;
#56226 = CARTESIAN_POINT ( 'NONE',  ( 159.3291946290163992, 279.0199804063916531, 10.96233109238993109 ) ) ;
#56227 = CARTESIAN_POINT ( 'NONE',  ( 203.4122341679774877, 270.0895123793504240, 6.031633626111155166 ) ) ;
#56228 = EDGE_CURVE ( 'NONE', #7719, #66239, #69044, .T. ) ;
#56229 = CARTESIAN_POINT ( 'NONE',  ( 42.23166870106845039, 201.3149278399160664, 9.188101187500093303 ) ) ;
#56230 = CARTESIAN_POINT ( 'NONE',  ( 67.24564144887035866, 66.53705660361565322, -8.596795619140232603 ) ) ;
#56231 = ADVANCED_FACE ( 'NONE', ( #93586 ), #10461, .T. ) ;
#56232 = EDGE_LOOP ( 'NONE', ( #41745, #23294, #76007, #98444 ) ) ;
#56233 = CARTESIAN_POINT ( 'NONE',  ( 77.36734184492237887, 49.76646884952617711, -14.99839566343147190 ) ) ;
#56234 = CARTESIAN_POINT ( 'NONE',  ( 150.6438662863770332, 269.7241650738195631, -14.92510732909997628 ) ) ;
#56235 = ORIENTED_EDGE ( 'NONE', *, *, #33705, .T. ) ;
#56236 = VECTOR ( 'NONE', #29734, 1000.000000000000000 ) ;
#56237 = CARTESIAN_POINT ( 'NONE',  ( 83.66574516303664666, 219.1115022471902591, 10.00000000000009592 ) ) ;
#56238 = LINE ( 'NONE', #17765, #5390 ) ;
#56239 = CARTESIAN_POINT ( 'NONE',  ( 159.7955030658553994, 278.5790326856259185, -10.80603072003405352 ) ) ;
#56240 = CARTESIAN_POINT ( 'NONE',  ( 163.7540506545266794, 282.2736363210526633, 10.04846317257458921 ) ) ;
#56241 = CARTESIAN_POINT ( 'NONE',  ( 26.72152145096863762, 27.37878583063842086, 9.188101187500006262 ) ) ;
#56242 = CARTESIAN_POINT ( 'NONE',  ( 202.2712651538608668, 280.3028871727136675, 16.13191389836473988 ) ) ;
#56243 = CARTESIAN_POINT ( 'NONE',  ( 149.6230451358742926, 271.4922791719315001, -12.72565967355361671 ) ) ;
#56244 = CARTESIAN_POINT ( 'NONE',  ( 185.8660564411877374, 268.0232567166196418, -14.37360442507078417 ) ) ;
#56245 = ORIENTED_EDGE ( 'NONE', *, *, #26269, .T. ) ;
#56246 = AXIS2_PLACEMENT_3D ( 'NONE', #45315, #89970, #20550 ) ;
#56247 = CARTESIAN_POINT ( 'NONE',  ( 6.965323710529800927, 24.99752408145590010, 5.678558825948276656 ) ) ;
#56248 = LINE ( 'NONE', #30954, #72770 ) ;
#56249 = CARTESIAN_POINT ( 'NONE',  ( 207.1610391518539984, 269.8335501706608284, 0.000000000000000000 ) ) ;
#56250 = ORIENTED_EDGE ( 'NONE', *, *, #47540, .T. ) ;
#56251 = CARTESIAN_POINT ( 'NONE',  ( 72.29163330765324247, 71.12640426941348437, -6.047334876408406501 ) ) ;
#56252 = DIRECTION ( 'NONE',  ( -0.8660254037844387076, -0.4999999999999998890, -0.000000000000000000 ) ) ;
#56253 = CARTESIAN_POINT ( 'NONE',  ( 177.3133037439327779, 256.0627534786006549, -7.214126111352222814 ) ) ;
#56254 = CARTESIAN_POINT ( 'NONE',  ( 190.7805732161387766, 300.2053494229706985, 4.237982805666590025 ) ) ;
#56255 = VERTEX_POINT ( 'NONE', #24154 ) ;
#56256 = EDGE_LOOP ( 'NONE', ( #72241, #70714, #55829, #36160 ) ) ;
#56257 = VECTOR ( 'NONE', #60572, 1000.000000000000114 ) ;
#56258 = EDGE_CURVE ( 'NONE', #33736, #213, #94588, .T. ) ;
#56260 = CARTESIAN_POINT ( 'NONE',  ( 177.5665759502285539, 275.7863988818428993, 17.69313789786682989 ) ) ;
#56259 = CARTESIAN_POINT ( 'NONE',  ( 189.6946965492525692, 274.3461288625165366, -15.70738189806986718 ) ) ;
#56261 = VERTEX_POINT ( 'NONE', #71774 ) ;
#56262 = FACE_OUTER_BOUND ( 'NONE', #91584, .T. ) ;
#56263 = DIRECTION ( 'NONE',  ( 0.4999999999999998335, -0.8660254037844389297, 0.000000000000000000 ) ) ;
#56264 = CARTESIAN_POINT ( 'NONE',  ( 72.77552873970981295, 57.60274552232836243, -16.30610872563569913 ) ) ;
#56265 = CYLINDRICAL_SURFACE ( 'NONE', #74291, 10.00000000000001066 ) ;
#56266 = CARTESIAN_POINT ( 'NONE',  ( 157.3029956111992362, 258.1902147490555421, -18.22269824972649843 ) ) ;
#56267 = CARTESIAN_POINT ( 'NONE',  ( 101.8248682511026573, 241.8464784336661637, 1.353441290958777525E-15 ) ) ;
#56268 = CARTESIAN_POINT ( 'NONE',  ( 87.85384634344086408, 209.9824982072973683, 3.021315404115420679E-15 ) ) ;
#56269 = ORIENTED_EDGE ( 'NONE', *, *, #44500, .T. ) ;
#56270 = CARTESIAN_POINT ( 'NONE',  ( 161.5510569556734026, 266.9624290277901082, 16.50852780982408063 ) ) ;
#56271 = ORIENTED_EDGE ( 'NONE', *, *, #54651, .F. ) ;
#56272 = CARTESIAN_POINT ( 'NONE',  ( 28.60632300232807879, 31.91421378149921040, 9.188101187500008038 ) ) ;
#56273 = DIRECTION ( 'NONE',  ( -0.8660254037844387076, -0.4999999999999998890, -0.000000000000000000 ) ) ;
#56274 = CARTESIAN_POINT ( 'NONE',  ( 69.68250337734514233, 70.54332952169561111, -4.835715172394301042 ) ) ;
#56275 = CARTESIAN_POINT ( 'NONE',  ( 63.26028190641562787, 198.1423013555410080, -4.594050593750043987 ) ) ;
#56276 = CARTESIAN_POINT ( 'NONE',  ( 73.78595477147815984, 68.43622263357737268, 10.95456581244436123 ) ) ;
#56277 = CARTESIAN_POINT ( 'NONE',  ( 191.2056514706806070, 299.4690922889112699, 7.290007621276087590 ) ) ;
#56278 = PLANE ( 'NONE',  #32076 ) ;
#56279 = CARTESIAN_POINT ( 'NONE',  ( -2.524136441754524451, 180.8967562850347406, 2.649461200531984646E-14 ) ) ;
#56280 = ORIENTED_EDGE ( 'NONE', *, *, #15389, .F. ) ;
#56281 = CARTESIAN_POINT ( 'NONE',  ( 78.05001017509421501, 57.38512016837487550, -16.19126229228278646 ) ) ;
#56282 = CARTESIAN_POINT ( 'NONE',  ( 178.0023654785463236, 288.9504702553427933, 11.05621428587497590 ) ) ;
#56283 = CARTESIAN_POINT ( 'NONE',  ( 78.77431960351366058, 58.56495644472522599, 16.58374741466410285 ) ) ;
#56284 = VECTOR ( 'NONE', #94777, 1000.000000000000227 ) ;
#56285 = ORIENTED_EDGE ( 'NONE', *, *, #43673, .F. ) ;
#56286 = CARTESIAN_POINT ( 'NONE',  ( 171.8293707807498265, 259.1554194294824924, -13.74145718453054954 ) ) ;
#56287 = CARTESIAN_POINT ( 'NONE',  ( 174.2793283849268562, 277.1922490460319182, -15.62918738185294742 ) ) ;
#56288 = CARTESIAN_POINT ( 'NONE',  ( 161.1150691641480535, 251.5875096731584506, -13.48836942566120101 ) ) ;
#56289 = DIRECTION ( 'NONE',  ( 1.000000000000000000, 0.000000000000000000, 0.000000000000000000 ) ) ;
#56290 = CARTESIAN_POINT ( 'NONE',  ( 50.57404612423096069, 211.5530062829863027, -4.648177544792955347E-16 ) ) ;
#56292 = EDGE_CURVE ( 'NONE', #89585, #17687, #25667, .T. ) ;
#56291 = AXIS2_PLACEMENT_3D ( 'NONE', #7179, #53766, #45183 ) ;
#56293 = CARTESIAN_POINT ( 'NONE',  ( 180.8203030686837280, 271.2954033567903025, 17.04059064758568454 ) ) ;
#56294 = FACE_OUTER_BOUND ( 'NONE', #24130, .T. ) ;
#56295 = CARTESIAN_POINT ( 'NONE',  ( 75.94688732371197659, 65.57317746828351801, 13.88815714291336967 ) ) ;
#56296 = CARTESIAN_POINT ( 'NONE',  ( 153.8622324351665043, 264.6225750775929555, -16.50275939780754086 ) ) ;
#56297 = CARTESIAN_POINT ( 'NONE',  ( 176.5738172124948164, 284.4749987453067774, 14.65120015815750421 ) ) ;
#56298 = VECTOR ( 'NONE', #49450, 1000.000000000000000 ) ;
#56299 = CARTESIAN_POINT ( 'NONE',  ( 110.1064097226738312, 240.5024278399161233, 9.188101187500095079 ) ) ;
#56300 = ORIENTED_EDGE ( 'NONE', *, *, #77679, .T. ) ;
#56301 = CARTESIAN_POINT ( 'NONE',  ( 147.1259762202154207, 275.8173294038533641, -0.6716460511724978710 ) ) ;
#56302 = LINE ( 'NONE', #64923, #80537 ) ;
#56303 = CARTESIAN_POINT ( 'NONE',  ( 202.9547455376043672, 279.1190644220934018, -15.19669173352461478 ) ) ;
#56304 = CARTESIAN_POINT ( 'NONE',  ( 204.2457645315488719, 276.8829539310449945, 14.53406579917280261 ) ) ;
#56305 = CARTESIAN_POINT ( 'NONE',  ( 83.78311978599397492, 51.75050911116664309, -14.85521894841905599 ) ) ;
#56306 = CARTESIAN_POINT ( 'NONE',  ( 175.0760097641222330, 252.5203264472857256, 5.202907413956480376 ) ) ;
#56307 = EDGE_LOOP ( 'NONE', ( #48818, #82493, #35756, #74745 ) ) ;
#56308 = CARTESIAN_POINT ( 'NONE',  ( 80.65713072601933220, 57.38499450659126921, -16.23539640514130866 ) ) ;
#56309 = CARTESIAN_POINT ( 'NONE',  ( 154.7226985476829384, 273.3457454102759812, -13.10063029118530586 ) ) ;
#56311 = CARTESIAN_POINT ( 'NONE',  ( 72.06633338339661066, 71.38138388103391208, 5.132520212388754111 ) ) ;
#56310 = CARTESIAN_POINT ( 'NONE',  ( 72.97386446981147401, 70.68132344495337804, 8.316175787459499702 ) ) ;
#56312 = CARTESIAN_POINT ( 'NONE',  ( 164.5696622524448287, 245.6039789247527096, -0.9250471598561700315 ) ) ;
#56313 = CARTESIAN_POINT ( 'NONE',  ( 144.0982539169780523, 247.8768266524160140, 9.188101187500096856 ) ) ;
#56314 = CARTESIAN_POINT ( 'NONE',  ( 198.6363782946250183, 286.5986958926748116, -18.50260615857378355 ) ) ;
#56315 = AXIS2_PLACEMENT_3D ( 'NONE', #13231, #75028, #47803 ) ;
#56316 = B_SPLINE_CURVE_WITH_KNOTS ( 'NONE', 3,
 ( #43768, #53367, #21973, #59960 ),
 .UNSPECIFIED., .F., .F.,
 ( 4, 4 ),
 ( 0.01375087555092867168, 0.01505699899481918562 ),
 .UNSPECIFIED. ) ;
#56317 = CARTESIAN_POINT ( 'NONE',  ( 190.0398248856338057, 298.8169614316505545, -8.166243001185458539 ) ) ;
#56318 = DIRECTION ( 'NONE',  ( -0.5346708562974005208, -0.8450603975019800318, 0.000000000000000000 ) ) ;
#56319 = CARTESIAN_POINT ( 'NONE',  ( 63.28708487846012076, 207.3458772461660544, 9.188101187500095079 ) ) ;
#56320 = CARTESIAN_POINT ( 'NONE',  ( 164.9779129355220562, 244.8968679994381148, -1.771286574179712803 ) ) ;
#56321 = CARTESIAN_POINT ( 'NONE',  ( 157.3198323354746435, 258.1610526871778006, -16.77630483474704093 ) ) ;
#56322 = CARTESIAN_POINT ( 'NONE',  ( 87.97560163977048830, 44.53565211440820804, -3.995394561512739973 ) ) ;
#56323 = FILL_AREA_STYLE_COLOUR ( '', #95131 ) ;
#56324 = CARTESIAN_POINT ( 'NONE',  ( 174.6693944358695774, 261.9625217202849399, 14.25614487736958047 ) ) ;
#56325 = CARTESIAN_POINT ( 'NONE',  ( 170.8865616681041786, 262.8912071418242817, 16.88624067591380040 ) ) ;
#56326 = CARTESIAN_POINT ( 'NONE',  ( 178.3571982967953602, 292.6181790745828835, -7.174879954037646002 ) ) ;
#56327 = DIRECTION ( 'NONE',  ( 0.000000000000000000, -0.000000000000000000, 1.000000000000000000 ) ) ;
#56328 = CARTESIAN_POINT ( 'NONE',  ( 178.3225333605271317, 261.2550961346064469, 13.20358700637163096 ) ) ;
#56329 = VECTOR ( 'NONE', #19368, 1000.000000000000000 ) ;
#56330 = CARTESIAN_POINT ( 'NONE',  ( 119.9486011388742384, 253.3927522451419350, 2.944929066748280225E-16 ) ) ;
#56331 = CARTESIAN_POINT ( 'NONE',  ( 78.96647079090445231, 52.43242654007526227, -15.54601558169038356 ) ) ;
#56332 = ORIENTED_EDGE ( 'NONE', *, *, #56105, .T. ) ;
#56333 = CARTESIAN_POINT ( 'NONE',  ( 148.1634546024981205, 274.0203641339852538, 9.324875965062235039 ) ) ;
#56334 = CARTESIAN_POINT ( 'NONE',  ( 87.77191196787447325, 44.75263600343390635, 5.004501849949501313 ) ) ;
#56335 = CARTESIAN_POINT ( 'NONE',  ( 41.52819660837609916, 194.7833772461660544, -9.188101187500095079 ) ) ;
#56336 = CARTESIAN_POINT ( 'NONE',  ( 20.52402715336229377, 23.80066082961421969, 10.00000000000000533 ) ) ;
#56337 = CARTESIAN_POINT ( 'NONE',  ( 88.17148522932362198, 43.68169873549415883, 0.1729226289268755989 ) ) ;
#56338 = CARTESIAN_POINT ( 'NONE',  ( 82.65769392073423205, 206.9824982072973683, 3.021315404115420679E-15 ) ) ;
#56339 = CARTESIAN_POINT ( 'NONE',  ( 147.4811722709131914, 275.2021117973970377, 3.890385073228495916 ) ) ;
#56340 = CARTESIAN_POINT ( 'NONE',  ( 73.99515186944866230, 54.97541550364575613, -16.60506967706033521 ) ) ;
#56342 = CARTESIAN_POINT ( 'NONE',  ( 67.12105150802354103, 202.8927522451418213, 10.00000000000009592 ) ) ;
#56341 = CARTESIAN_POINT ( 'NONE',  ( 27.76992210170819675, 43.29297894285233639, 10.00000000000000000 ) ) ;
#56343 = CARTESIAN_POINT ( 'NONE',  ( 163.0887663364496518, 256.3074304275255599, -16.05814244895578469 ) ) ;
#56344 = CARTESIAN_POINT ( 'NONE',  ( -2.070769811622824363, 179.6115022471903160, -5.000000000000047962 ) ) ;
#56345 = CYLINDRICAL_SURFACE ( 'NONE', #51686, 70.00000000000002842 ) ;
#56347 = ORIENTED_EDGE ( 'NONE', *, *, #737, .F. ) ;
#56346 = EDGE_CURVE ( 'NONE', #27863, #690, #11597, .T. ) ;
#56348 = ADVANCED_FACE ( 'NONE', ( #58535 ), #27667, .T. ) ;
#56349 = CARTESIAN_POINT ( 'NONE',  ( 33.00325904164698443, 189.8615022471902591, -10.00000000000009592 ) ) ;
#56350 = CARTESIAN_POINT ( 'NONE',  ( 184.6123843791924912, 294.3808565314488419, 10.01802650564912867 ) ) ;
#56351 = CARTESIAN_POINT ( 'NONE',  ( 202.4900219881211854, 279.9239892212719383, 15.63116161057562259 ) ) ;
#56352 = VECTOR ( 'NONE', #58411, 1000.000000000000114 ) ;
#56353 = CARTESIAN_POINT ( 'NONE',  ( 7.428446334363822956, 175.0958772461660544, -9.188101187500095079 ) ) ;
#56354 = CARTESIAN_POINT ( 'NONE',  ( 37.59133656659163591, 37.10171378149920685, 9.188101187500008038 ) ) ;
#56356 = CARTESIAN_POINT ( 'NONE',  ( 170.4241003537304096, 263.6404983464951215, 15.81189019553032971 ) ) ;
#56355 = DIRECTION ( 'NONE',  ( 0.000000000000000000, -1.000000000000000000, 0.000000000000000000 ) ) ;
#56357 = EDGE_CURVE ( 'NONE', #90465, #28481, #37142, .T. ) ;
#56358 = CARTESIAN_POINT ( 'NONE',  ( 32.40786657299730678, 179.5177522451417929, 5.000000000000051514 ) ) ;
#56359 = CARTESIAN_POINT ( 'NONE',  ( 26.18025557360336464, 27.06628583063842797, -9.188101187500006262 ) ) ;
#56360 = CARTESIAN_POINT ( 'NONE',  ( 23.96727898247415212, 22.03677371833801857, 10.00000000000000533 ) ) ;
#56362 = AXIS2_PLACEMENT_3D ( 'NONE', #75970, #60212, #98258 ) ;
#56361 = CARTESIAN_POINT ( 'NONE',  ( 87.99973427719299934, 43.78392399561506210, 2.406698522940700080 ) ) ;
#56363 = CARTESIAN_POINT ( 'NONE',  ( 66.34034349336292280, 68.67733634918475616, 2.360395268154211301 ) ) ;
#56364 = ORIENTED_EDGE ( 'NONE', *, *, #55946, .T. ) ;
#56365 = CARTESIAN_POINT ( 'NONE',  ( 76.32488315910845245, 203.3262482093458061, 3.021315404115420679E-15 ) ) ;
#56366 = LINE ( 'NONE', #47267, #87631 ) ;
#56367 =( LENGTH_UNIT ( ) NAMED_UNIT ( * ) SI_UNIT ( .MILLI., .METRE. ) );
#56368 = CIRCLE ( 'NONE', #54763, 60.00000000000001421 ) ;
#56369 = CARTESIAN_POINT ( 'NONE',  ( 15.84867609773810138, 11.01110640527290840, 2.839279412974134775 ) ) ;
#56370 = CARTESIAN_POINT ( 'NONE',  ( 153.3589871089347128, 277.7324385553121147, -5.220324751481857817 ) ) ;
#56371 = CARTESIAN_POINT ( 'NONE',  ( 21.91745948943429312, 13.44966523072494269, -2.296566073217252530E-15 ) ) ;
#56372 = DIRECTION ( 'NONE',  ( 0.4999999999999988343, -0.8660254037844393737, 0.000000000000000000 ) ) ;
#56373 = CARTESIAN_POINT ( 'NONE',  ( 84.74798064930895691, 49.97902072749974423, -13.66263633214625806 ) ) ;
#56374 = CARTESIAN_POINT ( 'NONE',  ( 206.7893622945242385, 272.4773133715531230, -10.52881283832460291 ) ) ;
#56375 = ORIENTED_EDGE ( 'NONE', *, *, #37709, .F. ) ;
#56376 = CARTESIAN_POINT ( 'NONE',  ( 152.9262073036446168, 265.7710344717137900, 16.19159804214501008 ) ) ;
#56377 = CARTESIAN_POINT ( 'NONE',  ( 165.0437781805843258, 244.7827860485373606, -2.050141714668513693 ) ) ;
#56378 = CARTESIAN_POINT ( 'NONE',  ( 99.25420243115655694, 228.1115022471902307, 10.00000000000009592 ) ) ;
#56379 = CARTESIAN_POINT ( 'NONE',  ( 87.47635513963552967, 45.03054629282574695, 6.933452704933705135 ) ) ;
#56380 = CARTESIAN_POINT ( 'NONE',  ( 194.2669918475045279, 294.1666952169902629, 14.00965265288584050 ) ) ;
#56381 = EDGE_LOOP ( 'NONE', ( #93181, #66278, #76522, #6682 ) ) ;
#56382 = AXIS2_PLACEMENT_3D ( 'NONE', #20803, #20298, #95847 ) ;
#56383 =( BOUNDED_CURVE ( )  B_SPLINE_CURVE ( 2, ( #49808, #3726, #27019, #71635, #2230, #94950, #25514, #56404, #87398, #17927, #48825, #79758, #41191 ),
 .UNSPECIFIED., .F., .T. ) 
 B_SPLINE_CURVE_WITH_KNOTS ( ( 3, 2, 2, 2, 2, 2, 3 ),
 ( 0.8875000000000000666, 0.8900000000000000133, 0.8950000000000000178, 0.9000000000000000222, 0.9050000000000000266, 0.9100000000000000311, 0.9125000000000000888 ),
 .UNSPECIFIED. ) 
 CURVE ( )  GEOMETRIC_REPRESENTATION_ITEM ( )  RATIONAL_B_SPLINE_CURVE ( ( 0.9755282581475767101, 0.9755282581475772652, 1.000000000000000000, 0.9510565162951535312, 1.000000000000000000, 0.9510565162951535312, 1.000000000000000000, 0.9510565162951535312, 1.000000000000000000, 0.9510565162951535312, 1.000000000000000000, 0.9755282581475761550, 0.9755282581475767101 ) ) 
 REPRESENTATION_ITEM ( '' )  );
#56384 = ORIENTED_EDGE ( 'NONE', *, *, #30739, .T. ) ;
#56385 = CARTESIAN_POINT ( 'NONE',  ( 159.1645459798114359, 278.1651338649389800, -9.804895797930408108 ) ) ;
#56386 = CARTESIAN_POINT ( 'NONE',  ( 86.47877272607206578, 47.40146553843635502, 10.34156286556493853 ) ) ;
#56387 = VERTEX_POINT ( 'NONE', #96601 ) ;
#56388 = CARTESIAN_POINT ( 'NONE',  ( 76.84822201109516016, 53.05882888382841855, 15.89418035136032969 ) ) ;
#56389 = CARTESIAN_POINT ( 'NONE',  ( 205.8099205723994203, 269.1131406545866298, -1.356034389334280776 ) ) ;
#56390 = VERTEX_POINT ( 'NONE', #82410 ) ;
#56391 = CARTESIAN_POINT ( 'NONE',  ( 78.39917873861809028, 61.30051739111549836, -15.87534687166327885 ) ) ;
#56392 = CARTESIAN_POINT ( 'NONE',  ( -27.52599651137551007, 146.7012482093458914, -1.732050807568756179 ) ) ;
#56393 = B_SPLINE_CURVE_WITH_KNOTS ( 'NONE', 3,
 ( #16584, #77399, #1898, #15566, #9501, #31278, #69285, #56061, #39362, #8985 ),
 .UNSPECIFIED., .F., .F.,
 ( 4, 2, 2, 2, 4 ),
 ( 0.000000000000000000, 0.2500000000000000000, 0.5000000000000000000, 0.7500000000000000000, 1.000000000000000000 ),
 .UNSPECIFIED. ) ;
#56394 = AXIS2_PLACEMENT_3D ( 'NONE', #24819, #85689, #87703 ) ;
#56395 = CARTESIAN_POINT ( 'NONE',  ( 177.5865089022509551, 268.7852845103913069, 17.37969943402860906 ) ) ;
#56396 = ORIENTED_EDGE ( 'NONE', *, *, #55087, .T. ) ;
#56397 = DIRECTION ( 'NONE',  ( 0.7694697644498922351, -0.6386832404231594928, 0.000000000000000000 ) ) ;
#56398 = CARTESIAN_POINT ( 'NONE',  ( 166.1221895601162544, 273.9771594711654643, -16.55413630177630324 ) ) ;
#56399 = CARTESIAN_POINT ( 'NONE',  ( 190.8443993347725325, 300.0947993426467519, 8.522468760355437212 ) ) ;
#56400 = CARTESIAN_POINT ( 'NONE',  ( 176.6379055597627428, 265.0600181157752218, 16.52625651101184445 ) ) ;
#56401 = PRODUCT_DEFINITION_SHAPE ( 'NONE', 'NONE',  #100296 ) ;
#56402 = ORIENTED_EDGE ( 'NONE', *, *, #13818, .T. ) ;
#56403 = CARTESIAN_POINT ( 'NONE',  ( 171.0309627268963482, 255.8151653478954017, -11.60038586255653570 ) ) ;
#56404 = CARTESIAN_POINT ( 'NONE',  ( 36.03590635313023682, 36.50829794293883168, -10.00000000000000355 ) ) ;
#56405 = ORIENTED_EDGE ( 'NONE', *, *, #51118, .F. ) ;
#56406 = VERTEX_POINT ( 'NONE', #2882 ) ;
#56407 = CYLINDRICAL_SURFACE ( 'NONE', #74194, 17.82106496071139645 ) ;
#56408 = ORIENTED_EDGE ( 'NONE', *, *, #67141, .T. ) ;
#56409 = DIRECTION ( 'NONE',  ( 0.8660254037844390407, 0.4999999999999993339, 0.000000000000000000 ) ) ;
#56410 = VERTEX_POINT ( 'NONE', #20067 ) ;
#56411 = PLANE ( 'NONE',  #78770 ) ;
#56412 = CARTESIAN_POINT ( 'NONE',  ( 194.0457541550190967, 294.5498901409245036, 13.79567330127564517 ) ) ;
#56413 = CARTESIAN_POINT ( 'NONE',  ( 179.8658285908990138, 290.6180032362764223, -9.493696763719416509 ) ) ;
#56414 = CARTESIAN_POINT ( 'NONE',  ( 70.84700895556564149, 68.24011015210355424, 9.176700790939991137 ) ) ;
#56415 = CARTESIAN_POINT ( 'NONE',  ( 193.7068637079588598, 294.3397739674867921, 13.92549557170472774 ) ) ;
#56416 = CARTESIAN_POINT ( 'NONE',  ( 82.51292938203759775, 53.28734884524191528, -15.32281082862661670 ) ) ;
#56417 = CARTESIAN_POINT ( 'NONE',  ( 158.8791574486372440, 255.4602223656619628, -17.57574691297732272 ) ) ;
#56418 = VERTEX_POINT ( 'NONE', #65644 ) ;
#56419 = DIRECTION ( 'NONE',  ( 0.4330127018922146354, 0.2500000000000017208, -0.8660254037844404840 ) ) ;
#56420 = CARTESIAN_POINT ( 'NONE',  ( 18.21401815691482895, 25.91421378149918198, 9.188101187500008038 ) ) ;
#56421 = EDGE_CURVE ( 'NONE', #35964, #79592, #35793, .T. ) ;
#56422 = CARTESIAN_POINT ( 'NONE',  ( 164.8537203408104972, 245.1119758834023230, 2.926011033004258355 ) ) ;
#56423 = CARTESIAN_POINT ( 'NONE',  ( 191.4930805452865741, 298.1933573230298862, -9.154694743737874063 ) ) ;
#56425 = EDGE_LOOP ( 'NONE', ( #54383, #10954, #13132, #21040 ) ) ;
#56424 = CARTESIAN_POINT ( 'NONE',  ( 75.15191903148871688, 52.97183600646508239, -16.48001256418180915 ) ) ;
#56426 = ORIENTED_EDGE ( 'NONE', *, *, #18384, .F. ) ;
#56427 = FACE_OUTER_BOUND ( 'NONE', #38836, .T. ) ;
#56428 = CARTESIAN_POINT ( 'NONE',  ( 169.9170831025614632, 258.3961534647858684, -13.99170300441150161 ) ) ;
#56429 = CARTESIAN_POINT ( 'NONE',  ( 186.0715527847238207, 298.7753624933060337, 1.084710433360843940 ) ) ;
#56430 = CARTESIAN_POINT ( 'NONE',  ( -22.42236680055709641, 157.8615022471902591, 0.000000000000000000 ) ) ;
#56431 = EDGE_CURVE ( 'NONE', #77218, #16945, #1091, .T. ) ;
#56432 = CARTESIAN_POINT ( 'NONE',  ( 200.8432122835317841, 282.7763473000181307, 17.15137370990203891 ) ) ;
#56433 = CARTESIAN_POINT ( 'NONE',  ( 191.4738032422262677, 260.7793432447242594, -0.2951778641931921410 ) ) ;
#56434 = ORIENTED_EDGE ( 'NONE', *, *, #48838, .F. ) ;
#56435 = CARTESIAN_POINT ( 'NONE',  ( -51.75017079496728201, 30.85748650210272359, 177.5919119679930134 ) ) ;
#56436 = CARTESIAN_POINT ( 'NONE',  ( 5.452216952852307230, 26.08080186712590631, -3.090169943749475845 ) ) ;
#56437 = CARTESIAN_POINT ( 'NONE',  ( 131.0625938207745662, 253.1427522451419350, 10.00000000000009415 ) ) ;
#56439 = ADVANCED_FACE ( 'NONE', ( #89033 ), #19582, .F. ) ;
#56438 = CARTESIAN_POINT ( 'NONE',  ( 189.4313974406659327, 277.5226620091338532, 17.67960062696096912 ) ) ;
#56440 = CARTESIAN_POINT ( 'NONE',  ( 22.95375591501717594, 177.3927522451418497, 10.00000000000009592 ) ) ;
#56441 = CARTESIAN_POINT ( 'NONE',  ( 88.99704050542813150, 228.3149278399160949, 9.188101187500093303 ) ) ;
#56442 = CARTESIAN_POINT ( 'NONE',  ( 82.23777015025109449, 40.85740305880240442, -1.202640854400347736 ) ) ;
#56443 = VECTOR ( 'NONE', #1789, 1000.000000000000114 ) ;
#56444 = CARTESIAN_POINT ( 'NONE',  ( 207.6470076888861342, 270.9918279736407385, 2.882721586646819212 ) ) ;
#56445 = AXIS2_PLACEMENT_3D ( 'NONE', #35004, #3152, #27429 ) ;
#56446 = CARTESIAN_POINT ( 'NONE',  ( 20.93329029645117245, 173.7048013555409796, 4.594050593750051981 ) ) ;
#56447 = CARTESIAN_POINT ( 'NONE',  ( 200.1662314894802819, 283.9489124310637180, 17.19420058542677054 ) ) ;
#56448 = ORIENTED_EDGE ( 'NONE', *, *, #91408, .F. ) ;
#56449 = AXIS2_PLACEMENT_3D ( 'NONE', #22561, #75788, #29177 ) ;
#56451 = EDGE_LOOP ( 'NONE', ( #16447, #4359, #30233, #1120 ) ) ;
#56450 = UNCERTAINTY_MEASURE_WITH_UNIT (LENGTH_MEASURE( 1.000000000000000082E-05 ), #72094, 'distance_accuracy_value', 'NONE');
#56452 = CARTESIAN_POINT ( 'NONE',  ( 198.3425264013990272, 266.1585612424889291, -2.872493559038742372 ) ) ;
#56453 = CARTESIAN_POINT ( 'NONE',  ( 80.74610282667754291, 46.90596778374671061, -12.61250437584052264 ) ) ;
#56454 = DIRECTION ( 'NONE',  ( 0.3297783986044514615, 0.8484238185761762141, 0.4140328874455545538 ) ) ;
#56455 = CARTESIAN_POINT ( 'NONE',  ( 194.8742882536625984, 264.7950142703134020, -4.379131112317717012 ) ) ;
#56456 = DIRECTION ( 'NONE',  ( -0.9923183454821322691, -0.1237105541964931832, 0.000000000000000000 ) ) ;
#56457 = CIRCLE ( 'NONE', #83986, 50.00000000000000711 ) ;
#56458 = CARTESIAN_POINT ( 'NONE',  ( 69.13686587061594935, 64.31895405193962745, 11.99662287724232357 ) ) ;
#56459 = CARTESIAN_POINT ( 'NONE',  ( 74.41721759878494424, 68.37665257406605690, -11.33153079197290580 ) ) ;
#56460 = CARTESIAN_POINT ( 'NONE',  ( 32.43492986863949312, 189.5333772461660544, 9.188101187500095079 ) ) ;
#56461 = CARTESIAN_POINT ( 'NONE',  ( 88.62734903533713293, 208.6427522451417644, 1.119607411625061291E-15 ) ) ;
#56462 = ORIENTED_EDGE ( 'NONE', *, *, #41371, .F. ) ;
#56463 = CARTESIAN_POINT ( 'NONE',  ( 81.74963128441575577, 42.78295644149261534, 7.706177857118651886 ) ) ;
#56464 = CARTESIAN_POINT ( 'NONE',  ( 179.0311786453646334, 258.6304024054584261, -10.01495405547345641 ) ) ;
#56465 = AXIS2_PLACEMENT_3D ( 'NONE', #42255, #87458, #71700 ) ;
#56466 = CARTESIAN_POINT ( 'NONE',  ( -3.586574591843265658, 177.9244531367911577, -4.594050593750046652 ) ) ;
#56467 = B_SPLINE_CURVE_WITH_KNOTS ( 'NONE', 3,
 ( #67978, #53271, #14277, #45169 ),
 .UNSPECIFIED., .F., .F.,
 ( 4, 4 ),
 ( 2.465251413651021934E-15, 0.003756095204294760022 ),
 .UNSPECIFIED. ) ;
#56468 = CARTESIAN_POINT ( 'NONE',  ( 68.91022223095966126, 64.71151235103670274, -12.22836756602027464 ) ) ;
#56469 = CARTESIAN_POINT ( 'NONE',  ( 161.5083988044524119, 250.9062427520286178, -14.53522982831775856 ) ) ;
#56470 = CARTESIAN_POINT ( 'NONE',  ( 187.8161210723351644, 283.3479265774896589, 16.26191486346292692 ) ) ;
#56471 = CARTESIAN_POINT ( 'NONE',  ( 194.8067605455144076, 293.2317884077015151, -16.00245909155922774 ) ) ;
#56472 = EDGE_CURVE ( 'NONE', #99390, #79855, #70647, .T. ) ;
#56473 = CARTESIAN_POINT ( 'NONE',  ( 70.21263088009048658, 68.31033697602117627, -9.405330560664618034 ) ) ;
#56474 = CARTESIAN_POINT ( 'NONE',  ( 164.4864504671816690, 245.7481059646165704, 6.337356894698421783 ) ) ;
#56475 = CARTESIAN_POINT ( 'NONE',  ( 146.6834825911944620, 276.5837508513432681, 0.6716460511724984261 ) ) ;
#56476 = CARTESIAN_POINT ( 'NONE',  ( 207.0548180518391916, 272.0175305127218053, 7.721676452263806389 ) ) ;
#56477 = ORIENTED_EDGE ( 'NONE', *, *, #99337, .T. ) ;
#56478 = CARTESIAN_POINT ( 'NONE',  ( 164.1146561143383167, 246.3920726737087534, -7.362905700427413436 ) ) ;
#56479 = CARTESIAN_POINT ( 'NONE',  ( 161.4628698183636857, 251.3853568467309572, -13.03279659859947870 ) ) ;
#56480 = CARTESIAN_POINT ( 'NONE',  ( 105.9656389868882513, 241.1744531367911577, 4.594050593750047540 ) ) ;
#56481 = CARTESIAN_POINT ( 'NONE',  ( 20.65814732634927609, 20.43085787977763346, -9.188101187500008038 ) ) ;
#56482 = CARTESIAN_POINT ( 'NONE',  ( 75.06873900396388422, 67.14982071245070472, 12.61085099019435951 ) ) ;
#56483 = ADVANCED_FACE ( 'NONE', ( #88020 ), #57819, .F. ) ;
#56484 = CARTESIAN_POINT ( 'NONE',  ( 156.6812872898450735, 261.2670451491295012, 0.000000000000000000 ) ) ;
#56486 = CARTESIAN_POINT ( 'NONE',  ( 185.5233448779797243, 288.1480361044887673, 15.07821780549886803 ) ) ;
#56485 = CARTESIAN_POINT ( 'NONE',  ( 195.6986305151803549, 291.6870243064952888, 16.84182339398051909 ) ) ;
#56487 = CARTESIAN_POINT ( 'NONE',  ( 150.7975480795134615, 269.4579803999092178, -13.77803079712401590 ) ) ;
#56488 = ORIENTED_EDGE ( 'NONE', *, *, #33829, .T. ) ;
#56489 = EDGE_CURVE ( 'NONE', #23455, #34725, #49601, .T. ) ;
#56490 = CARTESIAN_POINT ( 'NONE',  ( 189.8073911343818452, 261.0592632349233781, -4.572445870894544129 ) ) ;
#56491 = CARTESIAN_POINT ( 'NONE',  ( 149.3141802193904368, 272.0272488999566463, -11.40332369054239336 ) ) ;
#56492 = DIRECTION ( 'NONE',  ( 0.000000000000000000, 0.000000000000000000, 1.000000000000000000 ) ) ;
#56493 = CARTESIAN_POINT ( 'NONE',  ( 173.1255070585075941, 289.7719922078085233, -1.455481432696650979 ) ) ;
#56494 = CARTESIAN_POINT ( 'NONE',  ( 81.72556729995484659, 55.26675154459383066, -15.91896077131915455 ) ) ;
#56495 = ORIENTED_EDGE ( 'NONE', *, *, #73975, .F. ) ;
#56496 = CARTESIAN_POINT ( 'NONE',  ( 189.0598825607623326, 265.6785374324029476, 10.85450195960190634 ) ) ;
#56497 = CARTESIAN_POINT ( 'NONE',  ( 175.0906617674605741, 279.3930328189767920, 16.49259839202913724 ) ) ;
#56498 = CARTESIAN_POINT ( 'NONE',  ( 165.4679322623151734, 269.7639896636108006, -16.28713546330200046 ) ) ;
#56499 = CARTESIAN_POINT ( 'NONE',  ( 200.2206280980474276, 272.4473840335176078, 12.62891601330385427 ) ) ;
#56500 = CARTESIAN_POINT ( 'NONE',  ( 83.80743799779062897, 52.10092053580531513, -14.60766023568177197 ) ) ;
#56501 = CARTESIAN_POINT ( 'NONE',  ( 72.32516777325903945, 71.91622842696713747, -5.210293257461823480 ) ) ;
#56502 = CARTESIAN_POINT ( 'NONE',  ( 153.3616370783189211, 265.0168479788495688, 17.48287904751960653 ) ) ;
#56503 = ORIENTED_EDGE ( 'NONE', *, *, #40702, .F. ) ;
#56504 = CARTESIAN_POINT ( 'NONE',  ( -6.887318171848119341, 24.23892674679880699, 10.00000000000000000 ) ) ;
#56505 = CARTESIAN_POINT ( 'NONE',  ( 32.94608582406294772, 39.99752408145594984, 5.678558825948277544 ) ) ;
#56506 = CARTESIAN_POINT ( 'NONE',  ( 192.0496571061401028, 288.1032038373080582, -15.86509381273373442 ) ) ;
#56507 = ORIENTED_EDGE ( 'NONE', *, *, #89366, .F. ) ;
#56508 = CARTESIAN_POINT ( 'NONE',  ( 77.75702407734982557, 61.66006977308100545, 16.07490810555906791 ) ) ;
#56509 = CARTESIAN_POINT ( 'NONE',  ( 148.1974503712686158, 273.9614817352322120, -7.884397846570731616 ) ) ;
#56510 = DIRECTION ( 'NONE',  ( 0.000000000000000000, 0.000000000000000000, 1.000000000000000000 ) ) ;
#56511 = VERTEX_POINT ( 'NONE', #51949 ) ;
#56512 = AXIS2_PLACEMENT_3D ( 'NONE', #17889, #54864, #48788 ) ;
#56513 = CARTESIAN_POINT ( 'NONE',  ( 78.99750231315303495, 60.09927444898351467, 16.11767558604333317 ) ) ;
#56514 = CYLINDRICAL_SURFACE ( 'NONE', #36248, 17.82106496071139645 ) ;
#56515 = CARTESIAN_POINT ( 'NONE',  ( 88.39405946958876825, 44.08409158760228053, -2.802556091636618341 ) ) ;
#56516 = VECTOR ( 'NONE', #99573, 1000.000000000000000 ) ;
#56517 = CARTESIAN_POINT ( 'NONE',  ( 77.90281930814079203, 52.05526166391488374, -15.59995652318183978 ) ) ;
#56518 = CARTESIAN_POINT ( 'NONE',  ( 80.55420448732139960, 44.52191585150384157, 11.40672976540375672 ) ) ;
#56519 = CARTESIAN_POINT ( 'NONE',  ( 183.8043731368310603, 268.5938253857621589, 16.29461355553033997 ) ) ;
#56520 = CARTESIAN_POINT ( 'NONE',  ( 203.5258219653775313, 278.1299310341851765, -16.21052911601769608 ) ) ;
#56521 = ORIENTED_EDGE ( 'NONE', *, *, #25154, .F. ) ;
#56522 = ORIENTED_EDGE ( 'NONE', *, *, #68695, .T. ) ;
#56523 = CARTESIAN_POINT ( 'NONE',  ( 178.3597279735877805, 261.0516804887051308, 12.18819909079894082 ) ) ;
#56524 = ORIENTED_EDGE ( 'NONE', *, *, #54186, .F. ) ;
#56525 = CARTESIAN_POINT ( 'NONE',  ( 77.29488782935133884, 49.16221438579500358, -14.80191796116666048 ) ) ;
#56526 = ORIENTED_EDGE ( 'NONE', *, *, #49871, .T. ) ;
#56527 = CARTESIAN_POINT ( 'NONE',  ( 74.51129208461142639, 56.54966615295543164, 16.08098109482861204 ) ) ;
#56529 = CARTESIAN_POINT ( 'NONE',  ( 203.5258219653775313, 278.1299310341851765, -16.21052911601769608 ) ) ;
#56528 = AXIS2_PLACEMENT_3D ( 'NONE', #94186, #54622, #449 ) ;
#56530 = VERTEX_POINT ( 'NONE', #82889 ) ;
#56531 = CARTESIAN_POINT ( 'NONE',  ( 183.2409096537462290, 280.5924353467958667, -16.12459997820720758 ) ) ;
#56532 = CARTESIAN_POINT ( 'NONE',  ( 147.2639185929470216, 275.5784062057657025, -6.046059379523592625 ) ) ;
#56533 = CARTESIAN_POINT ( 'NONE',  ( 158.6745544753717354, 275.0482988461347986, -12.54501861896559056 ) ) ;
#56534 = CARTESIAN_POINT ( 'NONE',  ( -71.07364842061382149, 47.42355933771584375, 10.00000000000000000 ) ) ;
#56535 = CARTESIAN_POINT ( 'NONE',  ( 200.9812045408918380, 282.5373376992193926, -16.61165062382494284 ) ) ;
#56536 = LINE ( 'NONE', #18057, #58234 ) ;
#56537 = CARTESIAN_POINT ( 'NONE',  ( 157.3303612352329424, 280.6659801480934107, 2.084183637465919059 ) ) ;
#56538 = CARTESIAN_POINT ( 'NONE',  ( 129.0235653626489238, 254.4869531367911577, 4.594050593750046652 ) ) ;
#56539 = CARTESIAN_POINT ( 'NONE',  ( 70.98683038387876820, 61.11472152276905945, -14.49225651734631271 ) ) ;
#56540 = CARTESIAN_POINT ( 'NONE',  ( 3.154811933878272523, 22.79752408145590081, -5.678558825948271327 ) ) ;
#56541 = ORIENTED_EDGE ( 'NONE', *, *, #88562, .F. ) ;
#56542=STYLED_ITEM('',(#100338),#10898);
#56543 = EDGE_CURVE ( 'NONE', #68198, #49338, #21073, .T. ) ;
#56545 = VERTEX_POINT ( 'NONE', #22033 ) ;
#56544 = CARTESIAN_POINT ( 'NONE',  ( 153.9946444333862416, 274.9169454665982357, 12.01620693575389964 ) ) ;
#56546 = CARTESIAN_POINT ( 'NONE',  ( 200.9975768615754248, 274.6372745081091580, 13.39944341616547163 ) ) ;
#56547 = CARTESIAN_POINT ( 'NONE',  ( 178.1271951506071503, 254.3491337373919805, 1.338458689122108636 ) ) ;
#56548 = EDGE_CURVE ( 'NONE', #47191, #26620, #92800, .T. ) ;
#56549 = CARTESIAN_POINT ( 'NONE',  ( 173.2306762196021452, 290.4478550908166312, -4.991672751549263154 ) ) ;
#56550 = CARTESIAN_POINT ( 'NONE',  ( -77.74869931532474254, 54.01501336371526918, -10.00000000000000000 ) ) ;
#56551 = CARTESIAN_POINT ( 'NONE',  ( 156.6787608129567673, 279.1700930814473622, 7.332212251875458442 ) ) ;
#56552 = CARTESIAN_POINT ( 'NONE',  ( 200.6737073311291795, 283.0699384897140476, -17.61533935526990291 ) ) ;
#56553 = CARTESIAN_POINT ( 'NONE',  ( 177.0600935255706077, 288.7082641331545574, -9.311180906940547786 ) ) ;
#56554 = CARTESIAN_POINT ( 'NONE',  ( 6.335516158286851329, 48.33503367028950493, 59.99999999999999289 ) ) ;
#56555 = FACE_BOUND ( 'NONE', #45455, .T. ) ;
#56556 = ORIENTED_EDGE ( 'NONE', *, *, #63291, .T. ) ;
#56557 = CARTESIAN_POINT ( 'NONE',  ( 184.4132702264047623, 272.8584048094892296, -16.31558729584348200 ) ) ;
#56558 = CARTESIAN_POINT ( 'NONE',  ( 65.74195682738610458, 69.08314406761469684, -0.1047288108484802499 ) ) ;
#56559 = VERTEX_POINT ( 'NONE', #23511 ) ;
#56561 = ADVANCED_FACE ( 'NONE', ( #8337 ), #1753, .T. ) ;
#56560 = PLANE ( 'NONE',  #30550 ) ;
#56562 = CARTESIAN_POINT ( 'NONE',  ( 156.4559187165143612, 277.2225799599395373, 9.956371387236824688 ) ) ;
#56563 = CARTESIAN_POINT ( 'NONE',  ( 191.5479541429108963, 298.8762066690417782, -9.571052778213795520 ) ) ;
#56564 = CARTESIAN_POINT ( 'NONE',  ( 190.7705347155322499, 300.2227366160529414, 3.504769718465625239 ) ) ;
#56565 = CARTESIAN_POINT ( 'NONE',  ( 163.1484656051875106, 248.0655637253488806, 9.714247672444804138 ) ) ;
#56567 = CARTESIAN_POINT ( 'NONE',  ( 160.4083209155708118, 282.4522129528954224, 6.632880642079271638 ) ) ;
#56566 = CARTESIAN_POINT ( 'NONE',  ( 164.1916602900412840, 284.1804194194341449, -7.017349331522431122 ) ) ;
#56568 = PLANE ( 'NONE',  #26837 ) ;
#56569 = VERTEX_POINT ( 'NONE', #16923 ) ;
#56570 = CARTESIAN_POINT ( 'NONE',  ( 70.21442515943250839, 62.76251953271914630, -13.45827767252464824 ) ) ;
#56571 = DIRECTION ( 'NONE',  ( -0.7440200784635719877, -0.6681572590663519273, 0.000000000000000000 ) ) ;
#56572 = EDGE_CURVE ( 'NONE', #98426, #28484, #85902, .T. ) ;
#56573 = CARTESIAN_POINT ( 'NONE',  ( 70.94226914272195472, 66.08589450064482662, -11.46747304436338410 ) ) ;
#56574 = EDGE_CURVE ( 'NONE', #11342, #63646, #70115, .T. ) ;
#56575 = CARTESIAN_POINT ( 'NONE',  ( 21.76528272068881265, 171.8262482093457777, 3.021315404115420679E-15 ) ) ;
#56576 = CARTESIAN_POINT ( 'NONE',  ( 73.93840856004327122, 68.59252082510937498, 11.39217114877860659 ) ) ;
#56577 = CARTESIAN_POINT ( 'NONE',  ( 80.79374179619712493, 43.01268775703235292, -9.676513497087860571 ) ) ;
#56578 = CARTESIAN_POINT ( 'NONE',  ( 70.17798417058853033, 71.11987868467312524, -1.451298496092467971 ) ) ;
#56579 = CARTESIAN_POINT ( 'NONE',  ( -10.27112140336314994, 171.0024278399161233, -9.188101187500093303 ) ) ;
#56580 = CARTESIAN_POINT ( 'NONE',  ( 90.40467888234286420, 216.8768266524159856, -9.188101187500091527 ) ) ;
#56581 = CARTESIAN_POINT ( 'NONE',  ( 192.4172326059820648, 297.3705722050773943, -12.52563289807247848 ) ) ;
#56582 = CARTESIAN_POINT ( 'NONE',  ( -19.65312891409030271, 93.06504152958497400, -10.00000000000000888 ) ) ;
#56584 = FACE_OUTER_BOUND ( 'NONE', #44065, .T. ) ;
#56583 = AXIS2_PLACEMENT_3D ( 'NONE', #4340, #89021, #96590 ) ;
#56585 = PLANE ( 'NONE',  #37670 ) ;
#56586 = LINE ( 'NONE', #87574, #42117 ) ;
#56587 = CARTESIAN_POINT ( 'NONE',  ( 164.1212835565148396, 284.3603666608088929, 5.877658627662431634 ) ) ;
#56589 = CARTESIAN_POINT ( 'NONE',  ( 76.61245916897973984, 51.33784933831625352, 16.06823738657550038 ) ) ;
#56588 = CARTESIAN_POINT ( 'NONE',  ( 42.65610334793076674, 64.00004027534475881, -10.00000000000000000 ) ) ;
#56590 = CARTESIAN_POINT ( 'NONE',  ( 161.5437845330232278, 250.8449528722815387, 12.69943054604137700 ) ) ;
#56591 = EDGE_CURVE ( 'NONE', #56255, #66534, #46476, .T. ) ;
#56592 = CARTESIAN_POINT ( 'NONE',  ( -66.35579582111500940, 58.76611569233396182, 59.99999999999999289 ) ) ;
#56593 = CARTESIAN_POINT ( 'NONE',  ( 78.30173519175639285, 54.99922236594399294, -16.08531814199762877 ) ) ;
#56594 = CARTESIAN_POINT ( 'NONE',  ( 81.75863700535872169, 59.11420539249230899, 0.4987820251299123764 ) ) ;
#56595 = CARTESIAN_POINT ( 'NONE',  ( 73.40253668476441362, 69.84345263918817182, 9.170520863686014934 ) ) ;
#56596 = VECTOR ( 'NONE', #10639, 1000.000000000000000 ) ;
#56597 = EDGE_CURVE ( 'NONE', #45081, #22391, #88982, .T. ) ;
#56598 = CARTESIAN_POINT ( 'NONE',  ( 36.33204418566946714, 191.7833772461660544, -9.188101187500095079 ) ) ;
#56599 = B_SPLINE_CURVE_WITH_KNOTS ( 'NONE', 3,
 ( #87462, #86943, #88955, #49377 ),
 .UNSPECIFIED., .F., .F.,
 ( 4, 4 ),
 ( 0.008971156174964484836, 0.01512143528327676567 ),
 .UNSPECIFIED. ) ;
#56600 = CARTESIAN_POINT ( 'NONE',  ( 175.6775075963462882, 265.1320719190924819, -16.53680973885410310 ) ) ;
#56601 = CARTESIAN_POINT ( 'NONE',  ( 66.99449581658849695, 218.6744531367911293, 4.594050593750047540 ) ) ;
#56602 = CARTESIAN_POINT ( 'NONE',  ( 161.1232569692349443, 251.5733279787459367, -14.02750397520710557 ) ) ;
#56603 = CARTESIAN_POINT ( 'NONE',  ( 143.8748646542946688, 242.3262482093457777, 3.021315404115420679E-15 ) ) ;
#56604 = ADVANCED_FACE ( 'NONE', ( #40208 ), #48340, .F. ) ;
#56605 = CARTESIAN_POINT ( 'NONE',  ( 163.3771092991411820, 258.0155440589538784, 15.65363653094946983 ) ) ;
#56606 = CARTESIAN_POINT ( 'NONE',  ( 87.42943499906034788, 43.57385683440216440, -3.059512906073269978 ) ) ;
#56608 = VECTOR ( 'NONE', #81462, 1000.000000000000114 ) ;
#56607 = CARTESIAN_POINT ( 'NONE',  ( 175.6771667394953340, 269.4680136230451808, -17.60694476279005372 ) ) ;
#56609 = EDGE_CURVE ( 'NONE', #8540, #26223, #58739, .T. ) ;
#56610 = CARTESIAN_POINT ( 'NONE',  ( 25.31423016981892715, 26.56628583063841731, 9.188101187500006262 ) ) ;
#56611 = CARTESIAN_POINT ( 'NONE',  ( -32.30932376655839988, 25.48519649537502119, 10.00000000000000000 ) ) ;
#56612 = CARTESIAN_POINT ( 'NONE',  ( 79.64551941974546878, 47.76551340485320196, -13.52520812116594762 ) ) ;
#56613 = ORIENTED_EDGE ( 'NONE', *, *, #52945, .T. ) ;
#56614 = CARTESIAN_POINT ( 'NONE',  ( 19.81074232005190794, 13.29860640527291693, -2.839279412974138328 ) ) ;
#56615 = CARTESIAN_POINT ( 'NONE',  ( 83.28711936893076029, 209.7048013555409796, 4.594050593750051981 ) ) ;
#56616 = CARTESIAN_POINT ( 'NONE',  ( 76.63523979702124223, 63.50111620409151669, 15.35509843086873438 ) ) ;
#56617 = CARTESIAN_POINT ( 'NONE',  ( 173.0983074211377470, 289.6757823250843558, -1.024440707233354564 ) ) ;
#56618 = CARTESIAN_POINT ( 'NONE',  ( -32.08474812827099498, 93.55280042723998690, 10.69171554455069284 ) ) ;
#56619 = CARTESIAN_POINT ( 'NONE',  ( 202.0466495549300419, 280.6919328022345894, 16.59926557204200037 ) ) ;
#56620 = ADVANCED_FACE ( 'NONE', ( #93974 ), #22198, .T. ) ;
#56621 = ORIENTED_EDGE ( 'NONE', *, *, #19310, .F. ) ;
#56622 = CARTESIAN_POINT ( 'NONE',  ( 86.22850481619846619, 47.19188645326008924, 10.82438011396962096 ) ) ;
#56623 = CARTESIAN_POINT ( 'NONE',  ( 190.8236500841018426, 286.9672700043819873, 16.17145961683961275 ) ) ;
#56624 = CARTESIAN_POINT ( 'NONE',  ( 119.5336306364421404, 246.4865022471903160, 10.00000000000009237 ) ) ;
#56625 = CARTESIAN_POINT ( 'NONE',  ( 204.9184781223158609, 275.7177798128946620, -12.59106622113254126 ) ) ;
#56626 = CARTESIAN_POINT ( 'NONE',  ( 74.80005638580958305, 53.39398799171427612, 16.06185578139195869 ) ) ;
#56627 = ORIENTED_EDGE ( 'NONE', *, *, #4791, .F. ) ;
#56628 = CARTESIAN_POINT ( 'NONE',  ( 82.07265110639774264, 53.99302234254209054, 15.59308437138326831 ) ) ;
#56629 = EDGE_LOOP ( 'NONE', ( #37928, #35512, #90623, #1481 ) ) ;
#56630 = CARTESIAN_POINT ( 'NONE',  ( 202.8499463704053198, 279.3005819042728604, 17.04674939340617001 ) ) ;
#56631 = CARTESIAN_POINT ( 'NONE',  ( 207.4148751195968430, 270.8028853205232167, -0.5370135912211878582 ) ) ;
#56632 = CARTESIAN_POINT ( 'NONE',  ( 78.99848661620950452, 60.24637179098724005, -16.44349368446546222 ) ) ;
#56633 = ORIENTED_EDGE ( 'NONE', *, *, #74094, .F. ) ;
#56634 = CYLINDRICAL_SURFACE ( 'NONE', #95267, 70.00000000000002842 ) ;
#56635 = ORIENTED_EDGE ( 'NONE', *, *, #33849, .T. ) ;
#56636 = CARTESIAN_POINT ( 'NONE',  ( 189.2316387673287181, 290.2037436208335635, 14.34142323116202533 ) ) ;
#56637 = CARTESIAN_POINT ( 'NONE',  ( 170.6604352838296847, 250.4273314685328558, 3.327069490116406847 ) ) ;
#56638 = CARTESIAN_POINT ( 'NONE',  ( 206.9737897634393846, 271.6399641097157200, -5.521983748659117452 ) ) ;
#56639 = VERTEX_POINT ( 'NONE', #87424 ) ;
#56640 = CARTESIAN_POINT ( 'NONE',  ( 29.48198420892519067, 37.99752408145594273, 5.678558825948276656 ) ) ;
#56641 = CARTESIAN_POINT ( 'NONE',  ( 80.03260168065229152, 44.35101574960664550, 11.52491460830935921 ) ) ;
#56642 = CARTESIAN_POINT ( 'NONE',  ( 84.81351086726648703, 50.35522970061591508, -13.86072692636569670 ) ) ;
#56643 = CARTESIAN_POINT ( 'NONE',  ( 83.29144881691568969, 48.30668213657163079, -12.61020633307858141 ) ) ;
#56644 = FACE_OUTER_BOUND ( 'NONE', #19831, .T. ) ;
#56645 = FACE_OUTER_BOUND ( 'NONE', #16889, .T. ) ;
#56646 = ORIENTED_EDGE ( 'NONE', *, *, #19714, .F. ) ;
#56647 = VERTEX_POINT ( 'NONE', #39697 ) ;
#56648 = LINE ( 'NONE', #95201, #24963 ) ;
#56650 = CARTESIAN_POINT ( 'NONE',  ( 148.1632261683078013, 274.0207597936089883, -7.853210555358286271 ) ) ;
#56649 = CARTESIAN_POINT ( 'NONE',  ( 68.15538884038467415, 65.80901214634647545, 10.85944937509076880 ) ) ;
#56651 = CARTESIAN_POINT ( 'NONE',  ( 81.62233317761165097, 55.86806713927244772, -16.01587696651938941 ) ) ;
#56652 = CARTESIAN_POINT ( 'NONE',  ( 193.7114073116034945, 295.1289958610702797, 14.86160832869823345 ) ) ;
#56653 = CARTESIAN_POINT ( 'NONE',  ( 185.1804351182116193, 292.8895488603085937, -11.95798946474453928 ) ) ;
#56654 = CARTESIAN_POINT ( 'NONE',  ( 171.9695299662907360, 276.3046275190319534, -16.98996149290084645 ) ) ;
#56655 = CARTESIAN_POINT ( 'NONE',  ( 207.6348398075022317, 271.0129033624181147, -3.614878161448662031 ) ) ;
#56656 = CIRCLE ( 'NONE', #13009, 9.212605237762131694 ) ;
#56657 = CARTESIAN_POINT ( 'NONE',  ( 204.4836193250905012, 269.4642819889133989, 2.448151338453079973 ) ) ;
#56658 = CARTESIAN_POINT ( 'NONE',  ( 181.1477013271936016, 287.8971774238942203, -14.15342935774602218 ) ) ;
#56659 = CARTESIAN_POINT ( 'NONE',  ( 95.22211873877630239, 213.5327760586659451, 1.948934522072303157E-15 ) ) ;
#56660 = ORIENTED_EDGE ( 'NONE', *, *, #39316, .F. ) ;
#56661 = CARTESIAN_POINT ( 'NONE',  ( 150.3288696065234262, 271.5028661687476301, 12.61327273338345734 ) ) ;
#56662 = CARTESIAN_POINT ( 'NONE',  ( 164.8075539017095252, 280.4672370525465226, 12.63796469268613265 ) ) ;
#56663 = CARTESIAN_POINT ( 'NONE',  ( 77.79976927246816842, 61.42068562798239384, -16.13251659512815550 ) ) ;
#56664 = ORIENTED_EDGE ( 'NONE', *, *, #82172, .F. ) ;
#56665 = CARTESIAN_POINT ( 'NONE',  ( 168.3202193441510701, 267.1935196533576686, -17.15840090500419635 ) ) ;
#56666 = ORIENTED_EDGE ( 'NONE', *, *, #47497, .F. ) ;
#56667 = CARTESIAN_POINT ( 'NONE',  ( 80.24153816591007171, 44.93970165375741033, -11.25787842664069593 ) ) ;
#56668 = DIRECTION ( 'NONE',  ( -0.2503889871761755259, -0.9681453171404016400, 0.000000000000000000 ) ) ;
#56669 = DIRECTION ( 'NONE',  ( -0.000000000000000000, 0.000000000000000000, -1.000000000000000000 ) ) ;
#56670 = CARTESIAN_POINT ( 'NONE',  ( 159.8732321751776624, 253.7384344327741132, -15.51998349828054202 ) ) ;
#56671 = CARTESIAN_POINT ( 'NONE',  ( 207.6256228060221076, 271.0288676772754002, 1.885008341157026646 ) ) ;
#56672 = CARTESIAN_POINT ( 'NONE',  ( 92.97525793012167128, 233.6744531367911293, 4.594050593750047540 ) ) ;
#56673 = ORIENTED_EDGE ( 'NONE', *, *, #94253, .T. ) ;
#56674 = VECTOR ( 'NONE', #83141, 1000.000000000000227 ) ;
#56675 = ORIENTED_EDGE ( 'NONE', *, *, #14115, .F. ) ;
#56676 = B_SPLINE_SURFACE_WITH_KNOTS ( 'NONE', 3, 1, ( 
 ( #69050, #17742 ),
 ( #46755, #162 ),
 ( #31544, #99980 ),
 ( #7250, #14853 ),
 ( #54331, #31049 ),
 ( #53836, #48642 ),
 ( #62432, #61936 ),
 ( #23442, #84796 ),
 ( #85303, #15846 ),
 ( #77683, #15337 ),
 ( #71945, #10138 ),
 ( #8266, #80070 ),
 ( #38132, #70044 ),
 ( #61449, #93395 ),
 ( #23946, #46232 ),
 ( #30055, #25848 ),
 ( #77156, #41003 ),
 ( #18243, #10641 ),
 ( #84305, #45740 ),
 ( #76662, #81079 ),
 ( #72957, #13139 ),
 ( #80576, #27336 ),
 ( #90164, #72459 ),
 ( #11156, #65809 ),
 ( #64837, #59188 ),
 ( #5031, #35420 ),
 ( #96770, #42023 ),
 ( #58217, #73933 ),
 ( #89196, #34427 ),
 ( #12133, #12642 ),
 ( #66814, #26831 ),
 ( #19744, #73441 ),
 ( #4025, #43512 ),
 ( #20737, #19260 ) ),
 .UNSPECIFIED., .T., .F., .F.,
 ( 4, 2, 2, 2, 2, 2, 2, 2, 2, 2, 2, 2, 2, 2, 2, 2, 4 ),
 ( 2, 2 ),
 ( 0.000000000000000000, 0.06250000000000000000, 0.1250000000000000000, 0.1875000000000000000, 0.2500000000000000000, 0.3125000000000000000, 0.3750000000000000000, 0.4375000000000000000, 0.5000000000000000000, 0.5625000000000000000, 0.6250000000000000000, 0.6875000000000000000, 0.7500000000000000000, 0.8125000000000000000, 0.8750000000000000000, 0.9375000000000000000, 1.000000000000000000 ),
 ( 0.000000000000000000, 1.000000000000000000 ),
 .UNSPECIFIED. ) ;
#56677 = CARTESIAN_POINT ( 'NONE',  ( 162.6541320028305506, 248.9217746405196294, -10.16950121496441817 ) ) ;
#56678 = ORIENTED_EDGE ( 'NONE', *, *, #9835, .T. ) ;
#56679 = EDGE_CURVE ( 'NONE', #41296, #23987, #65924, .T. ) ;
#56680 = CARTESIAN_POINT ( 'NONE',  ( 75.89038410296754478, 65.15355031958958421, -14.48133090960389069 ) ) ;
#56681 = CARTESIAN_POINT ( 'NONE',  ( 165.2848724275795291, 285.9158859995100102, 1.309848662535952224 ) ) ;
#56682 = CARTESIAN_POINT ( 'NONE',  ( 87.45985321408362267, 44.85427673109838764, -6.610136163016259836 ) ) ;
#56683 = CARTESIAN_POINT ( 'NONE',  ( 77.38344707992528981, 49.10671604805792612, -15.27628165681131200 ) ) ;
#56684 = CARTESIAN_POINT ( 'NONE',  ( 87.69233101511819939, 44.71197863951398688, 5.019790285073527869 ) ) ;
#56685 = VERTEX_POINT ( 'NONE', #72668 ) ;
#56686 = CARTESIAN_POINT ( 'NONE',  ( 156.7173554537088194, 259.2045732567815435, 17.96992492779905959 ) ) ;
#56687 = CARTESIAN_POINT ( 'NONE',  ( 160.6540796618634488, 275.6309760589927578, 12.88432021873685329 ) ) ;
#56688 = CARTESIAN_POINT ( 'NONE',  ( 159.9647205790309101, 253.5799718689968927, -16.48298384325780219 ) ) ;
#56689 = CARTESIAN_POINT ( 'NONE',  ( 81.02345755814515371, 43.60871490852765930, 9.417864885350642368 ) ) ;
#56691 = ADVANCED_FACE ( 'NONE', ( #57420 ), #65527, .T. ) ;
#56690 = CARTESIAN_POINT ( 'NONE',  ( 165.0391502558331069, 249.6778246878102436, -10.74756611015070717 ) ) ;
#56692 =( BOUNDED_CURVE ( )  B_SPLINE_CURVE ( 2, ( #34804, #58595, #89568, #20130, #51002, #90055, #81954, #6420, #38286 ),
 .UNSPECIFIED., .F., .T. ) 
 B_SPLINE_CURVE_WITH_KNOTS ( ( 3, 2, 2, 2, 3 ),
 ( 0.4556451612903225645, 0.4569892473118279397, 0.4596774193548386900, 0.4623655913978494403, 0.4637096774193548154 ),
 .UNSPECIFIED. ) 
 CURVE ( )  GEOMETRIC_REPRESENTATION_ITEM ( )  RATIONAL_B_SPLINE_CURVE ( ( 0.9330127018922194093, 0.9330127018922194093, 1.000000000000000000, 0.8660254037844387076, 1.000000000000000000, 0.8660254037844387076, 1.000000000000000000, 0.9330127018922194093, 0.9330127018922194093 ) ) 
 REPRESENTATION_ITEM ( '' )  );
#56693 = CARTESIAN_POINT ( 'NONE',  ( 76.27763170702772300, 51.65450477961197606, -16.17713714789237045 ) ) ;
#56694 = EDGE_CURVE ( 'NONE', #55385, #92377, #84105, .T. ) ;
#56695 = CARTESIAN_POINT ( 'NONE',  ( -22.42236680055709641, 157.8615022471902591, 0.000000000000000000 ) ) ;
#56696 = VERTEX_POINT ( 'NONE', #27045 ) ;
#56697 = CARTESIAN_POINT ( 'NONE',  ( 149.0802483013170558, 274.4411750002399231, 9.053613739816581685 ) ) ;
#56698 = CARTESIAN_POINT ( 'NONE',  ( 200.1662314894802819, 283.9489124310637180, 17.19420058542677054 ) ) ;
#56699 = CARTESIAN_POINT ( 'NONE',  ( 85.81778828754448796, 44.78275566574458111, 7.330141423013616375 ) ) ;
#56700 = CARTESIAN_POINT ( 'NONE',  ( 167.6894627267040221, 249.8065173834789618, 7.802750152793692884 ) ) ;
#56701 = CARTESIAN_POINT ( 'NONE',  ( 77.92825354283080230, 61.79113456967466789, 16.06764011202815823 ) ) ;
#56702 = CARTESIAN_POINT ( 'NONE',  ( 79.14312167556931854, 57.64441083166269664, 0.000000000000000000 ) ) ;
#56703 = B_SPLINE_CURVE_WITH_KNOTS ( 'NONE', 3,
 ( #83856, #14422, #78220, #85876 ),
 .UNSPECIFIED., .F., .F.,
 ( 4, 4 ),
 ( 0.007911187398149459662, 0.01299107505613515852 ),
 .UNSPECIFIED. ) ;
#56704 = LINE ( 'NONE', #72938, #5794 ) ;
#56705 = EDGE_LOOP ( 'NONE', ( #91835, #33839, #6415, #10043 ) ) ;
#56706 = CARTESIAN_POINT ( 'NONE',  ( 36.19122982252199705, 21.86426979415092120, -3.090169943749474069 ) ) ;
#56707 = CARTESIAN_POINT ( 'NONE',  ( 165.0156970625405108, 244.8314239717225007, -1.890480716182876719 ) ) ;
#56708 = CARTESIAN_POINT ( 'NONE',  ( 182.1950578011920356, 264.4196723021682942, 13.52627809525725766 ) ) ;
#56709 = CARTESIAN_POINT ( 'NONE',  ( 181.4632975752175525, 255.1188003790442167, 1.936479460681336695 ) ) ;
#56710 = CARTESIAN_POINT ( 'NONE',  ( 37.75683693788968753, 23.92755873383628895, 6.180339887498953466 ) ) ;
#56711 = CARTESIAN_POINT ( 'NONE',  ( 30.34687108590970794, 93.06504152958497400, -25.00000000000000000 ) ) ;
#56712 = CARTESIAN_POINT ( 'NONE',  ( 180.7241246963670278, 273.1865840351073871, 16.76835723274534473 ) ) ;
#56713 = CARTESIAN_POINT ( 'NONE',  ( 161.1099616491931386, 273.3624908465563408, -15.23233197322572074 ) ) ;
#56714 = CARTESIAN_POINT ( 'NONE',  ( 84.89389514258827774, 43.37484338261454297, -5.486889282241953048 ) ) ;
#56715 = CARTESIAN_POINT ( 'NONE',  ( 161.4816992964961742, 250.9524876563463067, -12.92750327687364198 ) ) ;
#56716 = EDGE_CURVE ( 'NONE', #73949, #84464, #11850, .T. ) ;
#56717 = CARTESIAN_POINT ( 'NONE',  ( 7.212287079182728711, 162.7202760586659736, -5.415160957724236172E-17 ) ) ;
#56718 = CARTESIAN_POINT ( 'NONE',  ( 81.43924684539796033, 45.70540712647618875, 11.36428502046352307 ) ) ;
#56719 = ORIENTED_EDGE ( 'NONE', *, *, #80380, .T. ) ;
#56720 = CARTESIAN_POINT ( 'NONE',  ( 86.55741050250372837, 46.28210205434145053, 9.003020896430676601 ) ) ;
#56721 = EDGE_CURVE ( 'NONE', #49930, #91334, #26114, .T. ) ;
#56722 = CARTESIAN_POINT ( 'NONE',  ( -42.93703707550763937, 69.35047530159833684, -10.00000000000000000 ) ) ;
#56723 = CARTESIAN_POINT ( 'NONE',  ( 82.34816354767144730, 41.40331793722689468, 5.506344658241145495 ) ) ;
#56724 = CARTESIAN_POINT ( 'NONE',  ( 41.71789998727770410, 185.7048013555409796, 4.594050593750051981 ) ) ;
#56725 = CARTESIAN_POINT ( 'NONE',  ( 164.4698008747318738, 245.7769439046653019, -6.272955660526681854 ) ) ;
#56726 = CARTESIAN_POINT ( 'NONE',  ( 43.11943305279750405, 25.86426979415093186, -3.090169943749474069 ) ) ;
#56727 = CARTESIAN_POINT ( 'NONE',  ( 200.1294354126899009, 267.3366221627135246, -6.812218948514619399 ) ) ;
#56728 = CARTESIAN_POINT ( 'NONE',  ( 146.6138605399200117, 276.7043397814778132, -0.5394499176159462950 ) ) ;
#56729 = CARTESIAN_POINT ( 'NONE',  ( 149.5042310455230563, 271.6980712130745701, 11.54652286044134613 ) ) ;
#56730 = CARTESIAN_POINT ( 'NONE',  ( 182.5277673056334891, 280.1954785146588733, -16.09861734911579489 ) ) ;
#56731 = EDGE_CURVE ( 'NONE', #54308, #81557, #56221, .T. ) ;
#56732 = CARTESIAN_POINT ( 'NONE',  ( 186.5436611748800999, 296.3120891398685899, -8.818239198042506999 ) ) ;
#56733 = FACE_OUTER_BOUND ( 'NONE', #61787, .T. ) ;
#56734 = AXIS2_PLACEMENT_3D ( 'NONE', #58375, #89351, #19904 ) ;
#56735 = CARTESIAN_POINT ( 'NONE',  ( 80.56248746614240019, 223.9865022471902876, 10.00000000000009237 ) ) ;
#56736 = CARTESIAN_POINT ( 'NONE',  ( 70.77885289983220218, 66.68069319803313988, -10.82095828200581344 ) ) ;
#56737 = CARTESIAN_POINT ( 'NONE',  ( 28.99180842189336005, 40.23654200823203553, 1.583844403245397769 ) ) ;
#56738 = CARTESIAN_POINT ( 'NONE',  ( 41.20343708195693466, 194.5958772461660544, -9.188101187500095079 ) ) ;
#56739 = CARTESIAN_POINT ( 'NONE',  ( -1.617403181491035902, 158.3262482093458061, 3.021315404115420679E-15 ) ) ;
#56740 = ORIENTED_EDGE ( 'NONE', *, *, #11054, .T. ) ;
#56741 = CARTESIAN_POINT ( 'NONE',  ( -13.57166651430987514, 85.17168110439646966, 14.94339635218015694 ) ) ;
#56742 = CARTESIAN_POINT ( 'NONE',  ( 147.5848197185516142, 275.0225891520124151, 4.420251097676741736 ) ) ;
#56743 = FACE_OUTER_BOUND ( 'NONE', #23496, .T. ) ;
#56744 = ORIENTED_EDGE ( 'NONE', *, *, #11433, .F. ) ;
#56745 = CARTESIAN_POINT ( 'NONE',  ( 167.3695604279846805, 285.2551170359605521, 7.881098619243475767 ) ) ;
#56746 = DIRECTION ( 'NONE',  ( 0.8660254037844382635, 0.5000000000000005551, 0.000000000000000000 ) ) ;
#56747 = DIRECTION ( 'NONE',  ( -0.8916269620120498285, 0.4527707594502571875, 0.000000000000000000 ) ) ;
#56748 = CARTESIAN_POINT ( 'NONE',  ( 191.1996875990947444, 299.0642907557634658, -7.109168602002305271 ) ) ;
#56749 = CARTESIAN_POINT ( 'NONE',  ( 23.84800118292001159, 31.95586893147756058, 7.433330006724141015 ) ) ;
#56750 = CARTESIAN_POINT ( 'NONE',  ( 163.1484656051875106, 248.0655637253488806, 9.714247672444804138 ) ) ;
#56751 = CARTESIAN_POINT ( 'NONE',  ( 196.5475899070771675, 290.2165835061676944, -17.89382743182097002 ) ) ;
#56752 = CARTESIAN_POINT ( 'NONE',  ( 171.8181756328044116, 255.8907789784637998, 11.22456348869178910 ) ) ;
#56753 = VERTEX_POINT ( 'NONE', #89867 ) ;
#56754 = CARTESIAN_POINT ( 'NONE',  ( 11.61360469066603507, 28.74646525600389069, 2.839279412974139660 ) ) ;
#56755 = CARTESIAN_POINT ( 'NONE',  ( 44.85937643310610667, 116.8208962945185050, -10.00000000000000000 ) ) ;
#56756 = CARTESIAN_POINT ( 'NONE',  ( 71.92697733641804803, 72.63665773354594535, -0.7151800694983956319 ) ) ;
#56757 = ORIENTED_EDGE ( 'NONE', *, *, #20110, .T. ) ;
#56758 = CARTESIAN_POINT ( 'NONE',  ( 178.6323200210636344, 282.3665200627499416, 15.66371996646872056 ) ) ;
#56759 = CARTESIAN_POINT ( 'NONE',  ( 151.1926529451685326, 268.7736386982768408, 14.30343427984827365 ) ) ;
#56760 = LINE ( 'NONE', #3101, #71174 ) ;
#56761 = CARTESIAN_POINT ( 'NONE',  ( 48.05312180239142350, 111.8345470171556428, -10.00000000000000000 ) ) ;
#56762 = EDGE_LOOP ( 'NONE', ( #33339, #6605, #27104, #86969 ) ) ;
#56763 = EDGE_LOOP ( 'NONE', ( #5970, #97763, #53194, #9384 ) ) ;
#56765 = CARTESIAN_POINT ( 'NONE',  ( -29.91485116994501325, 25.08783183303773967, -10.00000000000000000 ) ) ;
#56764 = DIRECTION ( 'NONE',  ( -0.8770933717188628131, -0.4803199113995136327, 0.000000000000000000 ) ) ;
#56766 = CARTESIAN_POINT ( 'NONE',  ( 182.2373335159190901, 280.9600371166583841, -17.30031729693378040 ) ) ;
#56767 = ORIENTED_EDGE ( 'NONE', *, *, #9145, .F. ) ;
#56768 = CARTESIAN_POINT ( 'NONE',  ( 200.7484899876179441, 282.9404111291507888, -16.88964748465601673 ) ) ;
#56769 = CARTESIAN_POINT ( 'NONE',  ( 72.05747908138206981, 72.41062208079183904, -3.017343731799825512 ) ) ;
#56770 = CARTESIAN_POINT ( 'NONE',  ( 72.99661548417863344, 57.62305516421401563, -16.32377903997647550 ) ) ;
#56771 = CARTESIAN_POINT ( 'NONE',  ( 78.28473355307382064, 61.06446511097402663, -15.91087495820213427 ) ) ;
#56772 = EDGE_CURVE ( 'NONE', #77760, #43169, #78845, .T. ) ;
#56773 = CARTESIAN_POINT ( 'NONE',  ( 157.1269483542914998, 258.4951375425532092, -17.15328932028234377 ) ) ;
#56774 = CARTESIAN_POINT ( 'NONE',  ( 113.2460989071574460, 230.0643266524159856, 9.188101187500095079 ) ) ;
#56775 = CARTESIAN_POINT ( 'NONE',  ( 184.1050185429027124, 288.7504959939380456, -13.16857183658926367 ) ) ;
#56776 = ORIENTED_EDGE ( 'NONE', *, *, #38040, .F. ) ;
#56777 = CARTESIAN_POINT ( 'NONE',  ( 208.0692320075777957, 270.2605140014760536, 2.043861372130216569 ) ) ;
#56778 = ORIENTED_EDGE ( 'NONE', *, *, #51860, .T. ) ;
#56779 = CARTESIAN_POINT ( 'NONE',  ( 33.80247542503471436, 34.91421378149921395, 9.188101187500008038 ) ) ;
#56780 = CARTESIAN_POINT ( 'NONE',  ( 159.2511875226268216, 254.8158473755685520, 15.75855490706745599 ) ) ;
#56781 = CARTESIAN_POINT ( 'NONE',  ( 78.38442356856859305, 47.88785470443450976, -14.51451505513508877 ) ) ;
#56782 = CARTESIAN_POINT ( 'NONE',  ( 62.82726920452340380, 197.8923013555409796, 4.594050593750050204 ) ) ;
#56783 = CARTESIAN_POINT ( 'NONE',  ( 73.89028189157257032, 68.56231543382321547, 10.89439152759356944 ) ) ;
#56784 = CARTESIAN_POINT ( 'NONE',  ( 190.8623743139412454, 300.0636657654615647, 8.577953960666059530 ) ) ;
#56785 = CARTESIAN_POINT ( 'NONE',  ( 198.5799742811345823, 286.6963905097911152, 17.08859794237710261 ) ) ;
#56786 = CARTESIAN_POINT ( 'NONE',  ( 176.0425021715459195, 272.9246667940608972, 16.74622359246633962 ) ) ;
#56787 = ORIENTED_EDGE ( 'NONE', *, *, #48102, .T. ) ;
#56788 = CARTESIAN_POINT ( 'NONE',  ( 77.76107068773923459, 57.49243831483684630, -16.18103606519603588 ) ) ;
#56789 = CARTESIAN_POINT ( 'NONE',  ( 176.7233542493291907, 288.6475378244585954, 11.36909801418409494 ) ) ;
#56790 = DIRECTION ( 'NONE',  ( 0.000000000000000000, -0.000000000000000000, -1.000000000000000000 ) ) ;
#56791 = ORIENTED_EDGE ( 'NONE', *, *, #59835, .T. ) ;
#56792 = CARTESIAN_POINT ( 'NONE',  ( 110.2158993104859945, 222.8932355074535678, -2.679491924311248496 ) ) ;
#56793 = CARTESIAN_POINT ( 'NONE',  ( 68.18719692898707763, 69.37638032551880940, -4.036890616949536437 ) ) ;
#56794 = CARTESIAN_POINT ( 'NONE',  ( 161.8839333999304415, 250.2557977526613229, -13.90128376743482441 ) ) ;
#56795 = CARTESIAN_POINT ( 'NONE',  ( 44.44844410339184293, 68.22168590943847732, -10.00000000000000000 ) ) ;
#56796 = EDGE_CURVE ( 'NONE', #82804, #15274, #1891, .T. ) ;
#56797 = CARTESIAN_POINT ( 'NONE',  ( 190.7862358025146534, 300.1955415356651429, 3.573119809004446257 ) ) ;
#56798 = CARTESIAN_POINT ( 'NONE',  ( 177.1800844086890265, 269.5441809915307658, 16.12773907670574047 ) ) ;
#56799 = CARTESIAN_POINT ( 'NONE',  ( 205.8452707775803390, 274.1125278458945900, 11.42742867493066328 ) ) ;
#56800 = CARTESIAN_POINT ( 'NONE',  ( 75.63519723909450931, 65.56940250126960734, 13.79863107474653106 ) ) ;
#56801 = CARTESIAN_POINT ( 'NONE',  ( 164.5456390861338889, 254.4766699602316748, 14.11842207354146517 ) ) ;
#56802 = CARTESIAN_POINT ( 'NONE',  ( 164.4698008747318738, 245.7769439046653019, -6.272955660526681854 ) ) ;
#56803 = CARTESIAN_POINT ( 'NONE',  ( 124.5044291563551297, 236.5643266524159856, -9.188101187500093303 ) ) ;
#56804 = EDGE_LOOP ( 'NONE', ( #70987, #47280, #92112, #74341 ) ) ;
#56805 = CARTESIAN_POINT ( 'NONE',  ( 85.46896714245875160, 44.18043371586173151, -6.563648887624578876 ) ) ;
#56806 = DIRECTION ( 'NONE',  ( 0.9505498757754579087, -0.3105719460338643989, 0.000000000000000000 ) ) ;
#56807 = CARTESIAN_POINT ( 'NONE',  ( 173.4505375608857491, 284.9503170016366198, -13.05978560202663452 ) ) ;
#56808 = EDGE_CURVE ( 'NONE', #19318, #58918, #79161, .T. ) ;
#56809 = CARTESIAN_POINT ( 'NONE',  ( 204.1793240545508752, 276.9980322128846524, 14.17550310845996187 ) ) ;
#56810 = EDGE_CURVE ( 'NONE', #53896, #80748, #9259, .T. ) ;
#56811 = CARTESIAN_POINT ( 'NONE',  ( 126.8249895137406043, 232.4824982072973683, 3.021315404115420679E-15 ) ) ;
#56812 = AXIS2_PLACEMENT_3D ( 'NONE', #13070, #15021, #5452 ) ;
#56813 = CARTESIAN_POINT ( 'NONE',  ( 76.08933885469296854, 51.45880163392949669, -15.66904507028006321 ) ) ;
#56814 = EDGE_LOOP ( 'NONE', ( #15051, #34603, #52924, #96557, #5417, #1605, #90578, #1093, #13096, #49197, #36117, #68596, #42347, #81267, #10810, #97057, #84270, #9412, #1976, #88146 ) ) ;
#56815 = CARTESIAN_POINT ( 'NONE',  ( 80.65100716643621581, 57.48104863357441729, -16.23842874147667104 ) ) ;
#56816 = CARTESIAN_POINT ( 'NONE',  ( 158.4257592686963392, 274.9310561177994714, -12.53665520930496236 ) ) ;
#56817 = CARTESIAN_POINT ( 'NONE',  ( -56.14442822474984496, 33.32908021129815523, 10.00000000000000000 ) ) ;
#56818 = CARTESIAN_POINT ( 'NONE',  ( 206.2849804695184446, 273.3509283188774930, -9.687080623179198824 ) ) ;
#56819 = CARTESIAN_POINT ( 'NONE',  ( 140.9585647324944659, 258.3149278399160380, 9.188101187500093303 ) ) ;
#56820 = CARTESIAN_POINT ( 'NONE',  ( 195.7075834170777568, 263.4542553332885291, 0.8725129583350295093 ) ) ;
#56821 = CARTESIAN_POINT ( 'NONE',  ( 186.4625004638162977, 297.1001920529987501, 4.671785278466259683 ) ) ;
#56822 = CARTESIAN_POINT ( 'NONE',  ( 67.72909538816377051, 68.47758282218532599, 5.729597447110076125 ) ) ;
#56823 = CARTESIAN_POINT ( 'NONE',  ( 63.01627839189497138, 213.3149278399160949, 9.188101187500093303 ) ) ;
#56824 = CARTESIAN_POINT ( 'NONE',  ( 157.8696211474012330, 257.2087905314882619, -17.27527248276125604 ) ) ;
#56825 = CARTESIAN_POINT ( 'NONE',  ( 174.3370073287761670, 251.3632962845142629, 3.630733893980507609 ) ) ;
#56826 = CARTESIAN_POINT ( 'NONE',  ( 171.9118076701954578, 260.5665906372238396, 14.62201537552227393 ) ) ;
#56827 = CARTESIAN_POINT ( 'NONE',  ( 155.3846098364971056, 279.6728254248552048, -1.556306295007354956 ) ) ;
#56828 = CARTESIAN_POINT ( 'NONE',  ( 172.6426272267430022, 287.7740647968764733, -8.307796791299765005 ) ) ;
#56829 = CARTESIAN_POINT ( 'NONE',  ( 155.0304386007204016, 262.1263989543018056, -17.12961552904782181 ) ) ;
#56830 = CARTESIAN_POINT ( 'NONE',  ( 156.9852748171393273, 271.9751496516061025, -15.17404613224120880 ) ) ;
#56831 = EDGE_CURVE ( 'NONE', #67005, #52194, #32198, .T. ) ;
#56832 = CARTESIAN_POINT ( 'NONE',  ( 130.3409059842875877, 239.3927522451417929, -10.00000000000009059 ) ) ;
#56833 = FACE_OUTER_BOUND ( 'NONE', #17564, .T. ) ;
#56834 = VERTEX_POINT ( 'NONE', #16312 ) ;
#56835 = CARTESIAN_POINT ( 'NONE',  ( 160.3242080723612730, 258.1019776236436201, -17.22713985970005979 ) ) ;
#56836 = CARTESIAN_POINT ( 'NONE',  ( 4.289451341410245533, 161.0327760586659451, 1.948934522072302763E-15 ) ) ;
#56837 = CARTESIAN_POINT ( 'NONE',  ( 43.17879721251643588, 204.9244531367911293, -4.594050593750046652 ) ) ;
#56838 = CARTESIAN_POINT ( 'NONE',  ( 19.65800174957785629, 23.30066082961421969, -10.00000000000000533 ) ) ;
#56839 = CARTESIAN_POINT ( 'NONE',  ( 68.34576586436469370, 65.68917945663493185, -10.35820680181607401 ) ) ;
#56840 = CARTESIAN_POINT ( 'NONE',  ( 70.62955678152277983, 60.80479719363770386, -15.06269029744276899 ) ) ;
#56841 = CARTESIAN_POINT ( 'NONE',  ( 58.10966550219799132, 178.3759306620403606, -17.47570218321536473 ) ) ;
#56842 = CARTESIAN_POINT ( 'NONE',  ( 147.2443490232117256, 275.6123016948292275, 5.226063659459642352 ) ) ;
#56843 = FACE_OUTER_BOUND ( 'NONE', #72649, .T. ) ;
#56845 = CARTESIAN_POINT ( 'NONE',  ( 65.31683191680592415, 208.5177522451418497, -10.00000000000009592 ) ) ;
#56844 = CARTESIAN_POINT ( 'NONE',  ( 18.86588705934989108, 49.77739081350934924, 59.99999999999999289 ) ) ;
#56846 = CARTESIAN_POINT ( 'NONE',  ( 120.0388121219830282, 250.1115022471903160, -5.000000000000047962 ) ) ;
#56847 = CARTESIAN_POINT ( 'NONE',  ( 163.1238134150576968, 256.2434428063396581, -15.10086001857528970 ) ) ;
#56848 = CARTESIAN_POINT ( 'NONE',  ( 157.3198323354746435, 258.1610526871778006, -16.77630483474704093 ) ) ;
#56849 = CARTESIAN_POINT ( 'NONE',  ( 154.2194984598485519, 265.5309884801890234, 17.12742652472672944 ) ) ;
#56850 = CARTESIAN_POINT ( 'NONE',  ( 45.19978347827785825, 190.2365022471902023, 10.00000000000009592 ) ) ;
#56851 = CARTESIAN_POINT ( 'NONE',  ( -15.31269525828471068, 104.2312461070085021, 36.50000000000000000 ) ) ;
#56852 = CARTESIAN_POINT ( 'NONE',  ( 164.4698008747318738, 245.7769439046653019, -6.272955660526681854 ) ) ;
#56853 = CARTESIAN_POINT ( 'NONE',  ( 4.315907217689738395, 182.4869531367911293, 4.594050593750046652 ) ) ;
#56854 = CARTESIAN_POINT ( 'NONE',  ( 40.42214693012152793, 25.19860640527295104, 2.839279412974134775 ) ) ;
#56855 = CARTESIAN_POINT ( 'NONE',  ( 24.35067441160642687, 40.23626134430271861, -10.00000000000000000 ) ) ;
#56856 = CARTESIAN_POINT ( 'NONE',  ( 79.14312167556931854, 57.64441083166269664, 0.000000000000000000 ) ) ;
#56857 = CARTESIAN_POINT ( 'NONE',  ( 38.69009612255265296, 24.19860640527295104, 2.839279412974134775 ) ) ;
#56858 = CARTESIAN_POINT ( 'NONE',  ( -162.0327448629461742, 33.95614270198240803, 21.50000000000000000 ) ) ;
#56859 = CARTESIAN_POINT ( 'NONE',  ( -22.42236680055709641, 157.8615022471902591, 0.000000000000000000 ) ) ;
#56860 = CARTESIAN_POINT ( 'NONE',  ( 196.2379679265050925, 290.7528645076583871, -16.93678934971137906 ) ) ;
#56861 = B_SPLINE_CURVE_WITH_KNOTS ( 'NONE', 3,
 ( #100217, #92632, #23181, #18101, #11518, #49003, #18608, #57080, #65681, #56587, #79937, #10006, #11017, #10496, #2412, #88059, #87575, #12005, #81435, #42863, #41888, #80444, #80952, #33815, #33290, #41380, #65192, #25708, #27706, #40869, #34294, #72320, #2925, #64192, #95142, #64702, #4389, #73797, #73307, #35287, #96637, #71815, #95653, #26200, #49487, #72827, #50481, #3420, #96138, #26696 ),
 .UNSPECIFIED., .F., .F.,
 ( 4, 2, 2, 2, 2, 2, 2, 2, 2, 2, 2, 2, 2, 2, 2, 2, 2, 2, 2, 2, 2, 2, 2, 2, 4 ),
 ( 0.001054687649897483601, 0.001531829325746945436, 0.002008971001596407489, 0.002247541839521137973, 0.002486112677445868890, 0.002605398096408233916, 0.002724683515370599808, 0.002843968934332965267, 0.002963254353295330726, 0.003440396029144835929, 0.003917537704994342000, 0.004871821056693417459, 0.005826104408392492919, 0.006303246084241995520, 0.006780387760091497254, 0.006899673179053816309, 0.006959315888535009230, 0.007018958598016202151, 0.007138244016978573248, 0.007257529435940943477, 0.007496100273865653578, 0.007734671111790362812, 0.007973241949715072913, 0.008211812787639783881, 0.008688954463489200614 ),
 .UNSPECIFIED. ) ;
#56862 = CARTESIAN_POINT ( 'NONE',  ( 150.0694502760089222, 271.4680435213315945, -12.17790201236558545 ) ) ;
#56863 =( NAMED_UNIT ( * ) SI_UNIT ( $, .STERADIAN. ) SOLID_ANGLE_UNIT ( ) );
#56864 = EDGE_CURVE ( 'NONE', #77944, #24489, #47206, .T. ) ;
#56865 = CARTESIAN_POINT ( 'NONE',  ( 8.350964356584899662, 25.79752408145590792, -5.678558825948271327 ) ) ;
#56866 = CARTESIAN_POINT ( 'NONE',  ( 168.8436447018356716, 287.8931087461074299, 0.5168480269480507650 ) ) ;
#56867 = CARTESIAN_POINT ( 'NONE',  ( 11.93836421708519779, 28.93396525600389069, 2.839279412974139660 ) ) ;
#56868 = CARTESIAN_POINT ( 'NONE',  ( 160.6031540345039446, 252.4741726868657281, 15.87852846076284763 ) ) ;
#56869 = CARTESIAN_POINT ( 'NONE',  ( 153.2185337766395890, 277.6703050030072291, -5.188401963753405788 ) ) ;
#56870 = CARTESIAN_POINT ( 'NONE',  ( 84.58308955143566266, 49.89698236725671165, -13.67050406800346707 ) ) ;
#56871 = CARTESIAN_POINT ( 'NONE',  ( 159.6288139302610887, 254.1617792512662675, -15.32287760493869477 ) ) ;
#56872 = VERTEX_POINT ( 'NONE', #47697 ) ;
#56873 = CARTESIAN_POINT ( 'NONE',  ( 152.4293375737637177, 267.0122523221186839, 15.45871950931433325 ) ) ;
#56874 = CARTESIAN_POINT ( 'NONE',  ( 164.5867587387928950, 245.5743669417666126, -3.022048486790635202 ) ) ;
#56875 = CARTESIAN_POINT ( 'NONE',  ( 104.9037214839949002, 219.8262482093457777, 3.021315404115420679E-15 ) ) ;
#56876 = CARTESIAN_POINT ( 'NONE',  ( 87.20396902780147741, 45.40285486062717979, 7.109937478028163227 ) ) ;
#56877 = VECTOR ( 'NONE', #44636, 1000.000000000000114 ) ;
#56878 = CARTESIAN_POINT ( 'NONE',  ( 193.9966098916996771, 294.6350105018939871, 13.97117019253516013 ) ) ;
#56879 = ORIENTED_EDGE ( 'NONE', *, *, #75038, .F. ) ;
#56880 = VERTEX_POINT ( 'NONE', #22905 ) ;
#56881 = DIRECTION ( 'NONE',  ( 1.000000000000000000, 0.000000000000000000, 0.000000000000000000 ) ) ;
#56882 = CARTESIAN_POINT ( 'NONE',  ( 86.16320141619598871, 47.68791953076239309, 10.83576430555930514 ) ) ;
#56883 = ORIENTED_EDGE ( 'NONE', *, *, #14525, .F. ) ;
#56884 = CARTESIAN_POINT ( 'NONE',  ( 78.14700529810005492, 60.07939060848261192, 16.01736686316025171 ) ) ;
#56885 = LINE ( 'NONE', #1716, #82417 ) ;
#56886 = ORIENTED_EDGE ( 'NONE', *, *, #29398, .T. ) ;
#56887 = CARTESIAN_POINT ( 'NONE',  ( 78.17184439828042741, 61.78404217785180919, -15.73488545980961106 ) ) ;
#56888 = CARTESIAN_POINT ( 'NONE',  ( 83.70979198902698215, 48.81106761220289769, -12.83638129120513582 ) ) ;
#56889 = CARTESIAN_POINT ( 'NONE',  ( 80.73218360117679993, 43.11930967842982199, 9.845968670453535410 ) ) ;
#56890 = ORIENTED_EDGE ( 'NONE', *, *, #50555, .T. ) ;
#56891 = CARTESIAN_POINT ( 'NONE',  ( 173.7270898585821612, 267.2108298537337987, 16.98825523054146558 ) ) ;
#56892 = CARTESIAN_POINT ( 'NONE',  ( 169.3652806017343835, 276.2350476629839591, -15.58549988110435258 ) ) ;
#56893 = CARTESIAN_POINT ( 'NONE',  ( 13.75631770279071020, 31.55236904046464375, 10.00000000000000000 ) ) ;
#56894 = B_SPLINE_CURVE_WITH_KNOTS ( 'NONE', 3,
 ( #37411, #68317, #21241, #12145, #74462, #52118, #8039, #45998, #47517, #77939, #54600, #68814, #93155, #77441, #8529, #16619, #22732, #30827, #70830, #76917, #1441, #15606, #61214, #84568, #94164, #69816, #9024, #39401, #78444, #7515, #70315, #15106, #23211, #63222, #930, #85059, #32321, #428, #16125, #38409, #31315, #76443, #61713, #24716, #93664, #62204 ),
 .UNSPECIFIED., .F., .F.,
 ( 4, 1, 1, 1, 2, 2, 1, 1, 1, 2, 2, 1, 1, 2, 2, 1, 1, 2, 2, 1, 1, 2, 2, 1, 2, 2, 1, 2, 2, 4 ),
 ( 0.000000000000000000, 0.06249999999999045208, 0.09374999999998595568, 0.1093749999999837630, 0.1171874999999826666, 0.1249999999999815703, 0.1874999999999715505, 0.2187499999999681921, 0.2343749999999664990, 0.2421874999999656386, 0.2499999999999647504, 0.3124999999999691358, 0.3437499999999713562, 0.3593749999999705236, 0.3749999999999696909, 0.4374999999999719114, 0.4687499999999726885, 0.4843749999999730771, 0.4999999999999734657, 0.5624999999999801270, 0.5937499999999854561, 0.6093749999999880096, 0.6249999999999906741, 0.6874999999999933387, 0.7187499999999946709, 0.7499999999999960032, 0.8124999999999956701, 0.8437499999999957812, 0.8749999999999958922, 1.000000000000000000 ),
 .UNSPECIFIED. ) ;
#56895 = ORIENTED_EDGE ( 'NONE', *, *, #75807, .F. ) ;
#56896 = LINE ( 'NONE', #1731, #13150 ) ;
#56897 = CARTESIAN_POINT ( 'NONE',  ( 163.2835940097493790, 247.8315144631017404, 11.08416305054517359 ) ) ;
#56898 = ORIENTED_EDGE ( 'NONE', *, *, #47829, .T. ) ;
#56899 = VERTEX_POINT ( 'NONE', #70508 ) ;
#56900 = CARTESIAN_POINT ( 'NONE',  ( 157.8523751997425109, 267.2426576861807916, -16.20207976436619646 ) ) ;
#56901 = ORIENTED_EDGE ( 'NONE', *, *, #57496, .T. ) ;
#56902 = CARTESIAN_POINT ( 'NONE',  ( 66.31795133325435643, 69.20145725284447735, 2.477662600225434719 ) ) ;
#56903 = ORIENTED_EDGE ( 'NONE', *, *, #15929, .T. ) ;
#56904 = CARTESIAN_POINT ( 'NONE',  ( 83.59128512182542181, 50.22172742876573182, -14.18173862977107902 ) ) ;
#56905 = CARTESIAN_POINT ( 'NONE',  ( 193.5379746301957198, 295.4293900769612833, 13.37282311005296620 ) ) ;
#56906 = CARTESIAN_POINT ( 'NONE',  ( 177.3353965951741316, 288.8196383795363431, -9.382684147788728168 ) ) ;
#56907 = CARTESIAN_POINT ( 'NONE',  ( 69.52914236679859528, 65.28759244955678298, 11.39865997334715253 ) ) ;
#56908 = CARTESIAN_POINT ( 'NONE',  ( 192.0963028965829551, 297.9264387674147656, 11.34530024772836754 ) ) ;
#56909 = CARTESIAN_POINT ( 'NONE',  ( 175.3742949935872844, 291.1603597146743141, 6.550094823951227774 ) ) ;
#56910 = CARTESIAN_POINT ( 'NONE',  ( 192.9476382485522947, 262.0161990052710621, 3.467033003238014999 ) ) ;
#56911 = ORIENTED_EDGE ( 'NONE', *, *, #29335, .T. ) ;
#56912 = CARTESIAN_POINT ( 'NONE',  ( 26.18314342202568668, 41.82794442100486521, -10.00000000000000000 ) ) ;
#56913 = CARTESIAN_POINT ( 'NONE',  ( 20.98529944902502820, 27.51421378149918695, -9.188101187500004485 ) ) ;
#56914 = CARTESIAN_POINT ( 'NONE',  ( 206.2456893945931142, 273.4189824569319285, 10.13882547285618152 ) ) ;
#56916 = CARTESIAN_POINT ( 'NONE',  ( 206.0041637419966776, 273.8373171585603814, 11.66586596407113596 ) ) ;
#56915 = CARTESIAN_POINT ( 'NONE',  ( 196.6317700900902139, 290.0707791521982131, -17.91116578096951883 ) ) ;
#56917 = CARTESIAN_POINT ( 'NONE',  ( 159.5204760365350012, 254.3494259875849082, 16.90107507090185379 ) ) ;
#56918 = ORIENTED_EDGE ( 'NONE', *, *, #14892, .F. ) ;
#56919 = CARTESIAN_POINT ( 'NONE',  ( 187.6303425324672958, 277.1110116237759939, 17.31978431366381699 ) ) ;
#56920 = CARTESIAN_POINT ( 'NONE',  ( 171.2828659525146975, 259.2707523077851874, -13.88512410246953088 ) ) ;
#56921 = CARTESIAN_POINT ( 'NONE',  ( 15.56473500984127512, 9.390406791769814632, -7.779800476318352071E-15 ) ) ;
#56922 = DIRECTION ( 'NONE',  ( 0.9598361373656965068, -0.2805612043866717586, 0.000000000000000000 ) ) ;
#56923 = EDGE_CURVE ( 'NONE', #9815, #45024, #17345, .T. ) ;
#56924 = B_SPLINE_CURVE_WITH_KNOTS ( 'NONE', 3,
 ( #19680, #57142, #35851, #51038 ),
 .UNSPECIFIED., .F., .F.,
 ( 4, 4 ),
 ( 0.04746404433603530065, 0.04887066958154934887 ),
 .UNSPECIFIED. ) ;
#56925 = CARTESIAN_POINT ( 'NONE',  ( 199.3485334918771628, 285.3652069081594504, -18.27963836619689175 ) ) ;
#56926 = EDGE_CURVE ( 'NONE', #35722, #74770, #36799, .T. ) ;
#56927 = CARTESIAN_POINT ( 'NONE',  ( 190.7990164375790130, 261.9893415206284430, -0.6577425147695087349 ) ) ;
#56928 = VERTEX_POINT ( 'NONE', #77108 ) ;
#56929 = CARTESIAN_POINT ( 'NONE',  ( 158.7247586461176354, 260.9712587547172689, -17.77758391712495012 ) ) ;
#56930 = PLANE ( 'NONE',  #55994 ) ;
#56931 = EDGE_CURVE ( 'NONE', #74125, #35225, #26802, .T. ) ;
#56932 = CARTESIAN_POINT ( 'NONE',  ( -10.43439047959891397, 176.3297689869269220, -2.679491924311252493 ) ) ;
#56933 = EDGE_CURVE ( 'NONE', #2112, #71283, #56302, .T. ) ;
#56934 = CARTESIAN_POINT ( 'NONE',  ( 18.47929132879760417, 168.1427522451417644, 1.119607411625061291E-15 ) ) ;
#56935 = CARTESIAN_POINT ( 'NONE',  ( 101.4736528484039724, 220.2048013555409796, 4.594050593750051981 ) ) ;
#56936 = CARTESIAN_POINT ( 'NONE',  ( 82.71170519429942658, 40.59673265032024148, -1.400181599122515497 ) ) ;
#56937 = B_SPLINE_CURVE_WITH_KNOTS ( 'NONE', 3,
 ( #34746, #12978, #74777, #67144, #21076, #27167, #51952, #66156, #82892, #96101, #26660, #96604, #58055, #19585, #50449, #11969, #97103, #75763, #60518, #23513, #38723, #54406, #30134, #90991, #83887, #92472 ),
 .UNSPECIFIED., .F., .F.,
 ( 4, 2, 2, 2, 2, 2, 2, 2, 2, 2, 2, 2, 4 ),
 ( 0.0002293139140671511035, 0.0008647663282778704844, 0.001182492535383264680, 0.001341355638935961669, 0.001420787190712275360, 0.001460502966600432315, 0.001500218742488589052, 0.001579650294264903177, 0.001659081846041217520, 0.001817944949593846421, 0.002135671156699089478, 0.002453397363804332536, 0.002771123570909575593 ),
 .UNSPECIFIED. ) ;
#56938 = CARTESIAN_POINT ( 'NONE',  ( 19.36651902841724038, 19.38052372038640669, 10.00000000000000533 ) ) ;
#56939 = CARTESIAN_POINT ( 'NONE',  ( 162.7896496350696225, 248.6870512161599436, 11.81710663537990946 ) ) ;
#56940 = CARTESIAN_POINT ( 'NONE',  ( 25.61497981383703149, 185.5958772461660544, -9.188101187500095079 ) ) ;
#56941 = LINE ( 'NONE', #11386, #18743 ) ;
#56942 = ORIENTED_EDGE ( 'NONE', *, *, #27729, .T. ) ;
#56943 = ORIENTED_EDGE ( 'NONE', *, *, #43490, .F. ) ;
#56944 = CARTESIAN_POINT ( 'NONE',  ( 74.37117806044521728, 68.42743621588296321, -11.25900170040250003 ) ) ;
#56945 = CARTESIAN_POINT ( 'NONE',  ( 187.4166251561426293, 263.4339899954952102, 11.64397722261905166 ) ) ;
#56946 = CARTESIAN_POINT ( 'NONE',  ( 83.41573487747820081, 42.76472624850124760, 5.963828435803965711 ) ) ;
#56947 = DIRECTION ( 'NONE',  ( 0.5000000000000012212, -0.8660254037844380415, -0.000000000000000000 ) ) ;
#56948 = CARTESIAN_POINT ( 'NONE',  ( 207.2707369601997982, 271.6435479931266173, -5.381413637561199614 ) ) ;
#56949 = CARTESIAN_POINT ( 'NONE',  ( 5.871984111234073822, 29.22396284167519198, -10.00000000000000000 ) ) ;
#56950 = CARTESIAN_POINT ( 'NONE',  ( 48.58227110419247907, 77.44677708231240842, -10.00000000000000000 ) ) ;
#56951 = CARTESIAN_POINT ( 'NONE',  ( 42.55642822748762910, 201.5024278399160949, 9.188101187500095079 ) ) ;
#56952 = CARTESIAN_POINT ( 'NONE',  ( 80.03926378114135787, 227.0177522451419350, 5.000000000000046185 ) ) ;
#56953 = ORIENTED_EDGE ( 'NONE', *, *, #88172, .T. ) ;
#56954 = CARTESIAN_POINT ( 'NONE',  ( 82.41745805622035448, 43.86099032315292590, 8.743768202596600148 ) ) ;
#56955 = DIRECTION ( 'NONE',  ( -0.8660254037844387076, -0.4999999999999998890, -0.000000000000000000 ) ) ;
#56956 = CARTESIAN_POINT ( 'NONE',  ( 3.856091543753019213, 173.0333772461660828, 9.188101187500095079 ) ) ;
#56957 = CYLINDRICAL_SURFACE ( 'NONE', #56465, 70.00000000000002842 ) ;
#56958 = CARTESIAN_POINT ( 'NONE',  ( 151.0388915836658725, 269.0399611886400635, -14.24896787280406585 ) ) ;
#56959 = CARTESIAN_POINT ( 'NONE',  ( 186.3242389376556787, 283.0587387869642839, 16.24190855881933260 ) ) ;
#56960 = CARTESIAN_POINT ( 'NONE',  ( 192.6247335881259630, 297.0111699613833594, -13.30158778996737290 ) ) ;
#56961 = APPLICATION_CONTEXT ( 'automotive_design' ) ;
#56962 = CARTESIAN_POINT ( 'NONE',  ( 166.5418805794664934, 264.7512503615053561, 17.71810435351582669 ) ) ;
#56963 = CARTESIAN_POINT ( 'NONE',  ( 164.2297246530060875, 246.1927681183832988, 5.803160395959773510 ) ) ;
#56964 = CARTESIAN_POINT ( 'NONE',  ( 191.0702043019150835, 299.7036936669546776, -8.800021049343948576 ) ) ;
#56965 = CARTESIAN_POINT ( 'NONE',  ( 189.8147415777049218, 301.8782188922952514, -0.5019643756309712934 ) ) ;
#56966 = VERTEX_POINT ( 'NONE', #74026 ) ;
#56967 =( BOUNDED_CURVE ( )  B_SPLINE_CURVE ( 2, ( #90862, #4730, #97438, #11836, #44191, #58885, #28008, #66018, #88892, #43193, #42695, #73626, #21414 ),
 .UNSPECIFIED., .F., .T. ) 
 B_SPLINE_CURVE_WITH_KNOTS ( ( 3, 2, 2, 2, 2, 2, 3 ),
 ( 0.2374999999999999889, 0.2399999999999999911, 0.2449999999999999956, 0.2500000000000000000, 0.2550000000000000044, 0.2600000000000000089, 0.2625000000000000111 ),
 .UNSPECIFIED. ) 
 CURVE ( )  GEOMETRIC_REPRESENTATION_ITEM ( )  RATIONAL_B_SPLINE_CURVE ( ( 0.9755282581475768211, 0.9755282581475768211, 1.000000000000000000, 0.9510565162951535312, 1.000000000000000000, 0.9510565162951535312, 1.000000000000000000, 0.9510565162951535312, 1.000000000000000000, 0.9510565162951535312, 1.000000000000000000, 0.9755282581475768211, 0.9755282581475768211 ) ) 
 REPRESENTATION_ITEM ( '' )  );
#56968 = CARTESIAN_POINT ( 'NONE',  ( 1.754175721758543638, 158.4865022471901739, 1.119607411625061291E-15 ) ) ;
#56969 = PLANE ( 'NONE',  #28813 ) ;
#56970 = CARTESIAN_POINT ( 'NONE',  ( 126.3172359758225554, 252.9244531367911293, -4.594050593750046652 ) ) ;
#56971 = CARTESIAN_POINT ( 'NONE',  ( 27.11361191214091804, 16.44966523072495335, -2.296566073217252530E-15 ) ) ;
#56972 = CARTESIAN_POINT ( 'NONE',  ( 75.24247008381291835, 66.93257772500234637, 12.82047627203052009 ) ) ;
#56973 = CARTESIAN_POINT ( 'NONE',  ( -50.66096862766640641, 31.69950886434491721, -10.00000000000000000 ) ) ;
#56975 = CARTESIAN_POINT ( 'NONE',  ( 185.8594361394618204, 288.5116224014759041, 15.32760917146029200 ) ) ;
#56974 = CARTESIAN_POINT ( 'NONE',  ( 157.2464636617698375, 258.2881309577184652, 18.14284729738657731 ) ) ;
#56976 = CARTESIAN_POINT ( 'NONE',  ( 150.2557873729419669, 270.3963374692353341, -14.33267926939609005 ) ) ;
#56977 = VERTEX_POINT ( 'NONE', #3632 ) ;
#56978 = CARTESIAN_POINT ( 'NONE',  ( 189.6617571741743689, 261.1287600027826556, -4.536318394431146928 ) ) ;
#56979 = CARTESIAN_POINT ( 'NONE',  ( 149.6191398986701415, 271.4990432411842676, -11.66821883946526839 ) ) ;
#56980 = ADVANCED_FACE ( 'NONE', ( #33522 ), #34510, .F. ) ;
#56981 = CARTESIAN_POINT ( 'NONE',  ( 82.35643665848068906, 41.29992738147394959, -3.430024729213354107 ) ) ;
#56982 = CARTESIAN_POINT ( 'NONE',  ( 32.88524308553003550, 19.39040679176984838, -6.890680421881970419E-14 ) ) ;
#56983 = CARTESIAN_POINT ( 'NONE',  ( 81.77662633183955165, 55.53141904912255455, -15.95577929170707066 ) ) ;
#56984 = EDGE_LOOP ( 'NONE', ( #51913, #54362, #74849, #21571, #26996, #87856, #21177, #26109, #100288, #61769, #14274, #92853, #27887, #87648, #67709, #50932, #13347, #1875, #13683, #8963, #18796, #17836 ) ) ;
#56985 = CARTESIAN_POINT ( 'NONE',  ( 189.0176971330334368, 265.7359912712865366, 10.99843924538786233 ) ) ;
#56986 = VECTOR ( 'NONE', #42052, 1000.000000000000000 ) ;
#56987 = CARTESIAN_POINT ( 'NONE',  ( 195.2495212664957194, 275.1290853193528392, -16.26662379558266380 ) ) ;
#56988 = CARTESIAN_POINT ( 'NONE',  ( 165.6504798027754646, 269.1482514364597591, -16.93297765974685021 ) ) ;
#56989 = CARTESIAN_POINT ( 'NONE',  ( 71.92106615665200309, 72.60175000959986846, 1.189886861346824753 ) ) ;
#56990 = B_SPLINE_SURFACE_WITH_KNOTS ( 'NONE', 3, 1, ( 
 ( #85105, #55642 ),
 ( #39943, #100287 ),
 ( #48061, #69861 ),
 ( #87146, #76962 ),
 ( #473, #93199 ),
 ( #31852, #15654 ),
 ( #30872, #71389 ),
 ( #85625, #86628 ),
 ( #94703, #31362 ),
 ( #55150, #94209 ),
 ( #61756, #77982 ),
 ( #62246, #23753 ),
 ( #16170, #92705 ),
 ( #47067, #973 ),
 ( #70879, #17162 ),
 ( #86136, #9075 ),
 ( #23256, #70363 ),
 ( #8577, #93710 ),
 ( #38454, #39442 ),
 ( #62753, #69367 ),
 ( #1978, #63268 ),
 ( #16665, #47560 ),
 ( #78487, #24763 ),
 ( #79003, #9590 ),
 ( #32864, #63770 ),
 ( #25265, #56148 ),
 ( #17677, #90980 ),
 ( #25788, #12965 ),
 ( #98560, #12457 ),
 ( #36722, #98051 ),
 ( #89500, #74766 ),
 ( #44321, #49078 ),
 ( #43328, #43826 ),
 ( #87649, #97089 ) ),
 .UNSPECIFIED., .T., .F., .F.,
 ( 4, 2, 2, 2, 2, 2, 2, 2, 2, 2, 2, 2, 2, 2, 2, 2, 4 ),
 ( 2, 2 ),
 ( 0.000000000000000000, 0.06250000000000000000, 0.1250000000000000000, 0.1875000000000000000, 0.2500000000000000000, 0.3125000000000000000, 0.3750000000000000000, 0.4375000000000000000, 0.5000000000000000000, 0.5625000000000000000, 0.6250000000000000000, 0.6875000000000000000, 0.7500000000000000000, 0.8125000000000000000, 0.8750000000000000000, 0.9375000000000000000, 1.000000000000000000 ),
 ( 0.000000000000000000, 1.000000000000000000 ),
 .UNSPECIFIED. ) ;
#56991 = CARTESIAN_POINT ( 'NONE',  ( 197.9494925845387456, 271.7022998954425361, 12.11704210009641969 ) ) ;
#56992 = CARTESIAN_POINT ( 'NONE',  ( 155.8168635700358493, 261.2859049548226267, 17.07611989262474239 ) ) ;
#56993 = LINE ( 'NONE', #72229, #9706 ) ;
#56994 = CARTESIAN_POINT ( 'NONE',  ( 192.6797324865049745, 296.9159090750308110, 12.42053959885222625 ) ) ;
#56995 = ORIENTED_EDGE ( 'NONE', *, *, #47659, .T. ) ;
#56996 = CARTESIAN_POINT ( 'NONE',  ( 190.5716289146250517, 280.7215959158480132, 16.63595715464797564 ) ) ;
#56997 = CARTESIAN_POINT ( 'NONE',  ( 8.323093432028223049, 20.50829794293878905, -10.00000000000000355 ) ) ;
#56998 = FACE_OUTER_BOUND ( 'NONE', #88594, .T. ) ;
#56999 = ORIENTED_EDGE ( 'NONE', *, *, #64382, .T. ) ;
#57000 = CARTESIAN_POINT ( 'NONE',  ( 164.6784601142441318, 280.3721143660208099, 12.61989482521711636 ) ) ;
#57001 = EDGE_CURVE ( 'NONE', #59397, #9269, #1161, .T. ) ;
#57002 = CARTESIAN_POINT ( 'NONE',  ( 147.8308140999695866, 274.5965143850199865, -7.866624397492971710 ) ) ;
#57003 = CARTESIAN_POINT ( 'NONE',  ( 110.0000000000000000, -8.000000000000000000, -9.212605237762131694 ) ) ;
#57004 = B_SPLINE_CURVE_WITH_KNOTS ( 'NONE', 3,
 ( #54666, #78002, #16687, #38974 ),
 .UNSPECIFIED., .F., .F.,
 ( 4, 4 ),
 ( 0.001918581007240343240, 0.009849387959984160987 ),
 .UNSPECIFIED. ) ;
#57005 = VERTEX_POINT ( 'NONE', #89277 ) ;
#57006 = DIRECTION ( 'NONE',  ( -0.7352104281592222179, 0.6778389383370750920, 0.000000000000000000 ) ) ;
#57007 = CARTESIAN_POINT ( 'NONE',  ( 159.7080606971873920, 255.4347751002972871, 16.25053020610463861 ) ) ;
#57008 = CARTESIAN_POINT ( 'NONE',  ( 151.0036289208911171, 269.1010379121764799, 14.24595189915657478 ) ) ;
#57009 = DIRECTION ( 'NONE',  ( 0.06958655048003267729, -0.1205274409548735270, -0.9902680687415703620 ) ) ;
#57010 = CARTESIAN_POINT ( 'NONE',  ( 81.95257519206566599, 50.72568879219577553, -14.43282536261877524 ) ) ;
#57011 = CARTESIAN_POINT ( 'NONE',  ( 73.27328646083023500, 70.16270934360544231, -9.274526489422589393 ) ) ;
#57012 = CARTESIAN_POINT ( 'NONE',  ( 189.5797355942488025, 300.2297304461512795, 3.265020536630226733 ) ) ;
#57013 = CARTESIAN_POINT ( 'NONE',  ( 155.5066938333533528, 261.3015006940112244, -18.40036130547566273 ) ) ;
#57014 = ORIENTED_EDGE ( 'NONE', *, *, #90829, .F. ) ;
#57015 = ORIENTED_EDGE ( 'NONE', *, *, #87504, .T. ) ;
#57016 = CARTESIAN_POINT ( 'NONE',  ( 179.0589298886251868, 259.9615930511803867, 12.73898565628910085 ) ) ;
#57017 = VERTEX_POINT ( 'NONE', #65411 ) ;
#57018 = LINE ( 'NONE', #35226, #35270 ) ;
#57019 = ORIENTED_EDGE ( 'NONE', *, *, #95739, .T. ) ;
#57020 = CARTESIAN_POINT ( 'NONE',  ( 88.33249819345715537, 44.18347584668511985, -0.1457987645956864697 ) ) ;
#57021 = CARTESIAN_POINT ( 'NONE',  ( 79.20956237034324943, 53.22039654841660195, 15.72328171560790189 ) ) ;
#57022 = EDGE_LOOP ( 'NONE', ( #5767, #71127, #11825, #22153 ) ) ;
#57023 = CARTESIAN_POINT ( 'NONE',  ( 82.33552489548483777, 41.24829604067362254, 3.267574154620816795 ) ) ;
#57024 = CARTESIAN_POINT ( 'NONE',  ( 151.3198218389669023, 269.0401608486226337, 14.23401639979100430 ) ) ;
#57025 = CARTESIAN_POINT ( 'NONE',  ( 158.6150988756866127, 274.9578748594535682, -12.59651497174430013 ) ) ;
#57026 = CARTESIAN_POINT ( 'NONE',  ( 193.1444937042664094, 296.1109190324805240, -12.15243020627156767 ) ) ;
#57027 = CARTESIAN_POINT ( 'NONE',  ( 153.4495116231415750, 264.8646448025247082, -16.73555355292144498 ) ) ;
#57028 = CARTESIAN_POINT ( 'NONE',  ( 77.71695824120644147, 49.45779813244274692, 15.33409790704233799 ) ) ;
#57029 = CARTESIAN_POINT ( 'NONE',  ( 202.0032530003042552, 275.2598398602717680, -14.36878956143956643 ) ) ;
#57030 = CARTESIAN_POINT ( 'NONE',  ( 138.3604885211411499, 256.8149278399160949, 9.188101187500093303 ) ) ;
#57031 = CARTESIAN_POINT ( 'NONE',  ( 70.73063444094617580, 61.07312936796083847, -14.44582943987787260 ) ) ;
#57032 = CARTESIAN_POINT ( 'NONE',  ( 45.41683807177152232, 29.14754757982093736, -5.678558825948276656 ) ) ;
#57033 = ORIENTED_EDGE ( 'NONE', *, *, #33961, .T. ) ;
#57035 = VERTEX_POINT ( 'NONE', #88276 ) ;
#57034 = DIRECTION ( 'NONE',  ( 0.5000000000000014433, -0.8660254037844379305, 0.000000000000000000 ) ) ;
#57036 = CARTESIAN_POINT ( 'NONE',  ( -16.20514820903670028, 105.3874431953180135, 11.89003404754207160 ) ) ;
#57037 = EDGE_CURVE ( 'NONE', #6693, #20542, #4107, .T. ) ;
#57038 = CARTESIAN_POINT ( 'NONE',  ( 162.8996025780091941, 248.4966071325470125, 11.23567065566008516 ) ) ;
#57039 = DIRECTION ( 'NONE',  ( -0.000000000000000000, -0.000000000000000000, 1.000000000000000000 ) ) ;
#57040 = DIRECTION ( 'NONE',  ( -0.1710100716628374096, 0.2961981327260301833, 0.9396926207859057634 ) ) ;
#57041 = CARTESIAN_POINT ( 'NONE',  ( 153.2891369107873345, 276.9440725079709296, 6.996015511654989361 ) ) ;
#57042 = CARTESIAN_POINT ( 'NONE',  ( 200.6985908945154335, 283.0268388936558495, -17.74173253065502820 ) ) ;
#57043 = DIRECTION ( 'NONE',  ( 1.000000000000000000, 0.000000000000000000, 0.000000000000000000 ) ) ;
#57044 = B_SPLINE_CURVE_WITH_KNOTS ( 'NONE', 3,
 ( #27594, #80838, #59949, #58458, #81815, #97984, #73195, #57972, #43754, #5278, #28562, #88956, #19511, #20997, #81322, #90920, #11894, #35670, #13384, #51878, #42751, #73685 ),
 .UNSPECIFIED., .F., .F.,
 ( 4, 2, 2, 2, 2, 2, 2, 2, 2, 2, 4 ),
 ( 0.0002052773884520107852, 0.0006292189728194242651, 0.0007352043689112620429, 0.0007881970669571040618, 0.0008146934159800252881, 0.0008411897650029466229, 0.0008941824630486570197, 0.0009471751610943675249, 0.001053160557185625797, 0.001477102141550394989, 0.001901043725915164398 ),
 .UNSPECIFIED. ) ;
#57045 = CARTESIAN_POINT ( 'NONE',  ( 171.5253789402676716, 280.0391282839272549, 13.83596625797474644 ) ) ;
#57046 = CARTESIAN_POINT ( 'NONE',  ( -19.65312891409030271, 93.06504152958497400, 177.5919119679930134 ) ) ;
#57047 = LINE ( 'NONE', #1870, #95057 ) ;
#57048 = EDGE_LOOP ( 'NONE', ( #44769, #22478, #28536, #56405, #56280 ) ) ;
#57049 = CARTESIAN_POINT ( 'NONE',  ( 36.94473716931751284, 21.73415679381824361, -6.890680421881970419E-14 ) ) ;
#57050 = CARTESIAN_POINT ( 'NONE',  ( 66.22544434996629548, 69.36168404795429865, 0.1681498104656474202 ) ) ;
#57051 = ORIENTED_EDGE ( 'NONE', *, *, #80736, .T. ) ;
#57052 = CARTESIAN_POINT ( 'NONE',  ( 162.8901731922526039, 277.0746486824075419, 12.89396308544769276 ) ) ;
#57053 = EDGE_CURVE ( 'NONE', #42536, #73611, #61014, .T. ) ;
#57054 = CARTESIAN_POINT ( 'NONE',  ( 200.9393373695271805, 267.7870988455974270, -2.797138418476491584 ) ) ;
#57055 = CARTESIAN_POINT ( 'NONE',  ( 151.7482317558875593, 267.8113479705027657, -16.53675092648768086 ) ) ;
#57056 = CARTESIAN_POINT ( 'NONE',  ( 190.1190668544949460, 301.3511120508678118, 4.410340539513557090 ) ) ;
#57057 = CARTESIAN_POINT ( 'NONE',  ( 202.6551236945213361, 279.6380246773706517, 15.55476940527561425 ) ) ;
#57059 = CARTESIAN_POINT ( 'NONE',  ( 87.99156517466562377, 44.25173956186072388, 2.816193757564026789 ) ) ;
#57058 = CARTESIAN_POINT ( 'NONE',  ( 161.4341193711443054, 281.4014545508878768, -6.923656337983120856 ) ) ;
#57060 = CIRCLE ( 'NONE', #34368, 10.00000000000011369 ) ;
#57061 = DIRECTION ( 'NONE',  ( 0.5000000000000001110, -0.8660254037844385966, 2.065951763267645480E-16 ) ) ;
#57062 = ORIENTED_EDGE ( 'NONE', *, *, #41945, .F. ) ;
#57063 = CARTESIAN_POINT ( 'NONE',  ( 74.05886703568846485, 66.92701276778755926, 12.81588082616969970 ) ) ;
#57064 = DIRECTION ( 'NONE',  ( 1.000000000000000000, 0.000000000000000000, -0.000000000000000000 ) ) ;
#57065 = VECTOR ( 'NONE', #69822, 1000.000000000000114 ) ;
#57066 = PLANE ( 'NONE',  #67801 ) ;
#57067 = CARTESIAN_POINT ( 'NONE',  ( -48.34856483818852979, 28.93234566034054822, 10.00000000000000000 ) ) ;
#57068 = CARTESIAN_POINT ( 'NONE',  ( 80.69702293635484125, 43.52605551489090630, -9.543807321698503543 ) ) ;
#57069 = FACE_OUTER_BOUND ( 'NONE', #9313, .T. ) ;
#57070 = CARTESIAN_POINT ( 'NONE',  ( 162.8042930031641049, 248.6616881586264469, 11.14389129512055554 ) ) ;
#57071 = CARTESIAN_POINT ( 'NONE',  ( -3.180017766230537557, 156.7202760586659451, -5.415160957724236172E-17 ) ) ;
#57072 = CARTESIAN_POINT ( 'NONE',  ( 109.7008941843561445, 224.9548013555409796, -4.594050593750042211 ) ) ;
#57073 = CARTESIAN_POINT ( 'NONE',  ( 155.0304386007204016, 262.1263989543018056, -17.12961552904782181 ) ) ;
#57074 = CARTESIAN_POINT ( 'NONE',  ( 88.15573124791052351, 44.39703741701313078, -4.524867680024764915 ) ) ;
#57075 = CARTESIAN_POINT ( 'NONE',  ( 185.9470091674525349, 276.4697974381609242, -17.76503501984419131 ) ) ;
#57076 = PLANE ( 'NONE',  #2751 ) ;
#57077 = AXIS2_PLACEMENT_3D ( 'NONE', #66821, #67831, #82583 ) ;
#57078 = CARTESIAN_POINT ( 'NONE',  ( 194.3413770922408617, 282.8930799310762723, 17.82077676852630077 ) ) ;
#57079 = DIRECTION ( 'NONE',  ( 0.000000000000000000, 0.000000000000000000, 1.000000000000000000 ) ) ;
#57080 = CARTESIAN_POINT ( 'NONE',  ( 163.9292450293648074, 284.3952669320320865, 5.923242389932828367 ) ) ;
#57082 = CARTESIAN_POINT ( 'NONE',  ( 208.2874212803407090, 269.8825990953837390, -1.143705256421198690 ) ) ;
#57081 = DIRECTION ( 'NONE',  ( -0.8660254037844387076, -0.4999999999999998890, -0.000000000000000000 ) ) ;
#57083 = CARTESIAN_POINT ( 'NONE',  ( 162.0042060562265931, 250.0474794011949768, 13.08583584746748940 ) ) ;
#57084 = PRESENTATION_STYLE_ASSIGNMENT (( #24693 ) ) ;
#57085 = CARTESIAN_POINT ( 'NONE',  ( 74.41491511734228936, 56.32654587899735077, -16.10167882689214025 ) ) ;
#57086 = CARTESIAN_POINT ( 'NONE',  ( 83.53204454370724363, 52.39401912150450613, -15.17729711222452416 ) ) ;
#57087 = CARTESIAN_POINT ( 'NONE',  ( 73.30631488696991482, 69.89686749726290316, 9.630897265116471928 ) ) ;
#57088 = CARTESIAN_POINT ( 'NONE',  ( 52.43496435911014686, 191.8923013555410080, 4.594050593750050204 ) ) ;
#57089 = CARTESIAN_POINT ( 'NONE',  ( -22.42236680055709641, 157.8615022471902591, 0.000000000000000000 ) ) ;
#57090 = CARTESIAN_POINT ( 'NONE',  ( 83.63833477162944519, 231.3464784336661637, 1.353441290958777327E-15 ) ) ;
#57091 = CARTESIAN_POINT ( 'NONE',  ( 161.5083988044524119, 250.9062427520286178, -14.53522982831775856 ) ) ;
#57092 = CARTESIAN_POINT ( 'NONE',  ( 163.2699323312932904, 258.1949546823035462, 15.87757944056416015 ) ) ;
#57094 = DIRECTION ( 'NONE',  ( -0.9292718480896766664, -0.3693965786901617920, 0.000000000000000000 ) ) ;
#57093 = CARTESIAN_POINT ( 'NONE',  ( 84.13355168651825977, 43.02656781755162996, -6.806181843193294334 ) ) ;
#57095 = CARTESIAN_POINT ( 'NONE',  ( 173.5451919912859182, 268.4384502063331297, -16.29429379470302308 ) ) ;
#57096 = ADVANCED_FACE ( 'NONE', ( #79663 ), #26920, .T. ) ;
#57097 = CARTESIAN_POINT ( 'NONE',  ( 78.58115897284257301, 49.46449540821208757, -15.15569606598211116 ) ) ;
#57098 = CARTESIAN_POINT ( 'NONE',  ( 76.15623579681398780, 64.25551128800826461, 14.96979677531604480 ) ) ;
#57099 = ORIENTED_EDGE ( 'NONE', *, *, #65428, .T. ) ;
#57100 = CARTESIAN_POINT ( 'NONE',  ( 18.92609651878039756, 19.43085787977762280, -9.188101187500008038 ) ) ;
#57101 = CARTESIAN_POINT ( 'NONE',  ( 84.82981389336303835, 207.5327760586659451, 1.948934522072302763E-15 ) ) ;
#57102 = CARTESIAN_POINT ( 'NONE',  ( 88.52455635939595879, 233.4637435831425023, 2.679491924311251605 ) ) ;
#57103 = CYLINDRICAL_SURFACE ( 'NONE', #53927, 17.82106496071139645 ) ;
#57104 = CARTESIAN_POINT ( 'NONE',  ( 147.1603453755519695, 275.7578002805973370, -5.230822882238410187 ) ) ;
#57105 = CARTESIAN_POINT ( 'NONE',  ( 199.7408883951190717, 281.7026737086815160, 17.40441678530665470 ) ) ;
#57106 = EDGE_CURVE ( 'NONE', #100024, #67772, #25448, .T. ) ;
#57107 = B_SPLINE_CURVE_WITH_KNOTS ( 'NONE', 3,
 ( #2762, #18454, #34628, #4745, #18957, #33653, #66034, #57927, #96981, #26549, #26050, #80282, #35629, #72670, #10848, #27550, #43209, #80793 ),
 .UNSPECIFIED., .F., .F.,
 ( 4, 2, 2, 2, 2, 2, 2, 2, 4 ),
 ( 0.000000000000000000, 0.0003250734011923252882, 0.0006501468023846505764, 0.0009752202035769758645, 0.001300293604769301153, 0.001625367005961621562, 0.001950440407153941971, 0.002275513808346262164, 0.002600587209538582790 ),
 .UNSPECIFIED. ) ;
#57108 = CARTESIAN_POINT ( 'NONE',  ( 70.34454795187326681, 61.29844696719631969, 14.78467410917921043 ) ) ;
#57109 = CARTESIAN_POINT ( 'NONE',  ( 193.6538297768585153, 294.3106073703939387, 13.99927879369582406 ) ) ;
#57110 = CARTESIAN_POINT ( 'NONE',  ( 191.2104420009116836, 280.2857515794617598, 17.80337293751487593 ) ) ;
#57111 = CARTESIAN_POINT ( 'NONE',  ( 121.4100190113084636, 234.2365022471901739, -10.00000000000009059 ) ) ;
#57112 = CARTESIAN_POINT ( 'NONE',  ( 205.0716081116550527, 275.4525508911965517, -12.57761053684872188 ) ) ;
#57113 = DIRECTION ( 'NONE',  ( 0.000000000000000000, 0.000000000000000000, 1.000000000000000000 ) ) ;
#57114 = CARTESIAN_POINT ( 'NONE',  ( 165.6167443952357416, 246.9696370225337603, -1.864274362100295734 ) ) ;
#57115 = ORIENTED_EDGE ( 'NONE', *, *, #25022, .F. ) ;
#57116 = CARTESIAN_POINT ( 'NONE',  ( 163.0171530587457767, 248.2930037274571191, 9.677214176418313940 ) ) ;
#57117 = CARTESIAN_POINT ( 'NONE',  ( 178.0315741628076012, 287.5935043698759728, -13.06113257055532451 ) ) ;
#57118 = EDGE_CURVE ( 'NONE', #97948, #96856, #42591, .T. ) ;
#57119 = CARTESIAN_POINT ( 'NONE',  ( 72.67454777811306599, 57.54427597285661022, -16.30613687664699896 ) ) ;
#57120 = CARTESIAN_POINT ( 'NONE',  ( 77.26942776676457925, 63.03888086361324383, -15.26992705839576381 ) ) ;
#57121 = ORIENTED_EDGE ( 'NONE', *, *, #73874, .F. ) ;
#57122 = CARTESIAN_POINT ( 'NONE',  ( 189.6918891073893008, 290.1382577116506241, 14.45894197730551589 ) ) ;
#57123 = CARTESIAN_POINT ( 'NONE',  ( 172.7264208856190919, 290.8582626858774347, 2.771863430787652849 ) ) ;
#57124 = CARTESIAN_POINT ( 'NONE',  ( 158.1337577521140929, 257.6225849586518279, -16.81478466335610022 ) ) ;
#57125 = CARTESIAN_POINT ( 'NONE',  ( 201.4617167010348737, 281.7050662241970826, -17.43131506460443703 ) ) ;
#57126 = ORIENTED_EDGE ( 'NONE', *, *, #74547, .T. ) ;
#57127 = CARTESIAN_POINT ( 'NONE',  ( 41.30863684418880410, 35.80066082961425167, 10.00000000000000533 ) ) ;
#57128 = CARTESIAN_POINT ( 'NONE',  ( 36.43182450750799006, 23.96004757982092315, -5.678558825948275768 ) ) ;
#57129 = CARTESIAN_POINT ( 'NONE',  ( 79.76833976871120058, 44.78188551475517443, 11.36349263846995328 ) ) ;
#57130 = CARTESIAN_POINT ( 'NONE',  ( 84.29414043670328738, 48.06250324931478701, -12.02348180207343020 ) ) ;
#57131 = VECTOR ( 'NONE', #11778, 1000.000000000000114 ) ;
#57132 = CARTESIAN_POINT ( 'NONE',  ( 156.2224770818481545, 267.4677849582849376, -16.91854127892884208 ) ) ;
#57133 = EDGE_CURVE ( 'NONE', #86000, #92701, #98424, .T. ) ;
#57134 = PLANE ( 'NONE',  #56149 ) ;
#57135 = ORIENTED_EDGE ( 'NONE', *, *, #44414, .F. ) ;
#57136 = VERTEX_POINT ( 'NONE', #21799 ) ;
#57137 = CARTESIAN_POINT ( 'NONE',  ( 198.1847055346428590, 286.9842163890704683, 16.95145238430053070 ) ) ;
#57139 = CARTESIAN_POINT ( 'NONE',  ( 148.1004780136491377, 274.1294427855589788, -7.811560775291159331 ) ) ;
#57138 = CARTESIAN_POINT ( 'NONE',  ( 204.3951397407346064, 276.6242284793436852, 14.79595971842109137 ) ) ;
#57140 = CARTESIAN_POINT ( 'NONE',  ( -13.11024591527734628, 0.000000000000000000, -32.50000000000000000 ) ) ;
#57141 = CARTESIAN_POINT ( 'NONE',  ( 193.7999837595647250, 294.9755769528473479, 15.24609078262870199 ) ) ;
#57142 = CARTESIAN_POINT ( 'NONE',  ( 153.2685960449373681, 269.0240501674685447, -15.70450447371167790 ) ) ;
#57143 = CARTESIAN_POINT ( 'NONE',  ( 204.9463377925012253, 275.6695254486514841, -14.15865086131798378 ) ) ;
#57144 = CARTESIAN_POINT ( 'NONE',  ( 164.6993295494617939, 245.3793885782390589, 4.576454266300281404 ) ) ;
#57145 = CARTESIAN_POINT ( 'NONE',  ( 166.1014715941954591, 265.5448861341674274, 16.58231607936238916 ) ) ;
#57146 = AXIS2_PLACEMENT_3D ( 'NONE', #36181, #97047, #51900 ) ;
#57147 = DIRECTION ( 'NONE',  ( 0.06958655048003267729, -0.1205274409548735270, -0.9902680687415703620 ) ) ;
#57148 = CARTESIAN_POINT ( 'NONE',  ( 81.20281187136818346, 223.8149278399160664, 9.188101187500093303 ) ) ;
#57149 = ORIENTED_EDGE ( 'NONE', *, *, #100044, .F. ) ;
#57150 = DIRECTION ( 'NONE',  ( -0.000000000000000000, -0.000000000000000000, -1.000000000000000000 ) ) ;
#57151 = ORIENTED_EDGE ( 'NONE', *, *, #25902, .T. ) ;
#57152 = ORIENTED_EDGE ( 'NONE', *, *, #39324, .T. ) ;
#57153 = ORIENTED_EDGE ( 'NONE', *, *, #24101, .F. ) ;
#57154 = EDGE_CURVE ( 'NONE', #16006, #31346, #91258, .T. ) ;
#57155 = CARTESIAN_POINT ( 'NONE',  ( 80.32594557099248789, 44.72898953253431387, -11.70945978744232363 ) ) ;
#57156 = CARTESIAN_POINT ( 'NONE',  ( -77.42978507651396569, 55.80833764325424085, 10.00000000000000000 ) ) ;
#57157 = CARTESIAN_POINT ( 'NONE',  ( 164.1377787084186934, 249.9599717614572114, 10.21025470079037056 ) ) ;
#57158 = CARTESIAN_POINT ( 'NONE',  ( 206.8659638600981623, 272.3446355680395641, -10.26115277030573125 ) ) ;
#57159 = CARTESIAN_POINT ( 'NONE',  ( 207.0601855587586329, 271.2283032176189295, -4.679519923957272454 ) ) ;
#57160 = CARTESIAN_POINT ( 'NONE',  ( 97.65764163903753570, 221.0643266524160424, 9.188101187500095079 ) ) ;
#57161 = ORIENTED_EDGE ( 'NONE', *, *, #67829, .T. ) ;
#57162 = EDGE_CURVE ( 'NONE', #41308, #61729, #51392, .T. ) ;
#57163 = VERTEX_POINT ( 'NONE', #32393 ) ;
#57164 = CARTESIAN_POINT ( 'NONE',  ( -6.281727404287059890, 25.63055774385195917, -10.00000000000000000 ) ) ;
#57165 = VERTEX_POINT ( 'NONE', #38979 ) ;
#57166 = EDGE_CURVE ( 'NONE', #98884, #76355, #47583, .T. ) ;
#57167 = EDGE_CURVE ( 'NONE', #16883, #35964, #55665, .T. ) ;
#57168 = DIRECTION ( 'NONE',  ( 1.000000000000000000, -2.478176394252581023E-14, 0.000000000000000000 ) ) ;
#57169 = CARTESIAN_POINT ( 'NONE',  ( -30.04356256989597185, 94.88921800892812541, 43.89948692389422291 ) ) ;
#57171 = DIRECTION ( 'NONE',  ( -1.082076799516502080E-16, 0.000000000000000000, -1.000000000000000000 ) ) ;
#57170 = CARTESIAN_POINT ( 'NONE',  ( 136.3040252829181327, 243.3768266524159856, 9.188101187500098632 ) ) ;
#57172 = CARTESIAN_POINT ( 'NONE',  ( -1.367124174595798713, 160.0177522451418213, 5.000000000000051514 ) ) ;
#57173 = CARTESIAN_POINT ( 'NONE',  ( 87.93413682123004094, 44.35120838780621000, 4.768703809423659123 ) ) ;
#57174 = EDGE_LOOP ( 'NONE', ( #16778, #35943, #193, #5311, #79168, #58306, #73469, #61757, #9819, #81629, #40177, #95563, #94218, #28601, #99621, #16169, #67371, #54437, #83726, #95351, #19100, #43855, #7403, #97930, #17986, #50456, #40787, #63227, #48291, #9085, #62468, #88989, #99052, #25889 ) ) ;
#57175 = CARTESIAN_POINT ( 'NONE',  ( 157.0858749576330524, 258.5662787524049122, 18.43576942457294976 ) ) ;
#57176 = EDGE_CURVE ( 'NONE', #59093, #53284, #33924, .T. ) ;
#57177 = CARTESIAN_POINT ( 'NONE',  ( 160.4962995477943650, 275.9333967852908813, 14.18032076246626794 ) ) ;
#57178 = FACE_OUTER_BOUND ( 'NONE', #98167, .T. ) ;
#57179 = EDGE_CURVE ( 'NONE', #29884, #54945, #39966, .T. ) ;
#57180 = CARTESIAN_POINT ( 'NONE',  ( 80.72100776821309864, 43.43651575216833294, 9.420844811674243147 ) ) ;
#57181 = CARTESIAN_POINT ( 'NONE',  ( 174.5944895219865316, 283.7845549098777838, 13.67518389082495034 ) ) ;
#57182 = CARTESIAN_POINT ( 'NONE',  ( -48.47243291925848752, 30.64988553008148031, -10.00000000000000000 ) ) ;
#57183 = CARTESIAN_POINT ( 'NONE',  ( 77.58957552442460326, 61.75793702469097468, 15.67560070342385892 ) ) ;
#57184 = CARTESIAN_POINT ( 'NONE',  ( -19.65312891409030271, 93.06504152958497400, 59.99999999999999289 ) ) ;
#57185 = CARTESIAN_POINT ( 'NONE',  ( 161.1990332043106946, 251.4420796895884394, 14.26998817770995487 ) ) ;
#57186 = CARTESIAN_POINT ( 'NONE',  ( 86.40663024008399873, 45.92652238299617551, 8.627225980297390961 ) ) ;
#57187 = CARTESIAN_POINT ( 'NONE',  ( 16.27523747222386774, 28.13478043621388025, 8.090169943749478065 ) ) ;
#57188 = CARTESIAN_POINT ( 'NONE',  ( 83.24496396852070745, 52.35953078789503934, 14.85683903734107147 ) ) ;
#57189 = CARTESIAN_POINT ( 'NONE',  ( 175.9704269209120753, 290.3320350542924757, -6.214979091763118468 ) ) ;
#57190 = CARTESIAN_POINT ( 'NONE',  ( 195.8285188278500470, 273.2427770020486832, 15.26130794574777383 ) ) ;
#57191 = CARTESIAN_POINT ( 'NONE',  ( 27.78891098193510345, 37.81751292744058190, -6.180339887498951690 ) ) ;
#57192 = VECTOR ( 'NONE', #89566, 1000.000000000000114 ) ;
#57193 = CARTESIAN_POINT ( 'NONE',  ( 73.88036207731340710, 64.05502917650269978, -13.99130931570255143 ) ) ;
#57195 = CARTESIAN_POINT ( 'NONE',  ( 74.19373413002220730, 55.14634173073913814, 16.60422751163261879 ) ) ;
#57194 = CARTESIAN_POINT ( 'NONE',  ( 180.7942833579522812, 266.7097690628117448, -16.23795806611159520 ) ) ;
#57196 = CARTESIAN_POINT ( 'NONE',  ( 74.41009865654255862, 213.7677522451418497, 10.00000000000009592 ) ) ;
#57197 = CARTESIAN_POINT ( 'NONE',  ( 29.87413333957346140, 40.18080186712595747, 3.090169943749475401 ) ) ;
#57198 = CARTESIAN_POINT ( 'NONE',  ( 152.7314557461996571, 266.1083540640618708, 17.39314074348802208 ) ) ;
#57199 = CARTESIAN_POINT ( 'NONE',  ( 155.3250150347760723, 261.6161776038049425, -18.57420904020362684 ) ) ;
#57200 = DIRECTION ( 'NONE',  ( 0.2588190451025447203, 0.9659258262890618729, 2.299878683274449355E-16 ) ) ;
#57201 = CARTESIAN_POINT ( 'NONE',  ( 160.8072101477444846, 273.0293901340574507, -14.97921187206499027 ) ) ;
#57202 = CARTESIAN_POINT ( 'NONE',  ( 84.10129132598619606, 43.29379949965990448, -6.284272029605274312 ) ) ;
#57203 = CIRCLE ( 'NONE', #28213, 70.00000000000001421 ) ;
#57204 = CARTESIAN_POINT ( 'NONE',  ( 8.781437479894508513, 182.0024278399160949, 9.188101187500095079 ) ) ;
#57205 = VECTOR ( 'NONE', #97515, 1000.000000000000000 ) ;
#57206 = CARTESIAN_POINT ( 'NONE',  ( 82.79565879694258967, 50.14544268168955199, 13.93210848370866373 ) ) ;
#57207 = ORIENTED_EDGE ( 'NONE', *, *, #9039, .T. ) ;
#57209 = CARTESIAN_POINT ( 'NONE',  ( 87.13721241349922764, 46.29175778497492644, 8.541777034186077699 ) ) ;
#57208 = AXIS2_PLACEMENT_3D ( 'NONE', #86360, #62472, #16890 ) ;
#57210 = CARTESIAN_POINT ( 'NONE',  ( 37.46976539259314620, 180.8932355074535678, -2.679491924311248496 ) ) ;
#57211 = CARTESIAN_POINT ( 'NONE',  ( 71.92697733641804803, 72.63665773354594535, -0.7151800694983956319 ) ) ;
#57212 = CARTESIAN_POINT ( 'NONE',  ( 41.04123086662985997, 188.3768266524159856, -9.188101187500093303 ) ) ;
#57213 = EDGE_CURVE ( 'NONE', #86151, #72984, #85654, .T. ) ;
#57214 = CARTESIAN_POINT ( 'NONE',  ( 87.15721324309708962, 46.06501070407752252, 8.877681887861816890 ) ) ;
#57215 = CARTESIAN_POINT ( 'NONE',  ( 190.9498149295421570, 299.9122141765958531, -5.138500224925297566 ) ) ;
#57216 = CARTESIAN_POINT ( 'NONE',  ( 32.98506340464173547, 40.81751292744058901, -6.180339887498951690 ) ) ;
#57217 = CARTESIAN_POINT ( 'NONE',  ( 32.30839531297598910, 123.0650415295850593, 40.00000000000000000 ) ) ;
#57218 = CARTESIAN_POINT ( 'NONE',  ( 191.5324528500417216, 298.9030556958743432, -8.286652526617016790 ) ) ;
#57219 = CARTESIAN_POINT ( 'NONE',  ( -19.65312891409030271, 93.06504152958497400, 177.5919119679930134 ) ) ;
#57220 = CARTESIAN_POINT ( 'NONE',  ( 182.5821340850675938, 280.3201940986122054, -16.08842446693554606 ) ) ;
#57221 = DIRECTION ( 'NONE',  ( -0.000000000000000000, 0.000000000000000000, 1.000000000000000000 ) ) ;
#57222 = B_SPLINE_SURFACE_WITH_KNOTS ( 'NONE', 3, 1, ( 
 ( #23703, #31313 ),
 ( #7511, #75957 ),
 ( #62202, #29824 ),
 ( #77937, #23210 ),
 ( #76442, #61707 ),
 ( #30325, #7017 ),
 ( #39397, #54598 ),
 ( #37902, #61213 ),
 ( #92179, #53608 ),
 ( #85581, #70314 ),
 ( #16124, #927 ),
 ( #15105, #72852 ),
 ( #17114, #48012 ),
 ( #88088, #18637 ),
 ( #55107, #10034 ),
 ( #78955, #24715 ),
 ( #87603, #25740 ),
 ( #56102, #1439 ),
 ( #3444, #70829 ),
 ( #56619, #40404 ),
 ( #87093, #71341 ),
 ( #32819, #17630 ),
 ( #72352, #86581 ),
 ( #63220, #94162 ),
 ( #32319, #18129 ),
 ( #49030, #78441 ),
 ( #2956, #48533 ),
 ( #79964, #80471 ),
 ( #10532, #9022 ),
 ( #55598, #9544 ),
 ( #1933, #2443 ),
 ( #49516, #95171 ),
 ( #63724, #33321 ),
 ( #94661, #25217 ) ),
 .UNSPECIFIED., .T., .F., .F.,
 ( 4, 2, 2, 2, 2, 2, 2, 2, 2, 2, 2, 2, 2, 2, 2, 2, 4 ),
 ( 2, 2 ),
 ( 0.000000000000000000, 0.06250000000000000000, 0.1250000000000000000, 0.1875000000000000000, 0.2500000000000000000, 0.3125000000000000000, 0.3750000000000000000, 0.4375000000000000000, 0.5000000000000000000, 0.5625000000000000000, 0.6250000000000000000, 0.6875000000000000000, 0.7500000000000000000, 0.8125000000000000000, 0.8750000000000000000, 0.9375000000000000000, 1.000000000000000000 ),
 ( 0.000000000000000000, 1.000000000000000000 ),
 .UNSPECIFIED. ) ;
#57223 = CARTESIAN_POINT ( 'NONE',  ( 107.7317227740038987, 244.5530062829863311, -4.648177544792955347E-16 ) ) ;
#57224 = CARTESIAN_POINT ( 'NONE',  ( 83.21237853290490705, 230.3967562850347122, -4.648177544792955347E-16 ) ) ;
#57225 = CARTESIAN_POINT ( 'NONE',  ( 84.89261448506459828, 226.4865022471902876, -10.00000000000009415 ) ) ;
#57226 = DIRECTION ( 'NONE',  ( -0.000000000000000000, 0.000000000000000000, 1.000000000000000000 ) ) ;
#57227 = CARTESIAN_POINT ( 'NONE',  ( -50.66096862766640641, 31.69950886434491721, -10.00000000000000000 ) ) ;
#57228 = CARTESIAN_POINT ( 'NONE',  ( 45.37135788555205096, 190.8768266524159856, 9.188101187500098632 ) ) ;
#57229 = CYLINDRICAL_SURFACE ( 'NONE', #42341, 1.449999999999993072 ) ;
#57230 = VERTEX_POINT ( 'NONE', #68881 ) ;
#57231 = CARTESIAN_POINT ( 'NONE',  ( -15.54040582425010086, 84.12771141922644347, 14.97918986780710959 ) ) ;
#57232 = CARTESIAN_POINT ( 'NONE',  ( 198.4522155198218059, 286.9176751754968109, -17.57438352224490075 ) ) ;
#57233 = EDGE_CURVE ( 'NONE', #24654, #67131, #59813, .T. ) ;
#57234 = CARTESIAN_POINT ( 'NONE',  ( 67.03286369130589151, 67.01141394008774910, -8.665391638908033656 ) ) ;
#57235 = EDGE_LOOP ( 'NONE', ( #1486, #3778, #56918, #376 ) ) ;
#57236 = CARTESIAN_POINT ( 'NONE',  ( 167.4242128886634760, 285.3674954085350919, 7.916955735753099077 ) ) ;
#57237 = CARTESIAN_POINT ( 'NONE',  ( 206.9676408587583296, 272.1685258403992975, 7.544050792475608169 ) ) ;
#57238 = FACE_OUTER_BOUND ( 'NONE', #39660, .T. ) ;
#57239 = CARTESIAN_POINT ( 'NONE',  ( 33.71705561599726053, 20.26216523072496045, -2.296566073217252530E-15 ) ) ;
#57240 = CARTESIAN_POINT ( 'NONE',  ( 57.06414817410224316, 218.1868197944957330, -18.47570218321542157 ) ) ;
#57241 = CARTESIAN_POINT ( 'NONE',  ( 151.1044726995390306, 278.3667167227523009, 2.833052190833913464 ) ) ;
#57242 = CARTESIAN_POINT ( 'NONE',  ( 171.5228814212670159, 255.7221739033098800, 11.23420559966320553 ) ) ;
#57243 = VERTEX_POINT ( 'NONE', #58182 ) ;
#57244 = CARTESIAN_POINT ( 'NONE',  ( 10.42942532566755354, 26.99752408145591076, 5.678558825948276656 ) ) ;
#57245 = PLANE ( 'NONE',  #51048 ) ;
#57246 = CARTESIAN_POINT ( 'NONE',  ( 171.6147572926790303, 252.5492226098082824, 8.631356844989948485 ) ) ;
#57247 = CARTESIAN_POINT ( 'NONE',  ( 43.24043327773039636, 120.8247932685368227, 10.00000000000000000 ) ) ;
#57248 = EDGE_CURVE ( 'NONE', #86732, #4961, #85161, .T. ) ;
#57249 = ORIENTED_EDGE ( 'NONE', *, *, #68501, .T. ) ;
#57250 = CARTESIAN_POINT ( 'NONE',  ( 72.13998692144450331, 71.54377819717346654, -5.860361805407116265 ) ) ;
#57251 = CARTESIAN_POINT ( 'NONE',  ( 166.8885992513889960, 261.3854899355708881, 16.67823075215012452 ) ) ;
#57252 = ADVANCED_FACE ( 'NONE', ( #6489 ), #74417, .T. ) ;
#57253 = CARTESIAN_POINT ( 'NONE',  ( 177.9925615710933755, 254.8251403409008731, -7.350624415798725053 ) ) ;
#57254 = CARTESIAN_POINT ( 'NONE',  ( 73.09674767720407829, 64.62968492494913164, -13.92540306414895745 ) ) ;
#57255 = EDGE_LOOP ( 'NONE', ( #45443, #40436, #37355, #93997 ) ) ;
#57256 = VERTEX_POINT ( 'NONE', #52566 ) ;
#57258 = DIRECTION ( 'NONE',  ( -0.8660254037844387076, -0.4999999999999998890, -0.000000000000000000 ) ) ;
#57257 = CARTESIAN_POINT ( 'NONE',  ( 207.7320178805681508, 270.8445860024863237, -5.379955943374661764 ) ) ;
#57259 = CARTESIAN_POINT ( 'NONE',  ( 196.2630260332681189, 290.7094625936034049, -17.43112004684450866 ) ) ;
#57260 = VERTEX_POINT ( 'NONE', #82032 ) ;
#57261 = CARTESIAN_POINT ( 'NONE',  ( 65.92723761077292011, 68.94945291078158789, -2.624861927977415021 ) ) ;
#57262 = CARTESIAN_POINT ( 'NONE',  ( 173.4586948132588873, 285.6886373276996096, -12.44553698290859600 ) ) ;
#57263 = CARTESIAN_POINT ( 'NONE',  ( 71.08765421117847438, 71.69956734233102225, -3.661842409509368235 ) ) ;
#57264 = CARTESIAN_POINT ( 'NONE',  ( 78.18520617608054124, 61.02381034122267067, -15.90742658069108728 ) ) ;
#57265 = CARTESIAN_POINT ( 'NONE',  ( 157.4893260420801653, 257.8674809757739013, -18.30842125257398223 ) ) ;
#57267 = CARTESIAN_POINT ( 'NONE',  ( 120.7695210546522446, 240.5333772461660544, 9.188101187500095079 ) ) ;
#57266 = B_SPLINE_CURVE_WITH_KNOTS ( 'NONE', 3,
 ( #32092, #9830, #16897, #70093, #94443, #64005, #2730, #704, #63005, #71126, #55875, #86871, #17404, #33617, #79259, #40691, #71631, #2226, #64513, #94945, #87877, #73614, #43688, #5202, #66985, #74121, #58389, #72637 ),
 .UNSPECIFIED., .F., .F.,
 ( 4, 2, 2, 2, 2, 2, 2, 2, 2, 2, 2, 2, 2, 4 ),
 ( 0.0004012327469206063211, 0.001481470891302587214, 0.002561709035684567835, 0.003101828107875521066, 0.003236857875923203863, 0.003304372759947044828, 0.003338130201959010630, 0.003371887643970976865, 0.003439402527995009083, 0.003506917412019041301, 0.003641947180067237576, 0.004182066252259748589, 0.004452125788356024912, 0.004722185324452301235 ),
 .UNSPECIFIED. ) ;
#57268 = DIRECTION ( 'NONE',  ( -0.6602847420308683990, -0.7510153523339117010, 0.000000000000000000 ) ) ;
#57269 = FACE_OUTER_BOUND ( 'NONE', #81858, .T. ) ;
#57270 = EDGE_LOOP ( 'NONE', ( #13584, #27840, #48956, #21000 ) ) ;
#57271 = CARTESIAN_POINT ( 'NONE',  ( 164.3053959849042087, 246.0617015268593661, -7.251939739328854273 ) ) ;
#57272 = VERTEX_POINT ( 'NONE', #12608 ) ;
#57273 = CARTESIAN_POINT ( 'NONE',  ( 38.53854167689037524, 24.11110640527295246, -2.839279412974138328 ) ) ;
#57274 = FACE_BOUND ( 'NONE', #38063, .T. ) ;
#57275 = CARTESIAN_POINT ( 'NONE',  ( 78.51822142034139063, 47.92457381461660049, -14.49495123615230519 ) ) ;
#57276 = CARTESIAN_POINT ( 'NONE',  ( 71.75763553740291911, 221.4244531367911293, -4.594050593750046652 ) ) ;
#57277 = CARTESIAN_POINT ( 'NONE',  ( 73.77070425341645432, 68.39923094797843817, 11.48015304846416029 ) ) ;
#57278 =( BOUNDED_CURVE ( )  B_SPLINE_CURVE ( 2, ( #1041, #16732, #78048, #1553, #23321, #32927, #54209, #23822, #71951 ),
 .UNSPECIFIED., .F., .T. ) 
 B_SPLINE_CURVE_WITH_KNOTS ( ( 3, 2, 2, 2, 3 ),
 ( 0.1411290322580645296, 0.1424731182795699047, 0.1451612903225806550, 0.1478494623655914053, 0.1491935483870967805 ),
 .UNSPECIFIED. ) 
 CURVE ( )  GEOMETRIC_REPRESENTATION_ITEM ( )  RATIONAL_B_SPLINE_CURVE ( ( 0.9330127018922194093, 0.9330127018922200755, 1.000000000000000000, 0.8660254037844387076, 1.000000000000000000, 0.8660254037844387076, 1.000000000000000000, 0.9330127018922194093, 0.9330127018922194093 ) ) 
 REPRESENTATION_ITEM ( '' )  );
#57279 = CARTESIAN_POINT ( 'NONE',  ( 151.4281781455628675, 268.3656970847310390, 15.24742929158552585 ) ) ;
#57280 = CARTESIAN_POINT ( 'NONE',  ( 198.7564336180209068, 286.3907539728338634, 17.89468790901915796 ) ) ;
#57281 = CARTESIAN_POINT ( 'NONE',  ( 175.6467143226808503, 278.3879956775477922, 15.52796216301298315 ) ) ;
#57282 = ORIENTED_EDGE ( 'NONE', *, *, #35314, .T. ) ;
#57283 = VECTOR ( 'NONE', #887, 1000.000000000000114 ) ;
#57284 = EDGE_CURVE ( 'NONE', #64387, #48833, #54576, .T. ) ;
#57285 = CARTESIAN_POINT ( 'NONE',  ( 80.00759052209035360, 56.61424376545486581, -16.17082543645087256 ) ) ;
#57286 = CARTESIAN_POINT ( 'NONE',  ( 171.0076677319804332, 284.3901048210457247, 12.34237328981812176 ) ) ;
#57287 = ORIENTED_EDGE ( 'NONE', *, *, #98412, .F. ) ;
#57288 = DIRECTION ( 'NONE',  ( 0.000000000000000000, 0.000000000000000000, 1.000000000000000000 ) ) ;
#57289 = PLANE ( 'NONE',  #38777 ) ;
#57290 = CARTESIAN_POINT ( 'NONE',  ( 160.6728723076546430, 258.4027085289857837, -16.77127213560359920 ) ) ;
#57291 = CARTESIAN_POINT ( 'NONE',  ( 70.67536410627003818, 221.6115022471903160, -5.000000000000047962 ) ) ;
#57292 = ADVANCED_FACE ( 'NONE', ( #5489 ), #98709, .F. ) ;
#57293 = VECTOR ( 'NONE', #92766, 1000.000000000000114 ) ;
#57294 = EDGE_CURVE ( 'NONE', #81147, #73927, #35606, .T. ) ;
#57295 = CARTESIAN_POINT ( 'NONE',  ( 190.7805732161387766, 300.2053494229706985, 4.237982805666590025 ) ) ;
#57296 = CARTESIAN_POINT ( 'NONE',  ( 177.0083656731012525, 269.8104889733541540, 16.33643522331352216 ) ) ;
#57297 = CARTESIAN_POINT ( 'NONE',  ( 164.9171241593586217, 245.0021572482830550, 1.622680932994367220 ) ) ;
#57298 = CARTESIAN_POINT ( 'NONE',  ( 153.8341890703302113, 264.8936564568936660, -16.55105041955311407 ) ) ;
#57299 = VERTEX_POINT ( 'NONE', #68272 ) ;
#57300 = CARTESIAN_POINT ( 'NONE',  ( 207.8302079587528794, 270.6745157982714431, 3.572475529330238153 ) ) ;
#57301 = EDGE_CURVE ( 'NONE', #2820, #53182, #40434, .T. ) ;
#57302 = CARTESIAN_POINT ( 'NONE',  ( 125.9656734773588767, 243.5333772461660544, 9.188101187500095079 ) ) ;
#57303 = ORIENTED_EDGE ( 'NONE', *, *, #60320, .F. ) ;
#57304 = CARTESIAN_POINT ( 'NONE',  ( 82.35638529324310753, 44.23013856389444953, -9.288241028977028080 ) ) ;
#57305 = CARTESIAN_POINT ( 'NONE',  ( 84.91096221446015591, 42.98959058816011947, 4.352075159545532479 ) ) ;
#57306 = EDGE_CURVE ( 'NONE', #41965, #33184, #86444, .T. ) ;
#57307 = CARTESIAN_POINT ( 'NONE',  ( -29.91485116994501681, 25.08783183303773257, -10.00000000000000000 ) ) ;
#57308 = DIRECTION ( 'NONE',  ( 0.2471055264905481497, -0.9689885751534065284, 0.000000000000000000 ) ) ;
#57309 = CARTESIAN_POINT ( 'NONE',  ( -1.565588326081831072, 163.2365022471902307, 10.00000000000009948 ) ) ;
#57310 = CARTESIAN_POINT ( 'NONE',  ( 177.8439380257527489, 255.3043160970806582, 4.874347355181736674 ) ) ;
#57311 = VERTEX_POINT ( 'NONE', #85531 ) ;
#57312 = CARTESIAN_POINT ( 'NONE',  ( 80.46835216585913031, 57.85139773374410055, -16.60023610630909019 ) ) ;
#57313 = CARTESIAN_POINT ( 'NONE',  ( 157.9403153459281839, 276.0785681647408865, -12.83070520789915037 ) ) ;
#57315 = CARTESIAN_POINT ( 'NONE',  ( 182.1256972723869296, 260.2463563092551340, 10.61513437760372192 ) ) ;
#57314 = CARTESIAN_POINT ( 'NONE',  ( 25.34687108590969729, 93.06504152958497400, -45.00000000000001421 ) ) ;
#57316 = CARTESIAN_POINT ( 'NONE',  ( 164.3231499090067302, 246.0309508282801971, -1.360008376207661573 ) ) ;
#57317 = CARTESIAN_POINT ( 'NONE',  ( 132.6770232609232778, 259.6589784336661637, -6.496448406907676862E-16 ) ) ;
#57318 = CARTESIAN_POINT ( 'NONE',  ( -32.86949478547433046, 94.43171332246730287, 43.89948692389422291 ) ) ;
#57319 = CARTESIAN_POINT ( 'NONE',  ( 68.61230155682829945, 69.51726337545549939, 4.400640945930509140 ) ) ;
#57320 = CARTESIAN_POINT ( 'NONE',  ( 53.24634253151052832, 210.7369531367911293, -4.594050593750048428 ) ) ;
#57321 = CARTESIAN_POINT ( 'NONE',  ( 205.3708847852691406, 274.9341884869767227, -13.70973585089674174 ) ) ;
#57322 = CARTESIAN_POINT ( 'NONE',  ( 153.1198285439165545, 279.2890930352092482, 3.903594709581249322 ) ) ;
#57323 = CARTESIAN_POINT ( 'NONE',  ( 18.52134341065869805, 22.64441083166260427, -10.00000000000000533 ) ) ;
#57324 = CARTESIAN_POINT ( 'NONE',  ( 148.9230895364621574, 272.7046378331555161, 12.20434325797056019 ) ) ;
#57325 = CARTESIAN_POINT ( 'NONE',  ( 155.4143072506629721, 279.7256007574335968, -1.410841605574949531 ) ) ;
#57326 = CARTESIAN_POINT ( 'NONE',  ( 172.3432469182100988, 287.9044152303682154, -8.453389800301932766 ) ) ;
#57327 = CARTESIAN_POINT ( 'NONE',  ( 159.2554912534056939, 254.8083930951974878, 16.49944922174842432 ) ) ;
#57328 = CARTESIAN_POINT ( 'NONE',  ( 193.5827109575123188, 288.5416519977895291, 16.06052787264825810 ) ) ;
#57329 = CARTESIAN_POINT ( 'NONE',  ( 135.4648896233454991, 249.0177522451418497, -10.00000000000009592 ) ) ;
#57330 = CARTESIAN_POINT ( 'NONE',  ( 83.49981249572846309, 50.92614816156454083, -14.12294194579210682 ) ) ;
#57331 = EDGE_LOOP ( 'NONE', ( #3282, #26382, #72690, #79780, #90972 ) ) ;
#57332 = ADVANCED_FACE ( 'NONE', ( #91609, #62658 ), #92615, .T. ) ;
#57333 = CARTESIAN_POINT ( 'NONE',  ( 66.57729162794665001, 67.76982667965772578, -7.017260695426948303 ) ) ;
#57334 = CARTESIAN_POINT ( 'NONE',  ( 147.6121581866023007, 274.9752375363476631, 8.700660424766859080 ) ) ;
#57335 = CARTESIAN_POINT ( 'NONE',  ( -14.30363896367569509, 171.7369531367911293, -4.594050593750048428 ) ) ;
#57336 = CARTESIAN_POINT ( 'NONE',  ( 44.64073572505018461, 187.3923013555410080, 4.594050593750050204 ) ) ;
#57337 = CARTESIAN_POINT ( 'NONE',  ( 175.5279092779543646, 256.8636307276551634, -10.65721348558485282 ) ) ;
#57338 = CARTESIAN_POINT ( 'NONE',  ( 23.89366908878298190, 14.76426979415089846, 3.090169943749476733 ) ) ;
#57339 = LINE ( 'NONE', #9773, #59396 ) ;
#57340 = CARTESIAN_POINT ( 'NONE',  ( 157.3661765229227285, 258.0807821998820373, -18.27254492731150748 ) ) ;
#57341 = CARTESIAN_POINT ( 'NONE',  ( 72.22168947570742148, 72.04854175159199769, -3.193460859968826782 ) ) ;
#57342 = CARTESIAN_POINT ( 'NONE',  ( 190.3625087333586521, 300.9294583479858147, -4.271886578030237303 ) ) ;
#57343 = CARTESIAN_POINT ( 'NONE',  ( 74.07743547874019896, 55.48756474711195352, -16.11625136640599365 ) ) ;
#57345 = CARTESIAN_POINT ( 'NONE',  ( 48.42933654300934876, 208.7677522451419350, -5.000000000000047962 ) ) ;
#57344 = CARTESIAN_POINT ( 'NONE',  ( 171.0951295267471721, 257.9025284764553021, 14.56267897235280984 ) ) ;
#57346 = CARTESIAN_POINT ( 'NONE',  ( 180.8196955730123818, 256.2390112858561793, 1.639671592817103063 ) ) ;
#57347 = CARTESIAN_POINT ( 'NONE',  ( 205.3708847852691406, 274.9341884869767227, -13.70973585089674174 ) ) ;
#57348 = CARTESIAN_POINT ( 'NONE',  ( 162.2336410148055279, 251.8862672885301492, -14.09881826716025799 ) ) ;
#57349 = AXIS2_PLACEMENT_3D ( 'NONE', #55661, #76982, #70899 ) ;
#57350 = CARTESIAN_POINT ( 'NONE',  ( 50.39593590098449738, 193.2365022471902023, 10.00000000000009592 ) ) ;
#57351 = CARTESIAN_POINT ( 'NONE',  ( 181.3600705323845261, 292.3670172205969493, 9.011603952510858662 ) ) ;
#57352 = CARTESIAN_POINT ( 'NONE',  ( 49.43738778531180600, 210.8967562850346837, -4.648177544792955347E-16 ) ) ;
#57353 = CARTESIAN_POINT ( 'NONE',  ( 5.777845730223497789, 164.9548013555410080, -4.594050593750042211 ) ) ;
#57354 = CARTESIAN_POINT ( 'NONE',  ( 42.32740281844729680, 26.29860640527295601, -2.839279412974138328 ) ) ;
#57355 = CARTESIAN_POINT ( 'NONE',  ( 164.2487865911519975, 246.9563108291715992, 5.899911436263182374 ) ) ;
#57356 = CARTESIAN_POINT ( 'NONE',  ( 152.8107382695299918, 265.9710327055011589, 16.32045346488711246 ) ) ;
#57357 = CARTESIAN_POINT ( 'NONE',  ( 29.25887229277395463, 38.93396525600392266, 2.839279412974139660 ) ) ;
#57359 = EDGE_CURVE ( 'NONE', #60221, #23598, #77894, .T. ) ;
#57358 = AXIS2_PLACEMENT_3D ( 'NONE', #72134, #63012, #56409 ) ;
#57360 = CARTESIAN_POINT ( 'NONE',  ( 164.9335952247126045, 244.9736285262353306, -1.661461410667423255 ) ) ;
#57361 = DIRECTION ( 'NONE',  ( 0.08498217737243618508, 0.9963824715083258177, 0.000000000000000000 ) ) ;
#57362 = CARTESIAN_POINT ( 'NONE',  ( 196.3286486926436680, 290.5958008134369948, -16.58330917766970458 ) ) ;
#57363 = PLANE ( 'NONE',  #73113 ) ;
#57364 =( NAMED_UNIT ( * ) SI_UNIT ( $, .STERADIAN. ) SOLID_ANGLE_UNIT ( ) );
#57365 = CARTESIAN_POINT ( 'NONE',  ( 12.55777956335723644, 9.111106405272902720, -2.839279412974138328 ) ) ;
#57366 = CARTESIAN_POINT ( 'NONE',  ( 153.2953991261116187, 277.6583650081004748, -5.430105486410409021 ) ) ;
#57367 = CARTESIAN_POINT ( 'NONE',  ( 19.08966579672462416, 13.94754757982089011, 5.678558825948272215 ) ) ;
#57368 = CARTESIAN_POINT ( 'NONE',  ( 157.4627203480516755, 258.4629190429250798, 16.86169483958236626 ) ) ;
#57369 = CARTESIAN_POINT ( 'NONE',  ( 153.2427285380101978, 277.7181708921816607, -5.112331264339823989 ) ) ;
#57370 = CARTESIAN_POINT ( 'NONE',  ( 105.0000000000000142, 93.06504152958497400, -54.99999999999999289 ) ) ;
#57371 = CARTESIAN_POINT ( 'NONE',  ( 206.6912923161529818, 272.6471755567893638, -9.325620632947922317 ) ) ;
#57372 = CARTESIAN_POINT ( 'NONE',  ( 165.0391502558331069, 249.6778246878102436, -10.74756611015070717 ) ) ;
#57373 = EDGE_CURVE ( 'NONE', #30767, #52870, #82128, .T. ) ;
#57374 = ORIENTED_EDGE ( 'NONE', *, *, #53633, .T. ) ;
#57375 = CARTESIAN_POINT ( 'NONE',  ( 152.7531861616124615, 266.0707158804971186, 17.45453282433162556 ) ) ;
#57376 = CARTESIAN_POINT ( 'NONE',  ( 164.4858674010174298, 245.7491158648375347, -2.958464974013825355 ) ) ;
#57377 = LINE ( 'NONE', #88351, #2463 ) ;
#57378 = EDGE_CURVE ( 'NONE', #28585, #49558, #50136, .T. ) ;
#57379 = CARTESIAN_POINT ( 'NONE',  ( 87.43576499144317893, 45.00137247461035628, 6.922634181320205471 ) ) ;
#57380 = EDGE_LOOP ( 'NONE', ( #95777, #80384, #95710, #10435 ) ) ;
#57381 = ORIENTED_EDGE ( 'NONE', *, *, #36249, .T. ) ;
#57383 = CARTESIAN_POINT ( 'NONE',  ( 1.233819684896646951, 25.98176417558038764, 10.00000000000000000 ) ) ;
#57382 = DIRECTION ( 'NONE',  ( -0.8660254037844387076, -0.4999999999999998890, -0.000000000000000000 ) ) ;
#57384 = CARTESIAN_POINT ( 'NONE',  ( 86.41183189003805865, 47.25727891775800771, 10.78350007392548271 ) ) ;
#57385 = ORIENTED_EDGE ( 'NONE', *, *, #80492, .F. ) ;
#57386 = CARTESIAN_POINT ( 'NONE',  ( 77.07529298142445384, 54.05291532172810776, 16.01725459708226751 ) ) ;
#57387 = CARTESIAN_POINT ( 'NONE',  ( 174.3627903489640687, 262.5166068422508943, 14.67416242571188256 ) ) ;
#57388 = EDGE_LOOP ( 'NONE', ( #58995, #11321, #11170, #8935 ) ) ;
#57389 = CARTESIAN_POINT ( 'NONE',  ( 28.46864935082048831, 149.7156766241961350, 21.50000000000008527 ) ) ;
#57390 = CARTESIAN_POINT ( 'NONE',  ( 88.52345208173723279, 43.89072024811925843, -0.4439432684152969100 ) ) ;
#57391 = CARTESIAN_POINT ( 'NONE',  ( 81.74377432616384453, 48.00429482119757552, -13.52050817838834895 ) ) ;
#57392 = CARTESIAN_POINT ( 'NONE',  ( 80.55884490112875085, 43.45966037107459812, 9.562419172017994740 ) ) ;
#57393 = ORIENTED_EDGE ( 'NONE', *, *, #71624, .T. ) ;
#57394 = CARTESIAN_POINT ( 'NONE',  ( 174.2647729094104818, 267.6455815624914862, 16.44362021030165977 ) ) ;
#57395 = CARTESIAN_POINT ( 'NONE',  ( 169.1871453744360849, 276.0921898949916908, -15.50345989341305497 ) ) ;
#57396 = CARTESIAN_POINT ( 'NONE',  ( 50.34596055286377947, 92.70800680107760172, 177.5919119679930134 ) ) ;
#57397 = ORIENTED_EDGE ( 'NONE', *, *, #93120, .T. ) ;
#57398 = CARTESIAN_POINT ( 'NONE',  ( 171.0009588779175829, 254.8957903787501493, -11.39820321899803623 ) ) ;
#57399 = EDGE_LOOP ( 'NONE', ( #88104, #56719, #97689, #66472 ) ) ;
#57400 = CARTESIAN_POINT ( 'NONE',  ( 156.9694903541507074, 266.1758412851487492, -17.34135443527054576 ) ) ;
#57401 = ORIENTED_EDGE ( 'NONE', *, *, #58512, .T. ) ;
#57402 = CARTESIAN_POINT ( 'NONE',  ( 157.0523007431125961, 269.6879238887856332, 16.04707504889739056 ) ) ;
#57403 = ORIENTED_EDGE ( 'NONE', *, *, #98727, .T. ) ;
#57404 = ADVANCED_FACE ( 'NONE', ( #85010 ), #65103, .F. ) ;
#57405 = CARTESIAN_POINT ( 'NONE',  ( 193.9130084035158745, 294.7798125270166452, 13.46593982140802837 ) ) ;
#57406 = CARTESIAN_POINT ( 'NONE',  ( 180.4099482243281045, 291.1497967234276416, -9.622827375937299976 ) ) ;
#57407 = CYLINDRICAL_SURFACE ( 'NONE', #78679, 10.00000000000010658 ) ;
#57408 = CARTESIAN_POINT ( 'NONE',  ( 199.6570654737131747, 281.0878073294180695, -17.28888823238446193 ) ) ;
#57409 = CARTESIAN_POINT ( 'NONE',  ( 176.0858336914031383, 290.3330534276880144, 6.126020769380866149 ) ) ;
#57410 = CARTESIAN_POINT ( 'NONE',  ( 197.5632903914970768, 288.4573386618801010, -18.12045497471262578 ) ) ;
#57411 = EDGE_LOOP ( 'NONE', ( #17931, #63577, #89926, #14430 ) ) ;
#57412 = CARTESIAN_POINT ( 'NONE',  ( 93.82350145804369390, 231.6427522451419065, -10.00000000000009592 ) ) ;
#57413 = CARTESIAN_POINT ( 'NONE',  ( 24.98947064339976265, 26.37878583063841731, 9.188101187500006262 ) ) ;
#57414 = CARTESIAN_POINT ( 'NONE',  ( 164.5813345449211624, 245.5837619211427523, 1.447064457712487373 ) ) ;
#57415 = CARTESIAN_POINT ( 'NONE',  ( 164.2813349609167517, 246.1033764428878214, 1.949810150281061638 ) ) ;
#57417 = VERTEX_POINT ( 'NONE', #93440 ) ;
#57416 = CARTESIAN_POINT ( 'NONE',  ( 85.46847960764181096, 42.12007198895852156, -0.3052117524058582942 ) ) ;
#57418 = VERTEX_POINT ( 'NONE', #77722 ) ;
#57419 = CARTESIAN_POINT ( 'NONE',  ( 190.3549927569640943, 300.9424764009692126, 6.306669742828282743 ) ) ;
#57420 = FACE_OUTER_BOUND ( 'NONE', #87612, .T. ) ;
#57421 = EDGE_CURVE ( 'NONE', #30831, #80515, #61976, .T. ) ;
#57422 = CARTESIAN_POINT ( 'NONE',  ( 44.43605786102924782, 27.78380873178790722, -6.180339887498949025 ) ) ;
#57423 = CARTESIAN_POINT ( 'NONE',  ( -19.65312891409030271, 93.06504152958497400, 25.00000000000000000 ) ) ;
#57424 = VECTOR ( 'NONE', #41470, 1000.000000000000000 ) ;
#57425 = CARTESIAN_POINT ( 'NONE',  ( 198.8384730411855514, 286.2486575236893032, -17.11322556960806551 ) ) ;
#57426 = CARTESIAN_POINT ( 'NONE',  ( 190.6136768402189716, 300.4944224256624921, -0.6663190606136376593 ) ) ;
#57427 = ORIENTED_EDGE ( 'NONE', *, *, #15768, .F. ) ;
#57428 = CYLINDRICAL_SURFACE ( 'NONE', #5754, 17.82106496071139645 ) ;
#57429 = DIRECTION ( 'NONE',  ( -0.1654779384134575371, 0.9862134920484671996, 0.000000000000000000 ) ) ;
#57430 = CARTESIAN_POINT ( 'NONE',  ( 81.65310433048475147, 42.64019311979919280, 7.560891536010023728 ) ) ;
#57431 = CARTESIAN_POINT ( 'NONE',  ( -9.864998445682774175, 175.1115022471903160, -5.000000000000047962 ) ) ;
#57432 = CARTESIAN_POINT ( 'NONE',  ( 30.74798454907712397, 181.8927522451418213, 10.00000000000009592 ) ) ;
#57433 = CARTESIAN_POINT ( 'NONE',  ( 100.0117143358702236, 237.7369531367911009, -4.594050593750048428 ) ) ;
#57434 = VECTOR ( 'NONE', #79271, 1000.000000000000000 ) ;
#57435 = CARTESIAN_POINT ( 'NONE',  ( 168.2322000736707537, 260.5619311436532826, 16.64139255606118439 ) ) ;
#57436 = DIRECTION ( 'NONE',  ( -0.000000000000000000, -1.000000000000000000, -0.000000000000000000 ) ) ;
#57437 = CARTESIAN_POINT ( 'NONE',  ( 162.5429104506708597, 249.1144160197565043, 10.44355587256373674 ) ) ;
#57438 = EDGE_CURVE ( 'NONE', #84087, #99795, #54973, .T. ) ;
#57439 = CARTESIAN_POINT ( 'NONE',  ( 15.76359375002403596, 192.1589784336661637, -6.496448406907675876E-16 ) ) ;
#57440 = CARTESIAN_POINT ( 'NONE',  ( 161.8016137473484548, 250.3983795733946636, 14.25000412375400316 ) ) ;
#57441 = ORIENTED_EDGE ( 'NONE', *, *, #28208, .F. ) ;
#57442 = ORIENTED_EDGE ( 'NONE', *, *, #27387, .T. ) ;
#57443 = CARTESIAN_POINT ( 'NONE',  ( 185.3693644285349365, 260.1071722789047271, -5.798844428750127733 ) ) ;
#57444 = CARTESIAN_POINT ( 'NONE',  ( 80.89292881529833323, 46.87624008130001840, -12.53476188675516134 ) ) ;
#57445 = CARTESIAN_POINT ( 'NONE',  ( 146.8729474948188454, 276.2555880120147549, 3.934020695290606273 ) ) ;
#57446 = DIRECTION ( 'NONE',  ( -0.8660254037844387076, -0.4999999999999998890, -0.000000000000000000 ) ) ;
#57447 = EDGE_CURVE ( 'NONE', #42575, #43244, #23519, .T. ) ;
#57448 = CARTESIAN_POINT ( 'NONE',  ( 161.1093323826042933, 251.5974460702646809, -13.93502574894237078 ) ) ;
#57449 = DIRECTION ( 'NONE',  ( 0.5000000000000001110, -0.8660254037844385966, 0.000000000000000000 ) ) ;
#57450 = CARTESIAN_POINT ( 'NONE',  ( 74.14322651144246379, 67.86457474202013884, -11.65196598083728041 ) ) ;
#57451 = CARTESIAN_POINT ( 'NONE',  ( 45.07374842694240868, 187.6423013555410080, -4.594050593750043987 ) ) ;
#57452 = CARTESIAN_POINT ( 'NONE',  ( 88.77168660263453148, 215.3927522451418213, -10.00000000000009059 ) ) ;
#57453 = ADVANCED_FACE ( 'NONE', ( #46802 ), #42450, .F. ) ;
#57454 = CARTESIAN_POINT ( 'NONE',  ( 83.24352937575713440, 45.45189662214414028, 10.11960700973886951 ) ) ;
#57455 = CARTESIAN_POINT ( 'NONE',  ( 179.2638961323747537, 258.2260800035196553, -10.18064271055803616 ) ) ;
#57456 = CARTESIAN_POINT ( 'NONE',  ( -0.04102277327696322862, 170.7833772461660828, -9.188101187500095079 ) ) ;
#57457 = CARTESIAN_POINT ( 'NONE',  ( 68.49429924950833026, 64.43582602095906964, -12.25658928467158049 ) ) ;
#57458 = CARTESIAN_POINT ( 'NONE',  ( 150.9363692955544991, 269.2175350005573478, -14.27857383982596140 ) ) ;
#57459 = CARTESIAN_POINT ( 'NONE',  ( 42.33744422746375591, 122.7866300363639169, -10.00000000000000000 ) ) ;
#57460 = CARTESIAN_POINT ( 'NONE',  ( 192.6170194583582429, 297.0245312260774995, -11.90166228306590490 ) ) ;
#57461 = PLANE ( 'NONE',  #32835 ) ;
#57462 = CARTESIAN_POINT ( 'NONE',  ( 163.7136804588959649, 247.0865828815331042, 6.783386239354816105 ) ) ;
#57463 = CARTESIAN_POINT ( 'NONE',  ( 146.6138605399200117, 276.7043397814778132, -0.5394499176159462950 ) ) ;
#57464 = CARTESIAN_POINT ( 'NONE',  ( 206.9377610035629118, 272.2202792677204002, 7.440532334334675646 ) ) ;
#57465 = ORIENTED_EDGE ( 'NONE', *, *, #87323, .T. ) ;
#57466 = CARTESIAN_POINT ( 'NONE',  ( -2.503782513514959174, 159.3615022471902023, 5.000000000000051514 ) ) ;
#57467 = B_SPLINE_CURVE_WITH_KNOTS ( 'NONE', 3,
 ( #40115, #70024, #69534, #85280, #55314, #92866, #63930, #46212, #71054, #15826, #1656, #33030, #38624, #94869, #71554, #56322, #32541, #87316, #94373, #46729, #24928, #31519, #77657, #77131 ),
 .UNSPECIFIED., .F., .F.,
 ( 4, 2, 2, 2, 2, 2, 2, 2, 2, 2, 2, 4 ),
 ( 0.000000000000000000, 0.1249999999999977240, 0.2499999999999954481, 0.3749999999999931721, 0.4374999999999883427, 0.4999999999999834577, 0.5624999999999785727, 0.6249999999999736877, 0.6874999999999686917, 0.7499999999999638067, 0.8749999999999820144, 1.000000000000000000 ),
 .UNSPECIFIED. ) ;
#57468 = CARTESIAN_POINT ( 'NONE',  ( 84.27717094892697958, 45.26462376842967217, 9.982582507191876786 ) ) ;
#57469 = CARTESIAN_POINT ( 'NONE',  ( 129.8627877943888791, 245.7833772461660544, -9.188101187500095079 ) ) ;
#57470 = CARTESIAN_POINT ( 'NONE',  ( 21.91745948943428601, 13.44966523072494269, -2.296566073217252530E-15 ) ) ;
#57471 = CARTESIAN_POINT ( 'NONE',  ( 74.89568429962641005, 67.14399892254596125, 12.98700472788359406 ) ) ;
#57472 = DIRECTION ( 'NONE',  ( -0.8660254037844387076, -0.4999999999999998890, -0.000000000000000000 ) ) ;
#57474 = CARTESIAN_POINT ( 'NONE',  ( 185.6255372557312455, 288.0586212204385106, 14.85957563350848254 ) ) ;
#57473 = CARTESIAN_POINT ( 'NONE',  ( 81.78504375891562006, 41.48292696562020865, -5.073134180756075473 ) ) ;
#57475 = CARTESIAN_POINT ( 'NONE',  ( 190.5723142641005552, 300.5660645090316052, -7.285051322221389292 ) ) ;
#57476 = VERTEX_POINT ( 'NONE', #27373 ) ;
#57477 = CARTESIAN_POINT ( 'NONE',  ( 191.5451565139252068, 298.8810523045859213, 7.782291334092181323 ) ) ;
#57478 = CARTESIAN_POINT ( 'NONE',  ( 197.0184425104562820, 289.4010428742387262, -16.90752553128928426 ) ) ;
#57479 = CARTESIAN_POINT ( 'NONE',  ( 190.6149048745654966, 300.0785874667154758, 3.592099452960924477 ) ) ;
#57480 = CARTESIAN_POINT ( 'NONE',  ( 175.0221218187403451, 292.3615283621688832, -1.152100040113013479 ) ) ;
#57481 = ORIENTED_EDGE ( 'NONE', *, *, #99481, .F. ) ;
#57482 = CARTESIAN_POINT ( 'NONE',  ( 74.31929878905869202, 64.95657537261109837, -14.11942355924862014 ) ) ;
#57483 = CARTESIAN_POINT ( 'NONE',  ( 25.79892497710874366, 15.86426979415090166, -3.090169943749474069 ) ) ;
#57484 = CARTESIAN_POINT ( 'NONE',  ( 168.8129333540870221, 271.8871668449080516, -17.12755824114822900 ) ) ;
#57485 = CARTESIAN_POINT ( 'NONE',  ( 71.90360357134964886, 72.59530952775406831, 1.145984468326242789 ) ) ;
#57486 = EDGE_CURVE ( 'NONE', #83821, #60445, #49664, .T. ) ;
#57487 = CARTESIAN_POINT ( 'NONE',  ( 77.71695824127769470, 49.45779813231933986, 15.33409790721217369 ) ) ;
#57488 = CARTESIAN_POINT ( 'NONE',  ( 200.2688005423887603, 272.3943678420544074, 12.70188190611125556 ) ) ;
#57489 = VECTOR ( 'NONE', #2097, 1000.000000000000000 ) ;
#57490 = DIRECTION ( 'NONE',  ( -1.000000000000000000, 0.000000000000000000, 0.000000000000000000 ) ) ;
#57491 = EDGE_CURVE ( 'NONE', #39184, #21534, #41704, .T. ) ;
#57492 = CARTESIAN_POINT ( 'NONE',  ( 71.99762221142530905, 71.50039512193581004, -5.770478025556951884 ) ) ;
#57493 = CARTESIAN_POINT ( 'NONE',  ( 153.4578721839791342, 264.8501638863745029, 16.85421393845643223 ) ) ;
#57494 = ORIENTED_EDGE ( 'NONE', *, *, #89379, .F. ) ;
#57495 = CARTESIAN_POINT ( 'NONE',  ( 190.7685680519976188, 280.8244985282360631, 16.64107897673111580 ) ) ;
#57496 = EDGE_CURVE ( 'NONE', #4766, #3950, #83706, .T. ) ;
#57497 = CARTESIAN_POINT ( 'NONE',  ( 42.15722797529793553, 32.84335787977767041, 9.188101187500006262 ) ) ;
#57498 = CARTESIAN_POINT ( 'NONE',  ( 173.9239121147568881, 272.8349737613822867, -16.35791196226779931 ) ) ;
#57499 = VERTEX_POINT ( 'NONE', #74496 ) ;
#57500 = B_SPLINE_CURVE_WITH_KNOTS ( 'NONE', 3,
 ( #57473, #19522, #51889, #28081, #82830, #88456, #75200, #19015, #11908, #66089 ),
 .UNSPECIFIED., .F., .F.,
 ( 4, 2, 2, 2, 4 ),
 ( 0.000000000000000000, 0.2500000000000000000, 0.5000000000000000000, 0.7500000000000000000, 1.000000000000000000 ),
 .UNSPECIFIED. ) ;
#57501 = CARTESIAN_POINT ( 'NONE',  ( 164.5514333943684733, 280.2750504504191440, 12.59899363382133686 ) ) ;
#57502 = EDGE_CURVE ( 'NONE', #31691, #93599, #63418, .T. ) ;
#57503 = CARTESIAN_POINT ( 'NONE',  ( 147.7112127936102866, 274.8036699242858276, -9.124700685424272706 ) ) ;
#57504 = LINE ( 'NONE', #82856, #16031 ) ;
#57506 = ORIENTED_EDGE ( 'NONE', *, *, #79300, .F. ) ;
#57505 = AXIS2_PLACEMENT_3D ( 'NONE', #89807, #18895, #80730 ) ;
#57507 = CARTESIAN_POINT ( 'NONE',  ( -21.58168810074490551, 24.33735145887882112, 10.00000000000000000 ) ) ;
#57508 = LINE ( 'NONE', #50410, #68567 ) ;
#57509 = B_SPLINE_CURVE_WITH_KNOTS ( 'NONE', 3,
 ( #28669, #44363, #5877, #21579, #92021, #75794, #84404, #14949, #37751, #7874, #75296, #36763, #83915, #91016, #92498, #45838, #30164, #98601, #68657, #22067, #76761, #29185, #6380, #15440, #52464, #46339, #7356, #60052, #38240, #69155, #45358, #76290, #83408, #100084, #13979, #44854, #90530, #29670, #61046, #61552, #6862, #99088, #84899, #21101, #23043, #53939, #77262, #38750 ),
 .UNSPECIFIED., .F., .F.,
 ( 4, 2, 2, 2, 2, 2, 2, 2, 2, 2, 2, 2, 2, 2, 2, 2, 2, 2, 2, 2, 2, 2, 2, 4 ),
 ( 0.003026550417145748746, 0.003224528412346372268, 0.003422506407546995789, 0.003521495405147307550, 0.003620484402747619311, 0.003818462397948246302, 0.004214418388349643399, 0.004610374378751041363, 0.005402286359553663819, 0.006194198340356286275, 0.006986110321158909599, 0.007778022301961532055, 0.007877011299561914939, 0.007926505798362145847, 0.007976000297162375019, 0.008025494795962605926, 0.008074989294762836833, 0.008173978292363319464, 0.008371956287564218807, 0.008569934282765118150, 0.008767912277966019227, 0.008965890273166920305, 0.009163868268367819647, 0.009361846263568718990 ),
 .UNSPECIFIED. ) ;
#57510 = B_SPLINE_CURVE_WITH_KNOTS ( 'NONE', 3,
 ( #45626, #92776, #85706, #78056 ),
 .UNSPECIFIED., .F., .F.,
 ( 4, 4 ),
 ( 0.001468722747720561895, 0.009396689447536171053 ),
 .UNSPECIFIED. ) ;
#57511 = ORIENTED_EDGE ( 'NONE', *, *, #70785, .T. ) ;
#57512 = CARTESIAN_POINT ( 'NONE',  ( 78.74619901529338506, 51.78797505174686933, -15.41928803356502264 ) ) ;
#57513 = CARTESIAN_POINT ( 'NONE',  ( 84.49829320381432751, 49.81850184317473662, -13.23518311421627125 ) ) ;
#57514 = CARTESIAN_POINT ( 'NONE',  ( 185.0696649060035668, 259.9978788641606684, -6.171662045453295775 ) ) ;
#57515 = ORIENTED_EDGE ( 'NONE', *, *, #8917, .T. ) ;
#57516 = EDGE_LOOP ( 'NONE', ( #57924, #89693, #48684, #68954 ) ) ;
#57517 = DIRECTION ( 'NONE',  ( -0.9628097264997621529, 0.2701803667135219689, 0.000000000000000000 ) ) ;
#57518 = ORIENTED_EDGE ( 'NONE', *, *, #24922, .T. ) ;
#57519 = CYLINDRICAL_SURFACE ( 'NONE', #93510, 70.00000000000002842 ) ;
#57520 = VERTEX_POINT ( 'NONE', #3589 ) ;
#57521 = CARTESIAN_POINT ( 'NONE',  ( 74.75863154782773279, 57.63597024813910252, 16.00019208182263597 ) ) ;
#57522 = CARTESIAN_POINT ( 'NONE',  ( 205.5791761573774181, 272.5734172477073116, 10.13670412909801044 ) ) ;
#57523 = ORIENTED_EDGE ( 'NONE', *, *, #78238, .T. ) ;
#57524 = CARTESIAN_POINT ( 'NONE',  ( 182.8809842375080734, 280.3743175483600112, -16.11093289984563981 ) ) ;
#57525 = CARTESIAN_POINT ( 'NONE',  ( 81.90913890621609994, 41.07391263979702245, 3.568215028523603394 ) ) ;
#57526 = CARTESIAN_POINT ( 'NONE',  ( 162.4754228937684957, 255.5738001540079836, -14.97516694854825658 ) ) ;
#57527 = DIRECTION ( 'NONE',  ( -0.8660254037844387076, -0.4999999999999998890, -0.000000000000000000 ) ) ;
#57528 = CARTESIAN_POINT ( 'NONE',  ( 147.5540328368684300, 275.0759135952944234, -4.750028533202499403 ) ) ;
#57529 = DIRECTION ( 'NONE',  ( -0.4145187862775162602, 0.7179675985244458047, -0.5591929034707565638 ) ) ;
#57530 = CARTESIAN_POINT ( 'NONE',  ( 37.33196394253075567, 103.5643028465244555, 59.99999999999999289 ) ) ;
#57531 = CARTESIAN_POINT ( 'NONE',  ( 72.73940707191790978, 68.18235160057777478, -10.56708786553003065 ) ) ;
#57532 = CARTESIAN_POINT ( 'NONE',  ( 142.5284093247362591, 253.0958772461660544, -9.188101187500095079 ) ) ;
#57533 = CARTESIAN_POINT ( 'NONE',  ( 70.82864487769981565, 61.11463513126617642, -14.45246479568451825 ) ) ;
#57534 = VERTEX_POINT ( 'NONE', #73482 ) ;
#57535 = VECTOR ( 'NONE', #35985, 1000.000000000000114 ) ;
#57537 = EDGE_LOOP ( 'NONE', ( #86650, #25748, #73492, #10028 ) ) ;
#57536 = CARTESIAN_POINT ( 'NONE',  ( 85.33699565288863198, 48.33901173460944278, -12.30238903177781395 ) ) ;
#57538 = CARTESIAN_POINT ( 'NONE',  ( 3.125382611083894702, 162.6115022471902023, -5.000000000000041744 ) ) ;
#57539 = CARTESIAN_POINT ( 'NONE',  ( 181.4954090331713417, 255.0423029034424189, 0.9094182891644410072 ) ) ;
#57540 = CARTESIAN_POINT ( 'NONE',  ( 76.18525949220615701, 64.77142460697901072, -14.35656184529598711 ) ) ;
#57541 = CARTESIAN_POINT ( 'NONE',  ( 157.3462768699361902, 280.0432704934171397, -6.946531866745294437 ) ) ;
#57542 = CARTESIAN_POINT ( 'NONE',  ( 173.8469137325424185, 256.4471593116459189, -12.44389045026504270 ) ) ;
#57543 = PRODUCT_DEFINITION ( 'UNKNOWN', '', #91599, #63548 ) ;
#57544 = VECTOR ( 'NONE', #27898, 1000.000000000000000 ) ;
#57545 = CARTESIAN_POINT ( 'NONE',  ( 192.7433141272525745, 292.4329090757873360, -14.35978368495236168 ) ) ;
#57546 = CARTESIAN_POINT ( 'NONE',  ( 83.68679791621119080, 41.62673357145322228, 0.2031610672272064766 ) ) ;
#57547 = CARTESIAN_POINT ( 'NONE',  ( 88.15760586300541490, 44.17367696878018535, -1.747427669005709117 ) ) ;
#57548 = VERTEX_POINT ( 'NONE', #35955 ) ;
#57550 = CARTESIAN_POINT ( 'NONE',  ( 147.7112127936102866, 274.8036699242858276, -9.124700685424272706 ) ) ;
#57549 = B_SPLINE_CURVE_WITH_KNOTS ( 'NONE', 3,
 ( #67958, #98878, #68444, #20378 ),
 .UNSPECIFIED., .F., .F.,
 ( 4, 4 ),
 ( 0.01007977251148702881, 0.01610653884049561071 ),
 .UNSPECIFIED. ) ;
#57551 = CARTESIAN_POINT ( 'NONE',  ( 66.25373396628860689, 68.82734845049694172, 0.1167526145283954014 ) ) ;
#57552 = EDGE_LOOP ( 'NONE', ( #99784, #21401, #4582, #69206, #99441 ) ) ;
#57553 = DIRECTION ( 'NONE',  ( 0.000000000000000000, 0.000000000000000000, 1.000000000000000000 ) ) ;
#57554 = CARTESIAN_POINT ( 'NONE',  ( 201.2129524287560969, 267.2802673471600770, -2.216931291613017052 ) ) ;
#57555 = FACE_OUTER_BOUND ( 'NONE', #77829, .T. ) ;
#57556 = CARTESIAN_POINT ( 'NONE',  ( 190.7805732161387766, 300.2053494229706985, 4.237982805666590025 ) ) ;
#57557 = EDGE_CURVE ( 'NONE', #91708, #29127, #4066, .T. ) ;
#57558 = CARTESIAN_POINT ( 'NONE',  ( 163.0309151244508712, 248.2691671304387739, 11.27270415168660200 ) ) ;
#57560 = CARTESIAN_POINT ( 'NONE',  ( 88.24872265415196182, 44.28890599193383792, 2.074108197446814739 ) ) ;
#57559 = CARTESIAN_POINT ( 'NONE',  ( 156.5497824763685912, 272.6770023486104719, 14.78669166138748814 ) ) ;
#57561 = CARTESIAN_POINT ( 'NONE',  ( 203.9077188555663156, 269.1475184353535042, 5.568207685932024198 ) ) ;
#57562 = ORIENTED_EDGE ( 'NONE', *, *, #29469, .F. ) ;
#57563 = AXIS2_PLACEMENT_3D ( 'NONE', #28273, #50088, #73401 ) ;
#57564 = CARTESIAN_POINT ( 'NONE',  ( 6.860117161356328097, 174.7677522451418781, 10.00000000000009592 ) ) ;
#57565 = CARTESIAN_POINT ( 'NONE',  ( 189.8874520319352541, 274.0679647338298537, -15.62099291552114799 ) ) ;
#57566 = CARTESIAN_POINT ( 'NONE',  ( 25.98835327777827686, 41.64452202306098627, 10.00000000000000000 ) ) ;
#57567 = VECTOR ( 'NONE', #1954, 1000.000000000000000 ) ;
#57568 = LINE ( 'NONE', #88542, #66300 ) ;
#57569 =( BOUNDED_CURVE ( )  B_SPLINE_CURVE ( 2, ( #93772, #529, #72454, #3060, #19256, #49619, #42992, #80572, #50122, #88685, #97255, #88187, #11150 ),
 .UNSPECIFIED., .F., .T. ) 
 B_SPLINE_CURVE_WITH_KNOTS ( ( 3, 2, 2, 2, 2, 2, 3 ),
 ( 0.3125000000000000000, 0.3150000000000000022, 0.3200000000000000067, 0.3250000000000000111, 0.3300000000000000155, 0.3350000000000000200, 0.3375000000000000222 ),
 .UNSPECIFIED. ) 
 CURVE ( )  GEOMETRIC_REPRESENTATION_ITEM ( )  RATIONAL_B_SPLINE_CURVE ( ( 0.9755282581475768211, 0.9755282581475768211, 1.000000000000000000, 0.9510565162951535312, 1.000000000000000000, 0.9510565162951535312, 1.000000000000000000, 0.9510565162951535312, 1.000000000000000000, 0.9510565162951535312, 1.000000000000000000, 0.9755282581475768211, 0.9755282581475768211 ) ) 
 REPRESENTATION_ITEM ( '' )  );
#57570 = CARTESIAN_POINT ( 'NONE',  ( -47.71918240028242764, 48.07787485988725251, 59.99999999999999289 ) ) ;
#57571 = CARTESIAN_POINT ( 'NONE',  ( 174.4665098196985298, 288.5002641398569949, -10.08633113632384237 ) ) ;
#57572 = CARTESIAN_POINT ( 'NONE',  ( -15.48667327915257452, 102.2334782771513630, 44.45097685414082633 ) ) ;
#57573 = CARTESIAN_POINT ( 'NONE',  ( 1.609577830863368586, 180.9244531367911577, -4.594050593750046652 ) ) ;
#57574 = CARTESIAN_POINT ( 'NONE',  ( 108.2124997955428967, 221.0327760586659451, 1.948934522072303157E-15 ) ) ;
#57575 = CARTESIAN_POINT ( 'NONE',  ( 202.7973612924478743, 279.3916619310153919, -15.54732529288344089 ) ) ;
#57576 = CARTESIAN_POINT ( 'NONE',  ( 88.19119485691749105, 44.51220553762047416, -4.804906155116626110 ) ) ;
#57577 = CARTESIAN_POINT ( 'NONE',  ( 182.4824444819098801, 257.3791432140518509, -2.310616456812910169 ) ) ;
#57578 = EDGE_CURVE ( 'NONE', #62365, #71177, #17481, .T. ) ;
#57579 = CYLINDRICAL_SURFACE ( 'NONE', #38277, 17.82106496071139645 ) ;
#57580 = CARTESIAN_POINT ( 'NONE',  ( 76.92873890057782660, 49.89429371730488327, 15.13083596839045519 ) ) ;
#57581 = CARTESIAN_POINT ( 'NONE',  ( 152.6809499003229860, 273.9044486092186048, 12.24870461040242553 ) ) ;
#57582 = CARTESIAN_POINT ( 'NONE',  ( 148.3025927079438304, 273.7793698660844939, -8.046026357031887954 ) ) ;
#57583 = CARTESIAN_POINT ( 'NONE',  ( 181.7688134247665630, 291.5467564283949855, 9.356705366744733965 ) ) ;
#57584 = CARTESIAN_POINT ( 'NONE',  ( 205.5941538711272472, 274.5474750865108717, -13.11650762359312772 ) ) ;
#57585 = CARTESIAN_POINT ( 'NONE',  ( 76.93595106450065657, 55.49016027357946257, -16.15734999971556007 ) ) ;
#57586 = CARTESIAN_POINT ( 'NONE',  ( 166.1724940190044606, 253.7130649904839572, -13.33068584944167512 ) ) ;
#57587 = DIRECTION ( 'NONE',  ( -0.000000000000000000, 0.000000000000000000, -1.000000000000000000 ) ) ;
#57588 = FACE_OUTER_BOUND ( 'NONE', #69860, .T. ) ;
#57589 = CARTESIAN_POINT ( 'NONE',  ( 81.04025856027610075, 229.8464784336661353, 1.353441290958777327E-15 ) ) ;
#57590 = CARTESIAN_POINT ( 'NONE',  ( 207.8792014703394671, 270.5896565469619759, -5.780233892547864905 ) ) ;
#57591 = CARTESIAN_POINT ( 'NONE',  ( 73.05674748647940930, 57.23263728894347935, 15.90451911058029744 ) ) ;
#57592 = CARTESIAN_POINT ( 'NONE',  ( 163.5110577551225788, 257.9154526713028304, 15.56383249676774128 ) ) ;
#57594 = CARTESIAN_POINT ( 'NONE',  ( 151.7329441859792212, 267.8378268183080309, 16.45705841208969389 ) ) ;
#57593 = DIRECTION ( 'NONE',  ( -0.8660254037844387076, -0.4999999999999998890, -0.000000000000000000 ) ) ;
#57595 = CARTESIAN_POINT ( 'NONE',  ( 75.62238463899576857, 65.35737373615053514, 14.30258955018443601 ) ) ;
#57596 = CARTESIAN_POINT ( 'NONE',  ( -61.39381520214497812, 38.43978098112751951, -10.00000000000000000 ) ) ;
#57597 = VECTOR ( 'NONE', #4767, 1000.000000000000000 ) ;
#57598 = CARTESIAN_POINT ( 'NONE',  ( 27.72828276626169952, 36.98502408145593989, -5.678558825948271327 ) ) ;
#57599 = PLANE ( 'NONE',  #59625 ) ;
#57600 = CARTESIAN_POINT ( 'NONE',  ( 84.33507765194615047, 46.83375941775653217, -10.92698133767611779 ) ) ;
#57601 = ORIENTED_EDGE ( 'NONE', *, *, #90760, .T. ) ;
#57602 = CARTESIAN_POINT ( 'NONE',  ( 19.52749640002317122, 16.98920272979925628, 7.433330006724137462 ) ) ;
#57603 = CARTESIAN_POINT ( 'NONE',  ( 69.26781250152264136, 219.9869531367911293, 4.594050593750046652 ) ) ;
#57604 = CARTESIAN_POINT ( 'NONE',  ( 172.2702976754117401, 289.2103317004583118, -1.060902075591837468 ) ) ;
#57605 = CARTESIAN_POINT ( 'NONE',  ( 146.9700173529739970, 276.0874580858064746, -5.099093031535578469 ) ) ;
#57606 = CARTESIAN_POINT ( 'NONE',  ( 188.0806836029928490, 285.9827684710060112, -16.28010878645887871 ) ) ;
#57607 = VERTEX_POINT ( 'NONE', #45051 ) ;
#57608 = AXIS2_PLACEMENT_3D ( 'NONE', #50805, #51295, #12329 ) ;
#57609 = CARTESIAN_POINT ( 'NONE',  ( 86.18930939419189485, 47.16029689842823558, 10.81535065263619622 ) ) ;
#57610 = CARTESIAN_POINT ( 'NONE',  ( -48.71813016832984289, 30.75580926756359901, -10.00000000000000000 ) ) ;
#57611 = CARTESIAN_POINT ( 'NONE',  ( 32.30839531297598910, 123.0650415295850593, -10.00000000000000888 ) ) ;
#57612 = CARTESIAN_POINT ( 'NONE',  ( 134.4004000680750437, 241.7365022471901739, -10.00000000000009059 ) ) ;
#57613 = CARTESIAN_POINT ( 'NONE',  ( 205.2941531242069857, 275.0670916224857478, -13.92605142593109058 ) ) ;
#57614 = CARTESIAN_POINT ( 'NONE',  ( 85.35443477132466228, 48.30880629543902671, -11.80360700664790663 ) ) ;
#57615 = ORIENTED_EDGE ( 'NONE', *, *, #35325, .T. ) ;
#57616 = CARTESIAN_POINT ( 'NONE',  ( 168.2388598609233554, 248.3799976336047166, -1.878115610807055136 ) ) ;
#57617 = VERTEX_POINT ( 'NONE', #99276 ) ;
#57618 = FACE_OUTER_BOUND ( 'NONE', #60611, .T. ) ;
#57619 = CARTESIAN_POINT ( 'NONE',  ( 180.3910019823692323, 289.3959781800792257, -12.70720770915142062 ) ) ;
#57620 = CARTESIAN_POINT ( 'NONE',  ( 164.8489450237687493, 247.1202469751449939, -7.123750760659631531 ) ) ;
#57621 = EDGE_CURVE ( 'NONE', #566, #42468, #38378, .T. ) ;
#57622 = EDGE_LOOP ( 'NONE', ( #87915, #80484, #47185, #83728, #56901 ) ) ;
#57623 = CARTESIAN_POINT ( 'NONE',  ( 76.95433588952691650, 62.91899607007382400, -15.24877360450729036 ) ) ;
#57624 = EDGE_LOOP ( 'NONE', ( #15884, #83113, #23724, #45165 ) ) ;
#57625 = CARTESIAN_POINT ( 'NONE',  ( 189.1366665130657623, 290.3664947348045757, 14.33938321420245110 ) ) ;
#57626 = CARTESIAN_POINT ( 'NONE',  ( 167.6010540021560189, 247.4270797612363708, 3.638657435017179864 ) ) ;
#57627 = CARTESIAN_POINT ( 'NONE',  ( 148.5637841791828464, 247.3923013555409796, 4.594050593750050204 ) ) ;
#57628 = DIRECTION ( 'NONE',  ( -0.000000000000000000, -0.000000000000000000, -1.000000000000000000 ) ) ;
#57629 = VERTEX_POINT ( 'NONE', #76948 ) ;
#57630 = CARTESIAN_POINT ( 'NONE',  ( 25.29680607046014984, 36.64646525600391413, -2.839279412974133887 ) ) ;
#57631 = CIRCLE ( 'NONE', #9113, 70.00000000000001421 ) ;
#57632 = DIRECTION ( 'NONE',  ( -0.8868092729070087277, -0.4621356007560363244, 0.000000000000000000 ) ) ;
#57633 = CARTESIAN_POINT ( 'NONE',  ( 164.7481050786816468, 274.5153366401211770, 14.74424062371369004 ) ) ;
#57634 = CYLINDRICAL_SURFACE ( 'NONE', #1212, 10.00000000000010658 ) ;
#57635 = CONICAL_SURFACE ( 'NONE', #77011, 9.999999999999998224, 0.7853981633974214116 ) ;
#57636 = ORIENTED_EDGE ( 'NONE', *, *, #95305, .F. ) ;
#57637 = VERTEX_POINT ( 'NONE', #90718 ) ;
#57638 = CARTESIAN_POINT ( 'NONE',  ( 185.7832802462722555, 297.7360824256689966, 1.038627234575328240 ) ) ;
#57640 = CARTESIAN_POINT ( 'NONE',  ( -38.61298035630893111, 26.97617139035147460, 10.00000000000000000 ) ) ;
#57639 = CARTESIAN_POINT ( 'NONE',  ( 164.0777181605478745, 246.4560510864015441, 5.763760713451748785 ) ) ;
#57641 = CARTESIAN_POINT ( 'NONE',  ( 85.76547152072677704, 48.63404149359708128, -11.87225177386112485 ) ) ;
#57642 = CARTESIAN_POINT ( 'NONE',  ( 79.99999999999990052, 93.06504152958508769, 54.99999999999999289 ) ) ;
#57643 = CARTESIAN_POINT ( 'NONE',  ( -16.99542894172669349, 24.36904009834038476, -10.00000000000000000 ) ) ;
#57644 = CARTESIAN_POINT ( 'NONE',  ( 205.2391015854675516, 275.1624436846170738, -14.01434138479280911 ) ) ;
#57645 = CARTESIAN_POINT ( 'NONE',  ( 207.7489713718107396, 270.8152216942889368, -5.185099786540344979 ) ) ;
#57646 = CARTESIAN_POINT ( 'NONE',  ( 169.8538121856582563, 267.4705051540672116, 17.20835523141332146 ) ) ;
#57647 = CARTESIAN_POINT ( 'NONE',  ( -11.52846477932265756, 34.95471236983288321, 59.99999999999999289 ) ) ;
#57648 = CARTESIAN_POINT ( 'NONE',  ( 101.4736528484039724, 220.2048013555409796, 4.594050593750051981 ) ) ;
#57649 = EDGE_LOOP ( 'NONE', ( #1751, #51688, #48439, #25366 ) ) ;
#57650 = CARTESIAN_POINT ( 'NONE',  ( -19.65312891409030271, 93.06504152958497400, 59.99999999999999289 ) ) ;
#57651 = DIRECTION ( 'NONE',  ( -0.8660254037844377084, -0.5000000000000014433, -0.000000000000000000 ) ) ;
#57652 = CARTESIAN_POINT ( 'NONE',  ( 166.2874581756877035, 279.2881603620531337, -13.76640555504497954 ) ) ;
#57653 = ORIENTED_EDGE ( 'NONE', *, *, #88378, .F. ) ;
#57654 = ORIENTED_EDGE ( 'NONE', *, *, #8315, .T. ) ;
#57655 = CARTESIAN_POINT ( 'NONE',  ( 86.90364953904725098, 45.87765456670206277, -8.164248709133197224 ) ) ;
#57656 = CARTESIAN_POINT ( 'NONE',  ( 71.40026156493414078, 59.28187485775010401, 15.24249285347964289 ) ) ;
#57657 = CARTESIAN_POINT ( 'NONE',  ( 163.2352853045945267, 249.3765732455295563, 10.26252278998509659 ) ) ;
#57658 = CARTESIAN_POINT ( 'NONE',  ( 159.6962080797732710, 254.0450491601782232, -15.33973334987084947 ) ) ;
#57659 = CARTESIAN_POINT ( 'NONE',  ( 207.0998140485927479, 271.3089257990250758, -4.582213832299882661 ) ) ;
#57660 = CARTESIAN_POINT ( 'NONE',  ( 91.83912023130210400, 214.6423013555409796, -4.594050593750043987 ) ) ;
#57661 = ORIENTED_EDGE ( 'NONE', *, *, #14043, .T. ) ;
#57662 = VERTEX_POINT ( 'NONE', #6568 ) ;
#57663 = LINE ( 'NONE', #73391, #9122 ) ;
#57664 = CARTESIAN_POINT ( 'NONE',  ( 208.2912792141756029, 269.8759169579697641, -2.198672330625011995 ) ) ;
#57665 = EDGE_LOOP ( 'NONE', ( #39552, #37309, #14642, #62749, #51149, #35450 ) ) ;
#57666 = CARTESIAN_POINT ( 'NONE',  ( 75.95690509902382814, 65.20561023377018728, -14.47468716891346219 ) ) ;
#57667 = CARTESIAN_POINT ( 'NONE',  ( 153.6201142527220895, 265.1962041066475990, 16.40937927818958642 ) ) ;
#57669 = ADVANCED_FACE ( 'NONE', ( #13669 ), #27115, .F. ) ;
#57668 = VECTOR ( 'NONE', #5492, 1000.000000000000000 ) ;
#57670 = CARTESIAN_POINT ( 'NONE',  ( 5.181765596169280563, 27.61866642244642733, 10.00000000000000000 ) ) ;
#57672 = DIRECTION ( 'NONE',  ( 0.4999999999999992784, -0.8660254037844390407, 0.000000000000000000 ) ) ;
#57671 = CARTESIAN_POINT ( 'NONE',  ( 135.2750994722765654, 261.1589784336661637, -6.496448406907675876E-16 ) ) ;
#57673 = CARTESIAN_POINT ( 'NONE',  ( -13.92449252947024263, 172.7677522451419350, -5.000000000000047962 ) ) ;
#57674 = PLANE ( 'NONE',  #78775 ) ;
#57675 = ORIENTED_EDGE ( 'NONE', *, *, #15902, .F. ) ;
#57676 = CARTESIAN_POINT ( 'NONE',  ( 86.04035583496818163, 43.88013096475103225, -5.118424826341424705 ) ) ;
#57677 = CARTESIAN_POINT ( 'NONE',  ( 157.1320038828994257, 274.0846122766332087, 13.24865132448945104 ) ) ;
#57678 = CYLINDRICAL_SURFACE ( 'NONE', #9612, 10.00000000000010658 ) ;
#57679 = CARTESIAN_POINT ( 'NONE',  ( 189.4938711747170146, 269.6765502774059087, 15.12816668017716459 ) ) ;
#57680 = CARTESIAN_POINT ( 'NONE',  ( 167.4011299790239775, 281.5488363183706042, 12.98604958840868662 ) ) ;
#57681 = VECTOR ( 'NONE', #44323, 1000.000000000000227 ) ;
#57682 = PLANE ( 'NONE',  #90495 ) ;
#57683 = EDGE_CURVE ( 'NONE', #76974, #79042, #79504, .T. ) ;
#57684 = CARTESIAN_POINT ( 'NONE',  ( 195.8015466934768654, 279.9124873149544896, -16.84388544808167154 ) ) ;
#57685 = DIRECTION ( 'NONE',  ( -1.000000000000000000, 0.000000000000000000, 0.000000000000000000 ) ) ;
#57686 = CARTESIAN_POINT ( 'NONE',  ( 79.29854305342225018, 47.63708018034404290, 13.57368722073299239 ) ) ;
#57687 = CARTESIAN_POINT ( 'NONE',  ( 70.36141869169587437, 70.50703831449676784, -4.583400824472941615 ) ) ;
#57688 = CARTESIAN_POINT ( 'NONE',  ( 167.7122741723079002, 249.7662244187599185, 7.851770579763321933 ) ) ;
#57689 = CARTESIAN_POINT ( 'NONE',  ( 78.07729254143889364, 61.93885312825283052, 15.69741212657180540 ) ) ;
#57690 = CARTESIAN_POINT ( 'NONE',  ( 207.6875671281972870, 270.9215769640275653, -2.211577121115235300 ) ) ;
#57691 = EDGE_CURVE ( 'NONE', #62885, #2192, #4412, .T. ) ;
#57692 = CARTESIAN_POINT ( 'NONE',  ( 162.9298729957551473, 248.4441772310448755, -10.24417153209544651 ) ) ;
#57693 = VECTOR ( 'NONE', #13463, 1000.000000000000000 ) ;
#57694 = CARTESIAN_POINT ( 'NONE',  ( 71.00220796100531118, 64.77528057016907326, -12.50717593332708866 ) ) ;
#57695 = CARTESIAN_POINT ( 'NONE',  ( 185.2999266589457932, 266.4615743673832071, 13.16452756711701966 ) ) ;
#57696 = CARTESIAN_POINT ( 'NONE',  ( 184.7144364183202185, 266.1639934807288341, -14.90341959938623617 ) ) ;
#57697 = CARTESIAN_POINT ( 'NONE',  ( 31.86369474034375671, 37.13478043621390157, 8.090169943749478065 ) ) ;
#57698 = CARTESIAN_POINT ( 'NONE',  ( 77.93902080370800434, 47.95641163770635274, 14.13009455829524796 ) ) ;
#57699 = CARTESIAN_POINT ( 'NONE',  ( 203.2369479875374623, 278.6302754407888074, -16.66242713208754367 ) ) ;
#57700 = CARTESIAN_POINT ( 'NONE',  ( 157.6996016306053150, 271.0617617641458423, -14.71839889293659986 ) ) ;
#57701 = AXIS2_PLACEMENT_3D ( 'NONE', #28254, #57651, #58640 ) ;
#57702 = CARTESIAN_POINT ( 'NONE',  ( 83.66935810104509130, 43.26081338140035371, -6.695904667356427531 ) ) ;
#57703 = CARTESIAN_POINT ( 'NONE',  ( 17.63104780087548562, 190.1744531367911293, 4.594050593750047540 ) ) ;
#57704 = CARTESIAN_POINT ( 'NONE',  ( 90.45192255479418009, 211.4824982072973683, 3.021315404115420679E-15 ) ) ;
#57705 = ORIENTED_EDGE ( 'NONE', *, *, #20140, .F. ) ;
#57706 = CARTESIAN_POINT ( 'NONE',  ( 86.89976093607516816, 45.97909969559822940, 8.962991326411129833 ) ) ;
#57707 = CARTESIAN_POINT ( 'NONE',  ( 192.7619763870382315, 275.9402076810760036, 17.00737747304665959 ) ) ;
#57708 = CARTESIAN_POINT ( 'NONE',  ( 82.19706587503785045, 41.28416451854318581, 5.427054723112330059 ) ) ;
#57709 = CARTESIAN_POINT ( 'NONE',  ( 34.97905304013878691, 184.8768266524160140, 9.188101187500096856 ) ) ;
#57710 = LINE ( 'NONE', #18738, #89525 ) ;
#57711 = CARTESIAN_POINT ( 'NONE',  ( 147.5492216329511166, 275.0842468449245644, 4.751613690710122739 ) ) ;
#57712 = CARTESIAN_POINT ( 'NONE',  ( 34.30168821287347924, 42.73705186507756792, -3.090169943749475845 ) ) ;
#57713 = CARTESIAN_POINT ( 'NONE',  ( 199.8627835468920466, 267.3049400163769178, -6.768725752350158054 ) ) ;
#57714 = CARTESIAN_POINT ( 'NONE',  ( 177.7927449247031859, 293.7502563218264413, 2.765845172227290760 ) ) ;
#57715 = CARTESIAN_POINT ( 'NONE',  ( 179.3005203053959633, 278.5776234110656446, -17.15738409824242083 ) ) ;
#57716 = CARTESIAN_POINT ( 'NONE',  ( 160.4478367305730444, 269.5427765943644545, 17.02708557859721239 ) ) ;
#57717 = ADVANCED_FACE ( 'NONE', ( #17665 ), #961, .T. ) ;
#57718 = EDGE_CURVE ( 'NONE', #77450, #42396, #63758, .T. ) ;
#57719 = CARTESIAN_POINT ( 'NONE',  ( 166.3765111647684023, 257.7471643095800573, -15.10258006359619465 ) ) ;
#57720 = CARTESIAN_POINT ( 'NONE',  ( 83.70690788325238429, 51.99575818335755883, 14.97781791391902750 ) ) ;
#57721 = CARTESIAN_POINT ( 'NONE',  ( 81.06766895168334486, 217.6115022471902591, 10.00000000000009592 ) ) ;
#57722 = CARTESIAN_POINT ( 'NONE',  ( 75.48012123268173923, 53.33211347945791658, 16.49774674168797617 ) ) ;
#57723 = CARTESIAN_POINT ( 'NONE',  ( 185.2419368458229769, 261.1426024236396870, -10.52247972935524345 ) ) ;
#57724 = CARTESIAN_POINT ( 'NONE',  ( 48.05019010880389629, 207.7369531367911293, -4.594050593750048428 ) ) ;
#57725 = VERTEX_POINT ( 'NONE', #25776 ) ;
#57726 = CARTESIAN_POINT ( 'NONE',  ( -5.084612219170204561, 81.16070385630965234, 13.43819141829553665 ) ) ;
#57727 = CARTESIAN_POINT ( 'NONE',  ( 147.2494378675467033, 275.6034875578896504, 3.639370109197119341 ) ) ;
#57728 = CARTESIAN_POINT ( 'NONE',  ( 67.11837730215745523, 67.11470315592687541, -8.588528573970526381 ) ) ;
#57729 = EDGE_CURVE ( 'NONE', #66666, #11364, #80327, .T. ) ;
#57730 = ORIENTED_EDGE ( 'NONE', *, *, #4586, .F. ) ;
#57731 = CARTESIAN_POINT ( 'NONE',  ( 170.6096849177089894, 286.1922839665126048, 7.471123016262505523 ) ) ;
#57732 = CARTESIAN_POINT ( 'NONE',  ( 164.5867587387928950, 245.5743669417666126, -3.022048486790635202 ) ) ;
#57733 = CARTESIAN_POINT ( 'NONE',  ( 0.4893710859096792598, 78.77562236714182120, 52.49999999999999289 ) ) ;
#57734 = CARTESIAN_POINT ( 'NONE',  ( 30.72569264534336142, 26.24335787977765122, -9.188101187500008038 ) ) ;
#57735 = CARTESIAN_POINT ( 'NONE',  ( 188.5767478252478213, 265.3039102131422737, 10.74219168877824160 ) ) ;
#57736 = CARTESIAN_POINT ( 'NONE',  ( 86.53129273504272589, 47.24044952787517104, -10.15552464530777854 ) ) ;
#57737 = VECTOR ( 'NONE', #56790, 1000.000000000000000 ) ;
#57738 = CARTESIAN_POINT ( 'NONE',  ( 174.0983890414937321, 257.0653133237892121, 11.33330784449225703 ) ) ;
#57739 = ORIENTED_EDGE ( 'NONE', *, *, #2985, .F. ) ;
#57740 = AXIS2_PLACEMENT_3D ( 'NONE', #30474, #22376, #60852 ) ;
#57741 = CARTESIAN_POINT ( 'NONE',  ( 12.86511499041763074, 19.37878583063839244, 9.188101187500006262 ) ) ;
#57742 = EDGE_CURVE ( 'NONE', #62454, #28585, #39158, .T. ) ;
#57743 = DIRECTION ( 'NONE',  ( -0.4330127018922184656, -0.2499999999999943934, 0.8660254037844407060 ) ) ;
#57744 = CARTESIAN_POINT ( 'NONE',  ( 174.7807705099663451, 255.1531767004597953, 8.228258982011636746 ) ) ;
#57745 = EDGE_CURVE ( 'NONE', #23843, #54771, #67535, .T. ) ;
#57747 = ORIENTED_EDGE ( 'NONE', *, *, #19232, .T. ) ;
#57746 = B_SPLINE_CURVE_WITH_KNOTS ( 'NONE', 3,
 ( #57368, #88342, #18899, #49778, #11310, #70572, #32066, #62978, #97886, #88847, #11798, #42167, #43147, #42653, #65475, #89338, #19411, #44149, #13288, #75083, #74088, #74600, #73587, #96417 ),
 .UNSPECIFIED., .F., .F.,
 ( 4, 2, 2, 2, 2, 2, 2, 2, 2, 2, 2, 4 ),
 ( 0.0002774176761712133306, 0.001899884551711553300, 0.002102692911154076423, 0.002153395001014668606, 0.002204097090875261223, 0.002229448135805543654, 0.002254799180735826518, 0.002305501270596266913, 0.002711117989480261482, 0.003116734708364256919, 0.003319543067806199777, 0.003522351427248143069 ),
 .UNSPECIFIED. ) ;
#57748 = CARTESIAN_POINT ( 'NONE',  ( 72.32024965620544776, 71.13684411087814397, -6.061350040765782765 ) ) ;
#57749 = CARTESIAN_POINT ( 'NONE',  ( 164.7396270603856294, 269.0037874151494179, 17.61975801440670608 ) ) ;
#57750 = LINE ( 'NONE', #79615, #12970 ) ;
#57751 = DIRECTION ( 'NONE',  ( -0.06142469166374902451, -0.9981117208278906805, 0.000000000000000000 ) ) ;
#57752 = EDGE_LOOP ( 'NONE', ( #63037, #85883, #66806, #3730 ) ) ;
#57753 = ORIENTED_EDGE ( 'NONE', *, *, #28094, .T. ) ;
#57754 = CIRCLE ( 'NONE', #91775, 17.82106496071138935 ) ;
#57756 = CARTESIAN_POINT ( 'NONE',  ( 151.0052876815146590, 270.5891121319239687, -13.76719987110444876 ) ) ;
#57755 = CARTESIAN_POINT ( 'NONE',  ( 207.8570869662935365, 270.6279599915536664, -5.669188455878507504 ) ) ;
#57757 = DIRECTION ( 'NONE',  ( -0.8660254037844359321, -0.5000000000000051070, -0.000000000000000000 ) ) ;
#57758 = VERTEX_POINT ( 'NONE', #20169 ) ;
#57759 = DIRECTION ( 'NONE',  ( -1.000000000000000000, 0.000000000000000000, 0.000000000000000000 ) ) ;
#57760 = CARTESIAN_POINT ( 'NONE',  ( 197.9598023461055902, 287.7705598106892921, 18.23120408239484291 ) ) ;
#57761 = CARTESIAN_POINT ( 'NONE',  ( 72.80719422333380919, 57.61781679197407868, -16.30664549720600931 ) ) ;
#57762 = CARTESIAN_POINT ( 'NONE',  ( 78.37369994444134136, 61.17973184547403775, -15.89768920957586751 ) ) ;
#57763 = CARTESIAN_POINT ( 'NONE',  ( 157.0887340267001946, 258.5613266995183039, -17.61824281915036394 ) ) ;
#57764 = CARTESIAN_POINT ( 'NONE',  ( 112.7044859340271614, 242.0024278399160949, 9.188101187500095079 ) ) ;
#57765 = CARTESIAN_POINT ( 'NONE',  ( 181.8559320684326224, 273.7276056269956257, 17.73031764801637067 ) ) ;
#57766 = CARTESIAN_POINT ( 'NONE',  ( 74.86346528667428402, 202.4824982072973967, 3.021315404115420679E-15 ) ) ;
#57767 = ORIENTED_EDGE ( 'NONE', *, *, #84708, .T. ) ;
#57768 = AXIS2_PLACEMENT_3D ( 'NONE', #12177, #57757, #43557 ) ;
#57769 = CARTESIAN_POINT ( 'NONE',  ( 201.2806641633649747, 280.3747929596665927, 16.67906474368300707 ) ) ;
#57770 = B_SPLINE_CURVE_WITH_KNOTS ( 'NONE', 3,
 ( #88623, #35354, #58153, #19192, #97198, #82993, #27765, #36345, #59636, #19684, #28249, #89613, #12070, #81020, #20175, #75373, #13078, #82000, #42928, #90608, #59124, #73867, #51042, #43449, #34844, #11581, #42439, #74390, #97684, #73375, #43939, #74878, #98177, #67247, #21175, #44441, #5955, #67756, #75881, #76840, #61631, #7437, #92585, #69238, #29752, #54515, #100168, #85493, #29261, #38330, #8447, #92106, #23127, #6459, #54022, #6941 ),
 .UNSPECIFIED., .F., .F.,
 ( 4, 2, 2, 2, 2, 2, 2, 2, 2, 2, 2, 2, 2, 2, 2, 2, 2, 2, 2, 2, 2, 2, 2, 2, 2, 2, 2, 4 ),
 ( 0.0007988174167732828290, 0.001285921168468543568, 0.001773024920163804525, 0.002016576796011434677, 0.002260128671859065481, 0.002381904609782880666, 0.002503680547706696284, 0.002625456485630511469, 0.002747232423554327087, 0.002990784299402038555, 0.003234336175249749590, 0.003721439926945132627, 0.004695647430335955080, 0.005669854933726776666, 0.006156958685422224756, 0.006400510561269988699, 0.006644062437117751775, 0.006704950406079751742, 0.006765838375041750841, 0.006826726344003750807, 0.006887614312965749039, 0.007009390250889750706, 0.007131166188813752374, 0.007374718064661747903, 0.007618269940509743432, 0.007861821816357739828, 0.008105373692205734490, 0.008592477443901725548 ),
 .UNSPECIFIED. ) ;
#57771 = ORIENTED_EDGE ( 'NONE', *, *, #87641, .F. ) ;
#57772 = CARTESIAN_POINT ( 'NONE',  ( 37.04286019156342746, 27.10170272979929607, -7.433330006724141015 ) ) ;
#57773 = FACE_BOUND ( 'NONE', #23752, .T. ) ;
#57774 = CARTESIAN_POINT ( 'NONE',  ( 75.24181145021050554, 66.45540672401639881, -13.14705475788992040 ) ) ;
#57775 = CARTESIAN_POINT ( 'NONE',  ( 65.45180129215621889, 220.8464784336661637, 1.353441290958777525E-15 ) ) ;
#57776 = LINE ( 'NONE', #51173, #35219 ) ;
#57777 = DIRECTION ( 'NONE',  ( 0.000000000000000000, 1.000000000000000000, -0.000000000000000000 ) ) ;
#57778 = FACE_OUTER_BOUND ( 'NONE', #14160, .T. ) ;
#57779 = CARTESIAN_POINT ( 'NONE',  ( 173.2412943989675398, 277.7050541934257240, 16.79641741871846250 ) ) ;
#57780 = VERTEX_POINT ( 'NONE', #18670 ) ;
#57781 = CARTESIAN_POINT ( 'NONE',  ( 180.3268137483904354, 258.1330830615356149, 10.30874540274224849 ) ) ;
#57782 = AXIS2_PLACEMENT_3D ( 'NONE', #16352, #47246, #78166 ) ;
#57783 = CARTESIAN_POINT ( 'NONE',  ( 155.6281496932864457, 261.0911329737299980, -18.07904265579665548 ) ) ;
#57784 = EDGE_LOOP ( 'NONE', ( #65663, #29486, #61482, #54155, #22158 ) ) ;
#57785 = LINE ( 'NONE', #96338, #69030 ) ;
#57786 = CARTESIAN_POINT ( 'NONE',  ( 67.27025623861466386, 69.09150813649328882, -3.041265173945424838 ) ) ;
#57787 = CARTESIAN_POINT ( 'NONE',  ( 207.1019571622349815, 271.9358831784929293, -5.989975140547304733 ) ) ;
#57788 = CARTESIAN_POINT ( 'NONE',  ( 146.9129474150286683, 276.1863061179126930, -5.016087650759920358 ) ) ;
#57789 = CARTESIAN_POINT ( 'NONE',  ( 80.09487356998278074, 52.84115226274354171, 15.95029973925667832 ) ) ;
#57790 = CARTESIAN_POINT ( 'NONE',  ( 205.7576124508049418, 274.2643565215761328, 10.88614016733041545 ) ) ;
#57791 = EDGE_CURVE ( 'NONE', #72450, #36817, #93592, .T. ) ;
#57792 = CARTESIAN_POINT ( 'NONE',  ( 152.4046781316253316, 270.1998585947901006, -14.67976713775933639 ) ) ;
#57793 = LINE ( 'NONE', #19341, #71982 ) ;
#57794 = CARTESIAN_POINT ( 'NONE',  ( 167.2323824317113008, 256.3428130233486968, 13.71918974570849237 ) ) ;
#57795 = CARTESIAN_POINT ( 'NONE',  ( 208.2175703429120688, 270.0035844679667889, 2.257951022351344150 ) ) ;
#57796 = CARTESIAN_POINT ( 'NONE',  ( 124.8288415870092933, 249.0024278399161517, -9.188101187500093303 ) ) ;
#57797 = VERTEX_POINT ( 'NONE', #50056 ) ;
#57798 = CARTESIAN_POINT ( 'NONE',  ( 84.55722348921307230, 44.16439880798394313, -7.444406649127180309 ) ) ;
#57799 = DIRECTION ( 'NONE',  ( -0.000000000000000000, -0.000000000000000000, 1.000000000000000000 ) ) ;
#57800 = EDGE_CURVE ( 'NONE', #62226, #57476, #49550, .T. ) ;
#57801 = LINE ( 'NONE', #89757, #61910 ) ;
#57802 = CARTESIAN_POINT ( 'NONE',  ( 17.00529913897481293, 33.43149683636511327, -10.00000000000000000 ) ) ;
#57803 = CARTESIAN_POINT ( 'NONE',  ( 75.21950657921868810, 63.51667331280388851, 14.62111120148422394 ) ) ;
#57804 = CARTESIAN_POINT ( 'NONE',  ( 177.2585349158682959, 253.1952230001477915, 4.378219909316201530 ) ) ;
#57805 = VERTEX_POINT ( 'NONE', #35348 ) ;
#57806 = CARTESIAN_POINT ( 'NONE',  ( 177.1394999532559211, 267.7181704969479483, -17.21589890951720037 ) ) ;
#57807 = CARTESIAN_POINT ( 'NONE',  ( 155.1068683166927826, 274.9036901648098592, 12.61603981672170072 ) ) ;
#57809 = CARTESIAN_POINT ( 'NONE',  ( 207.1181895030469491, 269.9077679394811753, 1.745611964362854929 ) ) ;
#57808 = DIRECTION ( 'NONE',  ( -0.3666034970181814012, 0.9303772761487891785, 0.000000000000000000 ) ) ;
#57810 = CARTESIAN_POINT ( 'NONE',  ( 165.0803978706131545, 244.7193588848498678, -1.793249961207334486 ) ) ;
#57811 = PLANE ( 'NONE',  #85548 ) ;
#57812 = EDGE_CURVE ( 'NONE', #61768, #84261, #620, .T. ) ;
#57813 = DIRECTION ( 'NONE',  ( -0.8660254037844387076, -0.4999999999999998890, -0.000000000000000000 ) ) ;
#57814 = CARTESIAN_POINT ( 'NONE',  ( 155.0584575552912554, 280.8822639477641587, 1.046265068571241796 ) ) ;
#57815 = AXIS2_PLACEMENT_3D ( 'NONE', #44380, #98621, #13994 ) ;
#57816 = AXIS2_PLACEMENT_3D ( 'NONE', #7423, #77335, #69225 ) ;
#57817 = LINE ( 'NONE', #26935, #12382 ) ;
#57818 = EDGE_CURVE ( 'NONE', #2619, #79527, #18979, .T. ) ;
#57819 = B_SPLINE_SURFACE_WITH_KNOTS ( 'NONE', 3, 1, ( 
 ( #89986, #42826 ),
 ( #73760, #95612 ),
 ( #4352, #28145 ),
 ( #59017, #20563 ),
 ( #26161, #57038 ),
 ( #18569, #49448 ),
 ( #80402, #10972 ),
 ( #41844, #72792 ),
 ( #3382, #23017 ),
 ( #5845, #75261 ),
 ( #30132, #83378 ),
 ( #98570, #99060 ),
 ( #36731, #53424 ),
 ( #67140, #98062 ),
 ( #45809, #67636 ),
 ( #61526, #14921 ),
 ( #52431, #37234 ),
 ( #84374, #6833 ),
 ( #76734, #44825 ),
 ( #84869, #21549 ),
 ( #7328, #92470 ),
 ( #14446, #90500 ),
 ( #100052, #29153 ),
 ( #29642, #13944 ),
 ( #60024, #91987 ),
 ( #28638, #90988 ),
 ( #61015, #45327 ),
 ( #75760, #15412 ),
 ( #68132, #6346 ),
 ( #38208, #37718 ),
 ( #68628, #74774 ),
 ( #44329, #76261 ),
 ( #69126, #60515 ),
 ( #53910, #5353 ) ),
 .UNSPECIFIED., .T., .F., .F.,
 ( 4, 2, 2, 2, 2, 2, 2, 2, 2, 2, 2, 2, 2, 2, 2, 2, 4 ),
 ( 2, 2 ),
 ( 0.000000000000000000, 0.06250000000000000000, 0.1250000000000000000, 0.1875000000000000000, 0.2500000000000000000, 0.3125000000000000000, 0.3750000000000000000, 0.4375000000000000000, 0.5000000000000000000, 0.5625000000000000000, 0.6250000000000000000, 0.6875000000000000000, 0.7500000000000000000, 0.8125000000000000000, 0.8750000000000000000, 0.9375000000000000000, 1.000000000000000000 ),
 ( 0.000000000000000000, 1.000000000000000000 ),
 .UNSPECIFIED. ) ;
#57820 = CARTESIAN_POINT ( 'NONE',  ( 21.28706459136418871, 17.45404122711133255, -8.090169943749478065 ) ) ;
#57821 = EDGE_CURVE ( 'NONE', #28867, #24384, #28419, .T. ) ;
#57822 = DIRECTION ( 'NONE',  ( 0.1473778574936323582, 0.9890802632347824863, 0.000000000000000000 ) ) ;
#57823 = CARTESIAN_POINT ( 'NONE',  ( 154.8891180328150199, 280.6470120869327616, -0.9323348256675227930 ) ) ;
#57824 = CARTESIAN_POINT ( 'NONE',  ( 169.5939356907569788, 285.2851384293307433, -7.966250160088273802 ) ) ;
#57825 = CARTESIAN_POINT ( 'NONE',  ( 5.968649350820482979, 188.6868197944959320, -37.49999999999994316 ) ) ;
#57826 = CARTESIAN_POINT ( 'NONE',  ( 193.4739544967976883, 288.6957167552757255, 16.02685211616793381 ) ) ;
#57827 = CARTESIAN_POINT ( 'NONE',  ( 132.9389821956409037, 240.8927522451417929, -10.00000000000009059 ) ) ;
#57828 = CARTESIAN_POINT ( 'NONE',  ( 76.56471838561475352, 53.17383487477179926, -15.93209607857030008 ) ) ;
#57829 = ORIENTED_EDGE ( 'NONE', *, *, #21052, .T. ) ;
#57830 = CARTESIAN_POINT ( 'NONE',  ( 157.6335212189247557, 257.6177276032722716, 16.76495363836117036 ) ) ;
#57831 = CARTESIAN_POINT ( 'NONE',  ( 190.5893431400089923, 300.5365696307625853, -0.3099240395267599535 ) ) ;
#57832 = CARTESIAN_POINT ( 'NONE',  ( -5.047471817081990331, 158.7048013555409796, 4.594050593750051981 ) ) ;
#57833 = CARTESIAN_POINT ( 'NONE',  ( 36.49425040099653472, 198.0024278399160949, -9.188101187500093303 ) ) ;
#57834 = CARTESIAN_POINT ( 'NONE',  ( 175.4085403292222338, 256.6757290962687534, -10.74039065239221102 ) ) ;
#57835 = CARTESIAN_POINT ( 'NONE',  ( 25.62571989635185332, 15.76426979415090202, 3.090169943749476733 ) ) ;
#57836 = CARTESIAN_POINT ( 'NONE',  ( -69.40242143070358338, 43.82067236826411261, 10.00000000000000000 ) ) ;
#57837 = VECTOR ( 'NONE', #6935, 1000.000000000000227 ) ;
#57838 = CARTESIAN_POINT ( 'NONE',  ( 205.3465787480556344, 274.9762877783610406, -13.79319041940166279 ) ) ;
#57839 = CARTESIAN_POINT ( 'NONE',  ( 72.01037534753049840, 72.25474680761037405, -3.568257732133948590 ) ) ;
#57840 = CARTESIAN_POINT ( 'NONE',  ( 147.4963928429778264, 275.1757489932608109, 4.929816573182678852 ) ) ;
#57841 = CARTESIAN_POINT ( 'NONE',  ( 73.92320082988518948, 55.40069282120870042, -16.11615024270321328 ) ) ;
#57842 = EDGE_CURVE ( 'NONE', #511, #34323, #14105, .T. ) ;
#57843 = CARTESIAN_POINT ( 'NONE',  ( 74.41009865654255862, 213.7677522451418497, 10.00000000000009592 ) ) ;
#57844 = CARTESIAN_POINT ( 'NONE',  ( 76.01760950601774880, 55.66421313266628346, 16.60722370189778019 ) ) ;
#57845 = CARTESIAN_POINT ( 'NONE',  ( 23.79565599918673158, 37.23654200823203553, 1.583844403245397769 ) ) ;
#57846 = DIRECTION ( 'NONE',  ( -0.8660254037844387076, -0.4999999999999998890, -0.000000000000000000 ) ) ;
#57847 = ADVANCED_FACE ( 'NONE', ( #68234 ), #5454, .T. ) ;
#57848 = CARTESIAN_POINT ( 'NONE',  ( 180.0741617902815221, 294.2070188947237739, 1.027227668438557506 ) ) ;
#57849 = CARTESIAN_POINT ( 'NONE',  ( 42.09652578138363310, 185.1115022471902023, -5.000000000000041744 ) ) ;
#57850 = LINE ( 'NONE', #42639, #27998 ) ;
#57851 = B_SPLINE_CURVE_WITH_KNOTS ( 'NONE', 3,
 ( #39741, #32673, #15455, #1285, #32169, #85944, #78794, #63573, #86438, #77277, #77799, #7369, #23060, #275, #92512, #45853, #31655, #54447, #38765, #16472, #46353, #63073, #94016, #62051, #7888, #39249, #46873, #54965, #8382, #24568, #47367, #78290, #70160, #769, #16965, #47855, #9380, #71198, #84419, #76776, #69168, #100100, #30684, #61564, #11893, #17994 ),
 .UNSPECIFIED., .F., .F.,
 ( 4, 2, 2, 2, 2, 2, 2, 2, 2, 2, 2, 2, 2, 2, 2, 2, 2, 2, 2, 2, 2, 2, 4 ),
 ( 0.0009592261741756381941, 0.001443980160452349847, 0.001928734146729061717, 0.002171111139867377103, 0.002413488133005692489, 0.002534676629574850616, 0.002655865126144008742, 0.002777053622713166435, 0.002898242119282324562, 0.003140619112420641248, 0.003382996105558959236, 0.003867750091835591743, 0.004837258064388857623, 0.005806766036942124370, 0.006291520023218749071, 0.006776274009495372903, 0.006897462506064565291, 0.006958056754349161918, 0.007018651002633757678, 0.007261027995772108626, 0.007745781982048733326, 0.008230535968325358026, 0.008715289954601980124 ),
 .UNSPECIFIED. ) ;
#57852 = CARTESIAN_POINT ( 'NONE',  ( 163.3543347837650686, 247.7089878483399730, 10.92686688779373405 ) ) ;
#57853 = CARTESIAN_POINT ( 'NONE',  ( 3.179769518870181777, 163.4548013555410080, -4.594050593750042211 ) ) ;
#57854 = CARTESIAN_POINT ( 'NONE',  ( 33.90715327291019321, 42.68290643055189548, 3.479690158560446702E-15 ) ) ;
#57855 = CARTESIAN_POINT ( 'NONE',  ( 162.0143583332327921, 251.6182954191690726, 13.01856005289551277 ) ) ;
#57856 = CARTESIAN_POINT ( 'NONE',  ( 153.3920560952016956, 264.9641606960921649, 16.50453917291963535 ) ) ;
#57857 = CARTESIAN_POINT ( 'NONE',  ( 33.43441462842632461, 34.70171378149921537, -9.188101187500004485 ) ) ;
#57858 = DIRECTION ( 'NONE',  ( -0.8660254037844387076, -0.4999999999999998890, -0.000000000000000000 ) ) ;
#57859 = CARTESIAN_POINT ( 'NONE',  ( 179.4673683373077893, 277.3829114355249317, 16.47530701906485717 ) ) ;
#57860 = ADVANCED_FACE ( 'NONE', ( #91086 ), #82987, .T. ) ;
#57861 = CARTESIAN_POINT ( 'NONE',  ( 154.8679462054080318, 262.4078440388265676, 17.98338675682672871 ) ) ;
#57862 = CARTESIAN_POINT ( 'NONE',  ( 41.47628181354097165, 29.11029122506297995, -8.090169943749478065 ) ) ;
#57863 = CARTESIAN_POINT ( 'NONE',  ( 145.5865615336240353, 244.8615022471901739, 5.000000000000051514 ) ) ;
#57864 =( NAMED_UNIT ( * ) PLANE_ANGLE_UNIT ( ) SI_UNIT ( $, .RADIAN. ) );
#57865 = CARTESIAN_POINT ( 'NONE',  ( 12.18311320154372801, 9.960047579820882291, -5.678558825948276656 ) ) ;
#57866 = CARTESIAN_POINT ( 'NONE',  ( 71.90400658755810070, 72.53437165389429708, 1.750395423964758557 ) ) ;
#57867 = CARTESIAN_POINT ( 'NONE',  ( 16.80672687576512203, 25.10171378149917842, 9.188101187500008038 ) ) ;
#57868 = DIRECTION ( 'NONE',  ( 0.5000000000000001110, -0.8660254037844384856, -0.000000000000000000 ) ) ;
#57869 = EDGE_CURVE ( 'NONE', #61372, #17056, #22137, .T. ) ;
#57870 = CARTESIAN_POINT ( 'NONE',  ( 153.1651950822421213, 277.6376015683730998, -5.200947853335143201 ) ) ;
#57871 = ORIENTED_EDGE ( 'NONE', *, *, #8317, .T. ) ;
#57872 = CARTESIAN_POINT ( 'NONE',  ( 105.6772241758911264, 238.4865022471902876, -10.00000000000009592 ) ) ;
#57873 = EDGE_CURVE ( 'NONE', #99391, #21781, #37331, .T. ) ;
#57874 = CARTESIAN_POINT ( 'NONE',  ( -110.0000000000000000, 0.000000000000000000, -59.99999999999999289 ) ) ;
#57875 = ORIENTED_EDGE ( 'NONE', *, *, #4979, .T. ) ;
#57877 = CARTESIAN_POINT ( 'NONE',  ( 153.4389798490260262, 264.8828863703868137, 16.68923469758090761 ) ) ;
#57876 =( BOUNDED_CURVE ( )  B_SPLINE_CURVE ( 2, ( #55338, #40641, #25976, #78171, #87342, #33055, #56846, #85828, #2675 ),
 .UNSPECIFIED., .F., .T. ) 
 B_SPLINE_CURVE_WITH_KNOTS ( ( 3, 2, 2, 2, 3 ),
 ( 0.8508064516129032473, 0.8521505376344086224, 0.8548387096774193727, 0.8575268817204301230, 0.8588709677419354982 ),
 .UNSPECIFIED. ) 
 CURVE ( )  GEOMETRIC_REPRESENTATION_ITEM ( )  RATIONAL_B_SPLINE_CURVE ( ( 0.9330127018922194093, 0.9330127018922194093, 1.000000000000000000, 0.8660254037844387076, 1.000000000000000000, 0.8660254037844387076, 1.000000000000000000, 0.9330127018922194093, 0.9330127018922194093 ) ) 
 REPRESENTATION_ITEM ( '' )  );
#57878 = CARTESIAN_POINT ( 'NONE',  ( 164.4440639631384045, 245.8215215431751233, -2.910115319305802029 ) ) ;
#57879 = CARTESIAN_POINT ( 'NONE',  ( 66.27858692599893686, 68.56926275514072699, 4.816128439524981708 ) ) ;
#57880 = CARTESIAN_POINT ( 'NONE',  ( 125.2349645446897455, 233.1115022471901739, -5.000000000000041744 ) ) ;
#57881 = ORIENTED_EDGE ( 'NONE', *, *, #45583, .T. ) ;
#57882 = ORIENTED_EDGE ( 'NONE', *, *, #70803, .T. ) ;
#57884 = CARTESIAN_POINT ( 'NONE',  ( 204.7235752877335244, 276.0553614249301972, 14.82397698933823271 ) ) ;
#57883 = CARTESIAN_POINT ( 'NONE',  ( 164.5368030896599691, 246.5300180790061404, -4.380742116717776469 ) ) ;
#57885 = CARTESIAN_POINT ( 'NONE',  ( 192.0331311261993790, 298.0358554833232461, 11.82583305898340953 ) ) ;
#57886 = VERTEX_POINT ( 'NONE', #29745 ) ;
#57887 = VECTOR ( 'NONE', #49884, 1000.000000000000000 ) ;
#57888 = CARTESIAN_POINT ( 'NONE',  ( 193.4764931876557341, 292.8054267365567966, 15.43080237163636070 ) ) ;
#57889 = CARTESIAN_POINT ( 'NONE',  ( 178.1396926282777997, 263.7657380533013907, 15.23609645299708326 ) ) ;
#57890 = B_SPLINE_CURVE_WITH_KNOTS ( 'NONE', 3,
 ( #91894, #69037, #78157, #8253, #1155, #16344, #7237, #30551, #9252, #32029, #85816, #93382, #8745, #39118 ),
 .UNSPECIFIED., .F., .F.,
 ( 4, 2, 2, 2, 2, 2, 4 ),
 ( 0.001181140099763508013, 0.001412183555258165199, 0.001643227010752822386, 0.001874270466247479790, 0.002105313921742136760, 0.002567400832731370035, 0.003029487743720602876 ),
 .UNSPECIFIED. ) ;
#57891 = ORIENTED_EDGE ( 'NONE', *, *, #57578, .T. ) ;
#57892 = DIRECTION ( 'NONE',  ( -0.7300871660154473197, -0.6833540297821713017, 0.000000000000000000 ) ) ;
#57893 = CARTESIAN_POINT ( 'NONE',  ( 77.74234477000247523, 50.56326866554580590, -15.20697261137338074 ) ) ;
#57894 = AXIS2_PLACEMENT_3D ( 'NONE', #63666, #94605, #73776 ) ;
#57895 = CARTESIAN_POINT ( 'NONE',  ( 81.28922747573520269, 43.24881869083999675, 9.615907131230160942 ) ) ;
#57896 = ORIENTED_EDGE ( 'NONE', *, *, #33447, .T. ) ;
#57897 = CARTESIAN_POINT ( 'NONE',  ( 200.8551880497955437, 282.7556046643899776, 18.00894873733387058 ) ) ;
#57898 = CARTESIAN_POINT ( 'NONE',  ( 166.2168471871404734, 273.8149888340271900, -15.47012930002172837 ) ) ;
#57899 = AXIS2_PLACEMENT_3D ( 'NONE', #18046, #26635, #79878 ) ;
#57900 = CARTESIAN_POINT ( 'NONE',  ( -76.49344163160110099, 52.20945622995200353, 10.00000000000000000 ) ) ;
#57901 = VERTEX_POINT ( 'NONE', #23121 ) ;
#57902 = CARTESIAN_POINT ( 'NONE',  ( 190.0259678364800493, 301.5123642802043946, 4.004183174499006626 ) ) ;
#57903 = CARTESIAN_POINT ( 'NONE',  ( 203.0398866899141126, 278.9715956204779559, 16.57839218037009132 ) ) ;
#57904 = ORIENTED_EDGE ( 'NONE', *, *, #18282, .F. ) ;
#57905 = CARTESIAN_POINT ( 'NONE',  ( 156.8156315612123137, 266.4525211182331077, -16.29134938265778842 ) ) ;
#57906 = ORIENTED_EDGE ( 'NONE', *, *, #77673, .T. ) ;
#57907 = CARTESIAN_POINT ( 'NONE',  ( 157.1309033697166910, 269.5518756982808668, 15.81807010761959731 ) ) ;
#57908 = ORIENTED_EDGE ( 'NONE', *, *, #87119, .F. ) ;
#57909 = CIRCLE ( 'NONE', #78988, 70.00000000000001421 ) ;
#57910 = CARTESIAN_POINT ( 'NONE',  ( 159.0726324473315003, 259.5960639973407638, 16.73037245408614027 ) ) ;
#57911 = CARTESIAN_POINT ( 'NONE',  ( 193.6284877719895974, 295.2726167166218829, 14.91976605476162021 ) ) ;
#57912 = CARTESIAN_POINT ( 'NONE',  ( -19.77743847219115736, 93.13331211188449288, 59.99999999999999289 ) ) ;
#57913 = CARTESIAN_POINT ( 'NONE',  ( 138.2253456014563255, 250.6115022471902591, 10.00000000000009592 ) ) ;
#57914 = CARTESIAN_POINT ( 'NONE',  ( -73.81593683174928344, 48.72104262922893270, 177.5919119679930134 ) ) ;
#57915 = CARTESIAN_POINT ( 'NONE',  ( 164.5329775610532010, 278.6465748849269062, -13.92721442706176482 ) ) ;
#57916 = CARTESIAN_POINT ( 'NONE',  ( 158.7792683104916307, 255.6332354280542063, -16.04672224821257487 ) ) ;
#57917 = VECTOR ( 'NONE', #29473, 1000.000000000000114 ) ;
#57918 = ORIENTED_EDGE ( 'NONE', *, *, #27159, .F. ) ;
#57919 = LINE ( 'NONE', #10836, #60923 ) ;
#57920 = CARTESIAN_POINT ( 'NONE',  ( 22.11595037535113661, 30.95586893147756413, 7.433330006724141015 ) ) ;
#57921 = CARTESIAN_POINT ( 'NONE',  ( 106.5950644350847369, 243.8967562850346837, -4.648177544792955347E-16 ) ) ;
#57923 = ORIENTED_EDGE ( 'NONE', *, *, #40794, .T. ) ;
#57922 = CARTESIAN_POINT ( 'NONE',  ( 0.9806730298622799991, 159.8262482093458061, 3.021315404115420679E-15 ) ) ;
#57924 = ORIENTED_EDGE ( 'NONE', *, *, #62513, .T. ) ;
#57925 = CARTESIAN_POINT ( 'NONE',  ( 187.1732433188570894, 276.9074010399757526, 16.80578958361036257 ) ) ;
#57926 = CARTESIAN_POINT ( 'NONE',  ( 171.4502695138348543, 259.7973668612793290, -14.48892546229642520 ) ) ;
#57927 = CARTESIAN_POINT ( 'NONE',  ( 163.5859548838263038, 247.8737923133996901, 8.124920029444005820 ) ) ;
#57928 = LINE ( 'NONE', #4225, #81368 ) ;
#57929 = B_SPLINE_CURVE_WITH_KNOTS ( 'NONE', 3,
 ( #29977, #71991, #55745, #1084, #39052, #78089, #93309, #25374, #48691, #77596, #69964, #41055, #79626, #17791, #31962, #54758, #92808, #86235, #93822, #32482, #87258, #86737, #71497, #2596, #8183, #23866, #579, #10189, #31463, #85744, #9701 ),
 .UNSPECIFIED., .F., .F.,
 ( 4, 3, 3, 3, 3, 3, 3, 3, 3, 3, 4 ),
 ( 0.000000000000000000, 0.1333490885032357909, 0.3007194338854210502, 0.4699862290245036545, 0.5844252810809178467, 0.6686540514502550270, 0.7354980260655467061, 0.8028463152565693539, 0.8633854507757410257, 0.9437142632667440134, 1.000000000000000000 ),
 .UNSPECIFIED. ) ;
#57930 = CARTESIAN_POINT ( 'NONE',  ( 159.9421317827104758, 253.6190968119055356, -14.98049406679499640 ) ) ;
#57931 = DIRECTION ( 'NONE',  ( -0.4755282581475737680, 0.8236391035463299648, -0.3090169943749573878 ) ) ;
#57932 = ORIENTED_EDGE ( 'NONE', *, *, #33652, .T. ) ;
#57933 = CARTESIAN_POINT ( 'NONE',  ( 167.4864847214653594, 252.8241918798602228, -12.40380003664212616 ) ) ;
#57934 = CIRCLE ( 'NONE', #90385, 0.1418229129681557177 ) ;
#57935 = FACE_OUTER_BOUND ( 'NONE', #99892, .T. ) ;
#57936 = CARTESIAN_POINT ( 'NONE',  ( 164.9404048476745004, 244.9618339132846074, -2.801285734921658666 ) ) ;
#57937 = CARTESIAN_POINT ( 'NONE',  ( 32.84087927488948822, 189.7677522451418497, 10.00000000000009592 ) ) ;
#57938 = CARTESIAN_POINT ( 'NONE',  ( 105.1271107466783121, 225.3768266524160140, 9.188101187500096856 ) ) ;
#57939 = ADVANCED_FACE ( 'NONE', ( #68733 ), #60617, .T. ) ;
#57940 = CARTESIAN_POINT ( 'NONE',  ( 170.8865616681041786, 262.8912071418242817, 16.88624067591380040 ) ) ;
#57941 = CARTESIAN_POINT ( 'NONE',  ( 162.6515360750312027, 249.5066621596292293, -10.92528266655622815 ) ) ;
#57942 = CARTESIAN_POINT ( 'NONE',  ( 12.26669281485430929, 30.58029201028040944, 1.583844403245363353 ) ) ;
#57943 = CARTESIAN_POINT ( 'NONE',  ( 207.8833583980453739, 270.5824565369721313, 1.564926904161892285 ) ) ;
#57944 = CARTESIAN_POINT ( 'NONE',  ( 19.87790860953014160, 170.0327760586659736, 1.948934522072303157E-15 ) ) ;
#57945 = CARTESIAN_POINT ( 'NONE',  ( 174.8250621633554260, 255.6858076512632465, 11.15776497395374101 ) ) ;
#57946 = ORIENTED_EDGE ( 'NONE', *, *, #17857, .F. ) ;
#57947 = ORIENTED_EDGE ( 'NONE', *, *, #75812, .T. ) ;
#57948 = CARTESIAN_POINT ( 'NONE',  ( 147.5268811534417637, 275.7712507861047584, -0.5032726463638115266 ) ) ;
#57949 = EDGE_CURVE ( 'NONE', #84697, #71153, #6453, .T. ) ;
#57950 = DIRECTION ( 'NONE',  ( -0.8660254037844387076, -0.4999999999999998890, -0.000000000000000000 ) ) ;
#57951 = EDGE_CURVE ( 'NONE', #13801, #62993, #49960, .T. ) ;
#57952 = CARTESIAN_POINT ( 'NONE',  ( 190.4976253092930278, 300.6954295735222900, -5.764807383508308902 ) ) ;
#57953 = CARTESIAN_POINT ( 'NONE',  ( 148.1846401255833996, 275.9836697316168284, -5.368268268079755323 ) ) ;
#57954 = CARTESIAN_POINT ( 'NONE',  ( 207.1211793645798878, 271.9025893473983047, -6.294110402770905388 ) ) ;
#57955 = PLANE ( 'NONE',  #90407 ) ;
#57956 = CARTESIAN_POINT ( 'NONE',  ( 37.98264478980979675, 201.9244531367911293, -4.594050593750046652 ) ) ;
#57957 = CARTESIAN_POINT ( 'NONE',  ( 100.3908607700757472, 218.7677522451417644, -5.000000000000041744 ) ) ;
#57958 = CIRCLE ( 'NONE', #23955, 17.82106496071138224 ) ;
#57959 = ORIENTED_EDGE ( 'NONE', *, *, #91160, .T. ) ;
#57960 = CARTESIAN_POINT ( 'NONE',  ( 79.32558605478153879, 59.69129752972263248, -16.52184683405510768 ) ) ;
#57961 = AXIS2_PLACEMENT_3D ( 'NONE', #52958, #52456, #28662 ) ;
#57962 = CARTESIAN_POINT ( 'NONE',  ( 179.0719375569688623, 258.5579859881011657, -10.02328217832856438 ) ) ;
#57963 = VECTOR ( 'NONE', #14297, 1000.000000000000000 ) ;
#57964 = CARTESIAN_POINT ( 'NONE',  ( 8.700681467995980967, 166.6423013555410080, -4.594050593750043987 ) ) ;
#57965 = VECTOR ( 'NONE', #41339, 1000.000000000000000 ) ;
#57966 = CARTESIAN_POINT ( 'NONE',  ( 72.73269248836916745, 71.16345857084107251, -7.307540741686426422 ) ) ;
#57967 = CARTESIAN_POINT ( 'NONE',  ( 198.5511052797322975, 286.7463930869835167, -17.24711022262289006 ) ) ;
#57968 = CARTESIAN_POINT ( 'NONE',  ( -19.65312891409030271, 93.06504152958497400, 54.99999999999999289 ) ) ;
#57969 = CARTESIAN_POINT ( 'NONE',  ( 146.7842303614460207, 276.4092505945183689, -4.491116827832889236 ) ) ;
#57970 = B_SPLINE_CURVE_WITH_KNOTS ( 'NONE', 3,
 ( #39480, #61795, #54684, #31893 ),
 .UNSPECIFIED., .F., .F.,
 ( 4, 4 ),
 ( 0.01044120455681045272, 0.01649765149563178768 ),
 .UNSPECIFIED. ) ;
#57971 = CARTESIAN_POINT ( 'NONE',  ( 74.17788031095660983, 67.68212350510704312, -12.30096152613073279 ) ) ;
#57972 = CARTESIAN_POINT ( 'NONE',  ( 203.6934353594241713, 276.2490116884532654, 13.33169628994285993 ) ) ;
#57973 = CARTESIAN_POINT ( 'NONE',  ( 68.93032405664872897, 67.85419375520189078, 8.166185397134730906 ) ) ;
#57974 = CARTESIAN_POINT ( 'NONE',  ( 164.2953672501826929, 246.0790718049323687, -2.576662677987826111 ) ) ;
#57975 = VERTEX_POINT ( 'NONE', #69231 ) ;
#57976 = ADVANCED_FACE ( 'NONE', ( #99656 ), #14225, .F. ) ;
#57977 = DIRECTION ( 'NONE',  ( -0.000000000000000000, -1.000000000000000000, -0.000000000000000000 ) ) ;
#57978 = CARTESIAN_POINT ( 'NONE',  ( -9.431985743790550103, 175.3615022471903160, 5.000000000000046185 ) ) ;
#57979 = CARTESIAN_POINT ( 'NONE',  ( -62.06645187246645889, 33.74130844118090522, 10.00000000000000000 ) ) ;
#57980 = CARTESIAN_POINT ( 'NONE',  ( 129.3218690127885964, 233.2202760586659736, -5.415160957724236172E-17 ) ) ;
#57981 = CARTESIAN_POINT ( 'NONE',  ( 20.11807774711229868, 23.56628583063840665, 9.188101187500006262 ) ) ;
#57982 = CARTESIAN_POINT ( 'NONE',  ( 75.25170673533752108, 66.73598490943447814, 12.94887977284632363 ) ) ;
#57983 = CARTESIAN_POINT ( 'NONE',  ( 43.73836560584370403, 189.3927522451417929, 10.00000000000009948 ) ) ;
#57984 = VECTOR ( 'NONE', #62495, 1000.000000000000000 ) ;
#57986 = FACE_OUTER_BOUND ( 'NONE', #6355, .T. ) ;
#57985 = CARTESIAN_POINT ( 'NONE',  ( 196.0727848089514964, 291.0389700598140621, 17.56388901715066808 ) ) ;
#57987 = EDGE_CURVE ( 'NONE', #20542, #57548, #9441, .T. ) ;
#57988 = CARTESIAN_POINT ( 'NONE',  ( 150.2569279433535883, 270.3943619433326830, -14.69852926823082839 ) ) ;
#57989 = ORIENTED_EDGE ( 'NONE', *, *, #85701, .F. ) ;
#57990 = CARTESIAN_POINT ( 'NONE',  ( 150.6453220160077251, 269.7216436761371483, 14.94145576020818034 ) ) ;
#57991 = CARTESIAN_POINT ( 'NONE',  ( 208.0000668123412595, 270.3803116337406891, -0.2337639243167183301 ) ) ;
#57992 = CARTESIAN_POINT ( 'NONE',  ( 189.6738045434663320, 300.1223289962524063, 4.832295392723879424 ) ) ;
#57993 = CARTESIAN_POINT ( 'NONE',  ( 172.4614876683343425, 267.8189099582538120, -16.31738736074272467 ) ) ;
#57994 = CARTESIAN_POINT ( 'NONE',  ( 81.59924320624311633, 55.92250459863397083, -16.38315390958105766 ) ) ;
#57995 = VERTEX_POINT ( 'NONE', #40316 ) ;
#57996 = LINE ( 'NONE', #11918, #13410 ) ;
#57997 = CARTESIAN_POINT ( 'NONE',  ( 80.56131375285130503, 46.02381187782341243, 12.65584631694679274 ) ) ;
#57998 = EDGE_CURVE ( 'NONE', #91452, #184, #96081, .T. ) ;
#57999 = CARTESIAN_POINT ( 'NONE',  ( 84.27505121841375058, 43.30459200202938064, 6.061470481410601074 ) ) ;
#58000 = CARTESIAN_POINT ( 'NONE',  ( -71.61465314115659453, 63.06504152958490295, 20.00000000000001776 ) ) ;
#58001 = CARTESIAN_POINT ( 'NONE',  ( 182.0170707230944060, 295.5524055634063529, 4.928801494141618278 ) ) ;
#58002 = CARTESIAN_POINT ( 'NONE',  ( 72.01497877597556396, 71.50364303677275757, -5.786257741033058011 ) ) ;
#58003 = CARTESIAN_POINT ( 'NONE',  ( 150.7797507404552846, 277.9900660939502473, -8.190901894163754267E-05 ) ) ;
#58004 = CIRCLE ( 'NONE', #1398, 70.00000000000001421 ) ;
#58005 = ORIENTED_EDGE ( 'NONE', *, *, #24461, .F. ) ;
#58006 = CARTESIAN_POINT ( 'NONE',  ( 194.3983564485891975, 282.9291968243864517, 17.33109156482955626 ) ) ;
#58007 = CARTESIAN_POINT ( 'NONE',  ( 10.72711477659875534, 18.14441083166259361, 10.00000000000000533 ) ) ;
#58008 = DIRECTION ( 'NONE',  ( -0.000000000000000000, -0.000000000000000000, -1.000000000000000000 ) ) ;
#58009 = ORIENTED_EDGE ( 'NONE', *, *, #20721, .F. ) ;
#58010 = CARTESIAN_POINT ( 'NONE',  ( 161.5515493166768977, 252.8315038724842623, 14.92355679770252053 ) ) ;
#58011 = CARTESIAN_POINT ( 'NONE',  ( 196.4164021072083983, 270.5621661862001019, 13.33908636140236936 ) ) ;
#58012 = CARTESIAN_POINT ( 'NONE',  ( 159.7180752573169684, 264.1341207546815895, -17.45630029751305656 ) ) ;
#58013 = ORIENTED_EDGE ( 'NONE', *, *, #13054, .T. ) ;
#58014 = PLANE ( 'NONE',  #50633 ) ;
#58015 = CARTESIAN_POINT ( 'NONE',  ( 184.8456707333363909, 292.0357465481239387, 12.28532852304464207 ) ) ;
#58016 = B_SPLINE_CURVE_WITH_KNOTS ( 'NONE', 3,
 ( #27341, #72962, #10648, #49627 ),
 .UNSPECIFIED., .F., .F.,
 ( 4, 4 ),
 ( 0.01255948763041959439, 0.01883562040667947218 ),
 .UNSPECIFIED. ) ;
#58017 = CARTESIAN_POINT ( 'NONE',  ( 74.99511382823338579, 53.05528727595338978, -16.49829891682232486 ) ) ;
#58018 = CIRCLE ( 'NONE', #14340, 7.500000000000000000 ) ;
#58019 = CARTESIAN_POINT ( 'NONE',  ( 105.0000000000000000, 10.00000000000003197, -14.21260523776213347 ) ) ;
#58020 = ORIENTED_EDGE ( 'NONE', *, *, #90808, .T. ) ;
#58021 = CARTESIAN_POINT ( 'NONE',  ( 87.26533679362427165, 215.0643266524160140, 9.188101187500095079 ) ) ;
#58022 = CARTESIAN_POINT ( 'NONE',  ( 79.94457760174631744, 51.39983459170911573, -15.10834372778664658 ) ) ;
#58023 = CARTESIAN_POINT ( 'NONE',  ( 185.4243904228094095, 269.9367370257660355, 16.45094022865727368 ) ) ;
#58024 = CARTESIAN_POINT ( 'NONE',  ( 185.2398828118039660, 259.7113007520022734, -6.730862835317267034 ) ) ;
#58025 = ORIENTED_EDGE ( 'NONE', *, *, #98597, .T. ) ;
#58026 = ORIENTED_EDGE ( 'NONE', *, *, #43789, .F. ) ;
#58027 = CARTESIAN_POINT ( 'NONE',  ( 175.0695970114038005, 258.6570182761398655, 12.72039775904022996 ) ) ;
#58028 = ORIENTED_EDGE ( 'NONE', *, *, #6422, .F. ) ;
#58029 = CARTESIAN_POINT ( 'NONE',  ( 181.9559929377375056, 291.6402902057536721, -11.43735378946719372 ) ) ;
#58030 = VERTEX_POINT ( 'NONE', #54508 ) ;
#58031 = CARTESIAN_POINT ( 'NONE',  ( 75.56522282763701526, 61.49378516209786483, 15.36079468230518685 ) ) ;
#58032 = CARTESIAN_POINT ( 'NONE',  ( 202.9490938173916561, 279.1288534886517709, -16.56031645010252973 ) ) ;
#58033 = ORIENTED_EDGE ( 'NONE', *, *, #55089, .T. ) ;
#58034 = CARTESIAN_POINT ( 'NONE',  ( 207.3202802199240296, 271.5577365501114286, -6.820371601869826605 ) ) ;
#58035 = LINE ( 'NONE', #48947, #88654 ) ;
#58036 = CARTESIAN_POINT ( 'NONE',  ( 80.73992981690828685, 43.57577410340355328, -9.572596457172796391 ) ) ;
#58037 = CARTESIAN_POINT ( 'NONE',  ( 161.7372449923526005, 277.0660816109730717, -12.77480613138230581 ) ) ;
#58039 = EDGE_CURVE ( 'NONE', #40944, #76398, #58035, .T. ) ;
#58038 = CARTESIAN_POINT ( 'NONE',  ( 200.6985908945154335, 283.0268388936558495, -17.74173253065502820 ) ) ;
#58040 = DIRECTION ( 'NONE',  ( 0.000000000000000000, 0.000000000000000000, 1.000000000000000000 ) ) ;
#58042 = CARTESIAN_POINT ( 'NONE',  ( 0.1899651733832354861, 182.4637435831425307, 2.679491924311264039 ) ) ;
#58041 = AXIS2_PLACEMENT_3D ( 'NONE', #91174, #21250, #69334 ) ;
#58043 = CARTESIAN_POINT ( 'NONE',  ( 139.9303331133829715, 251.5958772461660544, -9.188101187500095079 ) ) ;
#58044 = CARTESIAN_POINT ( 'NONE',  ( 70.52664859635549988, 61.35291825783819064, -14.80704222503500844 ) ) ;
#58045 = CARTESIAN_POINT ( 'NONE',  ( 8.350964356584899662, 25.79752408145590792, -5.678558825948271327 ) ) ;
#58046 = VECTOR ( 'NONE', #38214, 1000.000000000000114 ) ;
#58047 = EDGE_LOOP ( 'NONE', ( #33657, #29010, #5061, #56627 ) ) ;
#58048 = VECTOR ( 'NONE', #46399, 1000.000000000000114 ) ;
#58050 = ORIENTED_EDGE ( 'NONE', *, *, #11399, .T. ) ;
#58049 = CARTESIAN_POINT ( 'NONE',  ( 85.48848937474792820, 48.32878387211594884, -12.22513733614603559 ) ) ;
#58051 = CARTESIAN_POINT ( 'NONE',  ( -7.194219815981691468, 36.47589951538922293, 59.99999999999999289 ) ) ;
#58052 = CARTESIAN_POINT ( 'NONE',  ( 78.23198182499388054, 47.91966744817526092, -14.02533881450480813 ) ) ;
#58053 = DIRECTION ( 'NONE',  ( 0.000000000000000000, -0.000000000000000000, -1.000000000000000000 ) ) ;
#58054 = CARTESIAN_POINT ( 'NONE',  ( 155.4334144234936446, 278.1011161893850954, 7.188626922287153498 ) ) ;
#58055 = CARTESIAN_POINT ( 'NONE',  ( 165.5206796362886053, 246.9121039173171539, -1.897138224611882640 ) ) ;
#58056 = CARTESIAN_POINT ( 'NONE',  ( 171.1951747928532086, 280.5720821316805313, 13.82413286205249214 ) ) ;
#58057 = CARTESIAN_POINT ( 'NONE',  ( 168.0789332142355761, 252.9049754911962964, 11.87642061956828421 ) ) ;
#58058 = CARTESIAN_POINT ( 'NONE',  ( 88.09265120180700137, 44.13139543698701317, -1.715510155970429995 ) ) ;
#58059 = VECTOR ( 'NONE', #37562, 1000.000000000000114 ) ;
#58060 = VERTEX_POINT ( 'NONE', #65136 ) ;
#58061 = DIRECTION ( 'NONE',  ( 0.000000000000000000, 0.000000000000000000, 1.000000000000000000 ) ) ;
#58062 = CARTESIAN_POINT ( 'NONE',  ( 66.45864018013874386, 68.94716056944170646, 0.01924691867824903160 ) ) ;
#58063 = ORIENTED_EDGE ( 'NONE', *, *, #82041, .T. ) ;
#58064 = CARTESIAN_POINT ( 'NONE',  ( 163.8880225243198083, 277.8562197680003010, 13.11111227161160997 ) ) ;
#58065 = CARTESIAN_POINT ( 'NONE',  ( 200.9648348225670986, 267.8090230095998550, -2.831290352090367612 ) ) ;
#58066 = CARTESIAN_POINT ( 'NONE',  ( 163.8376739375615614, 246.8718198766768808, -7.388296869948213441 ) ) ;
#58067 = CARTESIAN_POINT ( 'NONE',  ( 190.0445576990143195, 301.4801656937889902, 4.140328216824785912 ) ) ;
#58068 = CARTESIAN_POINT ( 'NONE',  ( 164.5368361882794943, 274.3627312642749416, 14.76381770633092216 ) ) ;
#58070 = CARTESIAN_POINT ( 'NONE',  ( 88.13736778048858866, 44.32197654044805546, 2.735995528162057155 ) ) ;
#58069 = CARTESIAN_POINT ( 'NONE',  ( 160.9899226891051569, 282.1625248316790362, -7.707013335689073763 ) ) ;
#58071 = AXIS2_PLACEMENT_3D ( 'NONE', #83168, #7622, #15712 ) ;
#58072 = CARTESIAN_POINT ( 'NONE',  ( 200.8804270585581833, 268.5305093043455145, 6.050783656218224671 ) ) ;
#58073 = VERTEX_POINT ( 'NONE', #96586 ) ;
#58074 = B_SPLINE_SURFACE_WITH_KNOTS ( 'NONE', 3, 1, ( 
 ( #58391, #96452 ),
 ( #27018, #88882 ),
 ( #57902, #4198 ),
 ( #97426, #81744 ),
 ( #50794, #74123 ),
 ( #4719, #66500 ),
 ( #58875, #89844 ),
 ( #53765, #8192 ),
 ( #29985, #54258 ),
 ( #93320, #13792 ),
 ( #62363, #97 ),
 ( #7686, #587 ),
 ( #39061, #60865 ),
 ( #22879, #69973 ),
 ( #91827, #14296 ),
 ( #45668, #53285 ),
 ( #31472, #15266 ),
 ( #98911, #29492 ),
 ( #37087, #46681 ),
 ( #52773, #68478 ),
 ( #84237, #99900 ),
 ( #52285, #14786 ),
 ( #85229, #60368 ),
 ( #44671, #30980 ),
 ( #61867, #21886 ),
 ( #83733, #46161 ),
 ( #91326, #45182 ),
 ( #6192, #83226 ),
 ( #76592, #22389 ),
 ( #76121, #75604 ),
 ( #6694, #23372 ),
 ( #67991, #7178 ),
 ( #77607, #30487 ),
 ( #37571, #99408 ) ),
 .UNSPECIFIED., .T., .F., .F.,
 ( 4, 2, 2, 2, 2, 2, 2, 2, 2, 2, 2, 2, 2, 2, 2, 2, 4 ),
 ( 2, 2 ),
 ( 0.000000000000000000, 0.06250000000000000000, 0.1250000000000000000, 0.1875000000000000000, 0.2500000000000000000, 0.3125000000000000000, 0.3750000000000000000, 0.4375000000000000000, 0.5000000000000000000, 0.5625000000000000000, 0.6250000000000000000, 0.6875000000000000000, 0.7500000000000000000, 0.8125000000000000000, 0.8750000000000000000, 0.9375000000000000000, 1.000000000000000000 ),
 ( 0.000000000000000000, 1.000000000000000000 ),
 .UNSPECIFIED. ) ;
#58075 = CARTESIAN_POINT ( 'NONE',  ( 77.75329651808065989, 60.51879551299917637, -15.90944513805293425 ) ) ;
#58076 = CARTESIAN_POINT ( 'NONE',  ( 190.2656474672665468, 273.4017421308091684, -16.11817620543089191 ) ) ;
#58077 = ADVANCED_FACE ( 'NONE', ( #4853 ), #11746, .T. ) ;
#58078 = CARTESIAN_POINT ( 'NONE',  ( 70.80625596290352064, 66.10710362255882444, -11.37769121604388367 ) ) ;
#58079 = CYLINDRICAL_SURFACE ( 'NONE', #64713, 10.00000000000010658 ) ;
#58080 = EDGE_CURVE ( 'NONE', #9320, #49412, #75746, .T. ) ;
#58081 = CARTESIAN_POINT ( 'NONE',  ( 80.61734525203304713, 43.35833479104773147, -9.401381521366195315 ) ) ;
#58082 = CARTESIAN_POINT ( 'NONE',  ( 70.48286763772495078, 52.64441083166268243, 0.000000000000000000 ) ) ;
#58083 = CARTESIAN_POINT ( 'NONE',  ( 9.052243966459650792, 176.0333772461660828, 9.188101187500095079 ) ) ;
#58084 = CARTESIAN_POINT ( 'NONE',  ( 110.0524566828198232, 234.3458772461660544, 9.188101187500095079 ) ) ;
#58085 = CARTESIAN_POINT ( 'NONE',  ( 155.3513572141771704, 261.5705516107003064, -17.00592413546589299 ) ) ;
#58086 = CARTESIAN_POINT ( 'NONE',  ( 87.63170318219839316, 44.36446170533410793, -4.079950490519348882 ) ) ;
#58087 = CARTESIAN_POINT ( 'NONE',  ( 180.1973933060313868, 254.8900073420350907, -2.451664709510168016 ) ) ;
#58088 = LINE ( 'NONE', #41886, #94969 ) ;
#58089 = FACE_OUTER_BOUND ( 'NONE', #86595, .T. ) ;
#58090 = DIRECTION ( 'NONE',  ( 0.4999999999999992784, -0.8660254037844390407, 0.000000000000000000 ) ) ;
#58091 = CARTESIAN_POINT ( 'NONE',  ( 147.9500839974939197, 274.3899328626944225, -9.375093207164509224 ) ) ;
#58092 = CARTESIAN_POINT ( 'NONE',  ( 84.40121558736829854, 50.67993577924135451, 13.77038979431789123 ) ) ;
#58093 = CARTESIAN_POINT ( 'NONE',  ( 79.23610557255210551, 54.64639511583943232, -15.99020243353516868 ) ) ;
#58094 = CARTESIAN_POINT ( 'NONE',  ( -76.23101443460923576, 54.01191295053621388, 10.00000000000000000 ) ) ;
#58095 = EDGE_CURVE ( 'NONE', #46807, #39534, #76721, .T. ) ;
#58096 = CARTESIAN_POINT ( 'NONE',  ( 173.1833993531181193, 264.1544810417100848, -15.45454764063065234 ) ) ;
#58097 = CARTESIAN_POINT ( 'NONE',  ( 70.64795371486285092, 223.8464784336661637, 1.353441290958777327E-15 ) ) ;
#58098 = CARTESIAN_POINT ( 'NONE',  ( 207.1211793645798878, 271.9025893473983047, -6.294110402770905388 ) ) ;
#58099 = DIRECTION ( 'NONE',  ( -0.8660254037844387076, -0.4999999999999998890, -0.000000000000000000 ) ) ;
#58100 = AXIS2_PLACEMENT_3D ( 'NONE', #3457, #41931, #11555 ) ;
#58101 = CARTESIAN_POINT ( 'NONE',  ( -16.67133665550712962, 103.7130579026488988, 12.74716765046184896 ) ) ;
#58103 = CARTESIAN_POINT ( 'NONE',  ( -19.58619053749203331, 92.94000956414772929, 59.99999999999999289 ) ) ;
#58102 = CARTESIAN_POINT ( 'NONE',  ( 157.7861133721078772, 257.3534302411229646, 18.03837896619386783 ) ) ;
#58104 = CARTESIAN_POINT ( 'NONE',  ( 198.7829547491859330, 286.3448180261817129, -18.59838968157616179 ) ) ;
#58105 = CARTESIAN_POINT ( 'NONE',  ( 196.8708119716154954, 268.3476497963631573, -11.07389558091716708 ) ) ;
#58106 = CARTESIAN_POINT ( 'NONE',  ( 27.52682148520507965, 37.93396525600392266, 2.839279412974139660 ) ) ;
#58107 = CARTESIAN_POINT ( 'NONE',  ( 80.55977923466276991, 44.53388773495298381, 11.41474457630165062 ) ) ;
#58108 = CARTESIAN_POINT ( 'NONE',  ( 75.82019069382886300, 62.35695433681328126, 15.58349134701113670 ) ) ;
#58109 = EDGE_LOOP ( 'NONE', ( #70582, #54619, #56269, #56507 ) ) ;
#58110 = CARTESIAN_POINT ( 'NONE',  ( 19.41443888993109823, 32.18502408145592852, 5.678558825948277544 ) ) ;
#58111 = VECTOR ( 'NONE', #251, 1000.000000000000000 ) ;
#58112 = CARTESIAN_POINT ( 'NONE',  ( 173.1286500857816293, 289.7119308821054346, -0.9330850667108907537 ) ) ;
#58113 = DIRECTION ( 'NONE',  ( 0.000000000000000000, 1.000000000000000000, 0.000000000000000000 ) ) ;
#58114 = CARTESIAN_POINT ( 'NONE',  ( 191.7217873212802601, 287.9217275298282743, -15.84537559439743326 ) ) ;
#58115 = CARTESIAN_POINT ( 'NONE',  ( 86.17334730086119521, 47.14257514812162952, 10.80675504988608715 ) ) ;
#58116 = CARTESIAN_POINT ( 'NONE',  ( 74.42628153207887465, 62.65944167963375122, 15.19835750912931971 ) ) ;
#58117 = DIRECTION ( 'NONE',  ( -0.8660254037844387076, -0.4999999999999998890, -0.000000000000000000 ) ) ;
#58118 = VECTOR ( 'NONE', #40933, 1000.000000000000000 ) ;
#58119 = CARTESIAN_POINT ( 'NONE',  ( 122.6368883333364295, 231.6115022471901739, -5.000000000000041744 ) ) ;
#58120 = CARTESIAN_POINT ( 'NONE',  ( 157.3198323354746435, 258.1610526871778006, -16.77630483474704093 ) ) ;
#58121 = CARTESIAN_POINT ( 'NONE',  ( 25.25549177415142310, 22.78052372038641238, -10.00000000000000355 ) ) ;
#58122 = VERTEX_POINT ( 'NONE', #28129 ) ;
#58123 = CARTESIAN_POINT ( 'NONE',  ( 166.1868863523491484, 247.3274724192857548, -1.867640438089152033 ) ) ;
#58124 = EDGE_LOOP ( 'NONE', ( #17574, #5575, #89898, #40330 ) ) ;
#58125 = CARTESIAN_POINT ( 'NONE',  ( 202.7865629936218284, 279.4103651332174536, 17.10878160033216133 ) ) ;
#58126 = CARTESIAN_POINT ( 'NONE',  ( 81.53115339410010165, 41.92267797703283350, -7.515177224638171616 ) ) ;
#58127 = EDGE_LOOP ( 'NONE', ( #4980, #86018, #87491, #64763 ) ) ;
#58128 = CARTESIAN_POINT ( 'NONE',  ( 85.47913374364790684, 42.62622548008751266, 0.2499991700750583967 ) ) ;
#58129 = ORIENTED_EDGE ( 'NONE', *, *, #48708, .T. ) ;
#58130 = CARTESIAN_POINT ( 'NONE',  ( 71.99267133948018227, 71.58944556433895912, 5.550980660130552913 ) ) ;
#58131 = CARTESIAN_POINT ( 'NONE',  ( 205.7209699951682182, 274.3278231164531462, 10.82489695893654158 ) ) ;
#58132 = DIRECTION ( 'NONE',  ( -1.000000000000000000, 0.000000000000000000, 0.000000000000000000 ) ) ;
#58133 = CARTESIAN_POINT ( 'NONE',  ( 88.09812594050896450, 44.33653194584124435, -4.440584375772045789 ) ) ;
#58134 = CARTESIAN_POINT ( 'NONE',  ( 195.0052008962354648, 274.1277100424396167, 15.91609426908852498 ) ) ;
#58135 = EDGE_CURVE ( 'NONE', #61485, #17141, #75248, .T. ) ;
#58136 = VECTOR ( 'NONE', #59453, 1000.000000000000000 ) ;
#58137 = CARTESIAN_POINT ( 'NONE',  ( 27.91350267930052809, 31.51421378149921182, -9.188101187500004485 ) ) ;
#58138 = CARTESIAN_POINT ( 'NONE',  ( 72.40300161649089716, 60.75817645194375416, -14.95975737059987409 ) ) ;
#58139 = CARTESIAN_POINT ( 'NONE',  ( 164.5161215291067549, 274.6587578575884550, 14.67424033123101879 ) ) ;
#58140 = CARTESIAN_POINT ( 'NONE',  ( 170.9811431790156462, 280.9458665424763240, 14.82329785628973440 ) ) ;
#58141 = VERTEX_POINT ( 'NONE', #36718 ) ;
#58142 = ORIENTED_EDGE ( 'NONE', *, *, #9427, .T. ) ;
#58143 = CARTESIAN_POINT ( 'NONE',  ( 182.7859092779136745, 296.3208846843115225, 0.2810723611678059286 ) ) ;
#58145 = CARTESIAN_POINT ( 'NONE',  ( 165.3416878791837803, 273.7316169911477459, -15.20817556363227574 ) ) ;
#58144 = CARTESIAN_POINT ( 'NONE',  ( 68.28786865650171478, 65.57955037385437436, 10.43542532682454649 ) ) ;
#58146 = CARTESIAN_POINT ( 'NONE',  ( 85.46201571263348740, 48.63304775035897620, 12.47391791266364791 ) ) ;
#58147 = CARTESIAN_POINT ( 'NONE',  ( 201.3405586841460035, 274.8867726572458423, -14.10034985609714298 ) ) ;
#58148 = CARTESIAN_POINT ( 'NONE',  ( 147.5531173542960062, 275.8601889253673676, 0.6003615892798087605 ) ) ;
#58149 = DIRECTION ( 'NONE',  ( -0.8450603975019854719, 0.5346708562973919721, 0.000000000000000000 ) ) ;
#58151 = LINE ( 'NONE', #11579, #54336 ) ;
#58150 = B_SPLINE_CURVE_WITH_KNOTS ( 'NONE', 3,
 ( #59193, #57714, #19264, #50131, #33954, #97262, #81083, #4524, #89679, #20240, #11649, #42509, #73445, #12647, #74456, #5036, #64841, #66819, #97747, #28315, #90169, #20742, #41520, #51629, #10645, #3068, #84563, #28829, #45008, #74943, #14127, #7508, #67315, #44507, #84074, #6020, #21234, #37899, #21722, #30322, #52113, #98243, #83563, #60196, #53117, #38405, #99235, #61704, #5527, #6530 ),
 .UNSPECIFIED., .F., .F.,
 ( 4, 2, 2, 2, 2, 2, 2, 2, 2, 2, 2, 2, 2, 2, 2, 2, 2, 2, 2, 2, 2, 2, 2, 2, 4 ),
 ( 0.0003069541420656791151, 0.0007786567417661697209, 0.001250359341466660218, 0.001368284991391783764, 0.001486210641316906660, 0.001604136291242029989, 0.001722061941167153318, 0.001957913241017399976, 0.002193764540867646634, 0.002665467140568139950, 0.003137169740268633700, 0.004080574939669620767, 0.005023980139070607399, 0.005495682738771066021, 0.005731534038621340435, 0.005849459688546477208, 0.005908422513509046028, 0.005967385338471614849, 0.006026348163434183669, 0.006085310988396752489, 0.006203236638321890997, 0.006439087938172168013, 0.006910790537872688218, 0.007382493137573210157, 0.007854195737273732963 ),
 .UNSPECIFIED. ) ;
#58152 = DIRECTION ( 'NONE',  ( -0.3696446237802450407, -0.9291732088853839056, 0.000000000000000000 ) ) ;
#58153 = CARTESIAN_POINT ( 'NONE',  ( 181.2447728743449318, 255.8601296356839327, 5.264276447811296222 ) ) ;
#58154 = CARTESIAN_POINT ( 'NONE',  ( 93.32716752435031538, 230.8149278399160949, -9.188101187500095079 ) ) ;
#58155 = VERTEX_POINT ( 'NONE', #12961 ) ;
#58156 = DIRECTION ( 'NONE',  ( 0.9659258262890731972, -0.2588190451025028094, 6.018451495431900886E-15 ) ) ;
#58157 = CARTESIAN_POINT ( 'NONE',  ( 166.8362749997322965, 278.2767805360451803, -13.32482071573584648 ) ) ;
#58158 = EDGE_LOOP ( 'NONE', ( #29035, #76035, #21093, #17784 ) ) ;
#58159 = ORIENTED_EDGE ( 'NONE', *, *, #46654, .F. ) ;
#58160 = CARTESIAN_POINT ( 'NONE',  ( 87.04446681553140763, 45.94690404971670716, -8.147129491944053115 ) ) ;
#58161 = CARTESIAN_POINT ( 'NONE',  ( 71.71749174456839171, 59.03106295208012710, 15.36370853995013697 ) ) ;
#58162 = CARTESIAN_POINT ( 'NONE',  ( 195.7291850945597957, 291.6341022226063160, 17.08310330964873813 ) ) ;
#58163 = CARTESIAN_POINT ( 'NONE',  ( 166.0506673010352472, 274.1027903476490337, -16.62009509085023851 ) ) ;
#58164 = CARTESIAN_POINT ( 'NONE',  ( 163.1177074157340030, 248.1188384722309195, 11.53923137679231026 ) ) ;
#58165 = CARTESIAN_POINT ( 'NONE',  ( 101.7984123748231298, 220.3923013555410080, 4.594050593750050204 ) ) ;
#58166 = VERTEX_POINT ( 'NONE', #60502 ) ;
#58167 =( BOUNDED_CURVE ( )  B_SPLINE_CURVE ( 2, ( #74585, #5164, #36043, #97874, #20878, #5652, #51767, #75072, #90805 ),
 .UNSPECIFIED., .F., .T. ) 
 B_SPLINE_CURVE_WITH_KNOTS ( ( 3, 2, 2, 2, 3 ),
 ( 0.1330645161290322509, 0.1344086021505376261, 0.1370967741935483764, 0.1397849462365591267, 0.1411290322580645296 ),
 .UNSPECIFIED. ) 
 CURVE ( )  GEOMETRIC_REPRESENTATION_ITEM ( )  RATIONAL_B_SPLINE_CURVE ( ( 0.9330127018922194093, 0.9330127018922194093, 1.000000000000000000, 0.8660254037844387076, 1.000000000000000000, 0.8660254037844387076, 1.000000000000000000, 0.9330127018922187432, 0.9330127018922194093 ) ) 
 REPRESENTATION_ITEM ( '' )  );
#58168 = FACE_OUTER_BOUND ( 'NONE', #33331, .T. ) ;
#58169 = DIRECTION ( 'NONE',  ( -0.9874311856918890351, 0.1580495287025880657, 0.000000000000000000 ) ) ;
#58170 = VERTEX_POINT ( 'NONE', #38196 ) ;
#58171 = VECTOR ( 'NONE', #7383, 1000.000000000000227 ) ;
#58172 = CARTESIAN_POINT ( 'NONE',  ( 194.0048607262993698, 265.9479453833899925, -7.746409940373651715 ) ) ;
#58173 = CARTESIAN_POINT ( 'NONE',  ( 29.97214642916971883, 17.70852965304480264, 1.583844403245330712 ) ) ;
#58174 = CARTESIAN_POINT ( 'NONE',  ( 70.49515160751757037, 69.39311819046854168, -7.234649680376111114 ) ) ;
#58176 = DIRECTION ( 'NONE',  ( -0.8660254037844387076, -0.4999999999999998890, -0.000000000000000000 ) ) ;
#58175 = CARTESIAN_POINT ( 'NONE',  ( 138.9021014942714487, 244.8768266524159856, 9.188101187500098632 ) ) ;
#58177 = CARTESIAN_POINT ( 'NONE',  ( -8.223158621222619757, 159.3927522451418213, 10.00000000000009592 ) ) ;
#58178 = CARTESIAN_POINT ( 'NONE',  ( 156.2745578679571565, 265.5782693780779482, -17.38162733845839369 ) ) ;
#58179 = VECTOR ( 'NONE', #25072, 1000.000000000000000 ) ;
#58180 = EDGE_LOOP ( 'NONE', ( #19026, #75134, #47728, #94220, #17915, #80592, #45763, #16664, #51273, #62543, #21187, #64369, #16171, #64790, #29854, #14763, #47304, #30392, #75867, #89754, #71964, #98594, #43946, #88487, #98854, #1842, #15390, #63630, #40235, #56190, #90373, #26278, #95084, #40716, #24127, #96761, #77655, #8217, #22285, #3659, #5543, #8083, #98543, #93240 ) ) ;
#58181 = CARTESIAN_POINT ( 'NONE',  ( 156.9196333786560160, 258.8542176135235877, 18.37000459710097644 ) ) ;
#58182 = CARTESIAN_POINT ( 'NONE',  ( 82.29734961797252879, 53.60383310410945512, 15.81226994477779790 ) ) ;
#58183 = CARTESIAN_POINT ( 'NONE',  ( 82.19743676121389342, 40.60779097105204727, -3.273795677556531114 ) ) ;
#58184 = CARTESIAN_POINT ( 'NONE',  ( 170.5373622343556690, 269.7751423367952270, 17.81562764448176850 ) ) ;
#58185 = CARTESIAN_POINT ( 'NONE',  ( 165.8206990081297931, 283.8978799598649516, 9.576760697357309837 ) ) ;
#58186 = ADVANCED_FACE ( 'NONE', ( #22019 ), #98553, .T. ) ;
#58187 = DIRECTION ( 'NONE',  ( 0.8660254037844385966, 0.5000000000000004441, 0.000000000000000000 ) ) ;
#58188 = CARTESIAN_POINT ( 'NONE',  ( 199.0694199359834045, 281.8589904182013015, -16.59703209974210836 ) ) ;
#58189 = ADVANCED_FACE ( 'NONE', ( #59003 ), #52919, .T. ) ;
#58190 = DIRECTION ( 'NONE',  ( -0.8660254037844387076, -0.4999999999999998890, -0.000000000000000000 ) ) ;
#58191 = VECTOR ( 'NONE', #21107, 1000.000000000000000 ) ;
#58192 = CARTESIAN_POINT ( 'NONE',  ( 80.38896062813260812, 51.85953464289088544, 15.18891967833937962 ) ) ;
#58193 = DIRECTION ( 'NONE',  ( 0.4999999999999998890, -0.8660254037844385966, 0.000000000000000000 ) ) ;
#58194 = EDGE_CURVE ( 'NONE', #82635, #23145, #51429, .T. ) ;
#58195 = CARTESIAN_POINT ( 'NONE',  ( 167.5939664823378337, 249.9752123500401524, 7.239111559830059939 ) ) ;
#58196 = CARTESIAN_POINT ( 'NONE',  ( 78.13090640523601849, 61.76054338150410672, 16.10053832301867871 ) ) ;
#58197 = CARTESIAN_POINT ( 'NONE',  ( 163.3473224498206093, 247.7211335670114352, -10.00320358166632850 ) ) ;
#58198 = DIRECTION ( 'NONE',  ( -0.8660254037844387076, -0.4999999999999998890, -0.000000000000000000 ) ) ;
#58199 = EDGE_CURVE ( 'NONE', #90841, #27648, #46336, .T. ) ;
#58200 = VECTOR ( 'NONE', #39657, 1000.000000000000000 ) ;
#58201 = CARTESIAN_POINT ( 'NONE',  ( 80.13399453211208368, 44.22126075786002275, -11.35348423903955783 ) ) ;
#58202 = CARTESIAN_POINT ( 'NONE',  ( 185.2385187869343213, 266.4459329430754906, 13.17615627545476720 ) ) ;
#58203 = CARTESIAN_POINT ( 'NONE',  ( 10.72711477659875534, 18.14441083166259361, 10.00000000000000533 ) ) ;
#58204 = VECTOR ( 'NONE', #51214, 1000.000000000000000 ) ;
#58205 = CARTESIAN_POINT ( 'NONE',  ( 38.41907791167486153, 30.38052372038643867, 10.00000000000000533 ) ) ;
#58206 = CARTESIAN_POINT ( 'NONE',  ( 192.1883190596398094, 297.7670620978826150, 12.41391288785556668 ) ) ;
#58207 = SURFACE_STYLE_FILL_AREA ( #80561 ) ;
#58208 = CARTESIAN_POINT ( 'NONE',  ( 157.6042236584425780, 270.9851239571572705, -14.73351287006370391 ) ) ;
#58209 = CARTESIAN_POINT ( 'NONE',  ( 86.54608540568763431, 43.64951324792490084, -3.608069729097785672 ) ) ;
#58210 = CARTESIAN_POINT ( 'NONE',  ( 13.97758990260114231, 185.0024278399160949, 9.188101187500095079 ) ) ;
#58211 = CARTESIAN_POINT ( 'NONE',  ( 207.0684042065635992, 270.3832170946865858, 3.383249001289787117 ) ) ;
#58212 = ORIENTED_EDGE ( 'NONE', *, *, #28118, .T. ) ;
#58213 = CARTESIAN_POINT ( 'NONE',  ( 86.94335770270596697, 46.00923847012510493, 8.969699243401572986 ) ) ;
#58214 = CARTESIAN_POINT ( 'NONE',  ( 29.10614472461697133, 197.6115022471903160, -5.000000000000047962 ) ) ;
#58215 = CARTESIAN_POINT ( 'NONE',  ( 71.72615628857761294, 72.05106317348395351, -1.629725736277438441 ) ) ;
#58216 = CARTESIAN_POINT ( 'NONE',  ( 38.76756708593069334, 199.3149278399161517, -9.188101187500095079 ) ) ;
#58217 = CARTESIAN_POINT ( 'NONE',  ( 200.8828793852583203, 282.7076418644388696, 17.90302398138411633 ) ) ;
#58218 = CARTESIAN_POINT ( 'NONE',  ( 190.9441801652054096, 299.9219738747156043, -4.765040093794296716 ) ) ;
#58219 = CARTESIAN_POINT ( 'NONE',  ( 40.62554608437772430, 25.58380873178790083, 6.180339887498953466 ) ) ;
#58220 = CARTESIAN_POINT ( 'NONE',  ( 23.64814127513158226, 118.0650415295850451, -45.00000000000001421 ) ) ;
#58221 = CARTESIAN_POINT ( 'NONE',  ( 146.8637854207107409, 276.2714571898724216, 0.7988785540157756770 ) ) ;
#58222 = CARTESIAN_POINT ( 'NONE',  ( 178.9700315119640663, 278.3247164859652685, -16.90640454279861160 ) ) ;
#58223 = DIRECTION ( 'NONE',  ( 0.000000000000000000, 0.000000000000000000, 1.000000000000000000 ) ) ;
#58224 = CARTESIAN_POINT ( 'NONE',  ( 166.8083734521890449, 257.5796782931630560, -15.79284703031436798 ) ) ;
#58225 = CARTESIAN_POINT ( 'NONE',  ( -19.65312891409030271, 93.06504152958497400, 10.00000000000000888 ) ) ;
#58226 = CARTESIAN_POINT ( 'NONE',  ( 86.26382137438996267, 220.6115022471902591, 10.00000000000009592 ) ) ;
#58227 = PLANE ( 'NONE',  #26426 ) ;
#58228 = CARTESIAN_POINT ( 'NONE',  ( 34.38043361391329711, 31.80066082961424812, 10.00000000000000533 ) ) ;
#58229 = ORIENTED_EDGE ( 'NONE', *, *, #64953, .F. ) ;
#58230 = CARTESIAN_POINT ( 'NONE',  ( 41.74435586355720318, 207.1589784336661637, -6.496448406907675876E-16 ) ) ;
#58231 = ORIENTED_EDGE ( 'NONE', *, *, #83285, .T. ) ;
#58232 = LINE ( 'NONE', #34444, #52941 ) ;
#58233 = CARTESIAN_POINT ( 'NONE',  ( 150.6815632051821581, 269.6588720951601772, -14.68790257316217307 ) ) ;
#58235 = CARTESIAN_POINT ( 'NONE',  ( 67.41728548999284953, 66.73849313723850685, -8.451184109718100856 ) ) ;
#58234 = VECTOR ( 'NONE', #79887, 1000.000000000000227 ) ;
#58236 = ORIENTED_EDGE ( 'NONE', *, *, #33693, .F. ) ;
#58237 = CARTESIAN_POINT ( 'NONE',  ( 167.3858196111910388, 285.2936306680765028, 7.894013122999995247 ) ) ;
#58238 = CARTESIAN_POINT ( 'NONE',  ( 164.9335952247126045, 244.9736285262353306, -1.661461410667423255 ) ) ;
#58239 = CARTESIAN_POINT ( 'NONE',  ( 72.11270410251323426, 62.11537045185059469, 14.87459164730639571 ) ) ;
#58240 = CARTESIAN_POINT ( 'NONE',  ( 34.69977369993912220, 22.96004757982091959, -5.678558825948276656 ) ) ;
#58241 = CARTESIAN_POINT ( 'NONE',  ( 187.1111986486765488, 263.3028977142639633, 11.61052883540825142 ) ) ;
#58242 = CARTESIAN_POINT ( 'NONE',  ( 86.30036054584773808, 46.98594781855085500, -10.02878425733469037 ) ) ;
#58243 = EDGE_CURVE ( 'NONE', #74723, #27875, #39684, .T. ) ;
#58244 = CARTESIAN_POINT ( 'NONE',  ( 171.3908936290850988, 255.6478991229282940, 12.28342243807102996 ) ) ;
#58245 = ORIENTED_EDGE ( 'NONE', *, *, #39446, .F. ) ;
#58246 = CARTESIAN_POINT ( 'NONE',  ( 11.44039960990914651, 28.64646525600389282, -2.839279412974133887 ) ) ;
#58247 = PLANE ( 'NONE',  #76935 ) ;
#58248 = CARTESIAN_POINT ( 'NONE',  ( 174.8768402572162302, 255.1920038171627709, 8.200017817996553049 ) ) ;
#58249 = CARTESIAN_POINT ( 'NONE',  ( 170.2148221929604119, 256.7370173464272511, -14.26952246837105598 ) ) ;
#58250 = ORIENTED_EDGE ( 'NONE', *, *, #81125, .T. ) ;
#58251 = CARTESIAN_POINT ( 'NONE',  ( 77.50334873148125325, 59.55703387409915450, 16.42230352199692689 ) ) ;
#58252 = CARTESIAN_POINT ( 'NONE',  ( 150.6655900823359389, 269.6865383554857090, 15.31288044136207205 ) ) ;
#58253 = CARTESIAN_POINT ( 'NONE',  ( 105.0000000000000000, 10.00000000000003197, 54.99999999999999289 ) ) ;
#58254 = EDGE_CURVE ( 'NONE', #28329, #22379, #426, .T. ) ;
#58255 = AXIS2_PLACEMENT_3D ( 'NONE', #56695, #24304, #80040 ) ;
#58256 = ORIENTED_EDGE ( 'NONE', *, *, #35572, .T. ) ;
#58258 = LINE ( 'NONE', #25368, #50773 ) ;
#58257 = CARTESIAN_POINT ( 'NONE',  ( 207.7296438747196134, 270.8486979012336633, -6.692930657757584001 ) ) ;
#58259 = CARTESIAN_POINT ( 'NONE',  ( 148.9831146496684084, 272.6006712873522133, -12.63706091291043343 ) ) ;
#58260 = VERTEX_POINT ( 'NONE', #86882 ) ;
#58261 = CARTESIAN_POINT ( 'NONE',  ( 66.07636532461724244, 68.52392620069937834, -2.382434824416819641 ) ) ;
#58262 = CARTESIAN_POINT ( 'NONE',  ( 171.5146026185341839, 284.8826077422594949, -12.15938192449176114 ) ) ;
#58263 = LINE ( 'NONE', #13672, #24050 ) ;
#58264 = CARTESIAN_POINT ( 'NONE',  ( 78.39570488777410162, 61.38734676664308409, -15.85619035535652799 ) ) ;
#58265 = ADVANCED_FACE ( 'NONE', ( #61512 ), #7825, .T. ) ;
#58266 = CARTESIAN_POINT ( 'NONE',  ( 197.9919592856120687, 286.7924423995140728, 16.94645048433601531 ) ) ;
#58267 = B_SPLINE_CURVE_WITH_KNOTS ( 'NONE', 3,
 ( #58011, #88992, #84342, #30101 ),
 .UNSPECIFIED., .F., .F.,
 ( 4, 4 ),
 ( 0.007886306542003318140, 0.01295349318365762899 ),
 .UNSPECIFIED. ) ;
#58268 = CARTESIAN_POINT ( 'NONE',  ( 104.4229444624559591, 243.3464784336661637, 1.353441290958777525E-15 ) ) ;
#58269 = CARTESIAN_POINT ( 'NONE',  ( 122.9742295596836925, 230.2592609112380160, 2.679491924311254714 ) ) ;
#58270 = DIRECTION ( 'NONE',  ( -0.8660254037844387076, -0.4999999999999998890, -0.000000000000000000 ) ) ;
#58271 = LINE ( 'NONE', #95837, #10758 ) ;
#58272 = ORIENTED_EDGE ( 'NONE', *, *, #65624, .T. ) ;
#58273 = CARTESIAN_POINT ( 'NONE',  ( 163.7423057141168385, 247.0370024851108610, -6.909410042141566066 ) ) ;
#58274 = ORIENTED_EDGE ( 'NONE', *, *, #8360, .F. ) ;
#58275 = CARTESIAN_POINT ( 'NONE',  ( 32.50825522076439000, 36.95586893147758190, 7.433330006724141015 ) ) ;
#58276 = FACE_BOUND ( 'NONE', #75587, .T. ) ;
#58277 = CARTESIAN_POINT ( 'NONE',  ( 194.9396225458042409, 291.6968222089742540, -15.91036236140263505 ) ) ;
#58278 = CARTESIAN_POINT ( 'NONE',  ( 80.33713356334875755, 211.0643266524159856, -9.188101187500093303 ) ) ;
#58279 = CARTESIAN_POINT ( 'NONE',  ( -5.676897265278508797, 155.9824982072973683, -6.972266317189433020E-16 ) ) ;
#58280 = CARTESIAN_POINT ( 'NONE',  ( 191.4484954869714954, 299.0484741143815199, 8.684991747358081327 ) ) ;
#58281 = CARTESIAN_POINT ( 'NONE',  ( -42.72532191160158987, 28.29708160126036987, -10.00000000000000000 ) ) ;
#58282 = CARTESIAN_POINT ( 'NONE',  ( 175.5122396641868079, 278.4443030880159426, 15.47154450738855225 ) ) ;
#58283 = VERTEX_POINT ( 'NONE', #16413 ) ;
#58284 = CARTESIAN_POINT ( 'NONE',  ( 71.24387660651150611, 63.97505982078597953, -13.10960455195070473 ) ) ;
#58285 = CARTESIAN_POINT ( 'NONE',  ( 88.28592015977814356, 44.16006502160688996, -0.2344584660017056954 ) ) ;
#58286 = CARTESIAN_POINT ( 'NONE',  ( 66.16089386745949241, 68.65346719215108351, -4.358124916883920008 ) ) ;
#58287 = ORIENTED_EDGE ( 'NONE', *, *, #75084, .F. ) ;
#58288 = CARTESIAN_POINT ( 'NONE',  ( 194.7230684019799867, 293.3767474524976251, 15.79132110000472444 ) ) ;
#58289 = CARTESIAN_POINT ( 'NONE',  ( 72.36856322112618045, 69.84542717626317199, -8.279172892043805021 ) ) ;
#58290 = CARTESIAN_POINT ( 'NONE',  ( 161.6923300915171922, 250.5876644177310482, -14.43081872899884566 ) ) ;
#58291 = LINE ( 'NONE', #43072, #43216 ) ;
#58292 = CARTESIAN_POINT ( 'NONE',  ( 79.84223750413882215, 51.63136904638950853, 15.66302827892303995 ) ) ;
#58293 = CARTESIAN_POINT ( 'NONE',  ( 176.9285354572846245, 269.9431028654713032, 17.13598235524080238 ) ) ;
#58294 = DIRECTION ( 'NONE',  ( 0.9669094993746140121, -0.2551196190400366048, 0.000000000000000000 ) ) ;
#58295 = FILL_AREA_STYLE_COLOUR ( '', #86561 ) ;
#58296 = CARTESIAN_POINT ( 'NONE',  ( 203.2757866645317222, 269.5093088776978334, -7.514607224931010521 ) ) ;
#58297 = CARTESIAN_POINT ( 'NONE',  ( 119.4704829489755724, 239.7833772461660544, -9.188101187500095079 ) ) ;
#58298 = ORIENTED_EDGE ( 'NONE', *, *, #63555, .F. ) ;
#58299 = CARTESIAN_POINT ( 'NONE',  ( 85.35694830404344202, 44.17699873431174495, -6.675819990932985171 ) ) ;
#58300 = CARTESIAN_POINT ( 'NONE',  ( 81.86698606425520097, 229.6199935810941213, 2.679491924311251605 ) ) ;
#58301 = EDGE_CURVE ( 'NONE', #87041, #79979, #52999, .T. ) ;
#58302 = CARTESIAN_POINT ( 'NONE',  ( 155.2193237801463113, 261.7992402267395846, -18.58295809893692407 ) ) ;
#58303 = CARTESIAN_POINT ( 'NONE',  ( 204.9780665305064531, 275.6145696623662502, 14.10615427165218883 ) ) ;
#58304 = CARTESIAN_POINT ( 'NONE',  ( -9.431985743790550103, 175.3615022471903160, 5.000000000000046185 ) ) ;
#58305 = CARTESIAN_POINT ( 'NONE',  ( 181.0465414429574480, 255.4906575730030340, -4.757053701627741660 ) ) ;
#58306 = ORIENTED_EDGE ( 'NONE', *, *, #30455, .T. ) ;
#58307 = CARTESIAN_POINT ( 'NONE',  ( 76.93992332084131647, 56.94179084800790491, 16.18160332842839466 ) ) ;
#58308 = CARTESIAN_POINT ( 'NONE',  ( 167.5331536921724194, 249.1563084341292154, -5.485378542569181448 ) ) ;
#58309 = FACE_OUTER_BOUND ( 'NONE', #93042, .T. ) ;
#58310 = CARTESIAN_POINT ( 'NONE',  ( 206.6672608846700427, 272.6887992170966299, -10.88770374553082121 ) ) ;
#58311 = ADVANCED_FACE ( 'NONE', ( #96588 ), #36586, .T. ) ;
#58312 = CARTESIAN_POINT ( 'NONE',  ( -21.31413092498266693, 24.33771760303832465, 10.00000000000000000 ) ) ;
#58313 = EDGE_CURVE ( 'NONE', #4228, #43534, #24651, .T. ) ;
#58314 = CARTESIAN_POINT ( 'NONE',  ( 147.3154503175461514, 275.4891506405583073, 3.671329888160011823 ) ) ;
#58315 = DIRECTION ( 'NONE',  ( 1.000000000000000000, 0.000000000000000000, 0.000000000000000000 ) ) ;
#58316 = EDGE_CURVE ( 'NONE', #53063, #57662, #5282, .T. ) ;
#58317 = CARTESIAN_POINT ( 'NONE',  ( 170.7054206766590880, 250.3903097054384546, 3.971403188103841408 ) ) ;
#58318 = CARTESIAN_POINT ( 'NONE',  ( 21.79139015901366960, 20.78052372038640883, -10.00000000000000355 ) ) ;
#58319 = CARTESIAN_POINT ( 'NONE',  ( 190.0340467409721441, 301.4983712071542641, 4.077645795029533282 ) ) ;
#58320 = CARTESIAN_POINT ( 'NONE',  ( 38.52196584993465223, 56.41980893122115504, -10.00000000000000000 ) ) ;
#58321 = CARTESIAN_POINT ( 'NONE',  ( 169.4000131232833155, 285.1406234409721492, -8.020725679492032967 ) ) ;
#58322 = CARTESIAN_POINT ( 'NONE',  ( 198.2114954873088948, 287.3346145022089786, 18.52864136173620935 ) ) ;
#58323 = AXIS2_PLACEMENT_3D ( 'NONE', #17448, #66049, #34159 ) ;
#58324 = CARTESIAN_POINT ( 'NONE',  ( 157.3983369238794410, 271.2561898657742745, -14.62425919491228044 ) ) ;
#58325 = CARTESIAN_POINT ( 'NONE',  ( 136.7639277290220718, 259.7677522451419350, -5.000000000000047962 ) ) ;
#58326 = CARTESIAN_POINT ( 'NONE',  ( 173.0666269367678751, 283.8557712307529073, -12.24563893785450297 ) ) ;
#58327 = ORIENTED_EDGE ( 'NONE', *, *, #23207, .T. ) ;
#58328 = CARTESIAN_POINT ( 'NONE',  ( 157.8360072705708603, 257.2670114739976839, 17.12122855844125269 ) ) ;
#58329 = CARTESIAN_POINT ( 'NONE',  ( 147.8465295590381743, 274.5692944114487091, 9.322947948439978205 ) ) ;
#58330 = CARTESIAN_POINT ( 'NONE',  ( -1.664820405372784862, 169.8458772461660544, 9.188101187500095079 ) ) ;
#58331 = CARTESIAN_POINT ( 'NONE',  ( 45.42531092540608029, 197.0333772461660828, 9.188101187500095079 ) ) ;
#58332 = CARTESIAN_POINT ( 'NONE',  ( 178.2615612386009047, 258.9310810631866389, -10.32181247301958571 ) ) ;
#58333 = CARTESIAN_POINT ( 'NONE',  ( 18.81282613181931040, 26.56454794089041727, 10.00000000000000355 ) ) ;
#58334 = CARTESIAN_POINT ( 'NONE',  ( 88.12195951149128348, 43.65269896049575493, 0.1370767085644954975 ) ) ;
#58335 = DIRECTION ( 'NONE',  ( 0.4999999999999992784, -0.8660254037844390407, 0.000000000000000000 ) ) ;
#58336 = CARTESIAN_POINT ( 'NONE',  ( 72.03933155393818311, 72.41131128147422658, -2.965003495713515402 ) ) ;
#58337 = DIRECTION ( 'NONE',  ( 1.000000000000000000, 0.000000000000000000, -0.000000000000000000 ) ) ;
#58338 = CARTESIAN_POINT ( 'NONE',  ( 74.15479259495415931, 55.62765001672816823, -16.59030973361144845 ) ) ;
#58340 = CARTESIAN_POINT ( 'NONE',  ( 61.85273030166814578, 216.5177522451419065, 5.000000000000046185 ) ) ;
#58339 = CARTESIAN_POINT ( 'NONE',  ( 171.3032759856405107, 258.3952365426850974, 14.09859993956650648 ) ) ;
#58341 = CARTESIAN_POINT ( 'NONE',  ( 75.17267702473046143, 67.05865199424735579, 12.71180004614658365 ) ) ;
#58342 = FACE_OUTER_BOUND ( 'NONE', #97442, .T. ) ;
#58343 = CARTESIAN_POINT ( 'NONE',  ( 162.2150750494025431, 251.9152425808378553, -13.05861332114117168 ) ) ;
#58344 = CARTESIAN_POINT ( 'NONE',  ( 40.00363105557123333, 187.2365022471902023, 10.00000000000009592 ) ) ;
#58345 = CARTESIAN_POINT ( 'NONE',  ( -13.11024591527734628, 0.000000000000000000, -45.00000000000000000 ) ) ;
#58346 = CARTESIAN_POINT ( 'NONE',  ( 163.4216610345155800, 247.5923753613567442, 10.58669027323842826 ) ) ;
#58347 = CARTESIAN_POINT ( 'NONE',  ( -3.478321416370212305, 177.9869531367911293, 4.594050593750046652 ) ) ;
#58348 = CARTESIAN_POINT ( 'NONE',  ( 165.7591614932538278, 285.0852518727915594, 4.131734285391062578 ) ) ;
#58349 = CARTESIAN_POINT ( 'NONE',  ( 79.43361010913639575, 59.55165593117043699, 16.18183685357123736 ) ) ;
#58350 = CARTESIAN_POINT ( 'NONE',  ( 38.86330120330953974, 24.29860640527295246, -2.839279412974138328 ) ) ;
#58351 = CARTESIAN_POINT ( 'NONE',  ( 17.74301629803562363, 32.01751292744056343, 6.180339887498949913 ) ) ;
#58352 = CARTESIAN_POINT ( 'NONE',  ( 207.6628070930962906, 270.9644626028195376, 7.378217122120054761 ) ) ;
#58353 = CARTESIAN_POINT ( 'NONE',  ( 154.8989000222956349, 262.3542304552891551, 17.41779271305265908 ) ) ;
#58354 = CARTESIAN_POINT ( 'NONE',  ( 196.3507576896697344, 290.5575069072837664, -17.68249398312240928 ) ) ;
#58355 = DIRECTION ( 'NONE',  ( 0.000000000000000000, 0.000000000000000000, 1.000000000000000000 ) ) ;
#58356 = DIRECTION ( 'NONE',  ( 0.000000000000000000, 0.000000000000000000, 1.000000000000000000 ) ) ;
#58357 = CARTESIAN_POINT ( 'NONE',  ( 14.28983037092611319, 10.11110640527290627, -2.839279412974138328 ) ) ;
#58358 = CARTESIAN_POINT ( 'NONE',  ( 165.4299515451023410, 285.6795224695716229, -0.1515405553588986542 ) ) ;
#58359 = CARTESIAN_POINT ( 'NONE',  ( 21.77916244986271366, 18.28920272979926764, -7.433330006724141015 ) ) ;
#58360 = CARTESIAN_POINT ( 'NONE',  ( -19.65312891409030271, 93.06504152958497400, -10.00000000000000888 ) ) ;
#58361 = ADVANCED_FACE ( 'NONE', ( #49435 ), #15822, .T. ) ;
#58362 = CARTESIAN_POINT ( 'NONE',  ( 193.7118145980225279, 295.1282904202991517, 14.61271143546694162 ) ) ;
#58363 = EDGE_LOOP ( 'NONE', ( #90690, #82280, #92200, #53060 ) ) ;
#58364 = DIRECTION ( 'NONE',  ( -0.5000000000000003331, 0.8660254037844383745, 0.000000000000000000 ) ) ;
#58365 = CARTESIAN_POINT ( 'NONE',  ( 75.13576154535616070, 53.51470238525797640, -16.05299128471374814 ) ) ;
#58366 = DIRECTION ( 'NONE',  ( 0.6602847420308605164, 0.7510153523339188064, 0.000000000000000000 ) ) ;
#58367 = EDGE_CURVE ( 'NONE', #49412, #12543, #41320, .T. ) ;
#58368 = ORIENTED_EDGE ( 'NONE', *, *, #6025, .T. ) ;
#58369 = CARTESIAN_POINT ( 'NONE',  ( 152.3564455502385044, 267.3888446593566641, 15.42595238024932414 ) ) ;
#58370 = CARTESIAN_POINT ( 'NONE',  ( 82.34753025084647504, 40.38730442864357428, 1.410118989783748278 ) ) ;
#58371 = CARTESIAN_POINT ( 'NONE',  ( 66.15678826669763168, 68.52882108677162876, 4.729996398140529301 ) ) ;
#58372 = CARTESIAN_POINT ( 'NONE',  ( 87.37622458635497935, 44.94434973981048387, 6.879737256407628010 ) ) ;
#58373 = EDGE_LOOP ( 'NONE', ( #37741, #69256, #64107, #77981 ) ) ;
#58374 = ORIENTED_EDGE ( 'NONE', *, *, #49148, .T. ) ;
#58376 = CARTESIAN_POINT ( 'NONE',  ( 204.2129321040862919, 276.9398213635460024, 14.41515352680879758 ) ) ;
#58375 = CARTESIAN_POINT ( 'NONE',  ( -19.65312891409030271, 93.06504152958497400, 177.5919119679930134 ) ) ;
#58377 = CARTESIAN_POINT ( 'NONE',  ( 192.0963028965829551, 297.9264387674147656, 11.34530024772836754 ) ) ;
#58378 = ORIENTED_EDGE ( 'NONE', *, *, #73954, .T. ) ;
#58379 = CARTESIAN_POINT ( 'NONE',  ( 80.47734257382147405, 57.78184453145892263, -16.59809864164601478 ) ) ;
#58380 = CARTESIAN_POINT ( 'NONE',  ( 168.4954155832338074, 247.6751246288074526, 2.275130870958896434 ) ) ;
#58382 = EDGE_CURVE ( 'NONE', #22391, #47320, #82665, .T. ) ;
#58381 = ORIENTED_EDGE ( 'NONE', *, *, #45726, .F. ) ;
#58383 = FACE_OUTER_BOUND ( 'NONE', #7226, .T. ) ;
#58384 = CARTESIAN_POINT ( 'NONE',  ( 78.23504418992378362, 222.6427522451419065, -10.00000000000009592 ) ) ;
#58385 = CARTESIAN_POINT ( 'NONE',  ( 81.05763270389508079, 43.67158023151815627, 9.470390458390101074 ) ) ;
#58386 = EDGE_LOOP ( 'NONE', ( #98400, #86231, #88632, #100051 ) ) ;
#58387 = CARTESIAN_POINT ( 'NONE',  ( 177.6900565734887323, 268.6111475138295646, 16.75654593232756540 ) ) ;
#58388 = CARTESIAN_POINT ( 'NONE',  ( 166.4818116705677653, 274.3668896485694404, -15.18083394624400562 ) ) ;
#58389 = CARTESIAN_POINT ( 'NONE',  ( 150.8884397357406328, 275.9708103743298580, -8.379586308329308508 ) ) ;
#58390 = ORIENTED_EDGE ( 'NONE', *, *, #55901, .F. ) ;
#58391 = CARTESIAN_POINT ( 'NONE',  ( 190.0445576990143195, 301.4801656937889902, 4.140328216824785912 ) ) ;
#58392 = CARTESIAN_POINT ( 'NONE',  ( 200.7812400522830956, 279.0213764812114050, 16.52495314239560287 ) ) ;
#58393 = ORIENTED_EDGE ( 'NONE', *, *, #76233, .F. ) ;
#58394 = ADVANCED_FACE ( 'NONE', ( #69486 ), #23375, .F. ) ;
#58395 = DIRECTION ( 'NONE',  ( -0.4999999999999987788, 0.8660254037844392627, 0.000000000000000000 ) ) ;
#58396 = ORIENTED_EDGE ( 'NONE', *, *, #82939, .T. ) ;
#58397 = CARTESIAN_POINT ( 'NONE',  ( 24.46206622376873696, 38.38158625946101665, -10.00000000000000000 ) ) ;
#58398 = AXIS2_PLACEMENT_3D ( 'NONE', #20519, #81356, #59981 ) ;
#58399 = ORIENTED_EDGE ( 'NONE', *, *, #59171, .T. ) ;
#58400 = CARTESIAN_POINT ( 'NONE',  ( 159.1259971461353473, 259.5205376126884858, 16.70218726448308999 ) ) ;
#58401 = CYLINDRICAL_SURFACE ( 'NONE', #69391, 17.82106496071139645 ) ;
#58402 = CARTESIAN_POINT ( 'NONE',  ( 193.9583149726292959, 294.7013392473955946, 13.54389207180881805 ) ) ;
#58403 = CARTESIAN_POINT ( 'NONE',  ( 188.5999732098899528, 298.6034004545671223, -4.739567632090335714 ) ) ;
#58404 = CARTESIAN_POINT ( 'NONE',  ( 132.5758265486178971, 258.8967562850347122, -4.648177544792955347E-16 ) ) ;
#58405 = CARTESIAN_POINT ( 'NONE',  ( 4.268087542569434234, 45.74354613382861601, 59.99999999999999289 ) ) ;
#58406 = CARTESIAN_POINT ( 'NONE',  ( 178.0302064638906074, 292.4640037680099454, 7.106335582765731296 ) ) ;
#58407 = CARTESIAN_POINT ( 'NONE',  ( 158.3871229378075611, 256.3124511374962253, -17.26248367166835607 ) ) ;
#58408 = ORIENTED_EDGE ( 'NONE', *, *, #13718, .F. ) ;
#58409 = CARTESIAN_POINT ( 'NONE',  ( 73.22055517253131995, 58.28100772285806386, -15.76052744220302770 ) ) ;
#58410 = DIRECTION ( 'NONE',  ( 0.2165469281463284490, -0.9762722099447412871, 0.000000000000000000 ) ) ;
#58411 = DIRECTION ( 'NONE',  ( 0.1266907948509091442, -0.9919422576440851680, 0.000000000000000000 ) ) ;
#58413 = ORIENTED_EDGE ( 'NONE', *, *, #17631, .T. ) ;
#58412 = CARTESIAN_POINT ( 'NONE',  ( 85.23385146218150510, 41.99429442906141929, -0.6099763831586285656 ) ) ;
#58414 = ORIENTED_EDGE ( 'NONE', *, *, #65985, .F. ) ;
#58415 = CARTESIAN_POINT ( 'NONE',  ( 190.4191603088290776, 300.8313349409419288, 6.519931150822659838 ) ) ;
#58416 = EDGE_CURVE ( 'NONE', #73348, #91080, #83736, .T. ) ;
#58417 = CARTESIAN_POINT ( 'NONE',  ( 83.08655343033629492, 51.67706410362837488, -14.60604715524620367 ) ) ;
#58418 = CARTESIAN_POINT ( 'NONE',  ( -22.42236680055709641, 157.8615022471902591, 0.000000000000000000 ) ) ;
#58419 = CARTESIAN_POINT ( 'NONE',  ( 177.9714937548455680, 255.7189482022137383, 8.882064279750110813 ) ) ;
#58420 = CARTESIAN_POINT ( 'NONE',  ( 160.0245045302084179, 253.4764230280800916, -16.06816193402951853 ) ) ;
#58421 = CARTESIAN_POINT ( 'NONE',  ( 190.1563334688368911, 301.2865643814013765, -1.454600626587476686 ) ) ;
#58422 = ORIENTED_EDGE ( 'NONE', *, *, #63334, .T. ) ;
#58424 = EDGE_CURVE ( 'NONE', #48945, #91686, #83780, .T. ) ;
#58423 = DIRECTION ( 'NONE',  ( -0.8660254037844375974, -0.5000000000000016653, 0.000000000000000000 ) ) ;
#58425 = CARTESIAN_POINT ( 'NONE',  ( -19.78671505388745899, 93.01741294681296779, 59.99999999999999289 ) ) ;
#58426 = CARTESIAN_POINT ( 'NONE',  ( 164.3774690880109119, 245.9368672504194819, -2.805681983503304000 ) ) ;
#58427 = CARTESIAN_POINT ( 'NONE',  ( 29.80979036164399432, 178.0177522451417929, 5.000000000000051514 ) ) ;
#58428 = CARTESIAN_POINT ( 'NONE',  ( 101.9874215621947116, 235.8149278399160949, 9.188101187500093303 ) ) ;
#58429 = CARTESIAN_POINT ( 'NONE',  ( 82.74024154138081144, 40.61182045439817756, -1.385978721574811834 ) ) ;
#58430 = EDGE_CURVE ( 'NONE', #91738, #25484, #7733, .T. ) ;
#58431 = CARTESIAN_POINT ( 'NONE',  ( 164.0889469084813186, 280.5819020075147705, -11.59149887344287677 ) ) ;
#58432 = CARTESIAN_POINT ( 'NONE',  ( 195.6974783896144174, 291.6890198465123945, 16.70600479393688431 ) ) ;
#58433 = CARTESIAN_POINT ( 'NONE',  ( 165.0952264510788154, 281.4963861521250124, -11.84807672454148886 ) ) ;
#58434 = CARTESIAN_POINT ( 'NONE',  ( 21.44705901024191874, 189.3149278399161233, 9.188101187500093303 ) ) ;
#58435 = CARTESIAN_POINT ( 'NONE',  ( 153.1198285439165545, 279.2890930352092482, 3.903594709581249322 ) ) ;
#58436 = ORIENTED_EDGE ( 'NONE', *, *, #86739, .T. ) ;
#58437 = VERTEX_POINT ( 'NONE', #39064 ) ;
#58439 = EDGE_CURVE ( 'NONE', #53634, #3488, #12472, .T. ) ;
#58438 = CARTESIAN_POINT ( 'NONE',  ( 71.94643353573427191, 71.53214566342799685, 5.625104812542565114 ) ) ;
#58440 = DIRECTION ( 'NONE',  ( 0.8660254037844375974, 0.5000000000000017764, 3.252519625699413953E-16 ) ) ;
#58441 = ADVANCED_FACE ( 'NONE', ( #31475 ), #20678, .T. ) ;
#58442 = LINE ( 'NONE', #82798, #56223 ) ;
#58443 = CARTESIAN_POINT ( 'NONE',  ( -61.39381520214497101, 38.43978098112751951, 10.00000000000000000 ) ) ;
#58444 = DIRECTION ( 'NONE',  ( -0.4330127018922203530, 0.7500000000000046629, 0.4999999999999919509 ) ) ;
#58445 =( BOUNDED_CURVE ( )  B_SPLINE_CURVE ( 2, ( #14200, #28393, #52678, #36990, #91726, #74530, #44576, #6095, #90248 ),
 .UNSPECIFIED., .F., .T. ) 
 B_SPLINE_CURVE_WITH_KNOTS ( ( 3, 2, 2, 2, 3 ),
 ( 0.3427419354838709964, 0.3440860215053763715, 0.3467741935483871218, 0.3494623655913978721, 0.3508064516129032473 ),
 .UNSPECIFIED. ) 
 CURVE ( )  GEOMETRIC_REPRESENTATION_ITEM ( )  RATIONAL_B_SPLINE_CURVE ( ( 0.9330127018922194093, 0.9330127018922207416, 1.000000000000000000, 0.8660254037844387076, 1.000000000000000000, 0.8660254037844387076, 1.000000000000000000, 0.9330127018922194093, 0.9330127018922194093 ) ) 
 REPRESENTATION_ITEM ( '' )  );
#58446 = CYLINDRICAL_SURFACE ( 'NONE', #31955, 49.99999999999999289 ) ;
#58447 = CYLINDRICAL_SURFACE ( 'NONE', #67724, 17.82106496071139645 ) ;
#58448 = CARTESIAN_POINT ( 'NONE',  ( 43.17879721251643588, 204.9244531367911293, -4.594050593750046652 ) ) ;
#58449 = CARTESIAN_POINT ( 'NONE',  ( 83.57553417992782840, 232.3927522451419350, 2.944929066748280225E-16 ) ) ;
#58450 = VERTEX_POINT ( 'NONE', #39561 ) ;
#58451 = CARTESIAN_POINT ( 'NONE',  ( 194.7794102799644520, 266.3152794235413126, -7.644990388705906526 ) ) ;
#58452 = CARTESIAN_POINT ( 'NONE',  ( 179.5827521140122087, 259.6898873773316723, -10.31498942205267078 ) ) ;
#58453 = CARTESIAN_POINT ( 'NONE',  ( 1.528821818964843482, 165.5643266524160140, 9.188101187500095079 ) ) ;
#58454 = CARTESIAN_POINT ( 'NONE',  ( 198.6363782946250183, 286.5986958926748116, -18.50260615857378355 ) ) ;
#58455 = CARTESIAN_POINT ( 'NONE',  ( 79.20094478699866158, 45.83966577849356838, -12.45917745233390406 ) ) ;
#58456 = CARTESIAN_POINT ( 'NONE',  ( 146.9978162861947908, 276.0393089210717790, -5.134868500856280882 ) ) ;
#58457 = CARTESIAN_POINT ( 'NONE',  ( 163.7423057141168385, 247.0370024851108610, -6.909410042141566066 ) ) ;
#58458 = CARTESIAN_POINT ( 'NONE',  ( 203.8087165842311776, 276.3139229654213409, 13.33924813713301738 ) ) ;
#58459 = CARTESIAN_POINT ( 'NONE',  ( 71.31959007138432582, 71.35434536779762027, 3.842738600495782197 ) ) ;
#58460 = CARTESIAN_POINT ( 'NONE',  ( 207.6628070930962906, 270.9644626028195376, 7.378217122120054761 ) ) ;
#58461 =( BOUNDED_CURVE ( )  B_SPLINE_CURVE ( 2, ( #69450, #76091, #60831, #14261, #7145, #84208, #69941, #54228, #39032, #7652, #53735, #22851, #83196 ),
 .UNSPECIFIED., .F., .T. ) 
 B_SPLINE_CURVE_WITH_KNOTS ( ( 3, 2, 2, 2, 2, 2, 3 ),
 ( 0.08750000000000000833, 0.08999999999999999667, 0.09500000000000000111, 0.1000000000000000056, 0.1049999999999999961, 0.1100000000000000006, 0.1125000000000000028 ),
 .UNSPECIFIED. ) 
 CURVE ( )  GEOMETRIC_REPRESENTATION_ITEM ( )  RATIONAL_B_SPLINE_CURVE ( ( 0.9755282581475768211, 0.9755282581475768211, 1.000000000000000000, 0.9510565162951535312, 1.000000000000000000, 0.9510565162951535312, 1.000000000000000000, 0.9510565162951535312, 1.000000000000000000, 0.9510565162951535312, 1.000000000000000000, 0.9755282581475768211, 0.9755282581475768211 ) ) 
 REPRESENTATION_ITEM ( '' )  );
#58462 = ORIENTED_EDGE ( 'NONE', *, *, #48245, .F. ) ;
#58463 = AXIS2_PLACEMENT_3D ( 'NONE', #98169, #37329, #22142 ) ;
#58464 = CARTESIAN_POINT ( 'NONE',  ( -2.070769811622737766, 159.6115022471902023, -5.000000000000041744 ) ) ;
#58465 = CARTESIAN_POINT ( 'NONE',  ( 84.53133730985203442, 45.87904168161020380, 10.50013902873333471 ) ) ;
#58466 = CARTESIAN_POINT ( 'NONE',  ( 123.7191597644692393, 251.4244531367911293, -4.594050593750046652 ) ) ;
#58467 = CARTESIAN_POINT ( 'NONE',  ( 22.87854050506884462, 34.18502408145592852, 5.678558825948277544 ) ) ;
#58468 = CARTESIAN_POINT ( 'NONE',  ( 164.4939982559556029, 245.7350328109756390, 0.9880945281613151554 ) ) ;
#58469 = CARTESIAN_POINT ( 'NONE',  ( 178.3571982967953602, 292.6181790745828835, -7.174879954037646002 ) ) ;
#58471 = CARTESIAN_POINT ( 'NONE',  ( 75.15246256102729205, 67.05878861674010238, 13.14576163508979434 ) ) ;
#58470 = CARTESIAN_POINT ( 'NONE',  ( 157.7365441389748923, 257.4392866714015895, 18.13124212464487073 ) ) ;
#58472 = CARTESIAN_POINT ( 'NONE',  ( 11.62691283633230377, 30.21091486745859811, -1.111400068045478839E-16 ) ) ;
#58473 = ORIENTED_EDGE ( 'NONE', *, *, #79542, .F. ) ;
#58474 = CARTESIAN_POINT ( 'NONE',  ( 151.3883635558152321, 268.4346579770563608, 15.44343517165679103 ) ) ;
#58475 = FACE_OUTER_BOUND ( 'NONE', #35370, .T. ) ;
#58476 = CARTESIAN_POINT ( 'NONE',  ( 190.6456776865061613, 300.0543483028657192, 3.690611039747805577 ) ) ;
#58477 = CARTESIAN_POINT ( 'NONE',  ( 172.9246534260911972, 268.4856987155242791, -16.42706699595391484 ) ) ;
#58478 = LINE ( 'NONE', #12411, #10303 ) ;
#58479 = ORIENTED_EDGE ( 'NONE', *, *, #20877, .F. ) ;
#58480 = CARTESIAN_POINT ( 'NONE',  ( 70.00968539685798930, 68.79935913217504151, 7.688938106457000821 ) ) ;
#58481 = FACE_OUTER_BOUND ( 'NONE', #96438, .T. ) ;
#58482 = CARTESIAN_POINT ( 'NONE',  ( 71.66539077729500207, 72.47145342129385881, 0.9585255015204302564 ) ) ;
#58483 = CARTESIAN_POINT ( 'NONE',  ( 77.55198886215855225, 49.72190584956302217, 14.94683709150641349 ) ) ;
#58484 = CARTESIAN_POINT ( 'NONE',  ( 197.4664967616869831, 271.4698837146752908, 12.07595270249984232 ) ) ;
#58485 = B_SPLINE_CURVE_WITH_KNOTS ( 'NONE', 3,
 ( #6858, #8365, #69150, #83910, #39232, #70140, #15436, #752, #46334, #24054, #7867, #258, #16451, #70652, #61042, #100079, #30668, #93999, #31636, #39723, #77258, #92493, #23039, #38746, #69651, #31140, #62536, #93496, #54949, #47349, #14473, #79314, #57444, #86925, #80302, #56453, #96498, #48366, #9882, #2278, #10370, #49854, #34651, #94493, #71684, #42242 ),
 .UNSPECIFIED., .F., .F.,
 ( 4, 1, 2, 2, 1, 2, 2, 1, 1, 2, 2, 1, 1, 2, 2, 1, 1, 2, 2, 1, 1, 1, 2, 2, 1, 1, 1, 2, 2, 4 ),
 ( 0.000000000000000000, 0.06250000000000428824, 0.09375000000000484335, 0.1250000000000054123, 0.1875000000000069111, 0.2187500000000092426, 0.2500000000000115463, 0.3125000000000164868, 0.3437500000000191513, 0.3593750000000205946, 0.3750000000000220379, 0.4375000000000278666, 0.4687500000000291989, 0.4843750000000298095, 0.5000000000000303091, 0.5625000000000234257, 0.5937500000000196509, 0.6093750000000160982, 0.6250000000000124345, 0.6875000000000081046, 0.7187500000000074385, 0.7343750000000071054, 0.7421875000000066613, 0.7500000000000061062, 0.8124999999999911182, 0.8437499999999836797, 0.8593749999999802380, 0.8671874999999783507, 0.8749999999999764633, 1.000000000000000000 ),
 .UNSPECIFIED. ) ;
#58486 = CARTESIAN_POINT ( 'NONE',  ( 185.8122340750109913, 296.6774856835382934, 4.673344314135899680 ) ) ;
#58487 = DIRECTION ( 'NONE',  ( -0.1039558454088829048, 0.1800568059919617214, 0.9781476007338041345 ) ) ;
#58488 = CARTESIAN_POINT ( 'NONE',  ( 148.4946753614456725, 273.9075993938183160, -8.034288511620331974 ) ) ;
#58489 = ORIENTED_EDGE ( 'NONE', *, *, #31168, .F. ) ;
#58490 = CARTESIAN_POINT ( 'NONE',  ( 194.4892283647733109, 282.9810723741138645, 17.41623236043902523 ) ) ;
#58491 = CARTESIAN_POINT ( 'NONE',  ( 12.43831579814173693, 15.38052372038639248, 10.00000000000000533 ) ) ;
#58492 = CARTESIAN_POINT ( 'NONE',  ( 81.75404519488073163, 42.76199632323480415, 8.646050847852000842 ) ) ;
#58493 = ORIENTED_EDGE ( 'NONE', *, *, #30280, .T. ) ;
#58494 = CYLINDRICAL_SURFACE ( 'NONE', #70851, 17.82106496071139645 ) ;
#58495 = CARTESIAN_POINT ( 'NONE',  ( 194.3011251241114508, 294.1075746476782342, -14.76047579547631905 ) ) ;
#58496 = CARTESIAN_POINT ( 'NONE',  ( 159.6022460529178488, 264.0598611018144766, -17.33694791066348273 ) ) ;
#58498 = EDGE_CURVE ( 'NONE', #56834, #91866, #64358, .T. ) ;
#58497 = ORIENTED_EDGE ( 'NONE', *, *, #26525, .T. ) ;
#58499 = CARTESIAN_POINT ( 'NONE',  ( 78.91446233654380649, 59.71533271261715470, 16.49719907270642238 ) ) ;
#58500 = DIRECTION ( 'NONE',  ( -0.8660254037844377084, -0.5000000000000014433, -0.000000000000000000 ) ) ;
#58501 = DIRECTION ( 'NONE',  ( -1.000000000000000000, 0.000000000000000000, 5.984665299743594308E-16 ) ) ;
#58502 = DIRECTION ( 'NONE',  ( -0.001635407438361268905, -0.9999986627203610867, 0.000000000000000000 ) ) ;
#58503 = VERTEX_POINT ( 'NONE', #88752 ) ;
#58504 = CARTESIAN_POINT ( 'NONE',  ( 89.32180003184730310, 228.5024278399160949, 9.188101187500095079 ) ) ;
#58505 = CARTESIAN_POINT ( 'NONE',  ( 202.9667708310126386, 279.0982360029344136, 16.24681954556558949 ) ) ;
#58506 = CARTESIAN_POINT ( 'NONE',  ( 84.48836950856804151, 49.89909654526366722, -13.70430404532020319 ) ) ;
#58507 = CARTESIAN_POINT ( 'NONE',  ( 182.0653602573277396, 257.7337868896066198, -5.961595716692482227 ) ) ;
#58508 = ORIENTED_EDGE ( 'NONE', *, *, #62275, .T. ) ;
#58509 = ADVANCED_FACE ( 'NONE', ( #19324 ), #66386, .T. ) ;
#58510 = VERTEX_POINT ( 'NONE', #58764 ) ;
#58511 = PLANE ( 'NONE',  #67513 ) ;
#58512 = EDGE_CURVE ( 'NONE', #97187, #48903, #27882, .T. ) ;
#58513 = ORIENTED_EDGE ( 'NONE', *, *, #91160, .F. ) ;
#58514 = CARTESIAN_POINT ( 'NONE',  ( 192.6361035247282985, 294.0892689374524593, 14.43747539422717630 ) ) ;
#58515 = ORIENTED_EDGE ( 'NONE', *, *, #43248, .F. ) ;
#58516 = CARTESIAN_POINT ( 'NONE',  ( 148.8636819117637629, 274.0699646975406836, 8.926834414297511344 ) ) ;
#58517 = LINE ( 'NONE', #89489, #28350 ) ;
#58518 = VERTEX_POINT ( 'NONE', #58279 ) ;
#58519 = FACE_OUTER_BOUND ( 'NONE', #70515, .T. ) ;
#58520 = CARTESIAN_POINT ( 'NONE',  ( 82.19410048901978882, 40.72072028018710199, 3.734475190160377434 ) ) ;
#58521 = CARTESIAN_POINT ( 'NONE',  ( 189.9342510962733002, 301.6712223341471031, 2.454586110798282039 ) ) ;
#58522 = CARTESIAN_POINT ( 'NONE',  ( 172.6012549852709412, 290.2025030293380610, -5.021894074213228087 ) ) ;
#58523 = PLANE ( 'NONE',  #21035 ) ;
#58524 = DIRECTION ( 'NONE',  ( -0.1239754375649670948, -0.9922852870422774751, 0.000000000000000000 ) ) ;
#58525 = CARTESIAN_POINT ( 'NONE',  ( 148.6720373546558847, 247.4548013555409796, -4.594050593750042211 ) ) ;
#58526 = CARTESIAN_POINT ( 'NONE',  ( 167.6713749921846102, 266.7905464791912777, -17.76959288544986393 ) ) ;
#58527 = ORIENTED_EDGE ( 'NONE', *, *, #10513, .F. ) ;
#58528 = CARTESIAN_POINT ( 'NONE',  ( 76.00843876396085363, 56.26865137601856048, 16.15028453724080393 ) ) ;
#58529 = CARTESIAN_POINT ( 'NONE',  ( 5.233272902960924178, 23.99752408145590010, 5.678558825948277544 ) ) ;
#58530 = ORIENTED_EDGE ( 'NONE', *, *, #15190, .T. ) ;
#58531 = CARTESIAN_POINT ( 'NONE',  ( -13.86269525828471849, 104.2312461070085021, 36.50000000000000000 ) ) ;
#58533 = VERTEX_POINT ( 'NONE', #43578 ) ;
#58532 = CARTESIAN_POINT ( 'NONE',  ( 203.5888533553347202, 271.6823068233347271, 9.589978014565568643 ) ) ;
#58534 = CARTESIAN_POINT ( 'NONE',  ( -14.80832225825293946, 105.5937860941667736, 10.75146334683068972 ) ) ;
#58535 = FACE_OUTER_BOUND ( 'NONE', #75754, .T. ) ;
#58536 = CARTESIAN_POINT ( 'NONE',  ( 76.27092524855413558, 64.92237886744916864, -14.30682806216622360 ) ) ;
#58537 = CARTESIAN_POINT ( 'NONE',  ( 156.6830332884052552, 279.5358271113678938, 7.481028761613042199 ) ) ;
#58538 = CARTESIAN_POINT ( 'NONE',  ( 179.0685761320505947, 258.5468394390073286, -11.57600102548048149 ) ) ;
#58539 = CARTESIAN_POINT ( 'NONE',  ( 192.7113383204448667, 292.2246753303537616, -14.48311065252534391 ) ) ;
#58540 = CARTESIAN_POINT ( 'NONE',  ( 86.03189311092296521, 43.36316420155662144, 3.487833995403543774 ) ) ;
#58541 = CARTESIAN_POINT ( 'NONE',  ( 88.41107184461979784, 44.00353577411875960, -2.298891457252526749 ) ) ;
#58542 = ORIENTED_EDGE ( 'NONE', *, *, #67322, .F. ) ;
#58544 = ADVANCED_FACE ( 'NONE', ( #26898 ), #90232, .F. ) ;
#58543 = DIRECTION ( 'NONE',  ( 0.4999999999999999445, -0.8660254037844385966, 0.000000000000000000 ) ) ;
#58545 = CARTESIAN_POINT ( 'NONE',  ( 65.77405155218870902, 69.10179338945289373, 0.09299488885824654105 ) ) ;
#58546 = ORIENTED_EDGE ( 'NONE', *, *, #54687, .T. ) ;
#58547 = CARTESIAN_POINT ( 'NONE',  ( 161.8699203163502034, 276.4193623153122417, 12.82305117122160887 ) ) ;
#58548 = EDGE_CURVE ( 'NONE', #45907, #57548, #57776, .T. ) ;
#58549 = EDGE_CURVE ( 'NONE', #54504, #11091, #59621, .T. ) ;
#58550 = CARTESIAN_POINT ( 'NONE',  ( -19.65312891409030271, 93.06504152958497400, -10.00000000000000888 ) ) ;
#58551 = LINE ( 'NONE', #65164, #85498 ) ;
#58552 = CARTESIAN_POINT ( 'NONE',  ( 190.8138402884741254, 300.1477291634665789, 4.037153726988762514 ) ) ;
#58553 = CARTESIAN_POINT ( 'NONE',  ( -19.65312891409030271, 93.06504152958497400, -10.00000000000000888 ) ) ;
#58555 = CARTESIAN_POINT ( 'NONE',  ( 151.2546443255573934, 275.3395117651207897, -9.775857568146751220 ) ) ;
#58554 = LINE ( 'NONE', #89526, #8020 ) ;
#58556 = CARTESIAN_POINT ( 'NONE',  ( 200.6684024474820944, 268.3695016763517742, 6.063491142324016536 ) ) ;
#58557 = ORIENTED_EDGE ( 'NONE', *, *, #94579, .F. ) ;
#58558 = ADVANCED_FACE ( 'NONE', ( #21294 ), #80639, .F. ) ;
#58559 = EDGE_LOOP ( 'NONE', ( #57882, #80523, #96057, #35342 ) ) ;
#58560 = CARTESIAN_POINT ( 'NONE',  ( 72.27428605645289394, 62.29733430174115227, -14.32261433990752941 ) ) ;
#58561 = EDGE_CURVE ( 'NONE', #6222, #3083, #79055, .T. ) ;
#58562 = CARTESIAN_POINT ( 'NONE',  ( 80.19866971488238505, 58.11932589254354298, 16.26542142913219635 ) ) ;
#58563 = EDGE_CURVE ( 'NONE', #16138, #64801, #16434, .T. ) ;
#58564 = FACE_OUTER_BOUND ( 'NONE', #46803, .T. ) ;
#58565 = CARTESIAN_POINT ( 'NONE',  ( 153.1314981037513121, 265.4154603756023789, 17.73969815997475408 ) ) ;
#58566 = CARTESIAN_POINT ( 'NONE',  ( 80.72225415553992889, 43.55209726595803943, -9.557057607487440265 ) ) ;
#58567 = CARTESIAN_POINT ( 'NONE',  ( 2.394847222749282079, 166.0643266524160140, -9.188101187500093303 ) ) ;
#58568 = CARTESIAN_POINT ( 'NONE',  ( 110.8105760068962127, 222.5327760586659736, 1.948934522072303157E-15 ) ) ;
#58569 = CARTESIAN_POINT ( 'NONE',  ( 186.1630411436486554, 296.9614825196608194, -7.488375694256206749 ) ) ;
#58570 = CARTESIAN_POINT ( 'NONE',  ( -12.91644128716779072, 174.8967562850347406, 1.347971487989956912E-14 ) ) ;
#58571 = B_SPLINE_CURVE_WITH_KNOTS ( 'NONE', 3,
 ( #49006, #71818, #94135, #11019, #79940, #48507, #72829, #40872, #31777, #2415, #41383, #39866, #72323, #9514, #95656, #26205, #78926, #40377, #71315, #63698, #62680, #24200, #86067, #16593, #47489, #78414, #34296, #26698, #96140, #88557, #19123, #42376, #57583, #65195, #49997, #80954, #11520, #3422, #53204, #85663, #46584, #22806, #60776, #62280, #92735, #69403, #83653, #7600 ),
 .UNSPECIFIED., .F., .F.,
 ( 4, 2, 2, 2, 2, 2, 2, 2, 2, 2, 2, 2, 2, 2, 2, 2, 2, 2, 2, 2, 2, 2, 2, 4 ),
 ( 0.001558436884926003851, 0.002019628477514530829, 0.002480820070103058241, 0.002711415866397258196, 0.002826713764544444910, 0.002942011662691631189, 0.003057309560838817469, 0.003172607458986004183, 0.003403203255280448300, 0.003864394847869302707, 0.004325586440458157114, 0.005247969625635865928, 0.006170352810813574743, 0.006631544403402352822, 0.007092735995991130034, 0.007208033894138404785, 0.007265682843212073819, 0.007323331792285742853, 0.007438629690433081788, 0.007553927588580421591, 0.008015119181169766058, 0.008476310773759109657, 0.008706906570053764977, 0.008937502366348420296 ),
 .UNSPECIFIED. ) ;
#58572 = AXIS2_PLACEMENT_3D ( 'NONE', #35471, #94944, #43567 ) ;
#58573 = DIRECTION ( 'NONE',  ( -0.8660254037844387076, -0.4999999999999998890, -0.000000000000000000 ) ) ;
#58574 = CARTESIAN_POINT ( 'NONE',  ( -19.65312891409030271, 93.06504152958497400, -45.00000000000001421 ) ) ;
#58575 = CARTESIAN_POINT ( 'NONE',  ( 194.9220242159064185, 293.0321458743159724, -14.92681063007793263 ) ) ;
#58576 = CARTESIAN_POINT ( 'NONE',  ( 84.51504024060453446, 50.21520769139153373, 13.87897165174792846 ) ) ;
#58577 = CARTESIAN_POINT ( 'NONE',  ( -19.65312891409030271, 93.06504152958497400, -10.00000000000000888 ) ) ;
#58578 = CARTESIAN_POINT ( 'NONE',  ( 79.36263291408793918, 45.67866562566761957, -12.88899626193393821 ) ) ;
#58579 = CARTESIAN_POINT ( 'NONE',  ( 176.0835288146691369, 265.6135182482621531, -15.96225161722567698 ) ) ;
#58580 = EDGE_CURVE ( 'NONE', #29626, #99384, #30568, .T. ) ;
#58581 = CARTESIAN_POINT ( 'NONE',  ( 82.06918437091763963, 212.0643266524160140, 9.188101187500095079 ) ) ;
#58582 = FACE_OUTER_BOUND ( 'NONE', #12476, .T. ) ;
#58583 = FACE_OUTER_BOUND ( 'NONE', #97319, .T. ) ;
#58585 = CARTESIAN_POINT ( 'NONE',  ( 86.02614724684285363, 42.97974342575955120, -1.241900217485796931 ) ) ;
#58584 = CARTESIAN_POINT ( 'NONE',  ( 157.1338510812060747, 258.4831816688264325, 17.88958125218800888 ) ) ;
#58586 = CARTESIAN_POINT ( 'NONE',  ( 75.59035046094346910, 65.27760725598233194, 14.33377162271303185 ) ) ;
#58587 = CARTESIAN_POINT ( 'NONE',  ( 204.6350011963004647, 275.7068757420208271, -12.64342396695018245 ) ) ;
#58588 = CARTESIAN_POINT ( 'NONE',  ( 30.66313333631612892, 33.10171378149921395, 9.188101187500008038 ) ) ;
#58589 = CARTESIAN_POINT ( 'NONE',  ( 147.5118896528469179, 275.1489077312122049, -3.975523961781759930 ) ) ;
#58590 = CARTESIAN_POINT ( 'NONE',  ( 134.4004000680750437, 241.7365022471901739, -10.00000000000009237 ) ) ;
#58591 = EDGE_LOOP ( 'NONE', ( #20438, #33945, #35361, #13057 ) ) ;
#58592 = CARTESIAN_POINT ( 'NONE',  ( 26.36427918851389407, 18.14754757982090894, -5.678558825948276656 ) ) ;
#58593 = CARTESIAN_POINT ( 'NONE',  ( 11.86377311551791358, 18.80066082961420548, 10.00000000000000533 ) ) ;
#58594 = CARTESIAN_POINT ( 'NONE',  ( -30.04356256989597895, 94.78415495659865542, 12.60013705013512819 ) ) ;
#58595 = CARTESIAN_POINT ( 'NONE',  ( 54.74956561180287196, 213.9637435831425307, 2.679491924311251605 ) ) ;
#58596 = ORIENTED_EDGE ( 'NONE', *, *, #7089, .T. ) ;
#58597 = CARTESIAN_POINT ( 'NONE',  ( 70.40814973419489320, 60.99421022303731377, 14.40290003289568510 ) ) ;
#58598 = CARTESIAN_POINT ( 'NONE',  ( 157.6629252921874240, 268.6179840388248863, 15.76425181776533790 ) ) ;
#58599 = CARTESIAN_POINT ( 'NONE',  ( 72.30023906772009923, 71.55035954458072922, 5.049600667910633334 ) ) ;
#58600 = CARTESIAN_POINT ( 'NONE',  ( 129.9259354818553618, 252.4865022471903160, 10.00000000000009237 ) ) ;
#58601 = CARTESIAN_POINT ( 'NONE',  ( 157.8820657059571033, 257.1872359237914338, -17.60412210594719440 ) ) ;
#58602 = CARTESIAN_POINT ( 'NONE',  ( 74.77656783286164455, 53.42788812744306881, 16.06606871515787205 ) ) ;
#58603 = EDGE_LOOP ( 'NONE', ( #93346, #27162, #12579, #80920 ) ) ;
#58604 = CARTESIAN_POINT ( 'NONE',  ( 80.01176385998078899, 46.97566021387115143, -13.51455718187173716 ) ) ;
#58605 = CARTESIAN_POINT ( 'NONE',  ( 166.6303123248438851, 247.5856509766914257, -1.864895467279636954 ) ) ;
#58606 = VERTEX_POINT ( 'NONE', #61762 ) ;
#58607 = CYLINDRICAL_SURFACE ( 'NONE', #20779, 10.00000000000010658 ) ;
#58608 = CARTESIAN_POINT ( 'NONE',  ( 85.52743691353181532, 43.19076203672399572, 3.962637686270520376 ) ) ;
#58609 = EDGE_LOOP ( 'NONE', ( #82638, #5942 ) ) ;
#58610 = CARTESIAN_POINT ( 'NONE',  ( 85.97353089263540937, 42.92677418585991234, 0.9306074700887760898 ) ) ;
#58612 = EDGE_CURVE ( 'NONE', #31579, #2203, #33087, .T. ) ;
#58611 = ORIENTED_EDGE ( 'NONE', *, *, #71694, .F. ) ;
#58613 = CARTESIAN_POINT ( 'NONE',  ( 72.21801880702699350, 71.73430858976985292, 5.514776891874389797 ) ) ;
#58614 = CARTESIAN_POINT ( 'NONE',  ( 205.6265063320869899, 274.4914389803786321, 12.09149883072402432 ) ) ;
#58615 = DIRECTION ( 'NONE',  ( -0.8660254037844378194, -0.5000000000000014433, -0.000000000000000000 ) ) ;
#58616 = CARTESIAN_POINT ( 'NONE',  ( 87.93946558867349950, 44.22841546557597781, -4.388681702043145449 ) ) ;
#58617 = CARTESIAN_POINT ( 'NONE',  ( 83.80885942164384517, 50.03953058205711102, 14.02354566334989094 ) ) ;
#58618 = DIRECTION ( 'NONE',  ( -0.000000000000000000, 0.000000000000000000, -1.000000000000000000 ) ) ;
#58619 = CARTESIAN_POINT ( 'NONE',  ( 27.31210279805776509, 33.95586893147756768, 7.433330006724141015 ) ) ;
#58620 = CARTESIAN_POINT ( 'NONE',  ( 71.85117389033869983, 60.90190494782929420, -14.78537330145037032 ) ) ;
#58622 = EDGE_CURVE ( 'NONE', #31579, #50345, #76492, .T. ) ;
#58621 = CARTESIAN_POINT ( 'NONE',  ( 61.87308422990769685, 194.9824982072973683, 3.021315404115420679E-15 ) ) ;
#58623 = CARTESIAN_POINT ( 'NONE',  ( 87.21028088194235295, 45.40991956565691368, 7.116430392365408863 ) ) ;
#58624 = ADVANCED_FACE ( 'NONE', ( #68372 ), #12586, .F. ) ;
#58625 = ORIENTED_EDGE ( 'NONE', *, *, #20019, .F. ) ;
#58626 = ORIENTED_EDGE ( 'NONE', *, *, #95172, .T. ) ;
#58627 = CARTESIAN_POINT ( 'NONE',  ( 81.13146525994932290, 42.42342676164043525, 7.700666981504315167 ) ) ;
#58628 = CARTESIAN_POINT ( 'NONE',  ( 84.41999685182091184, 50.11946239824889915, 13.85565564441014708 ) ) ;
#58630 = CARTESIAN_POINT ( 'NONE',  ( 147.8505793332463725, 274.5622799967613332, -9.317516487097901035 ) ) ;
#58629 = CARTESIAN_POINT ( 'NONE',  ( 204.5730103890532519, 276.3161474792809145, 14.88139715235883109 ) ) ;
#58631 = CARTESIAN_POINT ( 'NONE',  ( 85.77117071415351290, 48.61266522586591776, 12.32040783412941920 ) ) ;
#58632 = CARTESIAN_POINT ( 'NONE',  ( 156.6812872898450735, 261.2670451491295012, 0.000000000000000000 ) ) ;
#58633 = CARTESIAN_POINT ( 'NONE',  ( 147.7487589314264653, 276.5474923016458888, 0.9592504414694114079 ) ) ;
#58634 = CYLINDRICAL_SURFACE ( 'NONE', #3196, 16.60714546451156792 ) ;
#58635 = CARTESIAN_POINT ( 'NONE',  ( 181.3346534254663140, 271.3440730695800767, -17.45372068697093226 ) ) ;
#58636 = PLANE ( 'NONE',  #54980 ) ;
#58637 = CARTESIAN_POINT ( 'NONE',  ( 78.98760635313000478, 59.78900401997537273, 16.49402793498109077 ) ) ;
#58638 = VERTEX_POINT ( 'NONE', #10083 ) ;
#58639 = CARTESIAN_POINT ( 'NONE',  ( -19.65312891409030271, 93.06504152958497400, 177.5919119679930134 ) ) ;
#58640 = DIRECTION ( 'NONE',  ( 0.5000000000000013323, -0.8660254037844378194, 0.000000000000000000 ) ) ;
#58641 = CARTESIAN_POINT ( 'NONE',  ( 166.1101521600732269, 277.8106941408184412, -13.38614590722673903 ) ) ;
#58642 = ORIENTED_EDGE ( 'NONE', *, *, #87242, .T. ) ;
#58643 = CIRCLE ( 'NONE', #87873, 17.82106496071138224 ) ;
#58644 = ORIENTED_EDGE ( 'NONE', *, *, #67817, .T. ) ;
#58645 = VERTEX_POINT ( 'NONE', #63272 ) ;
#58646 = CARTESIAN_POINT ( 'NONE',  ( 87.19094985451131663, 46.20751697815333614, -8.392937380860479024 ) ) ;
#58647 = CIRCLE ( 'NONE', #451, 70.00000000000001421 ) ;
#58649 = B_SPLINE_SURFACE_WITH_KNOTS ( 'NONE', 3, 1, ( 
 ( #34679, #57982 ),
 ( #95032, #9906 ),
 ( #95550, #26098 ),
 ( #86952, #11416 ),
 ( #17485, #56972 ),
 ( #2307, #87470 ),
 ( #79832, #25596 ),
 ( #49887, #87957 ),
 ( #33188, #18005 ),
 ( #80333, #56482 ),
 ( #10902, #25077 ),
 ( #10399, #41777 ),
 ( #72723, #3314 ),
 ( #41268, #34194 ),
 ( #65085, #26597 ),
 ( #57471, #88454 ),
 ( #50379, #80846 ),
 ( #42270, #48393 ),
 ( #88965, #73203 ),
 ( #65581, #19519 ),
 ( #96529, #81332 ),
 ( #42761, #73693 ),
 ( #4277, #35177 ),
 ( #66087, #55957 ),
 ( #79336, #46718 ),
 ( #1648, #8231 ),
 ( #23916, #39598 ),
 ( #93870, #77646 ),
 ( #94365, #33532 ),
 ( #64429, #86283 ),
 ( #39099, #78644 ) ),
 .UNSPECIFIED., .F., .F., .F.,
 ( 4, 3, 3, 3, 3, 3, 3, 3, 3, 3, 4 ),
 ( 2, 2 ),
 ( 0.000000000000000000, 0.1333490885032276307, 0.3007194338854349835, 0.4699862290245034879, 0.5844252810809318355, 0.6686540514502756771, 0.7354980260655390456, 0.8028463152565503691, 0.8633854507757023899, 0.9437142632666907227, 1.000000000000000000 ),
 ( 0.000000000000000000, 1.000000000000000000 ),
 .UNSPECIFIED. ) ;
#58648 = DIRECTION ( 'NONE',  ( -1.000000000000000000, -9.785293164110126558E-14, 0.000000000000000000 ) ) ;
#58650 = CARTESIAN_POINT ( 'NONE',  ( 195.6974783896144174, 291.6890198465123945, 16.70600479393688431 ) ) ;
#58651 = CARTESIAN_POINT ( 'NONE',  ( 160.5099781893591455, 258.1706592185460067, -17.21824937912870013 ) ) ;
#58652 = DIRECTION ( 'NONE',  ( -0.9659258262890649815, 0.2588190451025335070, 8.659560562355099259E-17 ) ) ;
#58653 = ORIENTED_EDGE ( 'NONE', *, *, #41874, .F. ) ;
#58654 = ORIENTED_EDGE ( 'NONE', *, *, #28918, .T. ) ;
#58655 = ADVANCED_FACE ( 'NONE', ( #95227 ), #49082, .F. ) ;
#58656 = CARTESIAN_POINT ( 'NONE',  ( 58.31414817410232843, 216.0217562850347974, 5.155647304959626021E-14 ) ) ;
#58657 = ORIENTED_EDGE ( 'NONE', *, *, #86847, .F. ) ;
#58658 = CIRCLE ( 'NONE', #14978, 15.50000000000000000 ) ;
#58659 = CARTESIAN_POINT ( 'NONE',  ( 165.9969153545198708, 246.1123342570000716, -1.176638740111072723 ) ) ;
#58660 = CARTESIAN_POINT ( 'NONE',  ( 153.3625104204072613, 266.6599839071155884, 16.46888835387834860 ) ) ;
#58661 = CARTESIAN_POINT ( 'NONE',  ( 82.20451920363863962, 44.49317834911897052, 9.706292511583995974 ) ) ;
#58663 = CARTESIAN_POINT ( 'NONE',  ( 69.77715862259884716, 62.22749446745734758, -13.61937327518938723 ) ) ;
#58662 = CARTESIAN_POINT ( 'NONE',  ( 131.1078728602114722, 240.3768266524160424, 9.188101187500098632 ) ) ;
#58664 = DIRECTION ( 'NONE',  ( 0.9985601716053736920, -0.05364311403569550080, 0.000000000000000000 ) ) ;
#58665 = ORIENTED_EDGE ( 'NONE', *, *, #55084, .F. ) ;
#58666 = CARTESIAN_POINT ( 'NONE',  ( 205.0722772166587902, 275.4513919673344731, 14.18415804594472185 ) ) ;
#58667 = CARTESIAN_POINT ( 'NONE',  ( 71.59914813136816747, 63.10835605410795779, 13.72820954599041166 ) ) ;
#58668 = CARTESIAN_POINT ( 'NONE',  ( 81.98951371156157109, 41.06142891364449099, -3.326342120204745623 ) ) ;
#58669 = EDGE_CURVE ( 'NONE', #45905, #99910, #80015, .T. ) ;
#58670 = DIRECTION ( 'NONE',  ( -0.5372068985985075651, -0.8434505012732950169, 0.000000000000000000 ) ) ;
#58671 = CARTESIAN_POINT ( 'NONE',  ( 178.4342578914419732, 285.3753072366883430, 13.06730828328389649 ) ) ;
#58672 = CARTESIAN_POINT ( 'NONE',  ( 76.03251232036760143, 51.31991947663375697, -16.13754705453489180 ) ) ;
#58673 = CARTESIAN_POINT ( 'NONE',  ( 195.4363368379034966, 279.6451395730842364, -17.08598955341190262 ) ) ;
#58674 = CARTESIAN_POINT ( 'NONE',  ( 157.0239713899953244, 269.7369771206523978, 16.31777668093047851 ) ) ;
#58675 = CARTESIAN_POINT ( 'NONE',  ( 79.34578826044543121, 47.78602306556283708, 13.64286931921999368 ) ) ;
#58676 = CARTESIAN_POINT ( 'NONE',  ( -22.42236680055709641, 157.8615022471902591, 0.000000000000000000 ) ) ;
#58677 = CARTESIAN_POINT ( 'NONE',  ( 24.82038151633537026, 14.73415679381822230, 1.333680081654574804E-15 ) ) ;
#58678 = CARTESIAN_POINT ( 'NONE',  ( 77.75702407734982557, 61.66006977308100545, 16.07490810555907146 ) ) ;
#58679 = CARTESIAN_POINT ( 'NONE',  ( 207.8136982414359579, 270.7031114674828700, -0.9536989003868096004 ) ) ;
#58680 = CARTESIAN_POINT ( 'NONE',  ( 48.48788556946983874, 102.1758113618167982, 10.00000000000000000 ) ) ;
#58681 = ADVANCED_FACE ( 'NONE', ( #70886 ), #85630, .F. ) ;
#58682 = CARTESIAN_POINT ( 'NONE',  ( 69.00782751094600087, 70.34284141419077230, -1.981107559596647860 ) ) ;
#58683 = DIRECTION ( 'NONE',  ( 0.8660254037844377084, 0.5000000000000015543, 0.000000000000000000 ) ) ;
#58684 = CARTESIAN_POINT ( 'NONE',  ( -2.330697855141256269, 26.52822386297705393, -10.00000000000000000 ) ) ;
#58685 = CARTESIAN_POINT ( 'NONE',  ( 36.37119629183458613, 23.12755873383628114, -6.180339887498949025 ) ) ;
#58686 = CARTESIAN_POINT ( 'NONE',  ( 75.66122109319597655, 57.70107486379740180, -16.51614346280108947 ) ) ;
#58687 = DIRECTION ( 'NONE',  ( -0.1344185706417126702, 0.9909246428798905715, 0.000000000000000000 ) ) ;
#58688 = DIRECTION ( 'NONE',  ( 0.8660254037844389297, -0.4999999999999995004, 0.000000000000000000 ) ) ;
#58689 = CARTESIAN_POINT ( 'NONE',  ( 82.69282291038285848, 43.21275928182573267, -7.572188776693871581 ) ) ;
#58690 = CARTESIAN_POINT ( 'NONE',  ( 161.1093323826042933, 251.5974460702646809, -13.93502574894237078 ) ) ;
#58691 = CARTESIAN_POINT ( 'NONE',  ( 13.46382118881039602, 169.3923013555410080, 4.594050593750050204 ) ) ;
#58692 = CARTESIAN_POINT ( 'NONE',  ( 69.04267406240978744, 70.00324579014528581, 5.266832899270860402 ) ) ;
#58693 = ORIENTED_EDGE ( 'NONE', *, *, #100054, .T. ) ;
#58695 = CARTESIAN_POINT ( 'NONE',  ( 86.86399242946149002, 45.94634269538593685, 8.946615921987719489 ) ) ;
#58694 = B_SPLINE_CURVE_WITH_KNOTS ( 'NONE', 3,
 ( #68011, #75625, #6212, #76142 ),
 .UNSPECIFIED., .F., .F.,
 ( 4, 4 ),
 ( 0.000000000000000000, 0.1555655374897298437 ),
 .UNSPECIFIED. ) ;
#58696 = LINE ( 'NONE', #20231, #3063 ) ;
#58697 = CARTESIAN_POINT ( 'NONE',  ( 72.10465435074424079, 72.28376592976228210, -1.461586084520088091 ) ) ;
#58698 = CARTESIAN_POINT ( 'NONE',  ( 46.91405240998433612, 188.7048013555409796, 4.594050593750051981 ) ) ;
#58699 = VECTOR ( 'NONE', #78942, 1000.000000000000000 ) ;
#58700 = CARTESIAN_POINT ( 'NONE',  ( 86.80989918712758424, 45.87808919071956382, 8.896275332294523608 ) ) ;
#58701 = CARTESIAN_POINT ( 'NONE',  ( 171.2125587931870427, 286.8147667620277161, 7.172632356338288773 ) ) ;
#58702 = CARTESIAN_POINT ( 'NONE',  ( 146.8729474948188454, 276.2555880120147549, 3.934020695290606273 ) ) ;
#58703 = CARTESIAN_POINT ( 'NONE',  ( 7.127696690345725727, 16.06628583063839244, -9.188101187500006262 ) ) ;
#58704 = CARTESIAN_POINT ( 'NONE',  ( 198.1292909865887566, 287.0949182644739039, 16.93298125210290550 ) ) ;
#58705 = CARTESIAN_POINT ( 'NONE',  ( 146.5689048584090699, 276.7822053059436485, -0.4306668706573002492 ) ) ;
#58706 = CARTESIAN_POINT ( 'NONE',  ( 179.3320168101770378, 276.6075631236466847, 16.30429811271319451 ) ) ;
#58707 = CARTESIAN_POINT ( 'NONE',  ( 179.1186523009620544, 278.4480982664924795, -17.05943142709577387 ) ) ;
#58708 = CARTESIAN_POINT ( 'NONE',  ( 148.4572820722141557, 276.8246940256113930, 2.891641560416912338 ) ) ;
#58709 = CARTESIAN_POINT ( 'NONE',  ( 119.0307608796806278, 227.9824982072973683, 3.021315404115420679E-15 ) ) ;
#58710 = VECTOR ( 'NONE', #4903, 1000.000000000000114 ) ;
#58711 = DIRECTION ( 'NONE',  ( -0.8660254037844387076, -0.4999999999999998890, -0.000000000000000000 ) ) ;
#58712 = CARTESIAN_POINT ( 'NONE',  ( 89.29491028763546012, 232.3615022471903160, 5.000000000000046185 ) ) ;
#58713 = CARTESIAN_POINT ( 'NONE',  ( 81.90189478934432543, 58.86607563204950822, -0.3830222215594885626 ) ) ;
#58714 = CARTESIAN_POINT ( 'NONE',  ( 161.6164657043237014, 267.7223936679948224, -17.07498630821350005 ) ) ;
#58715 = ORIENTED_EDGE ( 'NONE', *, *, #39187, .T. ) ;
#58716 = CARTESIAN_POINT ( 'NONE',  ( 65.88516108981343677, 208.8458772461660544, 9.188101187500095079 ) ) ;
#58717 = VERTEX_POINT ( 'NONE', #55154 ) ;
#58718 = DIRECTION ( 'NONE',  ( -0.9839629614562445115, 0.1783728972749415165, 0.000000000000000000 ) ) ;
#58719 = PLANE ( 'NONE',  #74041 ) ;
#58720 = CARTESIAN_POINT ( 'NONE',  ( 67.44257088933083821, 67.25355904253446226, -8.657396272464442433 ) ) ;
#58721 = ORIENTED_EDGE ( 'NONE', *, *, #13604, .T. ) ;
#58723 = DIRECTION ( 'NONE',  ( -0.7694697644498993405, 0.6386832404231509441, 0.000000000000000000 ) ) ;
#58722 = VECTOR ( 'NONE', #13890, 1000.000000000000000 ) ;
#58724 = CARTESIAN_POINT ( 'NONE',  ( 164.8329445879545290, 245.1479605429143760, -2.955380775890217304 ) ) ;
#58725 = CARTESIAN_POINT ( 'NONE',  ( -19.65312891409030271, 93.06504152958497400, 177.5919119679930134 ) ) ;
#58726 = CARTESIAN_POINT ( 'NONE',  ( 29.48198420892518357, 37.99752408145594273, 5.678558825948277544 ) ) ;
#58727 = DIRECTION ( 'NONE',  ( -0.8035972437015875824, -0.5951734788405910193, 0.000000000000000000 ) ) ;
#58728 = FACE_OUTER_BOUND ( 'NONE', #85528, .T. ) ;
#58729 = CARTESIAN_POINT ( 'NONE',  ( 172.0805575621569687, 256.0411262410343625, 11.22366668844141202 ) ) ;
#58730 = ORIENTED_EDGE ( 'NONE', *, *, #28700, .T. ) ;
#58731 = CARTESIAN_POINT ( 'NONE',  ( 68.49108285301745980, 64.31732535079238744, 12.34849984288629976 ) ) ;
#58732 = DIRECTION ( 'NONE',  ( 0.000000000000000000, 0.000000000000000000, 1.000000000000000000 ) ) ;
#58733 = CARTESIAN_POINT ( 'NONE',  ( 16.56913029798217352, 168.8262482093458061, 3.021315404115420679E-15 ) ) ;
#58734 = ORIENTED_EDGE ( 'NONE', *, *, #70890, .T. ) ;
#58736 = ADVANCED_FACE ( 'NONE', ( #86140 ), #40947, .F. ) ;
#58735 = CARTESIAN_POINT ( 'NONE',  ( 77.68610095332765297, 61.14218577032889357, 16.17973444202652189 ) ) ;
#58737 = CARTESIAN_POINT ( 'NONE',  ( 151.2057546125658973, 268.7509459446807227, 15.78031848731319187 ) ) ;
#58738 = CARTESIAN_POINT ( 'NONE',  ( 159.6288139302610887, 254.1617792512662675, -15.32287760493869477 ) ) ;
#58739 = B_SPLINE_CURVE_WITH_KNOTS ( 'NONE', 3,
 ( #78248, #71155, #8828, #63529 ),
 .UNSPECIFIED., .F., .F.,
 ( 4, 4 ),
 ( 0.000000000000000000, 0.004615008360511261773 ),
 .UNSPECIFIED. ) ;
#58740 = EDGE_CURVE ( 'NONE', #61222, #69960, #77987, .T. ) ;
#58741 = VERTEX_POINT ( 'NONE', #1982 ) ;
#58742 = ORIENTED_EDGE ( 'NONE', *, *, #81639, .T. ) ;
#58744 = DIRECTION ( 'NONE',  ( 0.000000000000000000, 0.000000000000000000, 1.000000000000000000 ) ) ;
#58743 = CARTESIAN_POINT ( 'NONE',  ( 207.4541616930702617, 271.3258470364304458, -6.834942797545373594 ) ) ;
#58745 = CARTESIAN_POINT ( 'NONE',  ( 148.9322735291567597, 272.6887306911919495, -12.40988026045598858 ) ) ;
#58746 = ORIENTED_EDGE ( 'NONE', *, *, #3463, .T. ) ;
#58747 = CARTESIAN_POINT ( 'NONE',  ( 66.50139985668020870, 68.79878299985570322, -2.191674848154488764 ) ) ;
#58748 = EDGE_CURVE ( 'NONE', #42933, #34456, #4486, .T. ) ;
#58749 = CARTESIAN_POINT ( 'NONE',  ( 159.2077906806335932, 254.8910129107889588, 16.14624949541834553 ) ) ;
#58750 = DIRECTION ( 'NONE',  ( 2.816764622163176999E-16, 1.626259812849726945E-16, -1.000000000000000000 ) ) ;
#58751 = CARTESIAN_POINT ( 'NONE',  ( 78.14988184308933228, 61.89697373328141339, -16.07278474554906467 ) ) ;
#58752 = ADVANCED_FACE ( 'NONE', ( #25269 ), #71894, .T. ) ;
#58753 = CARTESIAN_POINT ( 'NONE',  ( 121.5276403787286341, 228.7202760586659736, -5.415160957724236172E-17 ) ) ;
#58754 = CARTESIAN_POINT ( 'NONE',  ( -76.86719868626529717, 52.73452925779879763, 10.00000000000000000 ) ) ;
#58755 = CYLINDRICAL_SURFACE ( 'NONE', #15686, 10.00000000000010658 ) ;
#58756 = CARTESIAN_POINT ( 'NONE',  ( 107.4814437671086580, 242.8615022471903160, 5.000000000000046185 ) ) ;
#58757 = ORIENTED_EDGE ( 'NONE', *, *, #48139, .F. ) ;
#58758 = CARTESIAN_POINT ( 'NONE',  ( 207.5570596878370679, 271.1476224814971374, 2.444960520848353358 ) ) ;
#58759 = ORIENTED_EDGE ( 'NONE', *, *, #72142, .T. ) ;
#58760 = ORIENTED_EDGE ( 'NONE', *, *, #41746, .F. ) ;
#58761 = FACE_BOUND ( 'NONE', #40565, .T. ) ;
#58762 = CARTESIAN_POINT ( 'NONE',  ( 75.30635741883537548, 66.56121636111578255, -13.10152444272999617 ) ) ;
#58763 = CARTESIAN_POINT ( 'NONE',  ( 68.53719034102077501, 216.5024278399160664, 9.188101187500095079 ) ) ;
#58764 = CARTESIAN_POINT ( 'NONE',  ( 28.28448313147312021, 16.73415679381822585, 1.333680081654574804E-15 ) ) ;
#58765 = CARTESIAN_POINT ( 'NONE',  ( 81.90070505019525626, 55.28399500932853528, 16.25061773925407493 ) ) ;
#58766 = CARTESIAN_POINT ( 'NONE',  ( 198.6455782124543248, 286.5827611675690605, 17.19551065434971093 ) ) ;
#58767 = FACE_OUTER_BOUND ( 'NONE', #28041, .T. ) ;
#58768 = ORIENTED_EDGE ( 'NONE', *, *, #50081, .T. ) ;
#58769 = CARTESIAN_POINT ( 'NONE',  ( 69.32120137048818265, 64.30962851660092383, -12.08911290385783488 ) ) ;
#58770 = CARTESIAN_POINT ( 'NONE',  ( 201.4520623681621316, 281.7217880192456505, -17.56577389517433119 ) ) ;
#58771 = CARTESIAN_POINT ( 'NONE',  ( 155.4661767250933622, 261.3716783840932294, -17.10192542004562810 ) ) ;
#58772 = ORIENTED_EDGE ( 'NONE', *, *, #59510, .T. ) ;
#58773 = CARTESIAN_POINT ( 'NONE',  ( 185.4867332780130766, 297.4061142773095412, 5.671143563000668131 ) ) ;
#58774 = CARTESIAN_POINT ( 'NONE',  ( 161.3145230519951951, 251.2420454056404822, -14.44869077440025151 ) ) ;
#58775 = CARTESIAN_POINT ( 'NONE',  ( 146.9422184197532317, 276.1356072505412840, -5.063317562214876943 ) ) ;
#58776 = CARTESIAN_POINT ( 'NONE',  ( 59.32682287396359300, 198.3927522451418213, 10.00000000000009948 ) ) ;
#58777 = CARTESIAN_POINT ( 'NONE',  ( 164.9103019330012216, 245.0139736909548560, 2.841678961959298810 ) ) ;
#58778 = CLOSED_SHELL ( 'NONE', ( #25626, #51936, #5896, #5479, #83177, #82515, #23630, #87689, #79528, #68882, #62176, #78872, #49495, #64910, #68368, #34148, #15314, #32997, #45883, #6375, #31333, #88629, #9506, #32411, #34796, #70340, #17365, #80228, #84872, #10849, #99041, #81917, #50749, #53458, #61264, #17082 ) ) ;
#58779 = CARTESIAN_POINT ( 'NONE',  ( 208.1757572214753793, 270.0760069187178374, 2.172546422564154867 ) ) ;
#58780 = B_SPLINE_CURVE_WITH_KNOTS ( 'NONE', 3,
 ( #11951, #28128, #67622, #66133 ),
 .UNSPECIFIED., .F., .F.,
 ( 4, 4 ),
 ( 0.04223839839039728733, 0.04887120950165271815 ),
 .UNSPECIFIED. ) ;
#58781 = CARTESIAN_POINT ( 'NONE',  ( 126.3172359758225554, 252.9244531367911293, -4.594050593750046652 ) ) ;
#58782 = EDGE_LOOP ( 'NONE', ( #11346, #42264, #4820, #29376, #99246, #24031 ) ) ;
#58783 = CARTESIAN_POINT ( 'NONE',  ( 82.57684337742131220, 44.21772893957315631, -9.119279311071077032 ) ) ;
#58784 = CARTESIAN_POINT ( 'NONE',  ( 85.77746269900303844, 44.00077978609508023, 5.766797212797135863 ) ) ;
#58785 = CARTESIAN_POINT ( 'NONE',  ( 203.2732885619977026, 278.5673317194472247, -16.64305493556850024 ) ) ;
#58786 = CARTESIAN_POINT ( 'NONE',  ( 79.36123937160471087, 59.78439649202068296, -16.16115984811566264 ) ) ;
#58787 = CARTESIAN_POINT ( 'NONE',  ( 75.44622636097695079, 64.91049876765895021, 14.07243495672977929 ) ) ;
#58788 = DIRECTION ( 'NONE',  ( 0.4999999999999998890, -0.8660254037844385966, 0.000000000000000000 ) ) ;
#58789 = ORIENTED_EDGE ( 'NONE', *, *, #36196, .T. ) ;
#58790 = CARTESIAN_POINT ( 'NONE',  ( 77.17013742012716193, 58.35697113532116731, 16.12913492606394428 ) ) ;
#58791 = CARTESIAN_POINT ( 'NONE',  ( 34.97213163436671124, 51.32435524152969464, 10.00000000000000000 ) ) ;
#58792 = AXIS2_PLACEMENT_3D ( 'NONE', #5906, #83442, #36796 ) ;
#58793 = CARTESIAN_POINT ( 'NONE',  ( 72.63051688559265529, 71.46180251613422740, -5.713833537422692288 ) ) ;
#58794 = PLANE ( 'NONE',  #98567 ) ;
#58795 = CARTESIAN_POINT ( 'NONE',  ( 38.03703169759616287, 182.7677522451417929, -5.000000000000041744 ) ) ;
#58796 = CARTESIAN_POINT ( 'NONE',  ( 202.6334567748964730, 267.3808444593984746, 0.8764476327814421097 ) ) ;
#58797 = CARTESIAN_POINT ( 'NONE',  ( 196.2953682204578456, 263.5854184417236752, 0.8810977108677261471 ) ) ;
#58798 = CIRCLE ( 'NONE', #75110, 0.1418229129684644985 ) ;
#58799 = CARTESIAN_POINT ( 'NONE',  ( 147.4317198359019301, 275.2877659273946733, 3.797273160043843188 ) ) ;
#58800 = DIRECTION ( 'NONE',  ( 0.000000000000000000, 0.000000000000000000, 1.000000000000000000 ) ) ;
#58801 = ADVANCED_FACE ( 'NONE', ( #66273 ), #82525, .T. ) ;
#58802 = CARTESIAN_POINT ( 'NONE',  ( 204.6475128369918082, 276.1871054541632020, -13.72068618491070779 ) ) ;
#58803 = CARTESIAN_POINT ( 'NONE',  ( 170.6625046707854665, 250.4727288339191773, 3.630827311776036570 ) ) ;
#58804 = CARTESIAN_POINT ( 'NONE',  ( 24.66226663818958187, 15.20801979619928979, -3.090169943749474069 ) ) ;
#58805 = CARTESIAN_POINT ( 'NONE',  ( 190.0226014859668453, 301.5181949703289774, 3.835066345245774500 ) ) ;
#58806 = DIRECTION ( 'NONE',  ( -1.804112415015878984E-15, 1.000000000000000000, -0.000000000000000000 ) ) ;
#58807 = CARTESIAN_POINT ( 'NONE',  ( 49.65150239490934325, 78.72539382324356438, 59.99999999999999289 ) ) ;
#58808 = CARTESIAN_POINT ( 'NONE',  ( 203.1044072055706806, 278.8598428092302584, -16.67109798570195878 ) ) ;
#58809 = CARTESIAN_POINT ( 'NONE',  ( 72.18990340680744566, 72.03918383723207342, -3.149060597287207219 ) ) ;
#58810 = CARTESIAN_POINT ( 'NONE',  ( 132.9389821956408184, 260.8927522451419918, 2.944929066748280225E-16 ) ) ;
#58811 = CARTESIAN_POINT ( 'NONE',  ( 175.4000927154525584, 286.5048389028432894, -12.54572841542827710 ) ) ;
#58812 = ORIENTED_EDGE ( 'NONE', *, *, #6405, .T. ) ;
#58813 = EDGE_CURVE ( 'NONE', #8200, #5590, #26775, .T. ) ;
#58814 = CARTESIAN_POINT ( 'NONE',  ( 196.2255671652529259, 290.7743432561995860, 16.01325193769018185 ) ) ;
#58815 = CARTESIAN_POINT ( 'NONE',  ( 151.4376533647338476, 268.3492855237141725, -15.16853828792834236 ) ) ;
#58816 = CARTESIAN_POINT ( 'NONE',  ( -2.963858511049441979, 169.0958772461660544, -9.188101187500095079 ) ) ;
#58817 = CARTESIAN_POINT ( 'NONE',  ( 54.00411475982191689, 211.1744531367911293, 4.594050593750047540 ) ) ;
#58818 = CARTESIAN_POINT ( 'NONE',  ( 178.9106358762607272, 258.8247338180944439, -11.56834183610952316 ) ) ;
#58819 = CARTESIAN_POINT ( 'NONE',  ( 23.98812876850004727, 25.80066082961422325, 10.00000000000000533 ) ) ;
#58820 = CARTESIAN_POINT ( 'NONE',  ( 85.56715572150820037, 48.66046822832736041, 12.44852408270450184 ) ) ;
#58821 = CARTESIAN_POINT ( 'NONE',  ( 205.2391015854675516, 275.1624436846170738, -14.01434138479280911 ) ) ;
#58822 = CARTESIAN_POINT ( 'NONE',  ( 72.09461912472968947, 72.35512880999853280, -3.358616764072534178 ) ) ;
#58823 = CARTESIAN_POINT ( 'NONE',  ( 74.04272560325144070, 55.47781366761107336, -16.11579405751482241 ) ) ;
#58825 = CARTESIAN_POINT ( 'NONE',  ( 62.79092448910127189, 220.3927522451419350, 2.944929066748280225E-16 ) ) ;
#58824 = CARTESIAN_POINT ( 'NONE',  ( 167.9782759209660128, 256.7986816940351105, 13.70024866366997962 ) ) ;
#58826 = CARTESIAN_POINT ( 'NONE',  ( 179.4461805389133531, 254.8738420869291019, -4.069619891950734036 ) ) ;
#58827 = CARTESIAN_POINT ( 'NONE',  ( 198.4383541551818553, 286.9416837633153250, 16.97133247567711578 ) ) ;
#58828 = CARTESIAN_POINT ( 'NONE',  ( 55.59208832369112230, 196.2365022471902023, 10.00000000000009592 ) ) ;
#58829 = DIRECTION ( 'NONE',  ( -0.8660254037844387076, -0.4999999999999998890, -0.000000000000000000 ) ) ;
#58830 = CARTESIAN_POINT ( 'NONE',  ( 147.6220714307702622, 274.9580672937808572, 8.392894244419288441 ) ) ;
#58831 = CARTESIAN_POINT ( 'NONE',  ( 16.25090658753528317, 186.3149278399161233, 9.188101187500093303 ) ) ;
#58832 = CARTESIAN_POINT ( 'NONE',  ( 72.84354978475252551, 71.10232518220604447, -7.524857974791624216 ) ) ;
#58833 = CARTESIAN_POINT ( 'NONE',  ( 78.96537477373632896, 60.10141448056572955, 16.11562121875446252 ) ) ;
#58834 = CARTESIAN_POINT ( 'NONE',  ( 39.87427548755113804, 25.94754757982092741, 5.678558825948272215 ) ) ;
#58835 = CARTESIAN_POINT ( 'NONE',  ( 159.8896510172052103, 272.0516993742419345, 16.05765770493651701 ) ) ;
#58836 = CARTESIAN_POINT ( 'NONE',  ( 181.2600193737777374, 277.7392251741971450, 16.38192420661602711 ) ) ;
#58837 = CARTESIAN_POINT ( 'NONE',  ( 80.88635954517316407, 43.32100077011654804, -9.977154956976749034 ) ) ;
#58838 = DIRECTION ( 'NONE',  ( -0.8660254037844377084, -0.5000000000000014433, -0.000000000000000000 ) ) ;
#58839 = CARTESIAN_POINT ( 'NONE',  ( 13.73114039420206645, 19.87878583063839955, -9.188101187500006262 ) ) ;
#58840 = CARTESIAN_POINT ( 'NONE',  ( 164.9538401224995425, 286.5040288536138746, -0.08628193082933090230 ) ) ;
#58841 = DIRECTION ( 'NONE',  ( -0.8660254037844387076, -0.4999999999999998890, -0.000000000000000000 ) ) ;
#58842 = CARTESIAN_POINT ( 'NONE',  ( 183.6964659824695332, 271.1858650112955615, -17.13366558732818135 ) ) ;
#58843 = AXIS2_PLACEMENT_3D ( 'NONE', #71469, #1055, #62 ) ;
#58844 = CARTESIAN_POINT ( 'NONE',  ( 78.55537653917157570, 48.00561504237174404, -13.97647359956260082 ) ) ;
#58845 = EDGE_LOOP ( 'NONE', ( #96473, #55782, #39793, #24078 ) ) ;
#58846 = CARTESIAN_POINT ( 'NONE',  ( 75.16744714750042533, 53.52973880860442080, -16.05274081456337143 ) ) ;
#58847 = DIRECTION ( 'NONE',  ( -0.5000000000000003331, 0.8660254037844383745, -9.251858538542983907E-17 ) ) ;
#58848 = EDGE_LOOP ( 'NONE', ( #48958, #86221, #76260, #52635, #44355, #857 ) ) ;
#58849 = CARTESIAN_POINT ( 'NONE',  ( 192.7693357657653053, 296.7607116428271183, 12.22606306887835714 ) ) ;
#58850 = LINE ( 'NONE', #67469, #67604 ) ;
#58851 = CARTESIAN_POINT ( 'NONE',  ( 66.74649031818020717, 68.37427386808708718, 4.497794777592671878 ) ) ;
#58852 = CARTESIAN_POINT ( 'NONE',  ( 202.7754741559590173, 279.4295715634463022, -15.65855077192107636 ) ) ;
#58853 = AXIS2_PLACEMENT_3D ( 'NONE', #18784, #50654, #80620 ) ;
#58854 = ORIENTED_EDGE ( 'NONE', *, *, #8879, .T. ) ;
#58855 = EDGE_LOOP ( 'NONE', ( #9889, #25087, #43846, #64929 ) ) ;
#58857 = CARTESIAN_POINT ( 'NONE',  ( 163.9587364689194260, 246.6621334214722481, 5.816126667419880825 ) ) ;
#58856 = CYLINDRICAL_SURFACE ( 'NONE', #55132, 10.00000000000010658 ) ;
#58858 = CARTESIAN_POINT ( 'NONE',  ( 152.8107382695299918, 265.9710327055011589, 16.32045346488711246 ) ) ;
#58859 = ORIENTED_EDGE ( 'NONE', *, *, #19232, .F. ) ;
#58860 = CARTESIAN_POINT ( 'NONE',  ( 88.01315147845571119, 43.76068472133272280, -2.215761827693341957 ) ) ;
#58861 = CARTESIAN_POINT ( 'NONE',  ( 80.71776722511965829, 57.44908488972237137, 16.57971273854668226 ) ) ;
#58862 = CARTESIAN_POINT ( 'NONE',  ( 174.8371417102094370, 262.4333147357459666, 14.35597617782233471 ) ) ;
#58863 = VERTEX_POINT ( 'NONE', #57156 ) ;
#58865 = EDGE_CURVE ( 'NONE', #39534, #76006, #29499, .T. ) ;
#58864 = CARTESIAN_POINT ( 'NONE',  ( 87.53583079710631409, 45.45925790797146249, -6.823327534849023657 ) ) ;
#58866 = CARTESIAN_POINT ( 'NONE',  ( 164.5139018292655919, 259.6662038739244736, -17.01387605652571366 ) ) ;
#58867 = AXIS2_PLACEMENT_3D ( 'NONE', #13653, #91180, #75976 ) ;
#58868 = CARTESIAN_POINT ( 'NONE',  ( 149.7200635338602410, 271.3242383773507527, -12.12223662813266500 ) ) ;
#58869 = ORIENTED_EDGE ( 'NONE', *, *, #89149, .T. ) ;
#58870 = DIRECTION ( 'NONE',  ( 0.5000000000000048850, -0.8660254037844358210, 0.000000000000000000 ) ) ;
#58871 = CARTESIAN_POINT ( 'NONE',  ( 164.2545401858843945, 246.1497863546213978, 2.275217130759496609 ) ) ;
#58872 = CARTESIAN_POINT ( 'NONE',  ( 73.86319654356421438, 60.42244647389022560, 15.35035339019570877 ) ) ;
#58873 = B_SPLINE_SURFACE_WITH_KNOTS ( 'NONE', 3, 1, ( 
 ( #12896, #10014 ),
 ( #13381, #43253 ),
 ( #49011, #63703 ),
 ( #94640, #43752 ),
 ( #74696, #25195 ),
 ( #79945, #2422 ),
 ( #64201, #36154 ),
 ( #5275, #10508 ),
 ( #33823, #81812 ),
 ( #72331, #2934 ),
 ( #17604, #67058 ),
 ( #56079, #97981 ),
 ( #28558, #48513 ),
 ( #95150, #56595 ),
 ( #95661, #26210 ),
 ( #57087, #88068 ),
 ( #18617, #50861 ),
 ( #74198, #4787 ),
 ( #35667, #21957 ),
 ( #15843, #90916 ),
 ( #7247, #31046 ),
 ( #21465, #14850 ),
 ( #60943, #68056 ),
 ( #5760, #6762 ),
 ( #14366, #46752 ),
 ( #15334, #98979 ),
 ( #69047, #29563 ),
 ( #38129, #99976 ),
 ( #61445, #60437 ),
 ( #61933, #92885 ),
 ( #38648, #98489 ) ),
 .UNSPECIFIED., .F., .F., .F.,
 ( 4, 3, 3, 3, 3, 3, 3, 3, 3, 3, 4 ),
 ( 2, 2 ),
 ( 0.000000000000000000, 0.1333490885032317663, 0.3007194338854262683, 0.4699862290245025997, 0.5844252810809391629, 0.6686540514502795629, 0.7354980260655534785, 0.8028463152565619154, 0.8633854507757232621, 0.9437142632667340214, 1.000000000000000000 ),
 ( 0.000000000000000000, 1.000000000000000000 ),
 .UNSPECIFIED. ) ;
#58874 = EDGE_LOOP ( 'NONE', ( #92420, #36559, #21572, #70587 ) ) ;
#58875 = CARTESIAN_POINT ( 'NONE',  ( 190.0896302098338424, 301.4020978150248311, 3.433521196325825642 ) ) ;
#58876 = CARTESIAN_POINT ( 'NONE',  ( 172.1455357562699362, 263.5618832647229510, -15.46582821167986488 ) ) ;
#58877 = VERTEX_POINT ( 'NONE', #13087 ) ;
#58878 = CARTESIAN_POINT ( 'NONE',  ( 31.31925169811195175, 41.58029201028044497, 1.583844403245397769 ) ) ;
#58879 = ORIENTED_EDGE ( 'NONE', *, *, #1124, .F. ) ;
#58880 = CARTESIAN_POINT ( 'NONE',  ( 157.7063754007213845, 268.8955880366740416, 15.63381455156026867 ) ) ;
#58881 = ORIENTED_EDGE ( 'NONE', *, *, #13818, .F. ) ;
#58882 = CARTESIAN_POINT ( 'NONE',  ( 156.5028614784543208, 266.9798413144324059, -16.21780324415792762 ) ) ;
#58883 = CARTESIAN_POINT ( 'NONE',  ( -1.087500518889665591, 25.57194971796826621, 177.5919119679930134 ) ) ;
#58884 = CARTESIAN_POINT ( 'NONE',  ( -7.720288864461156919, 177.8967562850347122, -4.648177544792955347E-16 ) ) ;
#58885 = CARTESIAN_POINT ( 'NONE',  ( 16.59523773630703758, 17.78052372038640172, -10.00000000000000355 ) ) ;
#58886 = CARTESIAN_POINT ( 'NONE',  ( 192.7693357657653053, 296.7607116428271183, 12.22606306887835714 ) ) ;
#58887 = CARTESIAN_POINT ( 'NONE',  ( 87.78081971166569986, 44.10618430004836910, 2.676874261813567468 ) ) ;
#58888 = CARTESIAN_POINT ( 'NONE',  ( 158.7310127332570460, 255.7168165395733581, -16.04306221441551017 ) ) ;
#58889 = ORIENTED_EDGE ( 'NONE', *, *, #42188, .T. ) ;
#58890 = CARTESIAN_POINT ( 'NONE',  ( 80.11389927631944374, 55.76916087316497084, -16.10389376604875977 ) ) ;
#58891 = CARTESIAN_POINT ( 'NONE',  ( 165.0538309624641613, 244.7653741195639157, 2.311334310144196547 ) ) ;
#58893 = VERTEX_POINT ( 'NONE', #97208 ) ;
#58892 = DIRECTION ( 'NONE',  ( 0.000000000000000000, 0.000000000000000000, 1.000000000000000000 ) ) ;
#58894 = CARTESIAN_POINT ( 'NONE',  ( 190.4556184745922280, 300.2183394804145564, 2.916409228186030322 ) ) ;
#58895 = B_SPLINE_CURVE_WITH_KNOTS ( 'NONE', 3,
 ( #86049, #48990, #56055, #71299 ),
 .UNSPECIFIED., .F., .F.,
 ( 4, 4 ),
 ( 0.01127661141674762141, 0.01717785629562665339 ),
 .UNSPECIFIED. ) ;
#58896 = CARTESIAN_POINT ( 'NONE',  ( 176.5821120313724464, 290.0546866683789062, -9.551980326619117889 ) ) ;
#58897 = ORIENTED_EDGE ( 'NONE', *, *, #9246, .T. ) ;
#58898 = CARTESIAN_POINT ( 'NONE',  ( 81.56337590313989949, 52.27981926771280285, -15.13415753732220281 ) ) ;
#58899 = CARTESIAN_POINT ( 'NONE',  ( 197.8666518381295987, 272.7614078478216015, 14.30677244657330860 ) ) ;
#58900 = CARTESIAN_POINT ( 'NONE',  ( 193.8003511027313550, 288.1208047801705447, 17.19107869180001913 ) ) ;
#58901 = CARTESIAN_POINT ( 'NONE',  ( 198.7680848198567674, 286.3705734992850580, -17.20718207227004015 ) ) ;
#58902 = CARTESIAN_POINT ( 'NONE',  ( 102.1896198688571644, 218.2592609112380160, 2.679491924311254714 ) ) ;
#58903 = ORIENTED_EDGE ( 'NONE', *, *, #3427, .T. ) ;
#58904 = CARTESIAN_POINT ( 'NONE',  ( 170.5267406923843510, 255.5323226702545583, -11.62603975033689352 ) ) ;
#58905 = CARTESIAN_POINT ( 'NONE',  ( 82.56870460112591559, 41.65958751012770733, 5.823109254649875055 ) ) ;
#58906 = B_SPLINE_CURVE_WITH_KNOTS ( 'NONE', 3,
 ( #2818, #56975, #87961, #49891, #86955, #25600, #56486, #18505, #87474, #65088, #26600, #57474, #88457, #19016, #51890, #5778, #52374, #74214, #36666, #29580, #12403, #67574, #82831, #75693, #21009, #35686, #98506, #13399, #44271, #89924, #50879, #51375, #4804, #75201, #82343, #12911, #42764, #59456, #66587, #59962, #83317, #37174, #43268, #97997, #60457, #67074 ),
 .UNSPECIFIED., .F., .F.,
 ( 4, 2, 2, 2, 2, 2, 2, 2, 2, 2, 2, 2, 2, 2, 2, 2, 2, 2, 2, 2, 2, 2, 4 ),
 ( 0.002536418406735530592, 0.002949603472297969257, 0.003156196005079241716, 0.003259492271469948202, 0.003362788537860654688, 0.003466084804251361607, 0.003569381070642068526, 0.003775973603423508820, 0.004189158668986388973, 0.005015528800112283719, 0.005841898931238180201, 0.006668269062364074948, 0.007081454127926947728, 0.007494639193489818774, 0.007597935459880630210, 0.007649583593076001234, 0.007701231726271372258, 0.007804527992662112570, 0.007907824259052854618, 0.008321009324615878319, 0.008734194390178900286, 0.008940786922960408667, 0.009147379455741920518 ),
 .UNSPECIFIED. ) ;
#58907 = CARTESIAN_POINT ( 'NONE',  ( 201.3505934466285510, 281.8975373467312693, -16.83770227898004279 ) ) ;
#58908 = CARTESIAN_POINT ( 'NONE',  ( 155.3874097416376969, 262.7157056314985653, 17.32087637530853641 ) ) ;
#58909 = CARTESIAN_POINT ( 'NONE',  ( 26.41785753015485128, 199.3927522451419634, 2.944929066748280225E-16 ) ) ;
#58910 = CARTESIAN_POINT ( 'NONE',  ( 112.3797264076079756, 241.8149278399160949, 9.188101187500093303 ) ) ;
#58911 = CARTESIAN_POINT ( 'NONE',  ( 82.79584117221035910, 40.63928722116583714, -1.337132909417009907 ) ) ;
#58912 = CARTESIAN_POINT ( 'NONE',  ( 164.1420675163463159, 280.3382853379264930, -11.37976142735245588 ) ) ;
#58913 = CARTESIAN_POINT ( 'NONE',  ( -4.731736819106164837, 24.67387208536690224, -10.00000000000000000 ) ) ;
#58914 = CARTESIAN_POINT ( 'NONE',  ( 33.95012722949724093, 202.6589784336661637, -6.496448406907675876E-16 ) ) ;
#58915 = EDGE_CURVE ( 'NONE', #21781, #79669, #17181, .T. ) ;
#58916 = CARTESIAN_POINT ( 'NONE',  ( 200.7523954295751594, 282.9336467052548869, 18.23634913067694185 ) ) ;
#58917 = VERTEX_POINT ( 'NONE', #18683 ) ;
#58918 = VERTEX_POINT ( 'NONE', #20677 ) ;
#58919 = CARTESIAN_POINT ( 'NONE',  ( 190.3268461984029614, 299.2279209427761657, 7.463966244697216368 ) ) ;
#58920 = CARTESIAN_POINT ( 'NONE',  ( 185.8237621104296409, 258.7144012905565660, -5.701851391998975949 ) ) ;
#58921 = CARTESIAN_POINT ( 'NONE',  ( 20.28351092001508960, 192.5177522451419350, 5.000000000000046185 ) ) ;
#58922 = CARTESIAN_POINT ( 'NONE',  ( 101.6898988757523625, 229.5177522451418781, -10.00000000000009592 ) ) ;
#58923 = AXIS2_PLACEMENT_3D ( 'NONE', #38249, #270, #84907 ) ;
#58924 = DIRECTION ( 'NONE',  ( 0.000000000000000000, 0.000000000000000000, 1.000000000000000000 ) ) ;
#58925 = FACE_OUTER_BOUND ( 'NONE', #1847, .T. ) ;
#58926 = CARTESIAN_POINT ( 'NONE',  ( 96.56591523669446531, 219.8927522451417929, -10.00000000000009059 ) ) ;
#58927 = VERTEX_POINT ( 'NONE', #90105 ) ;
#58928 = EDGE_CURVE ( 'NONE', #84360, #65090, #18575, .T. ) ;
#58929 = CARTESIAN_POINT ( 'NONE',  ( 194.8412596780180763, 266.4128482819364194, -7.732926466646180330 ) ) ;
#58930 = CARTESIAN_POINT ( 'NONE',  ( 202.6560281492536717, 279.6364581158209717, 17.15553667345918853 ) ) ;
#58931 = CARTESIAN_POINT ( 'NONE',  ( 162.6341128535665064, 248.9564488241690299, -10.63508949045170660 ) ) ;
#58932 = CARTESIAN_POINT ( 'NONE',  ( 15.03297158952216961, 188.6744531367911293, 4.594050593750047540 ) ) ;
#58933 = CARTESIAN_POINT ( 'NONE',  ( 150.8168331730346949, 269.4245776381016526, -15.71017957295074652 ) ) ;
#58934 = DIRECTION ( 'NONE',  ( -0.7080737730998298840, 0.7061384650677022812, 0.000000000000000000 ) ) ;
#58935 = CARTESIAN_POINT ( 'NONE',  ( 71.61432594831697429, 58.98614140521502236, -15.36087278562343705 ) ) ;
#58936 = CARTESIAN_POINT ( 'NONE',  ( 71.80545688294488116, 72.09185741349443788, -1.683858184180939466 ) ) ;
#58937 = CARTESIAN_POINT ( 'NONE',  ( 50.97302584657637681, 209.4244531367911577, -4.594050593750046652 ) ) ;
#58938 = CARTESIAN_POINT ( 'NONE',  ( 164.2090401137261892, 246.2285947913476889, -5.787448100099915393 ) ) ;
#58939 = CARTESIAN_POINT ( 'NONE',  ( 72.51713095402790543, 57.34819825014498917, 15.84120035366163748 ) ) ;
#58940 = CARTESIAN_POINT ( 'NONE',  ( 71.68417880216854599, 71.76513893551050671, 3.129347443225863667 ) ) ;
#58941 = CARTESIAN_POINT ( 'NONE',  ( 165.0387478276132072, 244.7914988754632191, -2.473354058663827626 ) ) ;
#58942 = EDGE_CURVE ( 'NONE', #4112, #44171, #6535, .T. ) ;
#58943 = ORIENTED_EDGE ( 'NONE', *, *, #15160, .T. ) ;
#58944 = CARTESIAN_POINT ( 'NONE',  ( 10.91961124514384274, 167.1115022471901739, -5.000000000000041744 ) ) ;
#58945 = LINE ( 'NONE', #28569, #4512 ) ;
#58946 = CARTESIAN_POINT ( 'NONE',  ( 131.4326323866306439, 240.5643266524160140, 9.188101187500095079 ) ) ;
#58947 = CARTESIAN_POINT ( 'NONE',  ( 31.56043161122053320, 21.14754757982091249, -5.678558825948276656 ) ) ;
#58948 = CARTESIAN_POINT ( 'NONE',  ( 206.9515461683482442, 272.1964026619218089, -8.225306050385031043 ) ) ;
#58949 = CARTESIAN_POINT ( 'NONE',  ( 188.6377010289637326, 260.8445305228526649, 6.834932301962454382 ) ) ;
#58950 = CYLINDRICAL_SURFACE ( 'NONE', #27113, 16.60714546451156792 ) ;
#58952 = CARTESIAN_POINT ( 'NONE',  ( 74.81608510805732237, 67.12708246140779522, 12.96692076351790313 ) ) ;
#58951 = CARTESIAN_POINT ( 'NONE',  ( 196.2048238403250764, 290.8102717488927169, 17.53926796892840656 ) ) ;
#58953 = CARTESIAN_POINT ( 'NONE',  ( 68.54233294502577678, 64.36627527950462024, 11.68987016893086661 ) ) ;
#58954 = EDGE_LOOP ( 'NONE', ( #26156, #747, #69244, #97412 ) ) ;
#58955 = CARTESIAN_POINT ( 'NONE',  ( 150.6533415055477008, 269.7077535128032082, 14.84621632544246062 ) ) ;
#58956 = CARTESIAN_POINT ( 'NONE',  ( 207.6123412471599181, 271.0518720120282978, -1.072722343106485843 ) ) ;
#58957 = CARTESIAN_POINT ( 'NONE',  ( 178.6423073663378602, 290.9544255387157818, 10.03153667033594765 ) ) ;
#58958 = CARTESIAN_POINT ( 'NONE',  ( 171.9228082726160096, 267.5004681726649096, -16.35366899046682221 ) ) ;
#58959 = CARTESIAN_POINT ( 'NONE',  ( 194.2019594945463723, 271.1902707947111253, -13.60880440021994531 ) ) ;
#58960 = EDGE_LOOP ( 'NONE', ( #45568, #58274, #42186, #95067 ) ) ;
#58961 = DIRECTION ( 'NONE',  ( 0.5000000000000003331, -0.8660254037844384856, 0.000000000000000000 ) ) ;
#58962 = CARTESIAN_POINT ( 'NONE',  ( 82.42550552036020406, 41.22741995948170057, -4.950294589197148376 ) ) ;
#58963 = EDGE_CURVE ( 'NONE', #81724, #35311, #59648, .T. ) ;
#58964 = ADVANCED_FACE ( 'NONE', ( #30762 ), #72247, .F. ) ;
#58965 = CARTESIAN_POINT ( 'NONE',  ( 71.85326037870230209, 72.57223462184859386, 1.067429543862054020 ) ) ;
#58966 = CARTESIAN_POINT ( 'NONE',  ( 85.61868005752367594, 45.39050660362939027, 8.416507326733476901 ) ) ;
#58967 = CARTESIAN_POINT ( 'NONE',  ( 196.2073114852891536, 270.9366426346837784, 12.15079365960697544 ) ) ;
#58968 = CARTESIAN_POINT ( 'NONE',  ( 181.9118032920808616, 295.3731262585166064, 4.899329891614067733 ) ) ;
#58969 = CARTESIAN_POINT ( 'NONE',  ( 69.52235898866341302, 70.68104077638899696, 1.790919661406474628 ) ) ;
#58970 = CARTESIAN_POINT ( 'NONE',  ( 150.8122822842734934, 278.1341709827950126, -0.0002939758904230073302 ) ) ;
#58971 = ADVANCED_FACE ( 'NONE', ( #38341 ), #61643, .F. ) ;
#58972 = B_SPLINE_CURVE_WITH_KNOTS ( 'NONE', 3,
 ( #30606, #45297, #14891, #60987 ),
 .UNSPECIFIED., .F., .F.,
 ( 4, 4 ),
 ( 0.009279588375480398582, 0.01508950711662758459 ),
 .UNSPECIFIED. ) ;
#58973 = CARTESIAN_POINT ( 'NONE',  ( 43.45144817956826699, 30.80170272979930601, 7.433330006724137462 ) ) ;
#58974 = CARTESIAN_POINT ( 'NONE',  ( 95.64807497750081211, 214.4824982072973683, 3.021315404115420679E-15 ) ) ;
#58975 = VERTEX_POINT ( 'NONE', #99672 ) ;
#58976 = LINE ( 'NONE', #21511, #30345 ) ;
#58977 = CARTESIAN_POINT ( 'NONE',  ( 86.19539083654223077, 46.94244887560866886, -10.58787169974291409 ) ) ;
#58978 = CARTESIAN_POINT ( 'NONE',  ( 159.0121568112382988, 263.7050002963263182, -17.11747536930247549 ) ) ;
#58979 = ORIENTED_EDGE ( 'NONE', *, *, #89920, .T. ) ;
#58981 = EDGE_CURVE ( 'NONE', #53400, #81007, #38207, .T. ) ;
#58980 = CARTESIAN_POINT ( 'NONE',  ( 191.1000148935602567, 299.6520602076213891, -9.462302242170249400 ) ) ;
#58982 = CARTESIAN_POINT ( 'NONE',  ( 184.8121857201937530, 292.0935771287341254, 12.40013839118309491 ) ) ;
#58983 = CARTESIAN_POINT ( 'NONE',  ( 164.4272222519600746, 245.8506922426221593, 7.021336339662529902 ) ) ;
#58984 = CARTESIAN_POINT ( 'NONE',  ( 160.9738207889920716, 284.1303138127853458, -2.465274816821101833 ) ) ;
#58985 = CARTESIAN_POINT ( 'NONE',  ( -22.42236680055709641, 157.8615022471902591, 0.000000000000000000 ) ) ;
#58986 = ORIENTED_EDGE ( 'NONE', *, *, #46022, .F. ) ;
#58987 = CARTESIAN_POINT ( 'NONE',  ( 86.64296780859545777, 211.6423013555409796, -4.594050593750043987 ) ) ;
#58988 = CARTESIAN_POINT ( 'NONE',  ( 155.2816187818737603, 261.6913421186901587, 18.56800597028529509 ) ) ;
#58989 = CARTESIAN_POINT ( 'NONE',  ( 181.1203783733027421, 271.7167412992034201, -16.96219288225206157 ) ) ;
#58990 = CARTESIAN_POINT ( 'NONE',  ( 184.6166050049803289, 259.6725624253173237, -5.813182908278067273 ) ) ;
#58991 = EDGE_CURVE ( 'NONE', #84837, #39540, #37841, .T. ) ;
#58992 = ORIENTED_EDGE ( 'NONE', *, *, #46941, .T. ) ;
#58993 = ORIENTED_EDGE ( 'NONE', *, *, #28974, .T. ) ;
#58994 = CARTESIAN_POINT ( 'NONE',  ( 88.40016726344319409, 43.81338102853380434, 0.1423130075416289830 ) ) ;
#58995 = ORIENTED_EDGE ( 'NONE', *, *, #41945, .T. ) ;
#58996 = CARTESIAN_POINT ( 'NONE',  ( 137.5794118583994532, 267.3524639162450853, 0.000000000000000000 ) ) ;
#58997 = AXIS2_PLACEMENT_3D ( 'NONE', #6716, #91852, #68506 ) ;
#58998 = ORIENTED_EDGE ( 'NONE', *, *, #64431, .T. ) ;
#58999 = CARTESIAN_POINT ( 'NONE',  ( 202.5128468779458331, 267.1751508879428343, 0.8823122286173835649 ) ) ;
#59000 = CARTESIAN_POINT ( 'NONE',  ( 155.6048174803203210, 261.1315455520403361, -17.38645169541727498 ) ) ;
#59001 = ORIENTED_EDGE ( 'NONE', *, *, #95434, .T. ) ;
#59002 = CARTESIAN_POINT ( 'NONE',  ( 164.9264240583707419, 244.9860493506886030, 2.333010560622383434 ) ) ;
#59003 = FACE_OUTER_BOUND ( 'NONE', #36917, .T. ) ;
#59004 = CARTESIAN_POINT ( 'NONE',  ( 28.46864935082048831, 149.7156766241961350, 21.50000000000008527 ) ) ;
#59005 = CARTESIAN_POINT ( 'NONE',  ( -23.58050215487121548, 99.69631501643195293, 45.19940618238346275 ) ) ;
#59006 = AXIS2_PLACEMENT_3D ( 'NONE', #93900, #25452, #80200 ) ;
#59007 = CARTESIAN_POINT ( 'NONE',  ( 74.05623475345210238, 67.87786276047000911, -11.59565021290446651 ) ) ;
#59008 = FACE_OUTER_BOUND ( 'NONE', #34585, .T. ) ;
#59009 = VERTEX_POINT ( 'NONE', #23138 ) ;
#59010 = LINE ( 'NONE', #89502, #57681 ) ;
#59011 = CARTESIAN_POINT ( 'NONE',  ( 3.501222095392049649, 22.99752408145588944, 5.678558825948277544 ) ) ;
#59012 = ORIENTED_EDGE ( 'NONE', *, *, #65872, .T. ) ;
#59013 = CARTESIAN_POINT ( 'NONE',  ( 166.8837065285814845, 246.9778330270648041, 3.492974035202267125 ) ) ;
#59014 = CARTESIAN_POINT ( 'NONE',  ( 199.9790510050489445, 270.1949291182149295, 9.285085457420754196 ) ) ;
#59015 = B_SPLINE_CURVE_WITH_KNOTS ( 'NONE', 3,
 ( #20576, #61031, #44840, #83392, #60532, #5367, #74789, #67654, #45342, #13475, #84387, #98074, #52948, #13961, #98585, #28652, #43349, #59534, #91485, #22048, #53436, #74297, #83897, #4880, #90514, #35762, #52447, #29168, #66658, #21086, #99563, #44346, #60036, #6847, #37733, #68642, #97589, #21564, #92003, #28160, #25041, #62022, #1255, #40227, #55918, #32137, #38223, #93485, #46322, #14933 ),
 .UNSPECIFIED., .F., .F.,
 ( 4, 2, 2, 2, 2, 2, 2, 2, 2, 2, 2, 2, 2, 2, 2, 2, 2, 2, 2, 2, 2, 2, 2, 2, 4 ),
 ( 0.0002342349665180101781, 0.001258123135262355667, 0.001770067219634560490, 0.002026039261820688272, 0.002154025282913752271, 0.002282011304006816271, 0.002409997325099880270, 0.002537983346192944269, 0.002793955388379072268, 0.003305899472751457503, 0.004329787641496161618, 0.005353675810240866167, 0.005865619894613221912, 0.006121591936799440983, 0.006377563978985659188, 0.006441556989532238459, 0.006505550000078817729, 0.006569543010625396133, 0.006633536021171974537, 0.006889508063358473766, 0.007401452147731471358, 0.007657424189917910740, 0.007913396232104349254, 0.008169368274290789503, 0.008425340316477228017 ),
 .UNSPECIFIED. ) ;
#59016 = CARTESIAN_POINT ( 'NONE',  ( -4.668846022976141263, 178.1115022471903160, -5.000000000000047962 ) ) ;
#59017 = CARTESIAN_POINT ( 'NONE',  ( 202.7041331321765938, 279.5531378413010657, 17.14708438049711248 ) ) ;
#59018 = CARTESIAN_POINT ( 'NONE',  ( 198.2505066714982149, 285.2670451491296149, 0.000000000000000000 ) ) ;
#59019 = CARTESIAN_POINT ( 'NONE',  ( 158.6703588719639697, 280.1886327639391538, -6.711918335171482397 ) ) ;
#59020 = CARTESIAN_POINT ( 'NONE',  ( 85.49318370521093868, 48.99722645306706426, -12.73116331006621316 ) ) ;
#59021 = CARTESIAN_POINT ( 'NONE',  ( 192.8135389063894820, 292.0478606184409500, -14.85096288738734671 ) ) ;
#59022 = CARTESIAN_POINT ( 'NONE',  ( 85.47549930518324857, 42.86882085676075604, 2.634943531499700509 ) ) ;
#59023 = CARTESIAN_POINT ( 'NONE',  ( 88.22236200735214595, 44.33456397151151407, -2.449239693650651972 ) ) ;
#59024 =( BOUNDED_CURVE ( )  B_SPLINE_CURVE ( 2, ( #17336, #1151, #148, #77138, #93888, #31527, #62418, #55321, #40121 ),
 .UNSPECIFIED., .F., .T. ) 
 B_SPLINE_CURVE_WITH_KNOTS ( ( 3, 2, 2, 2, 3 ),
 ( 0.1572580645161290314, 0.1586021505376344065, 0.1612903225806451568, 0.1639784946236559071, 0.1653225806451612823 ),
 .UNSPECIFIED. ) 
 CURVE ( )  GEOMETRIC_REPRESENTATION_ITEM ( )  RATIONAL_B_SPLINE_CURVE ( ( 0.9330127018922194093, 0.9330127018922194093, 1.000000000000000000, 0.8660254037844387076, 1.000000000000000000, 0.8660254037844387076, 1.000000000000000000, 0.9330127018922194093, 0.9330127018922194093 ) ) 
 REPRESENTATION_ITEM ( '' )  );
#59025 = ORIENTED_EDGE ( 'NONE', *, *, #24976, .F. ) ;
#59026 = CARTESIAN_POINT ( 'NONE',  ( 155.5450908721997791, 261.2349950718688660, -18.53705729126367530 ) ) ;
#59027 = CARTESIAN_POINT ( 'NONE',  ( 66.07564871127969752, 68.72588067980983340, 0.03328844042743933640 ) ) ;
#59028 = EDGE_LOOP ( 'NONE', ( #64497, #16200, #13581 ) ) ;
#59029 = CARTESIAN_POINT ( 'NONE',  ( 163.4341025207368716, 282.8476932499685859, 9.116081536633066307 ) ) ;
#59030 = DIRECTION ( 'NONE',  ( 0.9755587037855241173, -0.2197389712097240766, 0.000000000000000000 ) ) ;
#59031 = DIRECTION ( 'NONE',  ( 0.03004293549036790231, 0.9995486091367050685, 0.000000000000000000 ) ) ;
#59032 = CARTESIAN_POINT ( 'NONE',  ( 148.9230895364621574, 272.7046378331555161, 12.20434325797056019 ) ) ;
#59033 = CARTESIAN_POINT ( 'NONE',  ( 164.4537261901595286, 274.3242769609400398, 14.76238940331070815 ) ) ;
#59035 = CARTESIAN_POINT ( 'NONE',  ( 88.11819866784119881, 43.86870363832047559, 2.501606352371065878 ) ) ;
#59034 = DIRECTION ( 'NONE',  ( -0.8660254037844377084, -0.5000000000000014433, -0.000000000000000000 ) ) ;
#59037 = EDGE_CURVE ( 'NONE', #73274, #17687, #98184, .T. ) ;
#59036 = AXIS2_PLACEMENT_3D ( 'NONE', #29967, #15752, #39042 ) ;
#59038 = CARTESIAN_POINT ( 'NONE',  ( -22.42236680055709641, 157.8615022471902591, 0.000000000000000000 ) ) ;
#59039 = ORIENTED_EDGE ( 'NONE', *, *, #80791, .F. ) ;
#59040 = ORIENTED_EDGE ( 'NONE', *, *, #65121, .T. ) ;
#59041 = LINE ( 'NONE', #45351, #14512 ) ;
#59042 = CARTESIAN_POINT ( 'NONE',  ( 187.4955502139596888, 283.9325251962030734, -17.32086278988823125 ) ) ;
#59043 = ADVANCED_FACE ( 'NONE', ( #29761 ), #60634, .T. ) ;
#59044 = LINE ( 'NONE', #7225, #16021 ) ;
#59045 = CARTESIAN_POINT ( 'NONE',  ( 175.2000473418449360, 291.7498890306831072, 3.463214443597544268 ) ) ;
#59046 = CARTESIAN_POINT ( 'NONE',  ( -19.65312891409030271, 93.06504152958497400, -25.00000000000000000 ) ) ;
#59047 = CARTESIAN_POINT ( 'NONE',  ( -19.65312891409030271, 93.06504152958497400, 177.5919119679930134 ) ) ;
#59048 = CARTESIAN_POINT ( 'NONE',  ( 4.992923434102598534, 167.5643266524160140, -9.188101187500093303 ) ) ;
#59049 = CARTESIAN_POINT ( 'NONE',  ( 100.4447270377624477, 237.9869531367911293, 4.594050593750046652 ) ) ;
#59050 = CARTESIAN_POINT ( 'NONE',  ( 87.79556561918005286, 44.17086485108952587, -4.468589225908882412 ) ) ;
#59051 = CARTESIAN_POINT ( 'NONE',  ( 179.9270665230947657, 255.1929127066956937, -2.395391053091963762 ) ) ;
#59052 = EDGE_CURVE ( 'NONE', #13323, #98647, #80370, .T. ) ;
#59053 = CARTESIAN_POINT ( 'NONE',  ( 78.10701254639744207, 51.83640423345583059, 15.50559604832989002 ) ) ;
#59054 = CARTESIAN_POINT ( 'NONE',  ( 75.84078283921671471, 51.59066639860267145, 15.72938320682324154 ) ) ;
#59055 = CARTESIAN_POINT ( 'NONE',  ( 155.2695601165254402, 261.7122283397445131, 16.98599069618989077 ) ) ;
#59056 = CARTESIAN_POINT ( 'NONE',  ( 181.1390047055053287, 273.3328751412228144, 17.56653892176710130 ) ) ;
#59057 = CARTESIAN_POINT ( 'NONE',  ( 148.3625667886952044, 273.6754917110858401, -8.960758510948144462 ) ) ;
#59058 = EDGE_CURVE ( 'NONE', #71177, #39764, #14570, .T. ) ;
#59059 = CARTESIAN_POINT ( 'NONE',  ( 84.81065254960435595, 50.29073443720920977, 13.39702072830814394 ) ) ;
#59060 = CARTESIAN_POINT ( 'NONE',  ( 193.9296649147714788, 265.9040112472643500, 7.816750032855302344 ) ) ;
#59061 = DIRECTION ( 'NONE',  ( -0.000000000000000000, -0.000000000000000000, -1.000000000000000000 ) ) ;
#59062 = CARTESIAN_POINT ( 'NONE',  ( 58.31645990288170367, 211.1427522451419065, 10.00000000000009415 ) ) ;
#59063 = ADVANCED_FACE ( 'NONE', ( #13577 ), #28765, .F. ) ;
#59064 = VECTOR ( 'NONE', #34601, 1000.000000000000000 ) ;
#59065 = CARTESIAN_POINT ( 'NONE',  ( 42.77981749017101976, 207.0530062829863311, -4.648177544792955347E-16 ) ) ;
#59066 = DIRECTION ( 'NONE',  ( -0.8660254037844379305, -0.5000000000000014433, -0.000000000000000000 ) ) ;
#59067 = CARTESIAN_POINT ( 'NONE',  ( 81.01380268399661588, 208.3923013555409796, 4.594050593750050204 ) ) ;
#59068 = CARTESIAN_POINT ( 'NONE',  ( 161.8839333999304415, 250.2557977526613229, -13.90128376743482441 ) ) ;
#59069 =( GEOMETRIC_REPRESENTATION_CONTEXT ( 3 ) GLOBAL_UNCERTAINTY_ASSIGNED_CONTEXT ( ( #32145 ) ) GLOBAL_UNIT_ASSIGNED_CONTEXT ( ( #88338, #72606, #94414 ) ) REPRESENTATION_CONTEXT ( 'NONE', 'WORKASPACE' ) );
#59070 = CARTESIAN_POINT ( 'NONE',  ( 158.1254202985194581, 258.8215446263105832, -16.98779281373658989 ) ) ;
#59072 = CARTESIAN_POINT ( 'NONE',  ( 152.4345947225712621, 266.6225324397728400, 16.69537593800771091 ) ) ;
#59071 = CARTESIAN_POINT ( 'NONE',  ( 157.5710319558766344, 257.7259621817996162, 18.28704422422941533 ) ) ;
#59073 = DIRECTION ( 'NONE',  ( -0.000000000000000000, -0.000000000000000000, -1.000000000000000000 ) ) ;
#59074 = CARTESIAN_POINT ( 'NONE',  ( 75.69465226566293836, 65.43705427022661070, 14.28313312794709233 ) ) ;
#59075 = CARTESIAN_POINT ( 'NONE',  ( 173.1907548464488116, 268.0754673152154055, -16.28899667295896947 ) ) ;
#59076 = CARTESIAN_POINT ( 'NONE',  ( 40.03666203415436797, 35.06628583063844928, -9.188101187500006262 ) ) ;
#59077 = CARTESIAN_POINT ( 'NONE',  ( 147.2089949622447875, 275.6735367246781720, -3.633014386235353221 ) ) ;
#59078 = DIRECTION ( 'NONE',  ( -0.8660254037844387076, -0.4999999999999998890, -0.000000000000000000 ) ) ;
#59079 = ORIENTED_EDGE ( 'NONE', *, *, #37699, .F. ) ;
#59080 = CARTESIAN_POINT ( 'NONE',  ( 18.45699304436188015, 28.84336893147756342, -7.433330006724137462 ) ) ;
#59081 = CARTESIAN_POINT ( 'NONE',  ( 10.15257209397493199, 21.56454794089039950, 10.00000000000000355 ) ) ;
#59082 = CARTESIAN_POINT ( 'NONE',  ( 147.0456760057551833, 275.9564134551570760, -3.678503029046952033 ) ) ;
#59083 = CARTESIAN_POINT ( 'NONE',  ( 188.4945086955212901, 286.1460090028926402, -16.09362256013984194 ) ) ;
#59084 = EDGE_CURVE ( 'NONE', #87476, #57035, #47609, .T. ) ;
#59085 = ORIENTED_EDGE ( 'NONE', *, *, #54298, .F. ) ;
#59086 = CARTESIAN_POINT ( 'NONE',  ( 70.42963173116773135, 60.96378554420563489, 14.42110835124151080 ) ) ;
#59087 = CARTESIAN_POINT ( 'NONE',  ( 75.88031102442633369, 65.78928292664191702, -14.15509851726639390 ) ) ;
#59088 = CARTESIAN_POINT ( 'NONE',  ( 153.9489233572929834, 266.9981809298170106, 16.25793775942264219 ) ) ;
#59089 = CARTESIAN_POINT ( 'NONE',  ( 44.44844410339183582, 68.22168590943847732, -10.00000000000000000 ) ) ;
#59090 = CARTESIAN_POINT ( 'NONE',  ( 146.0195742355162452, 245.1115022471902023, -5.000000000000041744 ) ) ;
#59091 = CARTESIAN_POINT ( 'NONE',  ( 204.6149525604204769, 276.2435015074934199, -13.22810747389629960 ) ) ;
#59092 = EDGE_CURVE ( 'NONE', #36246, #31869, #5910, .T. ) ;
#59093 = VERTEX_POINT ( 'NONE', #47936 ) ;
#59094 = CARTESIAN_POINT ( 'NONE',  ( 88.62734903533704767, 228.6427522451418781, -10.00000000000009592 ) ) ;
#59095 = ORIENTED_EDGE ( 'NONE', *, *, #37040, .F. ) ;
#59096 = CARTESIAN_POINT ( 'NONE',  ( -21.58168810074490551, 24.33735145887882112, -10.00000000000000000 ) ) ;
#59097 = CARTESIAN_POINT ( 'NONE',  ( 86.98912267288208966, 45.08269913945084539, 6.733204870563289646 ) ) ;
#59099 = EDGE_CURVE ( 'NONE', #36590, #32767, #32249, .T. ) ;
#59098 = CARTESIAN_POINT ( 'NONE',  ( -50.14960082266475894, 51.27834073637188084, 59.99999999999999289 ) ) ;
#59100 = VERTEX_POINT ( 'NONE', #55040 ) ;
#59102 = EDGE_CURVE ( 'NONE', #72875, #91554, #95104, .T. ) ;
#59101 = CARTESIAN_POINT ( 'NONE',  ( 88.42017002704760387, 43.92753743058676008, 1.721442031696316599 ) ) ;
#59103 = CARTESIAN_POINT ( 'NONE',  ( 206.0686240106620915, 273.7256686981625080, 10.79590858600826309 ) ) ;
#59104 = CARTESIAN_POINT ( 'NONE',  ( 158.7005503356804752, 257.5255643194142863, -17.18125617848118480 ) ) ;
#59105 = CARTESIAN_POINT ( 'NONE',  ( 153.7116827962181560, 264.4105510104763539, -18.11656053488752605 ) ) ;
#59106 = CARTESIAN_POINT ( 'NONE',  ( 153.3544108199959908, 265.0293642254135307, -17.49105661178601423 ) ) ;
#59107 = VECTOR ( 'NONE', #59268, 1000.000000000000000 ) ;
#59108 = ADVANCED_FACE ( 'NONE', ( #24646 ), #62632, .F. ) ;
#59109 = CARTESIAN_POINT ( 'NONE',  ( 40.64525884627276042, 24.26216523072497466, -2.296566073217252530E-15 ) ) ;
#59110 = DIRECTION ( 'NONE',  ( -0.000000000000000000, -0.000000000000000000, 1.000000000000000000 ) ) ;
#59111 = CARTESIAN_POINT ( 'NONE',  ( 166.1866365242245536, 275.3519730907532335, 14.78294132260052152 ) ) ;
#59112 = CARTESIAN_POINT ( 'NONE',  ( 87.32503761238780271, 45.47676291781615276, 7.117495199483119706 ) ) ;
#59113 = ORIENTED_EDGE ( 'NONE', *, *, #24417, .F. ) ;
#59114 = EDGE_LOOP ( 'NONE', ( #19490, #32698, #99271, #82093 ) ) ;
#59115 = DIRECTION ( 'NONE',  ( 0.4525327339300069251, -0.8917477921037054722, 0.000000000000000000 ) ) ;
#59117 = CARTESIAN_POINT ( 'NONE',  ( 194.2900850603946310, 294.1266965989547657, -15.88613936555681505 ) ) ;
#59116 = CARTESIAN_POINT ( 'NONE',  ( -27.42236680055714260, 166.5217562850347406, 1.224646799147364892E-15 ) ) ;
#59118 = CARTESIAN_POINT ( 'NONE',  ( 85.37538261767947745, 48.57005942898851458, 12.46403972397472337 ) ) ;
#59119 = CARTESIAN_POINT ( 'NONE',  ( 66.25468035962502711, 68.66496212375022878, -2.132244879849610975 ) ) ;
#59120 = PLANE ( 'NONE',  #46378 ) ;
#59121 = CARTESIAN_POINT ( 'NONE',  ( 82.39721099679231031, 40.42262220688863295, 1.474573639680701431 ) ) ;
#59122 = CARTESIAN_POINT ( 'NONE',  ( 167.7492589498101268, 287.2853069970565230, -4.990612205622849906 ) ) ;
#59123 = CARTESIAN_POINT ( 'NONE',  ( 167.0261895629188302, 265.8937476829661364, 16.54818857680643163 ) ) ;
#59124 = CARTESIAN_POINT ( 'NONE',  ( 181.3894115369784572, 256.9812711509448491, 4.984939519295573440 ) ) ;
#59125 = CARTESIAN_POINT ( 'NONE',  ( 89.61940949045693117, 231.7369531367911009, -4.594050593750048428 ) ) ;
#59126 = ORIENTED_EDGE ( 'NONE', *, *, #62355, .F. ) ;
#59127 = CARTESIAN_POINT ( 'NONE',  ( 148.2529106943155455, 274.6458799743566033, -6.824415188474639571 ) ) ;
#59128 = CARTESIAN_POINT ( 'NONE',  ( 189.7493380202622291, 294.8126471784881915, -12.68491631734921299 ) ) ;
#59129 = CARTESIAN_POINT ( 'NONE',  ( 166.7606291933738021, 278.4628371803321443, -13.23787148276527681 ) ) ;
#59130 = VERTEX_POINT ( 'NONE', #40334 ) ;
#59131 = VECTOR ( 'NONE', #57977, 1000.000000000000000 ) ;
#59132 = ORIENTED_EDGE ( 'NONE', *, *, #78233, .T. ) ;
#59133 = CARTESIAN_POINT ( 'NONE',  ( 87.08635211577573898, 45.98159987514826241, -8.162078895322940397 ) ) ;
#59134 = CARTESIAN_POINT ( 'NONE',  ( 178.0175832155955220, 292.6799449813070169, -2.666636303287813092 ) ) ;
#59135 = CARTESIAN_POINT ( 'NONE',  ( 157.0848929289108469, 258.5679796760466047, 17.57466231005294688 ) ) ;
#59136 = CARTESIAN_POINT ( 'NONE',  ( 175.0125019719911847, 292.0719086349095051, 3.303583340955516423 ) ) ;
#59137 = CARTESIAN_POINT ( 'NONE',  ( -39.52511050156713424, 25.94496742513404541, 10.00000000000000000 ) ) ;
#59138 = ORIENTED_EDGE ( 'NONE', *, *, #27206, .T. ) ;
#59139 = AXIS2_PLACEMENT_3D ( 'NONE', #32816, #16121, #94159 ) ;
#59140 = ORIENTED_EDGE ( 'NONE', *, *, #39324, .F. ) ;
#59141 = CARTESIAN_POINT ( 'NONE',  ( 208.3764315856425640, 269.7284287242038658, -1.833640725398759441 ) ) ;
#59142 = ORIENTED_EDGE ( 'NONE', *, *, #51901, .T. ) ;
#59143 = ADVANCED_FACE ( 'NONE', ( #58475 ), #20924, .F. ) ;
#59144 = CARTESIAN_POINT ( 'NONE',  ( 191.7288270367013467, 263.6483701492742284, -8.196354403749188222 ) ) ;
#59145 = CARTESIAN_POINT ( 'NONE',  ( -22.42236680055709641, 157.8615022471902591, 0.000000000000000000 ) ) ;
#59146 = CARTESIAN_POINT ( 'NONE',  ( 84.05646506986525424, 49.99712786259807729, 13.48608966145228649 ) ) ;
#59148 = CARTESIAN_POINT ( 'NONE',  ( 69.42588139327764907, 62.69554889617239013, -13.80398409906540280 ) ) ;
#59147 = CARTESIAN_POINT ( 'NONE',  ( 133.7867050834633460, 257.2369531367911009, -4.594050593750048428 ) ) ;
#59149 = DIRECTION ( 'NONE',  ( -0.8660254037844387076, -0.4999999999999998890, -0.000000000000000000 ) ) ;
#59150 = ORIENTED_EDGE ( 'NONE', *, *, #91521, .F. ) ;
#59151 = B_SPLINE_CURVE_WITH_KNOTS ( 'NONE', 3,
 ( #39805, #86007, #9955, #86501, #47430, #78357, #32234, #338, #94080, #63135, #24633, #32733, #78861, #40814, #71761, #31229, #62115, #55513 ),
 .UNSPECIFIED., .F., .F.,
 ( 4, 2, 2, 2, 2, 2, 2, 2, 4 ),
 ( 0.003355772174813248000, 0.003464747999639208008, 0.003573723824465168016, 0.003682699649291128023, 0.003791675474117088031, 0.004009627123769074833, 0.004227578773421060768, 0.005099385372029013180, 0.006842998569244833004 ),
 .UNSPECIFIED. ) ;
#59152 = DIRECTION ( 'NONE',  ( 0.8660254037844382635, 0.5000000000000005551, 0.000000000000000000 ) ) ;
#59153 = CARTESIAN_POINT ( 'NONE',  ( 82.12032703770964304, 50.14001162089422081, 14.08521554294405931 ) ) ;
#59154 = CARTESIAN_POINT ( 'NONE',  ( 82.05174726562462695, 41.11851925668477747, -3.408449855420926156 ) ) ;
#59155 = CARTESIAN_POINT ( 'NONE',  ( 192.7653315510534924, 271.1824743346560922, 14.22424966267575819 ) ) ;
#59156 = CARTESIAN_POINT ( 'NONE',  ( 167.1866462610758788, 284.4963469294596621, 9.835208695640710985 ) ) ;
#59157 = CARTESIAN_POINT ( 'NONE',  ( 72.12859001842100781, 72.20979474176914437, 3.988024951247647110 ) ) ;
#59158 = CARTESIAN_POINT ( 'NONE',  ( 82.16472207147782569, 40.63388750005248085, -3.462830440365086027 ) ) ;
#59159 = CARTESIAN_POINT ( 'NONE',  ( 136.3105610988903607, 261.0530062829863027, -4.648177544792955347E-16 ) ) ;
#59160 = CARTESIAN_POINT ( 'NONE',  ( 183.3811779399601960, 287.6651436968118674, 15.08102091061752859 ) ) ;
#59161 = DIRECTION ( 'NONE',  ( 0.2398044646550112069, 0.9708212084269294273, 0.000000000000000000 ) ) ;
#59162 = CARTESIAN_POINT ( 'NONE',  ( 70.72975101405640430, 202.4548013555409796, -4.594050593750042211 ) ) ;
#59163 = CARTESIAN_POINT ( 'NONE',  ( 74.93017357788674815, 189.2419560658248940, 5.188172501216619860E-14 ) ) ;
#59164 = CARTESIAN_POINT ( 'NONE',  ( 0.4893710859096792598, 78.77562236714182120, 59.99999999999999289 ) ) ;
#59165 = CARTESIAN_POINT ( 'NONE',  ( 162.6341128535665064, 248.9564488241690299, -10.63508949045170660 ) ) ;
#59166 = EDGE_CURVE ( 'NONE', #45437, #78482, #63149, .T. ) ;
#59167 = VECTOR ( 'NONE', #84996, 1000.000000000000000 ) ;
#59168 = LINE ( 'NONE', #68786, #6056 ) ;
#59169 = CARTESIAN_POINT ( 'NONE',  ( -20.82151326869808017, 95.08966588713798274, 45.19948828869558355 ) ) ;
#59170 = CARTESIAN_POINT ( 'NONE',  ( 72.02976470237955198, 59.30830629416842470, -15.33705471575644808 ) ) ;
#59171 = EDGE_CURVE ( 'NONE', #93728, #2250, #14766, .T. ) ;
#59172 = CARTESIAN_POINT ( 'NONE',  ( 40.17197850526964942, 35.14441083166263979, 10.00000000000000533 ) ) ;
#59173 = B_SPLINE_CURVE_WITH_KNOTS ( 'NONE', 3,
 ( #49653, #28345, #58249, #36439 ),
 .UNSPECIFIED., .F., .F.,
 ( 4, 4 ),
 ( 0.004312638717203288660, 0.01230371896665270748 ),
 .UNSPECIFIED. ) ;
#59174 = DIRECTION ( 'NONE',  ( -0.2113248654052096720, -0.7886751345948050940, -0.5773502691896282846 ) ) ;
#59175 = CARTESIAN_POINT ( 'NONE',  ( 82.48682597242610370, 54.22050469884690216, 15.58985929802052617 ) ) ;
#59176 = CIRCLE ( 'NONE', #15510, 70.00000000000001421 ) ;
#59177 = DIRECTION ( 'NONE',  ( -0.8660254037844378194, -0.5000000000000014433, -0.000000000000000000 ) ) ;
#59178 = ADVANCED_FACE ( 'NONE', ( #35248 ), #49449, .T. ) ;
#59179 = CARTESIAN_POINT ( 'NONE',  ( 9.403806464923315289, 185.4244531367911293, -4.594050593750046652 ) ) ;
#59180 = CARTESIAN_POINT ( 'NONE',  ( 70.45698661661860740, 71.51623517888778281, 2.879531975083107653 ) ) ;
#59181 = ORIENTED_EDGE ( 'NONE', *, *, #33966, .F. ) ;
#59182 = CARTESIAN_POINT ( 'NONE',  ( 157.8849654228661166, 257.1822134667773980, 17.43614750057631468 ) ) ;
#59183 = CARTESIAN_POINT ( 'NONE',  ( 199.2604132571903790, 277.9333477773519121, 15.74201777144865844 ) ) ;
#59184 = CARTESIAN_POINT ( 'NONE',  ( 28.65277809448527080, 198.8967562850347122, -4.648177544792955347E-16 ) ) ;
#59185 = CARTESIAN_POINT ( 'NONE',  ( 208.3057440179679531, 269.8508631828800617, 2.969924427282375046 ) ) ;
#59186 = DIRECTION ( 'NONE',  ( 1.000000000000000000, -1.784287003861858500E-15, 0.000000000000000000 ) ) ;
#59187 = CARTESIAN_POINT ( 'NONE',  ( 57.30635725539759306, 194.7048013555409796, 4.594050593750051981 ) ) ;
#59188 = CARTESIAN_POINT ( 'NONE',  ( 161.8948331661419218, 250.2369188037922356, 13.64419044796309777 ) ) ;
#59189 = CARTESIAN_POINT ( 'NONE',  ( 198.9832789858017463, 285.9978462703757600, -18.55676541969546278 ) ) ;
#59190 = CARTESIAN_POINT ( 'NONE',  ( 190.8683709797118411, 300.0532792356709706, -4.461919767133968762 ) ) ;
#59191 = CARTESIAN_POINT ( 'NONE',  ( 36.79557518129325899, 43.01751292744061317, 6.180339887498949913 ) ) ;
#59192 = CARTESIAN_POINT ( 'NONE',  ( 159.8822213732012756, 255.7228646850775533, -16.63148941946954196 ) ) ;
#59193 = CARTESIAN_POINT ( 'NONE',  ( 177.6444986370304946, 293.6980009803469329, 2.770296639708824227 ) ) ;
#59194 = VECTOR ( 'NONE', #67798, 1000.000000000000000 ) ;
#59195 = ORIENTED_EDGE ( 'NONE', *, *, #30736, .T. ) ;
#59196 = CARTESIAN_POINT ( 'NONE',  ( 72.97333888298118154, 62.81283549581255699, 14.28620849118072833 ) ) ;
#59197 = CARTESIAN_POINT ( 'NONE',  ( 75.06695094285400671, 67.05599132900850634, -12.66018568268392208 ) ) ;
#59198 = AXIS2_PLACEMENT_3D ( 'NONE', #903, #62684, #71319 ) ;
#59199 = CARTESIAN_POINT ( 'NONE',  ( -74.22192597045216189, 49.22161114575668250, 177.5919119679930134 ) ) ;
#59200 = CARTESIAN_POINT ( 'NONE',  ( 97.08913892169542237, 236.8615022471903160, 5.000000000000046185 ) ) ;
#59201 = PLANE ( 'NONE',  #68480 ) ;
#59202 = EDGE_CURVE ( 'NONE', #1860, #71477, #43337, .T. ) ;
#59203 = CARTESIAN_POINT ( 'NONE',  ( 164.9009427471078766, 270.4319544559331234, -17.40525121274953335 ) ) ;
#59204 = EDGE_LOOP ( 'NONE', ( #85256, #13040, #3355, #40493 ) ) ;
#59205 = CARTESIAN_POINT ( 'NONE',  ( 67.69866210081085001, 200.7048013555409796, 4.594050593750051981 ) ) ;
#59206 = VERTEX_POINT ( 'NONE', #50942 ) ;
#59207 = CARTESIAN_POINT ( 'NONE',  ( 166.3615356672940777, 265.0576312756302286, 16.62332830971679698 ) ) ;
#59208 = CARTESIAN_POINT ( 'NONE',  ( 147.5492216329511166, 275.0842468449245644, 4.751613690710122739 ) ) ;
#59209 = CARTESIAN_POINT ( 'NONE',  ( 173.5247214620460738, 266.5572136672606689, 17.40638611211905484 ) ) ;
#59210 = ORIENTED_EDGE ( 'NONE', *, *, #31427, .T. ) ;
#59211 = LINE ( 'NONE', #90186, #44102 ) ;
#59213 = EDGE_CURVE ( 'NONE', #58260, #10169, #80403, .T. ) ;
#59212 = CARTESIAN_POINT ( 'NONE',  ( 207.6508796976096107, 270.9851214578045528, 6.713685698622268383 ) ) ;
#59214 = CARTESIAN_POINT ( 'NONE',  ( 71.63103492117564031, 72.07843208848032646, 3.395715836721231895 ) ) ;
#59215 = CARTESIAN_POINT ( 'NONE',  ( 28.76090768559789979, 38.64646525600391413, -2.839279412974133887 ) ) ;
#59216 = CARTESIAN_POINT ( 'NONE',  ( 189.7373781100581027, 264.4670991245342293, 10.92349686411582788 ) ) ;
#59217 = CARTESIAN_POINT ( 'NONE',  ( 149.2923684163597784, 272.0650280510108701, -12.99082738998495756 ) ) ;
#59218 = CARTESIAN_POINT ( 'NONE',  ( 204.3646970165318351, 276.6769568243839217, 14.33703115251539018 ) ) ;
#59219 = ORIENTED_EDGE ( 'NONE', *, *, #56574, .F. ) ;
#59220 = CARTESIAN_POINT ( 'NONE',  ( 23.79748941506785798, 22.24335787977763346, -9.188101187500008038 ) ) ;
#59221 = DIRECTION ( 'NONE',  ( -0.000000000000000000, -0.000000000000000000, -1.000000000000000000 ) ) ;
#59222 = CARTESIAN_POINT ( 'NONE',  ( 174.9566398689986499, 255.1230660018185574, 8.075064970304348222 ) ) ;
#59223 = CARTESIAN_POINT ( 'NONE',  ( -63.34358462235559273, 38.37368864812747660, 10.00000000000000000 ) ) ;
#59224 = EDGE_CURVE ( 'NONE', #15171, #92056, #2865, .T. ) ;
#59225 = ORIENTED_EDGE ( 'NONE', *, *, #38751, .F. ) ;
#59226 = CARTESIAN_POINT ( 'NONE',  ( 182.1243482512361709, 283.9946157055692879, 14.95652526196643883 ) ) ;
#59227 = CARTESIAN_POINT ( 'NONE',  ( 191.2729698983822288, 299.3524933518466469, 8.871011392605806734 ) ) ;
#59228 = CARTESIAN_POINT ( 'NONE',  ( 159.5221561062548972, 254.3465160214695118, -16.91023001054109542 ) ) ;
#59229 = ORIENTED_EDGE ( 'NONE', *, *, #58981, .T. ) ;
#59230 = ORIENTED_EDGE ( 'NONE', *, *, #91802, .T. ) ;
#59232 = CARTESIAN_POINT ( 'NONE',  ( -110.0000000000000000, 10.00000000000000000, 59.99999999999999289 ) ) ;
#59231 = CARTESIAN_POINT ( 'NONE',  ( 161.4816992964961742, 250.9524876563463067, -12.92750327687364198 ) ) ;
#59233 = CARTESIAN_POINT ( 'NONE',  ( 196.7130436017243653, 289.9300093007386749, -16.33278734947153765 ) ) ;
#59234 = ORIENTED_EDGE ( 'NONE', *, *, #64057, .F. ) ;
#59235 = CYLINDRICAL_SURFACE ( 'NONE', #35293, 70.00000000000002842 ) ;
#59236 = FACE_OUTER_BOUND ( 'NONE', #8674, .T. ) ;
#59237 = DIRECTION ( 'NONE',  ( -0.4999999999999987788, 0.8660254037844392627, 0.000000000000000000 ) ) ;
#59238 = CARTESIAN_POINT ( 'NONE',  ( 161.4611533925282458, 263.2350952187405255, -17.14425122640257726 ) ) ;
#59239 = CARTESIAN_POINT ( 'NONE',  ( 123.3675972660055749, 242.0333772461660544, 9.188101187500095079 ) ) ;
#59240 = CARTESIAN_POINT ( 'NONE',  ( 190.8623743139412454, 300.0636657654615647, 8.577953960666059530 ) ) ;
#59241 = ORIENTED_EDGE ( 'NONE', *, *, #30973, .F. ) ;
#59242 = CARTESIAN_POINT ( 'NONE',  ( 170.5590276664972862, 263.8138381775597736, 15.82950496912112470 ) ) ;
#59243 = CARTESIAN_POINT ( 'NONE',  ( 28.87159617421078295, 194.1427522451419350, -10.00000000000009592 ) ) ;
#59244 = AXIS2_PLACEMENT_3D ( 'NONE', #81778, #95994, #66042 ) ;
#59245 = EDGE_LOOP ( 'NONE', ( #4204, #52015, #45798, #42935 ) ) ;
#59246 = LINE ( 'NONE', #22268, #96374 ) ;
#59247 = AXIS2_PLACEMENT_3D ( 'NONE', #13343, #20954, #44207 ) ;
#59248 = ORIENTED_EDGE ( 'NONE', *, *, #16462, .T. ) ;
#59249 = VERTEX_POINT ( 'NONE', #72793 ) ;
#59250 = CARTESIAN_POINT ( 'NONE',  ( 198.6012358295098750, 286.6595644277572887, 18.21911298807435386 ) ) ;
#59251 = DIRECTION ( 'NONE',  ( 0.000000000000000000, 0.000000000000000000, 1.000000000000000000 ) ) ;
#59252 = CARTESIAN_POINT ( 'NONE',  ( 85.15457341978220995, 207.7202760586659167, -5.415160957724236172E-17 ) ) ;
#59253 = CARTESIAN_POINT ( 'NONE',  ( 173.8612121445452203, 290.1417140779839201, 6.947705100246971632 ) ) ;
#59254 = CARTESIAN_POINT ( 'NONE',  ( 81.68759648889933089, 55.58869686435339474, 15.96161034574012838 ) ) ;
#59255 = CARTESIAN_POINT ( 'NONE',  ( 198.1857676047573307, 287.3791765019590798, 18.47549341984830562 ) ) ;
#59256 = AXIS2_PLACEMENT_3D ( 'NONE', #67759, #37836, #37341 ) ;
#59257 = CARTESIAN_POINT ( 'NONE',  ( 171.9727612249948550, 276.6547058738756277, 16.01864781142220195 ) ) ;
#59258 = ORIENTED_EDGE ( 'NONE', *, *, #38471, .F. ) ;
#59259 = EDGE_CURVE ( 'NONE', #72252, #50208, #41310, .T. ) ;
#59260 = CARTESIAN_POINT ( 'NONE',  ( 71.31394413970843971, 63.96069529197309578, -13.14444410564831500 ) ) ;
#59261 = CARTESIAN_POINT ( 'NONE',  ( 201.4214977800931763, 281.7747274386935601, -17.04225209925078133 ) ) ;
#59262 = CARTESIAN_POINT ( 'NONE',  ( 87.87434464428623926, 43.89907206790573468, 3.349129858248744540 ) ) ;
#59263 = ORIENTED_EDGE ( 'NONE', *, *, #78367, .T. ) ;
#59264 = CARTESIAN_POINT ( 'NONE',  ( 73.51948839908328637, 69.73627507762921596, -9.361350578256052657 ) ) ;
#59265 = EDGE_CURVE ( 'NONE', #40206, #13906, #64123, .T. ) ;
#59266 = CARTESIAN_POINT ( 'NONE',  ( 76.08252525470864214, 51.16590352028240574, -16.09814970804995582 ) ) ;
#59267 = DIRECTION ( 'NONE',  ( -0.000000000000000000, -0.000000000000000000, -1.000000000000000000 ) ) ;
#59268 = DIRECTION ( 'NONE',  ( 0.000000000000000000, -0.000000000000000000, 1.000000000000000000 ) ) ;
#59269 = CARTESIAN_POINT ( 'NONE',  ( 206.4537138826727301, 273.0586734743599209, 11.45643784582899016 ) ) ;
#59270 = DIRECTION ( 'NONE',  ( -1.000000000000000000, 0.000000000000000000, 0.000000000000000000 ) ) ;
#59271 = ORIENTED_EDGE ( 'NONE', *, *, #56085, .F. ) ;
#59272 = CARTESIAN_POINT ( 'NONE',  ( 9.911560002841389050, 164.9824982072973967, 3.021315404115420679E-15 ) ) ;
#59273 = CARTESIAN_POINT ( 'NONE',  ( 143.8006444583684242, 244.6423013555409796, -4.594050593750043987 ) ) ;
#59274 = VERTEX_POINT ( 'NONE', #20564 ) ;
#59275 = VECTOR ( 'NONE', #13498, 1000.000000000000227 ) ;
#59276 = CARTESIAN_POINT ( 'NONE',  ( -3.369807917299440181, 168.8615022471902591, -10.00000000000009592 ) ) ;
#59277 = CARTESIAN_POINT ( 'NONE',  ( 67.94904719768317136, 67.86889835017325368, -8.208080553877501018 ) ) ;
#59278 = CARTESIAN_POINT ( 'NONE',  ( 155.6308784268266265, 261.7459045956564978, -16.98888936756683066 ) ) ;
#59279 = CONICAL_SURFACE ( 'NONE', #2709, 16.82106496071143908, 0.7853981633974241872 ) ;
#59280 = CARTESIAN_POINT ( 'NONE',  ( 204.4325665793906524, 276.5594032932251594, 13.33817701435311598 ) ) ;
#59281 = CARTESIAN_POINT ( 'NONE',  ( -19.65312891409030271, 93.06504152958497400, 10.00000000000000888 ) ) ;
#59282 = DIRECTION ( 'NONE',  ( -1.000000000000000000, 0.000000000000000000, 0.000000000000000000 ) ) ;
#59283 = VERTEX_POINT ( 'NONE', #2883 ) ;
#59284 = CARTESIAN_POINT ( 'NONE',  ( 76.46051236311743082, 54.44209003778230738, 16.09620867652457576 ) ) ;
#59285 = CARTESIAN_POINT ( 'NONE',  ( 182.3579730533000998, 275.1687724611243766, -17.70355169473433676 ) ) ;
#59286 = CARTESIAN_POINT ( 'NONE',  ( 72.48631355412707933, 71.22806908010377924, -6.072071567456138297 ) ) ;
#59287 = CARTESIAN_POINT ( 'NONE',  ( 205.9447606851647947, 273.9402062711180861, -10.75123264850128102 ) ) ;
#59288 = CARTESIAN_POINT ( 'NONE',  ( 200.9728293662470833, 267.3697413902040125, 0.8356558750402847124 ) ) ;
#59289 = CARTESIAN_POINT ( 'NONE',  ( 190.2287563641723978, 301.1611242470490311, -4.521471513871881953 ) ) ;
#59290 = CARTESIAN_POINT ( 'NONE',  ( 182.8870023055169156, 280.6774797787840612, 16.96697556416149411 ) ) ;
#59291 = CARTESIAN_POINT ( 'NONE',  ( 157.0887340267001946, 258.5613266995183039, -17.61824281915036394 ) ) ;
#59292 = CARTESIAN_POINT ( 'NONE',  ( 196.3186127241907570, 270.7072474025165434, 11.90743844834340059 ) ) ;
#59293 = EDGE_CURVE ( 'NONE', #57780, #80596, #74006, .T. ) ;
#59294 = CARTESIAN_POINT ( 'NONE',  ( 16.60635795911645829, 31.36126292948894445, 6.180339887498949913 ) ) ;
#59295 = CARTESIAN_POINT ( 'NONE',  ( 149.7166446726674565, 271.3301600186404698, 12.26048591517335495 ) ) ;
#59296 = CARTESIAN_POINT ( 'NONE',  ( 82.06776773193392671, 41.79991662876560099, 5.443441096911677768 ) ) ;
#59297 = PLANE ( 'NONE',  #59583 ) ;
#59298 = CARTESIAN_POINT ( 'NONE',  ( 197.9002057575219453, 287.8737841300738296, 18.01270164875645818 ) ) ;
#59299 = ADVANCED_FACE ( 'NONE', ( #75761 ), #43837, .F. ) ;
#59300 = CARTESIAN_POINT ( 'NONE',  ( 207.1811000426777980, 271.7988036885084853, 5.430390748498256315 ) ) ;
#59301 = CARTESIAN_POINT ( 'NONE',  ( 132.7946446283434341, 254.1427522451419065, -10.00000000000009415 ) ) ;
#59302 = EDGE_CURVE ( 'NONE', #29626, #68532, #36235, .T. ) ;
#59303 = CARTESIAN_POINT ( 'NONE',  ( 172.2205269341238250, 283.6848208328027567, -12.54202715120148959 ) ) ;
#59304 = ORIENTED_EDGE ( 'NONE', *, *, #20347, .T. ) ;
#59305 = ADVANCED_FACE ( 'NONE', ( #38209 ), #50557, .F. ) ;
#59306 = B_SPLINE_CURVE_WITH_KNOTS ( 'NONE', 3,
 ( #24179, #25169, #8974, #39352, #48484, #54548, #30785, #61666, #56051, #31754, #55061, #46976, #100200, #7989, #9488, #16572 ),
 .UNSPECIFIED., .F., .F.,
 ( 4, 2, 2, 2, 2, 2, 2, 4 ),
 ( 0.000000000000000000, 0.0003786681000627616523, 0.0007573362001255233046, 0.001136004300188284740, 0.001514672400251046609, 0.001893340500313808262, 0.002272008600376569480, 0.003029344800502104494 ),
 .UNSPECIFIED. ) ;
#59307 = CARTESIAN_POINT ( 'NONE',  ( 39.00599428327696216, 91.66936899913777381, 59.99999999999999289 ) ) ;
#59308 = CARTESIAN_POINT ( 'NONE',  ( 198.4427928769277969, 286.9339956717308837, -17.97122743692687763 ) ) ;
#59309 = CARTESIAN_POINT ( 'NONE',  ( 6.887527552763561545, 162.5327760586659736, 1.948934522072302763E-15 ) ) ;
#59310 = CIRCLE ( 'NONE', #15652, 0.1418229129681591871 ) ;
#59311 = CARTESIAN_POINT ( 'NONE',  ( 178.4620001282691248, 259.0559472856667185, -10.32065242460678789 ) ) ;
#59312 = CARTESIAN_POINT ( 'NONE',  ( 23.82048379914786906, 32.49103043416550207, -8.090169943749479842 ) ) ;
#59313 = CARTESIAN_POINT ( 'NONE',  ( 85.11013511109823071, 48.98411268001765251, 12.43910323488882241 ) ) ;
#59314 = CARTESIAN_POINT ( 'NONE',  ( 204.7519188734507622, 276.0062688943993408, -12.76027478560537531 ) ) ;
#59315 = CARTESIAN_POINT ( 'NONE',  ( 71.89533859728123844, 71.71086590489794332, -3.843102063196407681 ) ) ;
#59316 = CARTESIAN_POINT ( 'NONE',  ( 73.82984320377984488, 55.19439280614383847, -16.12229116386306771 ) ) ;
#59318 = CARTESIAN_POINT ( 'NONE',  ( 64.45080651302146180, 218.0177522451419065, 5.000000000000046185 ) ) ;
#59317 = CARTESIAN_POINT ( 'NONE',  ( 168.3523909146705080, 257.0143146618579522, 13.69849197686756526 ) ) ;
#59319 = CARTESIAN_POINT ( 'NONE',  ( 75.73386563160880769, 54.39615213926118287, 16.57551599053614311 ) ) ;
#59320 = CARTESIAN_POINT ( 'NONE',  ( 198.7076130252130497, 286.4753137200327728, 17.36142183403824291 ) ) ;
#59321 = CARTESIAN_POINT ( 'NONE',  ( 51.26196130476884605, 213.7365022471903160, 2.944929066748280225E-16 ) ) ;
#59322 = CARTESIAN_POINT ( 'NONE',  ( -19.65312891409030271, 93.06504152958497400, 177.5919119679930134 ) ) ;
#59323 = EDGE_CURVE ( 'NONE', #21672, #13779, #44234, .T. ) ;
#59324 = CARTESIAN_POINT ( 'NONE',  ( -63.39619785071779035, 38.08345695496143435, 10.00000000000000000 ) ) ;
#59325 = CARTESIAN_POINT ( 'NONE',  ( 6.913983429043053519, 183.9869531367911009, 4.594050593750046652 ) ) ;
#59326 = CARTESIAN_POINT ( 'NONE',  ( 72.84756190538608678, 70.91156448913383770, -7.844936087786376966 ) ) ;
#59327 = CARTESIAN_POINT ( 'NONE',  ( 152.8522706834672533, 265.8990964544007056, 17.63080661522264947 ) ) ;
#59328 = CARTESIAN_POINT ( 'NONE',  ( 43.33837710268888799, 27.94754757982092741, 5.678558825948272215 ) ) ;
#59329 = CARTESIAN_POINT ( 'NONE',  ( 133.7124848875370731, 259.5530062829863596, -4.648177544792955347E-16 ) ) ;
#59330 = CARTESIAN_POINT ( 'NONE',  ( 179.4408063581041688, 277.4340371255875652, 17.62723233342114071 ) ) ;
#59331 = CARTESIAN_POINT ( 'NONE',  ( 185.2668547008559301, 266.6439737122302631, 14.32305106529361893 ) ) ;
#59332 = LINE ( 'NONE', #90312, #28291 ) ;
#59333 = CARTESIAN_POINT ( 'NONE',  ( 160.8582016657742031, 280.1240471360480910, 9.077153339507843199 ) ) ;
#59334 = APPLICATION_PROTOCOL_DEFINITION ( 'draft international standard', 'automotive_design', 1998, #50890 ) ;
#59335 = CARTESIAN_POINT ( 'NONE',  ( 14.74991654177707723, 23.91421378149918198, 9.188101187500008038 ) ) ;
#59336 = CARTESIAN_POINT ( 'NONE',  ( 71.96242732416024523, 72.61395932958828325, 1.324942441655010628 ) ) ;
#59337 = DIRECTION ( 'NONE',  ( 0.4999999999999992784, -0.8660254037844390407, 0.000000000000000000 ) ) ;
#59338 = CARTESIAN_POINT ( 'NONE',  ( 187.4908492809263691, 258.5206764845227099, -1.234691217589329870 ) ) ;
#59339 = CONICAL_SURFACE ( 'NONE', #20559, 9.999999999999998224, 0.7853981633974214116 ) ;
#59340 = CARTESIAN_POINT ( 'NONE',  ( 194.3252252352508265, 294.0658320307167628, 14.07225870721148731 ) ) ;
#59341 = VERTEX_POINT ( 'NONE', #56921 ) ;
#59342 = AXIS2_PLACEMENT_3D ( 'NONE', #29891, #99806, #38477 ) ;
#59343 = CARTESIAN_POINT ( 'NONE',  ( 181.7253891428028396, 289.6325948940144599, 12.87432269931904649 ) ) ;
#59344 = CARTESIAN_POINT ( 'NONE',  ( 156.6168467568483891, 276.9391697405689001, 11.51099842983860633 ) ) ;
#59345 = CARTESIAN_POINT ( 'NONE',  ( 159.3995226465659982, 254.5589234043588078, -16.81133486613867234 ) ) ;
#59346 = DIRECTION ( 'NONE',  ( -0.8660254037844387076, -0.4999999999999998890, -0.000000000000000000 ) ) ;
#59347 = VERTEX_POINT ( 'NONE', #3263 ) ;
#59348 = CARTESIAN_POINT ( 'NONE',  ( 196.5932062138799949, 289.3313561647224219, -16.66630370796737282 ) ) ;
#59349 = CARTESIAN_POINT ( 'NONE',  ( 82.53995181069322484, 40.45689495123288282, 0.8907401359745065195 ) ) ;
#59350 = VECTOR ( 'NONE', #13913, 1000.000000000000000 ) ;
#59351 = CARTESIAN_POINT ( 'NONE',  ( 66.18541256665433536, 68.53576410546624231, 4.757783260268557690 ) ) ;
#59352 = CARTESIAN_POINT ( 'NONE',  ( 203.0862352702880003, 278.8913175244117610, -15.09542727681365015 ) ) ;
#59353 = VERTEX_POINT ( 'NONE', #11369 ) ;
#59354 = ORIENTED_EDGE ( 'NONE', *, *, #11853, .T. ) ;
#59356 = CARTESIAN_POINT ( 'NONE',  ( 164.0777181605478745, 246.4560510864015441, 5.763760713451748785 ) ) ;
#59355 = CARTESIAN_POINT ( 'NONE',  ( 159.6554334375900055, 278.4301001067392463, -9.783717483729949649 ) ) ;
#59357 = CARTESIAN_POINT ( 'NONE',  ( 192.0645969571214096, 297.9813550654635605, 11.46542907566974812 ) ) ;
#59358 = ORIENTED_EDGE ( 'NONE', *, *, #12881, .T. ) ;
#59359 = CARTESIAN_POINT ( 'NONE',  ( 190.7851866479434761, 300.1973587246873194, 7.931162401707728016 ) ) ;
#59360 = CARTESIAN_POINT ( 'NONE',  ( 80.31556117237309422, 57.81632953744806258, 16.60139635717628082 ) ) ;
#59361 = CARTESIAN_POINT ( 'NONE',  ( 177.4308907843801535, 263.7877129026015268, 14.57181058525106643 ) ) ;
#59362 = VERTEX_POINT ( 'NONE', #64541 ) ;
#59363 = CARTESIAN_POINT ( 'NONE',  ( 79.14312167556931854, 57.64441083166269664, 0.000000000000000000 ) ) ;
#59364 = ADVANCED_FACE ( 'NONE', ( #10349 ), #74153, .T. ) ;
#59365 = CARTESIAN_POINT ( 'NONE',  ( 81.01203187699685770, 43.60516739924280216, 9.421401130122879053 ) ) ;
#59366 = ORIENTED_EDGE ( 'NONE', *, *, #93323, .F. ) ;
#59367 = CARTESIAN_POINT ( 'NONE',  ( 164.8616299252405213, 245.0982760813026857, 1.544363874765093625 ) ) ;
#59368 = CARTESIAN_POINT ( 'NONE',  ( 74.14512716957341354, 61.63656387330870956, 15.03512766998534467 ) ) ;
#59369 = VERTEX_POINT ( 'NONE', #41216 ) ;
#59370 = CARTESIAN_POINT ( 'NONE',  ( 174.4235015103839430, 277.1789894570474644, -15.65561870163843139 ) ) ;
#59371 = CARTESIAN_POINT ( 'NONE',  ( 170.6146014438598399, 262.6168579639755762, -15.59251864883664496 ) ) ;
#59372 = ORIENTED_EDGE ( 'NONE', *, *, #63866, .T. ) ;
#59373 = DIRECTION ( 'NONE',  ( 0.000000000000000000, -0.000000000000000000, -1.000000000000000000 ) ) ;
#59374 = CARTESIAN_POINT ( 'NONE',  ( 193.2140586456748679, 295.9904290195353269, -12.67640480829088823 ) ) ;
#59375 = ORIENTED_EDGE ( 'NONE', *, *, #65804, .F. ) ;
#59376 = CARTESIAN_POINT ( 'NONE',  ( 157.6447300738524007, 268.8659721402340210, 15.63426755860266049 ) ) ;
#59377 = ORIENTED_EDGE ( 'NONE', *, *, #33382, .F. ) ;
#59378 = CARTESIAN_POINT ( 'NONE',  ( 73.52359277784351832, 69.81900013914946612, 9.283661257273005063 ) ) ;
#59379 = CARTESIAN_POINT ( 'NONE',  ( 168.9258527264130976, 272.6118975377002016, 16.11663601824622560 ) ) ;
#59380 = CARTESIAN_POINT ( 'NONE',  ( 190.7569505155522904, 300.2462651405980978, -5.670926626284815697 ) ) ;
#59381 = CARTESIAN_POINT ( 'NONE',  ( 188.6309741990370981, 298.5980790689797004, -4.273843755561794744 ) ) ;
#59382 = LINE ( 'NONE', #90358, #9100 ) ;
#59383 = FACE_OUTER_BOUND ( 'NONE', #87108, .T. ) ;
#59384 = CARTESIAN_POINT ( 'NONE',  ( 191.0852157684255133, 299.6776930442621278, 8.737980942128526607 ) ) ;
#59385 = CARTESIAN_POINT ( 'NONE',  ( 146.5157004908022031, 276.8743579738231233, -0.1877253132609108255 ) ) ;
#59386 = ORIENTED_EDGE ( 'NONE', *, *, #75121, .T. ) ;
#59387 = CARTESIAN_POINT ( 'NONE',  ( 73.13914032746497185, 58.30547864447190420, -15.74582499144751679 ) ) ;
#59388 = VECTOR ( 'NONE', #90547, 1000.000000000000114 ) ;
#59389 = CARTESIAN_POINT ( 'NONE',  ( 32.48073783699224748, 37.49103043416551628, -8.090169943749479842 ) ) ;
#59391 = CARTESIAN_POINT ( 'NONE',  ( 164.5813345449211624, 245.5837619211427523, 1.447064457712487373 ) ) ;
#59390 = CARTESIAN_POINT ( 'NONE',  ( 196.3286486926436680, 290.5958008134369948, -16.58330917766970458 ) ) ;
#59393 = ORIENTED_EDGE ( 'NONE', *, *, #17792, .F. ) ;
#59392 = CARTESIAN_POINT ( 'NONE',  ( 67.08913548327878118, 66.86964105702345762, 8.907371351497101131 ) ) ;
#59394 = CARTESIAN_POINT ( 'NONE',  ( 171.4377615637976646, 289.1140544575544595, 4.296774136842674174 ) ) ;
#59395 = CARTESIAN_POINT ( 'NONE',  ( 176.6326841078148107, 289.9666541282182948, -9.329455955297444092 ) ) ;
#59396 = VECTOR ( 'NONE', #41636, 1000.000000000000000 ) ;
#59397 = VERTEX_POINT ( 'NONE', #49342 ) ;
#59398 = CARTESIAN_POINT ( 'NONE',  ( 190.3115065349328177, 301.0177967469567761, -3.259545964094417769 ) ) ;
#59399 = CARTESIAN_POINT ( 'NONE',  ( 71.78685388442551130, 69.08504693158637622, 8.871386085792403620 ) ) ;
#59400 = CARTESIAN_POINT ( 'NONE',  ( 202.8915528389443068, 277.8823096497555412, 15.16837591707065869 ) ) ;
#59401 = CARTESIAN_POINT ( 'NONE',  ( 79.19103031000082638, 46.13451125956017052, 12.66280935556781095 ) ) ;
#59402 = CARTESIAN_POINT ( 'NONE',  ( 160.1334858203248643, 253.2876618965237867, -16.18833947189418510 ) ) ;
#59403 = CARTESIAN_POINT ( 'NONE',  ( 189.9981042791225150, 301.5606253772268133, -1.333257489390088368 ) ) ;
#59404 = ORIENTED_EDGE ( 'NONE', *, *, #5913, .T. ) ;
#59405 = CARTESIAN_POINT ( 'NONE',  ( 170.7953178271928039, 255.2457615276028093, -12.92277808742838374 ) ) ;
#59406 = VECTOR ( 'NONE', #76031, 1000.000000000000000 ) ;
#59407 = CARTESIAN_POINT ( 'NONE',  ( 193.8354046899084153, 268.4885937380259406, 12.87375928640720524 ) ) ;
#59408 = CARTESIAN_POINT ( 'NONE',  ( 164.2578067403839555, 246.1441285162624126, -2.322300236470859591 ) ) ;
#59409 = CARTESIAN_POINT ( 'NONE',  ( 39.40823858692152015, 186.8927522451417929, -10.00000000000009059 ) ) ;
#59410 = CARTESIAN_POINT ( 'NONE',  ( 122.6912752411227103, 232.4548013555409796, -4.594050593750042211 ) ) ;
#59411 = CARTESIAN_POINT ( 'NONE',  ( 199.0773057068961123, 285.8349872121713702, -17.17316764978006560 ) ) ;
#59412 = CARTESIAN_POINT ( 'NONE',  ( 47.96820964746023463, 80.67316705762479501, -10.00000000000000000 ) ) ;
#59413 = CARTESIAN_POINT ( 'NONE',  ( -22.42236680055709641, 157.8615022471902591, 0.000000000000000000 ) ) ;
#59414 = CARTESIAN_POINT ( 'NONE',  ( 208.2161171980831682, 270.0061013886409569, 2.944709006235987747 ) ) ;
#59415 = CARTESIAN_POINT ( 'NONE',  ( 29.51209413086700906, 187.8458772461660544, 9.188101187500095079 ) ) ;
#59416 = DIRECTION ( 'NONE',  ( 0.000000000000000000, 0.000000000000000000, 1.000000000000000000 ) ) ;
#59417 = VECTOR ( 'NONE', #64256, 1000.000000000000227 ) ;
#59418 = ORIENTED_EDGE ( 'NONE', *, *, #47144, .F. ) ;
#59419 = CARTESIAN_POINT ( 'NONE',  ( 174.5508403973756515, 260.3590064504865040, -14.93617697178709314 ) ) ;
#59420 = CARTESIAN_POINT ( 'NONE',  ( 181.2785360512119155, 267.7684897940154656, 14.99012931819231653 ) ) ;
#59421 = EDGE_CURVE ( 'NONE', #13195, #64017, #57107, .T. ) ;
#59422 = CARTESIAN_POINT ( 'NONE',  ( 69.74575514227493045, 70.90735852889230273, 0.2747676320513545156 ) ) ;
#59423 = CARTESIAN_POINT ( 'NONE',  ( 105.5870131927823792, 221.7677522451417929, -5.000000000000041744 ) ) ;
#59424 = CARTESIAN_POINT ( 'NONE',  ( 13.50812563192542548, 9.927558733836244542, 6.180339887498953466 ) ) ;
#59425 = EDGE_CURVE ( 'NONE', #38681, #53400, #27046, .T. ) ;
#59426 = CARTESIAN_POINT ( 'NONE',  ( 179.2989983647532881, 287.9912263975500650, -12.74886096560045878 ) ) ;
#59427 = CARTESIAN_POINT ( 'NONE',  ( 164.1030008762014063, 250.1404465237781949, 10.60968069481521781 ) ) ;
#59428 = AXIS2_PLACEMENT_3D ( 'NONE', #56199, #48630, #42012 ) ;
#59429 = CARTESIAN_POINT ( 'NONE',  ( 101.7620676594010973, 222.8927522451418213, -10.00000000000009059 ) ) ;
#59430 = VERTEX_POINT ( 'NONE', #73158 ) ;
#59431 = CARTESIAN_POINT ( 'NONE',  ( 198.7756665828275686, 267.6177563492644254, -8.240796915055890182 ) ) ;
#59432 = ADVANCED_FACE ( 'NONE', ( #66528 ), #41725, .T. ) ;
#59433 = CARTESIAN_POINT ( 'NONE',  ( 156.6246755477763202, 280.3786321986610233, -1.584460325695541849 ) ) ;
#59434 = DIRECTION ( 'NONE',  ( 1.000000000000000000, 0.000000000000000000, 0.000000000000000000 ) ) ;
#59435 = CARTESIAN_POINT ( 'NONE',  ( 19.44454881187291662, 182.0333772461660544, 9.188101187500095079 ) ) ;
#59436 = CARTESIAN_POINT ( 'NONE',  ( 10.11087252192314345, 14.03677371833799548, 10.00000000000000533 ) ) ;
#59437 = CARTESIAN_POINT ( 'NONE',  ( 80.06754722118087386, 49.20904160353000378, 14.67962688378318958 ) ) ;
#59438 = CARTESIAN_POINT ( 'NONE',  ( 71.46737963517870185, 59.24065988555543782, -15.76538128299026909 ) ) ;
#59439 = CARTESIAN_POINT ( 'NONE',  ( -48.71813016832984289, 30.75580926756358480, -10.00000000000000000 ) ) ;
#59440 = CARTESIAN_POINT ( 'NONE',  ( 59.55252387252222945, 199.0643266524159856, -9.188101187500093303 ) ) ;
#59441 = CARTESIAN_POINT ( 'NONE',  ( 207.7655736232174206, 270.7864657513322300, 3.530742899761726949 ) ) ;
#59442 = CARTESIAN_POINT ( 'NONE',  ( 164.2712161151136172, 246.1209027979328710, 7.276091357954241445 ) ) ;
#59443 = PLANE ( 'NONE',  #11689 ) ;
#59444 = CARTESIAN_POINT ( 'NONE',  ( 149.0155189933042266, 277.2682270220686291, -2.168681601895305011 ) ) ;
#59445 = EDGE_LOOP ( 'NONE', ( #47079, #22516, #44055, #40181 ) ) ;
#59446 = CARTESIAN_POINT ( 'NONE',  ( 208.3132655666949233, 269.8378354783333180, 2.688523655043302707 ) ) ;
#59447 = CARTESIAN_POINT ( 'NONE',  ( 21.31191609055711211, 173.1115022471901739, -5.000000000000041744 ) ) ;
#59448 = DIRECTION ( 'NONE',  ( -0.2033683215378938036, 0.3522442655536374700, -0.9135454576426059736 ) ) ;
#59449 = AXIS2_PLACEMENT_3D ( 'NONE', #34882, #65296, #64807 ) ;
#59450 = CARTESIAN_POINT ( 'NONE',  ( 145.2890388471816721, 248.5643266524159856, -9.188101187500093303 ) ) ;
#59451 = CARTESIAN_POINT ( 'NONE',  ( 28.18775043786755319, 21.98920272979927759, 7.433330006724137462 ) ) ;
#59452 = CARTESIAN_POINT ( 'NONE',  ( 165.0094001503442485, 244.8423305435771624, 1.224072641870707301 ) ) ;
#59453 = DIRECTION ( 'NONE',  ( 0.4458072818673325943, 0.8951289669282637140, 0.000000000000000000 ) ) ;
#59454 = CARTESIAN_POINT ( 'NONE',  ( 75.03531058944138010, 53.45646444308351874, -16.05297267460561628 ) ) ;
#59456 = CARTESIAN_POINT ( 'NONE',  ( 189.5229297568409663, 289.6899146468908270, 14.72468552167156908 ) ) ;
#59455 = LINE ( 'NONE', #66586, #77564 ) ;
#59457 = CARTESIAN_POINT ( 'NONE',  ( 68.99476962784538614, 64.41967618265260853, 12.49304100067268486 ) ) ;
#59458 = ORIENTED_EDGE ( 'NONE', *, *, #26141, .T. ) ;
#59459 = CARTESIAN_POINT ( 'NONE',  ( 150.7254409736883645, 269.5828735707850683, 14.54962197351449049 ) ) ;
#59460 = CARTESIAN_POINT ( 'NONE',  ( 163.3401907624258627, 247.7334860119229063, 8.055311219927849820 ) ) ;
#59461 = CARTESIAN_POINT ( 'NONE',  ( 187.4171132689631634, 261.5282790321019206, -9.397869408254909018 ) ) ;
#59462 = CARTESIAN_POINT ( 'NONE',  ( 173.0074926688108405, 268.3266801289679506, -16.33672149581441246 ) ) ;
#59463 = CARTESIAN_POINT ( 'NONE',  ( 197.3443253216253481, 273.2483388696968518, -14.62721317763432971 ) ) ;
#59464 = VERTEX_POINT ( 'NONE', #3751 ) ;
#59465 = CARTESIAN_POINT ( 'NONE',  ( 69.88579529611078556, 68.58817071522582864, 7.900203795979792609 ) ) ;
#59466 = CIRCLE ( 'NONE', #54620, 70.00000000000001421 ) ;
#59467 = CARTESIAN_POINT ( 'NONE',  ( 170.8306833669449247, 284.5486215507588099, -11.65048194455012620 ) ) ;
#59468 = CARTESIAN_POINT ( 'NONE',  ( 71.96958093079467744, 72.27199135482793224, 0.6334255257473564438 ) ) ;
#59469 = B_SPLINE_SURFACE_WITH_KNOTS ( 'NONE', 3, 1, ( 
 ( #40151, #31059 ),
 ( #53848, #39144 ),
 ( #16866, #94409 ),
 ( #7773, #47752 ),
 ( #9795, #77169 ),
 ( #78185, #24962 ),
 ( #46769, #15861 ),
 ( #672, #9278 ),
 ( #84808, #77694 ),
 ( #31555, #1181 ),
 ( #8277, #70056 ),
 ( #71093, #40655 ),
 ( #15348, #62967 ),
 ( #79221, #85315 ),
 ( #93412, #23961 ),
 ( #61949, #24470 ),
 ( #55840, #86835 ),
 ( #2188, #17369 ),
 ( #23452, #46244 ),
 ( #71593, #38665 ),
 ( #62444, #69568 ),
 ( #176, #54863 ),
 ( #92900, #54344 ),
 ( #85843, #47263 ),
 ( #18383, #66461 ),
 ( #35560, #18889 ),
 ( #95437, #19882 ),
 ( #25989, #41658 ),
 ( #87844, #27483 ),
 ( #49278, #34090 ),
 ( #73576, #10281 ),
 ( #64979, #41151 ),
 ( #42158, #96912 ),
 ( #3686, #26976 ) ),
 .UNSPECIFIED., .T., .F., .F.,
 ( 4, 2, 2, 2, 2, 2, 2, 2, 2, 2, 2, 2, 2, 2, 2, 2, 4 ),
 ( 2, 2 ),
 ( 0.000000000000000000, 0.06250000000000000000, 0.1250000000000000000, 0.1875000000000000000, 0.2500000000000000000, 0.3125000000000000000, 0.3750000000000000000, 0.4375000000000000000, 0.5000000000000000000, 0.5625000000000000000, 0.6250000000000000000, 0.6875000000000000000, 0.7500000000000000000, 0.8125000000000000000, 0.8750000000000000000, 0.9375000000000000000, 1.000000000000000000 ),
 ( 0.000000000000000000, 1.000000000000000000 ),
 .UNSPECIFIED. ) ;
#59470 = CARTESIAN_POINT ( 'NONE',  ( -62.55022349715819274, 61.89794670847138747, 59.99999999999999289 ) ) ;
#59471 = DIRECTION ( 'NONE',  ( -1.110223024625156343E-15, 1.000000000000000000, 0.000000000000000000 ) ) ;
#59472 = CARTESIAN_POINT ( 'NONE',  ( 185.7378568990949645, 296.6331975062905144, 4.666997342915078839 ) ) ;
#59473 = CARTESIAN_POINT ( 'NONE',  ( 67.07226750202337939, 68.19592289027032450, 5.518172639132539636 ) ) ;
#59474 = CYLINDRICAL_SURFACE ( 'NONE', #30646, 10.00000000000001066 ) ;
#59475 = CARTESIAN_POINT ( 'NONE',  ( 153.3544108199959908, 265.0293642254135307, -17.49105661178601423 ) ) ;
#59476 = VECTOR ( 'NONE', #31521, 1000.000000000000227 ) ;
#59477 = CARTESIAN_POINT ( 'NONE',  ( 14.19121639173650706, 20.14441083166259716, 10.00000000000000533 ) ) ;
#59478 = DIRECTION ( 'NONE',  ( 0.8868092729070038427, 0.4621356007560455392, 0.000000000000000000 ) ) ;
#59479 = VERTEX_POINT ( 'NONE', #89394 ) ;
#59480 = CARTESIAN_POINT ( 'NONE',  ( 73.83109025078562127, 55.13289435005326311, 16.60030462077566327 ) ) ;
#59481 = CARTESIAN_POINT ( 'NONE',  ( 86.48326989762649930, 47.07371192975631402, -10.55119608217690441 ) ) ;
#59482 = CARTESIAN_POINT ( 'NONE',  ( 156.8307661425255048, 262.4341872189889386, -16.93460929011386540 ) ) ;
#59483 = ORIENTED_EDGE ( 'NONE', *, *, #77639, .F. ) ;
#59484 = CARTESIAN_POINT ( 'NONE',  ( 147.2937583206075942, 275.5267222813735088, 0.1877253132609109920 ) ) ;
#59485 = CARTESIAN_POINT ( 'NONE',  ( 205.1818214405880951, 273.2280494462991101, -9.772995860142792424 ) ) ;
#59486 = VECTOR ( 'NONE', #100007, 999.9999999999998863 ) ;
#59487 = CARTESIAN_POINT ( 'NONE',  ( 204.1793240545508752, 276.9980322128846524, 14.17550310845996187 ) ) ;
#59488 = CARTESIAN_POINT ( 'NONE',  ( 157.7632566947985708, 282.3764601569879460, -1.694678876849560645 ) ) ;
#59489 = EDGE_CURVE ( 'NONE', #47559, #77633, #50327, .T. ) ;
#59490 = DIRECTION ( 'NONE',  ( 0.4999999999999992784, -0.8660254037844390407, 0.000000000000000000 ) ) ;
#59491 = ORIENTED_EDGE ( 'NONE', *, *, #86667, .F. ) ;
#59492 = CARTESIAN_POINT ( 'NONE',  ( 89.59260651841245249, 222.5333772461660544, 9.188101187500095079 ) ) ;
#59493 = CARTESIAN_POINT ( 'NONE',  ( 174.3282188611405559, 255.0574352009110157, -10.77860568660477902 ) ) ;
#59494 = VECTOR ( 'NONE', #14434, 1000.000000000000114 ) ;
#59495 = CARTESIAN_POINT ( 'NONE',  ( 73.11394343355392778, 69.60018041412448042, -9.852821959973875110 ) ) ;
#59496 = CARTESIAN_POINT ( 'NONE',  ( 178.0813752549872504, 269.0315758126946548, -16.95330150772717204 ) ) ;
#59497 = CARTESIAN_POINT ( 'NONE',  ( 81.38913804857537571, 41.97458054521010951, -7.739545251740827858 ) ) ;
#59498 = ORIENTED_EDGE ( 'NONE', *, *, #95301, .T. ) ;
#59499 = ORIENTED_EDGE ( 'NONE', *, *, #98104, .T. ) ;
#59500 = DIRECTION ( 'NONE',  ( 0.5000000000000004441, -0.8660254037844383745, 0.000000000000000000 ) ) ;
#59501 = VERTEX_POINT ( 'NONE', #11851 ) ;
#59502 = CARTESIAN_POINT ( 'NONE',  ( -22.42236680055709641, 157.8615022471902591, 0.000000000000000000 ) ) ;
#59504 = EDGE_CURVE ( 'NONE', #76998, #4619, #60677, .T. ) ;
#59503 = ORIENTED_EDGE ( 'NONE', *, *, #6276, .T. ) ;
#59505 = DIRECTION ( 'NONE',  ( 0.9919084036772433111, -0.1269555777209603886, 0.000000000000000000 ) ) ;
#59506 = VERTEX_POINT ( 'NONE', #42709 ) ;
#59507 = CARTESIAN_POINT ( 'NONE',  ( 164.9546295582813400, 248.3711573621226023, -9.130659607263403643 ) ) ;
#59508 = VECTOR ( 'NONE', #90553, 1000.000000000000227 ) ;
#59510 = EDGE_CURVE ( 'NONE', #934, #63771, #50820, .T. ) ;
#59509 = CARTESIAN_POINT ( 'NONE',  ( 43.16562282991919375, 123.9487658730721904, -10.00000000000000000 ) ) ;
#59511 = CARTESIAN_POINT ( 'NONE',  ( -23.48760161379543732, 99.79357714821047409, 45.19946697165472216 ) ) ;
#59512 = CARTESIAN_POINT ( 'NONE',  ( 71.26654922642217116, 68.38198715351988710, -9.349859695236091284 ) ) ;
#59513 = CARTESIAN_POINT ( 'NONE',  ( 165.4931806181214995, 265.5848062394981639, -16.61349363679761026 ) ) ;
#59514 = EDGE_LOOP ( 'NONE', ( #64727, #74632, #93980, #17934 ) ) ;
#59515 = CARTESIAN_POINT ( 'NONE',  ( 76.83134550358633419, 60.61061650515956956, 15.77294948966528132 ) ) ;
#59516 = CARTESIAN_POINT ( 'NONE',  ( 2.405479210251257438, 24.49540643055184930, 3.479690158560446702E-15 ) ) ;
#59517 = ORIENTED_EDGE ( 'NONE', *, *, #70209, .T. ) ;
#59518 = CARTESIAN_POINT ( 'NONE',  ( 167.2093226243390802, 283.7324425667255241, 9.043444139037532636 ) ) ;
#59520 = ORIENTED_EDGE ( 'NONE', *, *, #59691, .F. ) ;
#59519 = CARTESIAN_POINT ( 'NONE',  ( 199.9158715130028838, 270.2492972290452826, 9.939794670651632913 ) ) ;
#59521 = DIRECTION ( 'NONE',  ( 0.4999999999999995559, -0.8660254037844389297, 0.000000000000000000 ) ) ;
#59522 = CARTESIAN_POINT ( 'NONE',  ( 206.8317058779879574, 272.4039721336197317, -10.41591514895975834 ) ) ;
#59523 = CARTESIAN_POINT ( 'NONE',  ( 149.0752043596417593, 276.3754483912217097, -5.522432154670898541 ) ) ;
#59524 = CARTESIAN_POINT ( 'NONE',  ( 80.50527454617468948, 50.48295520238254142, -15.12725957157805823 ) ) ;
#59525 = CARTESIAN_POINT ( 'NONE',  ( 158.6496056213609904, 257.8578177934796258, 17.38082990300775776 ) ) ;
#59526 = DIRECTION ( 'NONE',  ( -0.8660254037844392627, -0.4999999999999987232, 0.000000000000000000 ) ) ;
#59527 = CARTESIAN_POINT ( 'NONE',  ( 88.32926345284593594, 43.93619003093853337, -2.170256470903187740 ) ) ;
#59528 = ORIENTED_EDGE ( 'NONE', *, *, #93051, .T. ) ;
#59529 = CARTESIAN_POINT ( 'NONE',  ( 147.7395812515338491, 275.4447818272566337, 3.760927250875937489 ) ) ;
#59530 = CARTESIAN_POINT ( 'NONE',  ( 74.97996761797446652, 67.38724533294661967, -12.85106452774880204 ) ) ;
#59531 = ORIENTED_EDGE ( 'NONE', *, *, #65564, .F. ) ;
#59532 = VECTOR ( 'NONE', #20873, 1000.000000000000000 ) ;
#59533 = CARTESIAN_POINT ( 'NONE',  ( 160.9531570974293402, 275.8817019889240214, 12.81199482524368882 ) ) ;
#59534 = CARTESIAN_POINT ( 'NONE',  ( 171.9666747079280071, 279.8309318510848698, -14.47863982768428137 ) ) ;
#59535 = CARTESIAN_POINT ( 'NONE',  ( 164.0970344217799948, 246.4225943405349710, -8.491506243827155131 ) ) ;
#59536 = CARTESIAN_POINT ( 'NONE',  ( -54.21831688459418785, 33.63902229265146104, -10.00000000000000000 ) ) ;
#59537 = AXIS2_PLACEMENT_3D ( 'NONE', #76593, #37572, #16283 ) ;
#59538 = CARTESIAN_POINT ( 'NONE',  ( 160.9791900386504722, 272.6641784107281410, 15.33525930436291951 ) ) ;
#59540 = CARTESIAN_POINT ( 'NONE',  ( 76.12511762330939291, 65.41126435427986507, 14.01861623752280650 ) ) ;
#59539 = CARTESIAN_POINT ( 'NONE',  ( -8.160010933756074891, 166.0958772461660544, -9.188101187500095079 ) ) ;
#59541 = CARTESIAN_POINT ( 'NONE',  ( 16.91508078042228647, 192.1199935810941213, 2.679491924311251605 ) ) ;
#59542 = ORIENTED_EDGE ( 'NONE', *, *, #94384, .F. ) ;
#59543 = AXIS2_PLACEMENT_3D ( 'NONE', #31860, #62252, #54150 ) ;
#59544 = ORIENTED_EDGE ( 'NONE', *, *, #56489, .T. ) ;
#59545 = CARTESIAN_POINT ( 'NONE',  ( 13.97105408662886461, 167.3262482093458061, -5.229199737892075682E-14 ) ) ;
#59546 = DIRECTION ( 'NONE',  ( -0.3402761906661169178, -0.9403255362191098587, 0.000000000000000000 ) ) ;
#59547 = EDGE_CURVE ( 'NONE', #36835, #47529, #19646, .T. ) ;
#59548 = CARTESIAN_POINT ( 'NONE',  ( 67.77468730211444381, 66.37560510333101149, -9.226434066144044266 ) ) ;
#59549 = DIRECTION ( 'NONE',  ( 1.000000000000000000, -8.921435019309292501E-15, 0.000000000000000000 ) ) ;
#59550 = DIRECTION ( 'NONE',  ( -0.8660254037844387076, -0.4999999999999998890, -0.000000000000000000 ) ) ;
#59551 = AXIS2_PLACEMENT_3D ( 'NONE', #51625, #21230, #52601 ) ;
#59552 = CARTESIAN_POINT ( 'NONE',  ( 84.68381221926802027, 47.49403502698439894, 11.40130350688633420 ) ) ;
#59553 = CARTESIAN_POINT ( 'NONE',  ( 172.3741624485570867, 252.4865239976215037, 8.880853820034850798 ) ) ;
#59554 = CARTESIAN_POINT ( 'NONE',  ( 3.504529045289348055, 163.6423013555410080, -4.594050593750043987 ) ) ;
#59555 = CARTESIAN_POINT ( 'NONE',  ( 108.9156247924702114, 239.8149278399160949, -9.188101187500095079 ) ) ;
#59556 = CARTESIAN_POINT ( 'NONE',  ( 36.90037335867692292, 202.1115022471903160, -5.000000000000047962 ) ) ;
#59557 = CARTESIAN_POINT ( 'NONE',  ( 183.1379727938016799, 294.1415918804704575, -7.857043814308706686 ) ) ;
#59558 = CARTESIAN_POINT ( 'NONE',  ( 77.84078212536968522, 50.78282023170922344, 15.24705710655046786 ) ) ;
#59559 = EDGE_CURVE ( 'NONE', #91371, #57418, #45694, .T. ) ;
#59560 = CIRCLE ( 'NONE', #62814, 17.82106496071138935 ) ;
#59561 = EDGE_CURVE ( 'NONE', #86137, #94561, #2670, .T. ) ;
#59562 = CARTESIAN_POINT ( 'NONE',  ( 81.98204644731730184, 41.14170830008083612, -5.380964918418895238 ) ) ;
#59563 = CARTESIAN_POINT ( 'NONE',  ( 69.66731286396763778, 199.4824982072973967, 3.021315404115420679E-15 ) ) ;
#59564 = DIRECTION ( 'NONE',  ( -8.673617379884075901E-16, 0.000000000000000000, 1.000000000000000000 ) ) ;
#59565 = CARTESIAN_POINT ( 'NONE',  ( 207.8996209429610360, 270.5542889829179103, -5.987818313449536411 ) ) ;
#59566 = CARTESIAN_POINT ( 'NONE',  ( 148.1632261683078013, 274.0207597936089883, -7.853210555358286271 ) ) ;
#59567 = CARTESIAN_POINT ( 'NONE',  ( 84.59313982267055110, 50.24721290632345472, 13.87151924479132425 ) ) ;
#59568 = CARTESIAN_POINT ( 'NONE',  ( 190.4356836585210431, 300.3996184492839916, -0.5836641476860114919 ) ) ;
#59569 = CARTESIAN_POINT ( 'NONE',  ( 46.72328617017402053, 209.3297689869269504, -2.679491924311201423 ) ) ;
#59570 = CARTESIAN_POINT ( 'NONE',  ( 162.7494290383994553, 250.9923089725520242, -12.89632743124666803 ) ) ;
#59571 = DIRECTION ( 'NONE',  ( 0.4999999999999998890, -0.8660254037844385966, 0.000000000000000000 ) ) ;
#59572 = AXIS2_PLACEMENT_3D ( 'NONE', #78153, #38115, #78657 ) ;
#59573 = CARTESIAN_POINT ( 'NONE',  ( 175.8807902318873744, 265.5460882003382039, -15.84645557839000496 ) ) ;
#59574 = CARTESIAN_POINT ( 'NONE',  ( 97.65764163903753570, 221.0643266524160424, 9.188101187500095079 ) ) ;
#59575 = CARTESIAN_POINT ( 'NONE',  ( 6.332637391379750014, 21.84336893147753855, -7.433330006724137462 ) ) ;
#59576 = CARTESIAN_POINT ( 'NONE',  ( 150.6487462746963502, 269.7157126861102370, 15.18501655901553704 ) ) ;
#59577 = CARTESIAN_POINT ( 'NONE',  ( 39.25774830830064843, 55.25619937740605536, -10.00000000000000000 ) ) ;
#59579 = CARTESIAN_POINT ( 'NONE',  ( 200.3578380681407793, 283.6170401017593576, 17.20245520226215774 ) ) ;
#59578 = CARTESIAN_POINT ( 'NONE',  ( 157.2744851780909414, 258.2395962677452985, 18.17792129701959070 ) ) ;
#59580 = CARTESIAN_POINT ( 'NONE',  ( 196.3322077676189394, 290.5896363147520560, 17.46901783180497603 ) ) ;
#59581 = CARTESIAN_POINT ( 'NONE',  ( 151.4376533647338476, 268.3492855237141725, -15.16853828792834236 ) ) ;
#59582 = CARTESIAN_POINT ( 'NONE',  ( -43.77314298070450604, 40.37936670953467910, 59.99999999999999289 ) ) ;
#59583 = AXIS2_PLACEMENT_3D ( 'NONE', #37997, #45602, #76535 ) ;
#59584 = CARTESIAN_POINT ( 'NONE',  ( 39.32338737416051089, 38.10171378149922106, 9.188101187500008038 ) ) ;
#59585 = CARTESIAN_POINT ( 'NONE',  ( 192.6789561813392595, 296.9172536750198219, -11.84591848451790952 ) ) ;
#59586 = FACE_BOUND ( 'NONE', #65533, .T. ) ;
#59587 = VERTEX_POINT ( 'NONE', #51312 ) ;
#59588 = CARTESIAN_POINT ( 'NONE',  ( 28.09632999608277615, 19.14754757982091604, -5.678558825948276656 ) ) ;
#59589 = DIRECTION ( 'NONE',  ( 0.000000000000000000, 0.000000000000000000, 1.000000000000000000 ) ) ;
#59590 = CARTESIAN_POINT ( 'NONE',  ( 146.9422184197532317, 276.1356072505412840, -5.063317562214876943 ) ) ;
#59591 = CARTESIAN_POINT ( 'NONE',  ( 47.78135487164287554, 106.4364430393875267, 10.00000000000000000 ) ) ;
#59592 = ORIENTED_EDGE ( 'NONE', *, *, #13491, .T. ) ;
#59593 = CARTESIAN_POINT ( 'NONE',  ( 70.94178428196880759, 60.98283367154441947, 14.53595739235115936 ) ) ;
#59594 = CARTESIAN_POINT ( 'NONE',  ( 159.5573297132660002, 254.2855935470410031, 16.91607698584599007 ) ) ;
#59595 = CARTESIAN_POINT ( 'NONE',  ( 154.0583916588297768, 267.0402830145829967, 16.21101371575731065 ) ) ;
#59596 = DIRECTION ( 'NONE',  ( 0.3301025504114333264, 0.9439450758449176027, 0.000000000000000000 ) ) ;
#59597 = CARTESIAN_POINT ( 'NONE',  ( 133.4622058806418750, 257.8615022471902876, 5.000000000000046185 ) ) ;
#59598 = EDGE_LOOP ( 'NONE', ( #4332, #76928, #35412, #46442 ) ) ;
#59599 = DIRECTION ( 'NONE',  ( 0.9795703749556662343, -0.2011016670970565412, 0.000000000000000000 ) ) ;
#59600 = VECTOR ( 'NONE', #67509, 1000.000000000000000 ) ;
#59601 = ORIENTED_EDGE ( 'NONE', *, *, #72458, .T. ) ;
#59602 = DIRECTION ( 'NONE',  ( 1.000000000000000000, 1.038851544470682011E-13, 0.000000000000000000 ) ) ;
#59603 = CARTESIAN_POINT ( 'NONE',  ( 85.26196194431867070, 42.92904878948160530, 3.532607271268957572 ) ) ;
#59604 = ORIENTED_EDGE ( 'NONE', *, *, #74787, .T. ) ;
#59605 = CARTESIAN_POINT ( 'NONE',  ( 181.8498033080804248, 291.5435437066161626, -11.41179615309663120 ) ) ;
#59606 = ORIENTED_EDGE ( 'NONE', *, *, #62730, .T. ) ;
#59607 = AXIS2_PLACEMENT_3D ( 'NONE', #70326, #32332, #23717 ) ;
#59608 = DIRECTION ( 'NONE',  ( 0.000000000000000000, -0.3470917258701586294, -0.9378311862123559495 ) ) ;
#59609 = CARTESIAN_POINT ( 'NONE',  ( 158.6518137166425788, 255.8539932602588181, 16.06016111216393583 ) ) ;
#59610 = CARTESIAN_POINT ( 'NONE',  ( 190.7226089735735570, 278.2851069703174289, -16.65597922127235719 ) ) ;
#59611 = CARTESIAN_POINT ( 'NONE',  ( 88.13402233310422673, 44.37312773088997631, -4.489783613381807648 ) ) ;
#59612 = CARTESIAN_POINT ( 'NONE',  ( 201.0732166862245549, 282.3779679885897167, -18.18766936363638820 ) ) ;
#59613 = VECTOR ( 'NONE', #10228, 1000.000000000000227 ) ;
#59614 = EDGE_CURVE ( 'NONE', #16011, #10482, #25741, .T. ) ;
#59615 = VECTOR ( 'NONE', #58750, 1000.000000000000000 ) ;
#59616 = CARTESIAN_POINT ( 'NONE',  ( 43.73469409959700016, 27.11110640527295956, -2.839279412974138328 ) ) ;
#59617 = CARTESIAN_POINT ( 'NONE',  ( 75.75053192129530544, 59.74695923988007706, -15.79163679635876427 ) ) ;
#59618 = EDGE_CURVE ( 'NONE', #97695, #97906, #37721, .T. ) ;
#59619 = CARTESIAN_POINT ( 'NONE',  ( 40.34888600819125060, 126.6204015641749834, -10.00000000000000000 ) ) ;
#59620 = CARTESIAN_POINT ( 'NONE',  ( -55.56624327025929944, 44.99999999999998579, 10.00000000000000000 ) ) ;
#59621 = B_SPLINE_CURVE_WITH_KNOTS ( 'NONE', 3,
 ( #43058, #81140, #59253, #12707 ),
 .UNSPECIFIED., .F., .F.,
 ( 4, 4 ),
 ( 0.01172910784184959775, 0.01779018763767279548 ),
 .UNSPECIFIED. ) ;
#59622 = ORIENTED_EDGE ( 'NONE', *, *, #99403, .T. ) ;
#59623 = EDGE_LOOP ( 'NONE', ( #1484, #93607, #84572, #89579 ) ) ;
#59624 = CARTESIAN_POINT ( 'NONE',  ( 182.9391731548801943, 296.0526933300616861, 0.3971291663347272238 ) ) ;
#59625 = AXIS2_PLACEMENT_3D ( 'NONE', #88579, #19141, #50015 ) ;
#59626 =( BOUNDED_CURVE ( )  B_SPLINE_CURVE ( 2, ( #49759, #79207, #25456, #2677, #63460, #18372, #56344, #41645, #55827 ),
 .UNSPECIFIED., .F., .T. ) 
 B_SPLINE_CURVE_WITH_KNOTS ( ( 3, 2, 2, 2, 3 ),
 ( 0.09274193548387096864, 0.09408602150537634379, 0.09677419354838709409, 0.09946236559139784439, 0.1008064516129032334 ),
 .UNSPECIFIED. ) 
 CURVE ( )  GEOMETRIC_REPRESENTATION_ITEM ( )  RATIONAL_B_SPLINE_CURVE ( ( 0.9330127018922194093, 0.9330127018922194093, 1.000000000000000000, 0.8660254037844387076, 1.000000000000000000, 0.8660254037844387076, 1.000000000000000000, 0.9330127018922189652, 0.9330127018922192983 ) ) 
 REPRESENTATION_ITEM ( '' )  );
#59628 = CARTESIAN_POINT ( 'NONE',  ( 162.2331215717501607, 272.2958999960979440, -15.94685713422084739 ) ) ;
#59627 = CARTESIAN_POINT ( 'NONE',  ( 174.4196659502841271, 257.0085290835094156, -12.24909860563172259 ) ) ;
#59629 = CARTESIAN_POINT ( 'NONE',  ( 165.0817809681736037, 244.7169632896033136, -1.727194264083430131 ) ) ;
#59630 = PLANE ( 'NONE',  #79680 ) ;
#59631 = CARTESIAN_POINT ( 'NONE',  ( 203.4435754520237651, 276.2723861740593634, 14.48166091637323483 ) ) ;
#59632 = CARTESIAN_POINT ( 'NONE',  ( 82.18773400532718654, 40.81893033463614984, 1.092004392742265795 ) ) ;
#59634 = EDGE_CURVE ( 'NONE', #45676, #62226, #14323, .T. ) ;
#59633 = CARTESIAN_POINT ( 'NONE',  ( 170.6833767652849758, 288.4039556261358825, -4.055045876719096221 ) ) ;
#59635 = CARTESIAN_POINT ( 'NONE',  ( 165.8447336379009300, 265.9679405602628890, 17.68066565608797092 ) ) ;
#59636 = CARTESIAN_POINT ( 'NONE',  ( 181.9564058445976400, 256.6289831591705592, 5.167692713115564551 ) ) ;
#59637 = CARTESIAN_POINT ( 'NONE',  ( 115.5194155920915620, 231.3768266524159856, 9.188101187500098632 ) ) ;
#59639 = ORIENTED_EDGE ( 'NONE', *, *, #23766, .F. ) ;
#59638 = B_SPLINE_CURVE_WITH_KNOTS ( 'NONE', 3,
 ( #25403, #71529, #10718, #54799 ),
 .UNSPECIFIED., .F., .F.,
 ( 4, 4 ),
 ( 0.008498457973065165830, 0.01488670130818619056 ),
 .UNSPECIFIED. ) ;
#59641 = CARTESIAN_POINT ( 'NONE',  ( -19.65312891409030271, 93.06504152958497400, 177.5919119679930134 ) ) ;
#59640 = B_SPLINE_CURVE_WITH_KNOTS ( 'NONE', 3,
 ( #3635, #12228, #58787, #81166, #65415, #27430, #4110, #80164, #57803, #73042, #65905, #20327, #96358, #42108, #66413, #72548, #5117, #87794, #43086, #74539, #74029, #64421, #19829, #12737, #97339, #88782, #50213, #4617, #42595, #81654, #82162, #34038, #89280, #19352, #27907, #50700, #34516, #95384, #41605, #35510, #18336, #49230, #26924, #96862, #43602, #73529 ),
 .UNSPECIFIED., .F., .F.,
 ( 4, 1, 2, 2, 1, 2, 2, 1, 1, 2, 2, 1, 1, 2, 2, 1, 1, 2, 2, 1, 1, 1, 2, 2, 1, 1, 1, 2, 2, 4 ),
 ( 0.000000000000000000, 0.06249999999998762101, 0.09374999999998372135, 0.1249999999999798217, 0.1874999999999718003, 0.2187499999999678035, 0.2499999999999638067, 0.3124999999999550915, 0.3437499999999526490, 0.3593749999999524825, 0.3749999999999522604, 0.4374999999999585887, 0.4687499999999626965, 0.4843749999999644174, 0.4999999999999661382, 0.5624999999999762412, 0.5937499999999804601, 0.6093749999999825695, 0.6249999999999846789, 0.6874999999999930056, 0.7187499999999977796, 0.7343750000000009992, 0.7421875000000016653, 0.7500000000000023315, 0.8125000000000105471, 0.8437500000000147660, 0.8593750000000154321, 0.8671875000000148770, 0.8750000000000143219, 1.000000000000000000 ),
 .UNSPECIFIED. ) ;
#59642 = CARTESIAN_POINT ( 'NONE',  ( 188.2915414428695726, 273.5140509337351773, 15.65656605059880313 ) ) ;
#59643 = VERTEX_POINT ( 'NONE', #99435 ) ;
#59644 = VECTOR ( 'NONE', #82681, 1000.000000000000000 ) ;
#59645 = VERTEX_POINT ( 'NONE', #97456 ) ;
#59646 = CARTESIAN_POINT ( 'NONE',  ( 87.24292777721575476, 46.11748857515735267, -8.882011181227387198 ) ) ;
#59647 = EDGE_CURVE ( 'NONE', #26502, #72620, #95753, .T. ) ;
#59648 = LINE ( 'NONE', #22666, #47905 ) ;
#59649 = CARTESIAN_POINT ( 'NONE',  ( 196.4982648257524147, 290.3020170531091821, 16.69353242256149628 ) ) ;
#59650 = CARTESIAN_POINT ( 'NONE',  ( 206.4640281786353171, 273.0408085897082060, -10.81921452789957883 ) ) ;
#59651 = DIRECTION ( 'NONE',  ( -0.8660254037844387076, -0.4999999999999998890, -0.000000000000000000 ) ) ;
#59652 = EDGE_CURVE ( 'NONE', #31643, #7307, #87347, .T. ) ;
#59653 = ORIENTED_EDGE ( 'NONE', *, *, #75974, .T. ) ;
#59654 = ORIENTED_EDGE ( 'NONE', *, *, #87942, .F. ) ;
#59655 = CARTESIAN_POINT ( 'NONE',  ( 12.00096474099108690, 32.03863464977599307, -10.00000000000000000 ) ) ;
#59656 = VERTEX_POINT ( 'NONE', #70003 ) ;
#59657 = CARTESIAN_POINT ( 'NONE',  ( 194.6804144021959928, 266.4464820258078817, -8.228719024875283949 ) ) ;
#59658 = CARTESIAN_POINT ( 'NONE',  ( -2.962795650140754855, 157.5494855054052152, -2.679491924311252493 ) ) ;
#59659 = CARTESIAN_POINT ( 'NONE',  ( 83.83418024175072958, 48.96564077411333926, 12.89930316525782850 ) ) ;
#59661 = CARTESIAN_POINT ( 'NONE',  ( 69.63548731322468655, 62.62411233422432133, -13.34129631502566227 ) ) ;
#59660 = CARTESIAN_POINT ( 'NONE',  ( 184.3888951012362440, 288.9016753704191274, -13.18852512495808860 ) ) ;
#59662 = CARTESIAN_POINT ( 'NONE',  ( 169.7943624855302858, 249.0057814370864833, -4.764873173913280802 ) ) ;
#59663 = ORIENTED_EDGE ( 'NONE', *, *, #31411, .T. ) ;
#59664 = CARTESIAN_POINT ( 'NONE',  ( 64.01779381112929457, 207.7677522451418497, 10.00000000000009592 ) ) ;
#59665 = DIRECTION ( 'NONE',  ( -0.1344185706417126702, 0.9909246428798905715, 0.000000000000000000 ) ) ;
#59666 = EDGE_CURVE ( 'NONE', #74753, #5335, #93349, .T. ) ;
#59667 = CARTESIAN_POINT ( 'NONE',  ( 82.47313821142903123, 40.87591070147813355, -3.712110524942620948 ) ) ;
#59668 = CARTESIAN_POINT ( 'NONE',  ( 173.2640478233614374, 251.6539192559667413, -0.3386657152870858334 ) ) ;
#59669 = CARTESIAN_POINT ( 'NONE',  ( 42.45923888023187232, 122.5484010731363043, -10.00000000000000000 ) ) ;
#59670 = CARTESIAN_POINT ( 'NONE',  ( 71.88653196722606253, 72.25570330380722339, 3.269911192557279911 ) ) ;
#59671 = CARTESIAN_POINT ( 'NONE',  ( 82.69055213595072473, 42.56357957931876967, 6.360044358398685205 ) ) ;
#59672 = CARTESIAN_POINT ( 'NONE',  ( 126.5340026503663466, 243.8615022471902591, -10.00000000000009592 ) ) ;
#59673 = EDGE_CURVE ( 'NONE', #58450, #61729, #93400, .T. ) ;
#59674 = CARTESIAN_POINT ( 'NONE',  ( 80.74302285234506371, 53.94966248920944452, 15.73036127202275658 ) ) ;
#59675 = CARTESIAN_POINT ( 'NONE',  ( 206.5092799326709780, 271.9210634963550888, 7.392161875056491915 ) ) ;
#59676 = CIRCLE ( 'NONE', #98554, 0.1418229129681557177 ) ;
#59677 = CARTESIAN_POINT ( 'NONE',  ( 64.58612298413676456, 208.0958772461660544, -9.188101187500095079 ) ) ;
#59678 = CARTESIAN_POINT ( 'NONE',  ( 159.2102594322688844, 254.8867369075254885, -16.13039487917589199 ) ) ;
#59679 = CARTESIAN_POINT ( 'NONE',  ( 77.58957552442460326, 61.75793702469097468, 15.67560070342386602 ) ) ;
#59680 = CARTESIAN_POINT ( 'NONE',  ( 178.1650032105745538, 292.9353035937096479, -5.923887690835723419 ) ) ;
#59682 = CARTESIAN_POINT ( 'NONE',  ( 66.44743792946236738, 67.95054874496071307, 6.521299778128105018 ) ) ;
#59681 = AXIS2_PLACEMENT_3D ( 'NONE', #89904, #72711, #3301 ) ;
#59683 = EDGE_CURVE ( 'NONE', #5590, #49899, #18199, .T. ) ;
#59684 = VECTOR ( 'NONE', #39106, 1000.000000000000000 ) ;
#59685 = EDGE_CURVE ( 'NONE', #34673, #91537, #33909, .T. ) ;
#59686 = AXIS2_PLACEMENT_3D ( 'NONE', #99189, #82025, #14078 ) ;
#59687 = CARTESIAN_POINT ( 'NONE',  ( 207.4218731373931632, 271.3817724553659332, -5.249531240730909154 ) ) ;
#59688 = CARTESIAN_POINT ( 'NONE',  ( -110.0000000000000000, 0.000000000000000000, 59.99999999999999289 ) ) ;
#59690 = CARTESIAN_POINT ( 'NONE',  ( 185.8045553127517451, 265.6963936551481424, 13.19588143967888350 ) ) ;
#59689 = CARTESIAN_POINT ( 'NONE',  ( 73.45606387015448036, 70.03420106287664737, -9.568701002945239509 ) ) ;
#59691 = EDGE_CURVE ( 'NONE', #66505, #28484, #88151, .T. ) ;
#59692 = DIRECTION ( 'NONE',  ( 0.4803199113995043623, -0.8770933717188679202, 0.000000000000000000 ) ) ;
#59693 = EDGE_CURVE ( 'NONE', #20300, #77610, #8718, .T. ) ;
#59694 = DIRECTION ( 'NONE',  ( 0.000000000000000000, -0.000000000000000000, -1.000000000000000000 ) ) ;
#59695 = DIRECTION ( 'NONE',  ( -0.9186857246103535823, 0.3949892902309500298, 0.000000000000000000 ) ) ;
#59696 = CARTESIAN_POINT ( 'NONE',  ( 157.6394123119580968, 270.8627004967905805, -14.82514603415767063 ) ) ;
#59697 = CARTESIAN_POINT ( 'NONE',  ( 72.11463582380375215, 72.32045887020245800, 3.546959094384888100 ) ) ;
#59698 = CIRCLE ( 'NONE', #38657, 0.1418229129681539691 ) ;
#59699 = CARTESIAN_POINT ( 'NONE',  ( 27.50958393249801404, 180.5643266524160424, 9.188101187500095079 ) ) ;
#59700 = CARTESIAN_POINT ( 'NONE',  ( 196.0034224882197975, 291.1591091234520263, 17.53794140922627776 ) ) ;
#59701 = B_SPLINE_CURVE_WITH_KNOTS ( 'NONE', 3,
 ( #98916, #20421, #44675, #52778 ),
 .UNSPECIFIED., .F., .F.,
 ( 4, 4 ),
 ( 0.007301977675103129943, 0.01234114840196185066 ),
 .UNSPECIFIED. ) ;
#59702 = CARTESIAN_POINT ( 'NONE',  ( 200.1719577690460881, 277.9335415779574419, 15.23757986191821345 ) ) ;
#59703 = CARTESIAN_POINT ( 'NONE',  ( 164.6150166221017912, 248.5083581723461350, -9.597476261921807250 ) ) ;
#59704 = CARTESIAN_POINT ( 'NONE',  ( 71.54037008220826976, 72.37285432226113358, -1.295160433098011543 ) ) ;
#59705 = CARTESIAN_POINT ( 'NONE',  ( 54.03161192339643293, 195.8768266524159856, -9.188101187500093303 ) ) ;
#59706 = VECTOR ( 'NONE', #65582, 1000.000000000000000 ) ;
#59707 = CARTESIAN_POINT ( 'NONE',  ( 22.44070990177030112, 31.14336893147756413, 7.433330006724141015 ) ) ;
#59708 = CARTESIAN_POINT ( 'NONE',  ( 170.6125138170483524, 287.8455895967342144, 7.516220978703161748 ) ) ;
#59709 = CARTESIAN_POINT ( 'NONE',  ( -20.01016364259690050, 23.06595206263088116, 177.5919119679930134 ) ) ;
#59710 = CARTESIAN_POINT ( 'NONE',  ( 41.30863684418880410, 35.80066082961425167, 10.00000000000000533 ) ) ;
#59711 = CARTESIAN_POINT ( 'NONE',  ( 180.3600075739701651, 254.8198211655269176, -3.768796009823502047 ) ) ;
#59712 = CARTESIAN_POINT ( 'NONE',  ( 76.42791049025993289, 61.90737760121017885, 15.82173950495353232 ) ) ;
#59713 = ORIENTED_EDGE ( 'NONE', *, *, #23778, .F. ) ;
#59714 = CARTESIAN_POINT ( 'NONE',  ( 73.42682404930152984, 64.53156016964122443, 13.57139978262335234 ) ) ;
#59715 = CARTESIAN_POINT ( 'NONE',  ( 70.84057020560329931, 67.84468212244721030, -9.645047131074784730 ) ) ;
#59716 = B_SPLINE_SURFACE_WITH_KNOTS ( 'NONE', 3, 1, ( 
 ( #54254, #54767 ),
 ( #30483, #78600 ),
 ( #85749, #30975 ),
 ( #62872, #93830 ),
 ( #15770, #46676 ),
 ( #77603, #76589 ),
 ( #45665, #84723 ),
 ( #47172, #8188 ),
 ( #92329, #7174 ),
 ( #78093, #38060 ),
 ( #39056, #8684 ),
 ( #68974, #15263 ),
 ( #46158, #77077 ),
 ( #38572, #76897 ),
 ( #53105, #22208 ),
 ( #60682, #7001 ),
 ( #84060, #90667 ),
 ( #36903, #22714 ),
 ( #92164, #15091 ),
 ( #82571, #99223 ),
 ( #14116, #67304 ),
 ( #98231, #35907 ),
 ( #37887, #59182 ),
 ( #29809, #6009 ),
 ( #13133, #61195 ),
 ( #44994, #14616 ),
 ( #52103, #6518 ),
 ( #83551, #45494 ),
 ( #67815, #91146 ),
 ( #76428, #53594 ),
 ( #36399, #28816 ),
 ( #5515, #91641 ),
 ( #68796, #68300 ),
 ( #59700, #43991 ) ),
 .UNSPECIFIED., .T., .F., .F.,
 ( 4, 2, 2, 2, 2, 2, 2, 2, 2, 2, 2, 2, 2, 2, 2, 2, 4 ),
 ( 2, 2 ),
 ( 0.000000000000000000, 0.06250000000000000000, 0.1250000000000000000, 0.1875000000000000000, 0.2500000000000000000, 0.3125000000000000000, 0.3750000000000000000, 0.4375000000000000000, 0.5000000000000000000, 0.5625000000000000000, 0.6250000000000000000, 0.6875000000000000000, 0.7500000000000000000, 0.8125000000000000000, 0.8750000000000000000, 0.9375000000000000000, 1.000000000000000000 ),
 ( 0.000000000000000000, 1.000000000000000000 ),
 .UNSPECIFIED. ) ;
#59717 = CARTESIAN_POINT ( 'NONE',  ( 163.2851116495353665, 256.0038574147548616, -14.89960205689385120 ) ) ;
#59718 = CYLINDRICAL_SURFACE ( 'NONE', #54185, 10.00000000000010658 ) ;
#59719 = CARTESIAN_POINT ( 'NONE',  ( 90.08876690777121610, 229.4865022471902876, -10.00000000000009415 ) ) ;
#59720 = CARTESIAN_POINT ( 'NONE',  ( 200.4403816905005158, 283.4740703539914648, 16.81798557643505987 ) ) ;
#59721 = CARTESIAN_POINT ( 'NONE',  ( 164.9043417134678577, 286.5925546497160212, 0.04530247668140159611 ) ) ;
#59722 = EDGE_LOOP ( 'NONE', ( #43186, #13320, #45879, #99664 ) ) ;
#59723 = CARTESIAN_POINT ( 'NONE',  ( 53.67935523340274528, 210.9869531367911009, 4.594050593750046652 ) ) ;
#59724 = ORIENTED_EDGE ( 'NONE', *, *, #9240, .T. ) ;
#59725 = CARTESIAN_POINT ( 'NONE',  ( 164.4943844331201603, 264.4168344445729417, 16.69252833053101526 ) ) ;
#59726 = CARTESIAN_POINT ( 'NONE',  ( 190.8683709797118411, 300.0532792356709706, -4.461919767133968762 ) ) ;
#59727 = CARTESIAN_POINT ( 'NONE',  ( 82.63281508726200286, 40.94328431233920895, -3.617117793111275681 ) ) ;
#59728 = ORIENTED_EDGE ( 'NONE', *, *, #45697, .F. ) ;
#59729 = DIRECTION ( 'NONE',  ( -0.8660254037844379305, -0.5000000000000011102, 0.000000000000000000 ) ) ;
#59730 = CARTESIAN_POINT ( 'NONE',  ( 79.07447601446385477, 46.01053808348076046, -12.62649058706214511 ) ) ;
#59731 = DIRECTION ( 'NONE',  ( 0.8080546441192343332, -0.5891075386695858729, 0.000000000000000000 ) ) ;
#59732 = CARTESIAN_POINT ( 'NONE',  ( 72.96265021447784704, 70.35314760898533848, -8.120586438831022491 ) ) ;
#59733 = DIRECTION ( 'NONE',  ( 0.8660254037844390407, 0.4999999999999993339, 0.000000000000000000 ) ) ;
#59734 = CARTESIAN_POINT ( 'NONE',  ( 204.9134960529544287, 275.7264090101555212, 14.56629498631681408 ) ) ;
#59735 = VERTEX_POINT ( 'NONE', #46710 ) ;
#59736 = CARTESIAN_POINT ( 'NONE',  ( 25.69310950058095955, 17.76004757982089899, 5.678558825948272215 ) ) ;
#59737 = CARTESIAN_POINT ( 'NONE',  ( 26.58620497985335973, 27.30066082961423035, -10.00000000000000533 ) ) ;
#59738 = CARTESIAN_POINT ( 'NONE',  ( 175.5824964429158399, 254.0579991535531406, 8.209342937837284637 ) ) ;
#59739 = CARTESIAN_POINT ( 'NONE',  ( 75.22859809181653645, 66.95660471994222007, -12.79880029611497427 ) ) ;
#59740 = VERTEX_POINT ( 'NONE', #78130 ) ;
#59741 = LINE ( 'NONE', #73475, #95139 ) ;
#59742 = CARTESIAN_POINT ( 'NONE',  ( 167.0738366597983031, 261.5866074660107188, 16.40510134541907661 ) ) ;
#59743 = CARTESIAN_POINT ( 'NONE',  ( 206.1405152101578437, 273.6011494880188479, -9.618815605734603480 ) ) ;
#59744 = VERTEX_POINT ( 'NONE', #39090 ) ;
#59746 = CARTESIAN_POINT ( 'NONE',  ( 61.41971759977600698, 196.2677522451418213, -5.000000000000041744 ) ) ;
#59745 = CARTESIAN_POINT ( 'NONE',  ( 159.7553372911454233, 283.1775518570184431, -3.360441317989244947 ) ) ;
#59747 = CARTESIAN_POINT ( 'NONE',  ( 207.6067494229581314, 271.0615573356529353, -1.924113146155245868 ) ) ;
#59748 = CARTESIAN_POINT ( 'NONE',  ( 66.23237210115183871, 68.64930917983895142, -2.151527110974545298 ) ) ;
#59749 = CARTESIAN_POINT ( 'NONE',  ( 198.3150362131025588, 287.1552767044814800, 18.53472937702030521 ) ) ;
#59750 = LINE ( 'NONE', #21276, #11133 ) ;
#59751 = CARTESIAN_POINT ( 'NONE',  ( 162.1286899612119612, 263.6308679106482487, -16.92993415948811986 ) ) ;
#59753 = ADVANCED_FACE ( 'NONE', ( #95238 ), #618, .F. ) ;
#59752 = CARTESIAN_POINT ( 'NONE',  ( 128.2121871902485566, 235.6423013555409796, -4.594050593750043987 ) ) ;
#59754 = VECTOR ( 'NONE', #32035, 1000.000000000000000 ) ;
#59755 = FACE_OUTER_BOUND ( 'NONE', #20510, .T. ) ;
#59756 = VERTEX_POINT ( 'NONE', #80533 ) ;
#59757 = FACE_OUTER_BOUND ( 'NONE', #63144, .T. ) ;
#59758 = FACE_OUTER_BOUND ( 'NONE', #38985, .T. ) ;
#59759 = VERTEX_POINT ( 'NONE', #69003 ) ;
#59760 = VECTOR ( 'NONE', #24547, 1000.000000000000000 ) ;
#59761 = DIRECTION ( 'NONE',  ( 0.9954067278227227700, -0.09573633691164462611, 0.000000000000000000 ) ) ;
#59762 = VERTEX_POINT ( 'NONE', #99931 ) ;
#59763 = ORIENTED_EDGE ( 'NONE', *, *, #98811, .F. ) ;
#59764 = CARTESIAN_POINT ( 'NONE',  ( 81.69914580506154778, 224.6427522451419065, 10.00000000000009415 ) ) ;
#59765 = CARTESIAN_POINT ( 'NONE',  ( 75.32358509735726670, 66.62760184127506591, -13.06371402686526473 ) ) ;
#59766 = CARTESIAN_POINT ( 'NONE',  ( 195.3630008912252549, 285.3603474548959298, 16.99413665511329086 ) ) ;
#59767 = EDGE_CURVE ( 'NONE', #12230, #52681, #30516, .T. ) ;
#59768 = CARTESIAN_POINT ( 'NONE',  ( -31.31209261750204931, 96.33089062496601684, 12.38423361974427372 ) ) ;
#59769 = CARTESIAN_POINT ( 'NONE',  ( 81.89559477234445239, 55.33976261442212774, 16.26127046582525892 ) ) ;
#59770 = CARTESIAN_POINT ( 'NONE',  ( 194.1153812227096864, 294.4292925221022870, 15.54001482840963710 ) ) ;
#59771 = CARTESIAN_POINT ( 'NONE',  ( 72.38282305304500142, 69.07686135063536881, 9.305092211891095033 ) ) ;
#59772 = EDGE_CURVE ( 'NONE', #13298, #22379, #8666, .T. ) ;
#59773 = ORIENTED_EDGE ( 'NONE', *, *, #46049, .F. ) ;
#59774 = AXIS2_PLACEMENT_3D ( 'NONE', #74302, #59034, #41867 ) ;
#59775 = CARTESIAN_POINT ( 'NONE',  ( 73.64227373014415434, 63.39856954260761057, -14.21043620611602698 ) ) ;
#59776 = DIRECTION ( 'NONE',  ( -0.6118251767726359258, -0.7909930170786165782, 0.000000000000000000 ) ) ;
#59777 = DIRECTION ( 'NONE',  ( 0.3595896960900372696, 0.9331105242498740626, 0.000000000000000000 ) ) ;
#59778 = VERTEX_POINT ( 'NONE', #66779 ) ;
#59779 = CARTESIAN_POINT ( 'NONE',  ( 71.70884033504357546, 69.86088245213113623, -7.641946344699698024 ) ) ;
#59780 = CARTESIAN_POINT ( 'NONE',  ( 76.04814661432739342, 51.39648587280629499, -16.15155320745066803 ) ) ;
#59781 = CARTESIAN_POINT ( 'NONE',  ( 164.1943448329197395, 246.6690389504045413, 4.590013871137070822 ) ) ;
#59782 = B_SPLINE_CURVE_WITH_KNOTS ( 'NONE', 3,
 ( #16642, #88111, #71869, #78466, #87122, #94188, #9567, #79990, #94683, #47537, #33347, #2981, #18662, #70855, #39920, #40921, #78981, #64246, #24741, #41943, #17140, #72878, #95707, #9050, #72374, #79494, #48037, #2467, #3470, #34347, #96188, #33873, #56643, #1464, #40429, #10056, #26255, #57130, #32840, #26748, #32344, #95196, #10558, #25768, #87626, #49541 ),
 .UNSPECIFIED., .F., .F.,
 ( 4, 1, 1, 1, 2, 2, 1, 1, 1, 2, 2, 1, 1, 2, 2, 1, 1, 2, 2, 1, 1, 2, 2, 1, 2, 2, 1, 2, 2, 4 ),
 ( 0.000000000000000000, 0.06249999999996047606, 0.09374999999994101940, 0.1093749999999315409, 0.1171874999999289180, 0.1249999999999263089, 0.1874999999998932521, 0.2187499999998767930, 0.2343749999998704092, 0.2421874999998690769, 0.2499999999998677724, 0.3124999999998596123, 0.3437499999998554490, 0.3593749999998534506, 0.3749999999998514522, 0.4374999999998536726, 0.4687499999998547828, 0.4843749999998554490, 0.4999999999998561151, 0.5624999999998625544, 0.5937499999998642197, 0.6093749999998666622, 0.6249999999998691047, 0.6874999999998885336, 0.7187499999998983036, 0.7499999999999080735, 0.8124999999999311662, 0.8437499999999426015, 0.8749999999999540368, 1.000000000000000000 ),
 .UNSPECIFIED. ) ;
#59783 = CARTESIAN_POINT ( 'NONE',  ( 193.6564271169084464, 262.6014873983580742, -4.146719891036213745 ) ) ;
#59784 = AXIS2_PLACEMENT_3D ( 'NONE', #39863, #77407, #8499 ) ;
#59785 = CARTESIAN_POINT ( 'NONE',  ( 195.1154436510188077, 279.2972436967689873, 16.36790060704208116 ) ) ;
#59786 = CARTESIAN_POINT ( 'NONE',  ( 164.4678285797544106, 245.7803600197737524, -6.875991496205872799 ) ) ;
#59787 = CARTESIAN_POINT ( 'NONE',  ( 130.4037065759891334, 258.3464784336661637, 1.353441290958777327E-15 ) ) ;
#59788 = ORIENTED_EDGE ( 'NONE', *, *, #62772, .T. ) ;
#59789 = CARTESIAN_POINT ( 'NONE',  ( -0.6995629222973920314, 163.7365022471902023, -10.00000000000009237 ) ) ;
#59790 = CARTESIAN_POINT ( 'NONE',  ( 183.8210692855788864, 257.9504670327482927, 6.873620218444065344 ) ) ;
#59791 = LINE ( 'NONE', #76509, #31866 ) ;
#59792 = FACE_OUTER_BOUND ( 'NONE', #10328, .T. ) ;
#59793 = CARTESIAN_POINT ( 'NONE',  ( 185.8492146212669240, 258.6745004276652935, -5.862532207920108540 ) ) ;
#59794 = ORIENTED_EDGE ( 'NONE', *, *, #83368, .F. ) ;
#59795 = CARTESIAN_POINT ( 'NONE',  ( 76.16668535934209672, 53.10184382116266022, 15.96041101260095907 ) ) ;
#59796 = DIRECTION ( 'NONE',  ( -0.4999999999999995004, 0.8660254037844389297, -1.249000902703319567E-14 ) ) ;
#59797 = ADVANCED_FACE ( 'NONE', ( #12602 ), #27790, .T. ) ;
#59798 = CARTESIAN_POINT ( 'NONE',  ( 167.6136624610167019, 249.2005778497498341, -6.016629856180416347 ) ) ;
#59799 = CARTESIAN_POINT ( 'NONE',  ( 79.67161915667092842, 46.83867530445827043, 12.95308866772764311 ) ) ;
#59800 = CARTESIAN_POINT ( 'NONE',  ( 73.66290725793270155, 69.32596597699954089, -9.966140398900341424 ) ) ;
#59801 = ADVANCED_FACE ( 'NONE', ( #20692 ), #19846, .T. ) ;
#59802 = CARTESIAN_POINT ( 'NONE',  ( 147.5693121967435957, 275.0494489676833041, 4.210973343677100189 ) ) ;
#59803 = ADVANCED_FACE ( 'NONE', ( #23652 ), #52562, .T. ) ;
#59804 = CARTESIAN_POINT ( 'NONE',  ( 186.5492813281628912, 282.5551454570558008, 16.18981372509010797 ) ) ;
#59805 = CARTESIAN_POINT ( 'NONE',  ( 205.0520875136525376, 275.4863615587311756, -14.16385635411862509 ) ) ;
#59806 = CARTESIAN_POINT ( 'NONE',  ( 194.3107701606939486, 269.6703757554475942, 12.05248313980574615 ) ) ;
#59807 = ADVANCED_FACE ( 'NONE', ( #21683 ), #46451, .F. ) ;
#59808 = EDGE_CURVE ( 'NONE', #93198, #68897, #39862, .T. ) ;
#59809 = CARTESIAN_POINT ( 'NONE',  ( 17.99199860517156324, 32.16126292948895582, -6.180339887498951690 ) ) ;
#59810 = CARTESIAN_POINT ( 'NONE',  ( 190.1190668544949460, 301.3511120508678118, 4.410340539513557090 ) ) ;
#59811 = CARTESIAN_POINT ( 'NONE',  ( 172.0910100529608258, 260.0785035667472584, 15.53398388876759206 ) ) ;
#59812 = LINE ( 'NONE', #60792, #90396 ) ;
#59813 = B_SPLINE_CURVE_WITH_KNOTS ( 'NONE', 3,
 ( #69394, #24298, #30394, #92249, #22799, #53678, #15173, #46074, #76986, #1999, #87168, #87670, #57677, #88656, #2510, #96734, #32885, #79543, #48603, #71409, #3515, #10100, #71909, #65291, #80539, #63788, #33393, #19221, #34392, #88156, #18205, #56687, #89166, #49098, #41474, #3026, #11611, #41988, #96232, #64295, #11118, #48085, #50092, #33915, #9615, #80033, #26301, #57177 ),
 .UNSPECIFIED., .F., .F.,
 ( 4, 2, 2, 2, 2, 2, 2, 2, 2, 2, 2, 2, 2, 2, 2, 2, 2, 2, 2, 2, 2, 2, 2, 4 ),
 ( 0.0007190175845426069901, 0.0009287040927872296453, 0.001138390601031852301, 0.001243233855154209436, 0.001348077109276566788, 0.001557763617521332015, 0.001977136634010862037, 0.002396509650500392493, 0.003235255683479394857, 0.004074001716458396788, 0.004912747749437398719, 0.005332120765926939149, 0.005541807274171669899, 0.005646650528294073004, 0.005699072155355274123, 0.005751493782416475242, 0.005856337036538874011, 0.005961180290661273647, 0.006170866798906022611, 0.006590239815395467632, 0.006799926323640210525, 0.007009612831884953418, 0.007219299340129695444, 0.007428985848374438337 ),
 .UNSPECIFIED. ) ;
#59814 = CARTESIAN_POINT ( 'NONE',  ( 197.9952413503812352, 287.7091776547143809, 17.17611241386010690 ) ) ;
#59815 = CARTESIAN_POINT ( 'NONE',  ( 161.3042361785515197, 251.2598627930960333, 13.07175971676398341 ) ) ;
#59816 = CARTESIAN_POINT ( 'NONE',  ( -3.667330603741788320, 162.5643266524160140, 9.188101187500095079 ) ) ;
#59817 = CARTESIAN_POINT ( 'NONE',  ( 175.7917838780750799, 285.8274689740071608, -11.81341207233009705 ) ) ;
#59818 = VERTEX_POINT ( 'NONE', #84025 ) ;
#59819 = CIRCLE ( 'NONE', #85796, 17.82106496071138224 ) ;
#59820 = CARTESIAN_POINT ( 'NONE',  ( 66.83424962952723547, 68.16180659050830570, -6.545639671669595927 ) ) ;
#59821 = CARTESIAN_POINT ( 'NONE',  ( 73.08532603445986808, 70.49974493736067416, -7.999444584973850247 ) ) ;
#59822 = CARTESIAN_POINT ( 'NONE',  ( 198.8570476668614049, 286.2164853282868080, -17.01721544293231858 ) ) ;
#59824 = CARTESIAN_POINT ( 'NONE',  ( 6.480970727150832111, 183.7369531367911009, -4.594050593750048428 ) ) ;
#59823 = B_SPLINE_CURVE_WITH_KNOTS ( 'NONE', 3,
 ( #2284, #31144, #77781, #70657 ),
 .UNSPECIFIED., .F., .F.,
 ( 4, 4 ),
 ( 0.01157169839800022484, 0.01758127579506474358 ),
 .UNSPECIFIED. ) ;
#59825 = CARTESIAN_POINT ( 'NONE',  ( 181.7611970338358560, 276.1868128385311252, -16.62830721219069119 ) ) ;
#59826 = CARTESIAN_POINT ( 'NONE',  ( 30.82187231905848535, 18.76426979415091267, 3.090169943749476733 ) ) ;
#59827 = CARTESIAN_POINT ( 'NONE',  ( 85.59998877908455484, 48.66343243370425142, 12.43629469118824638 ) ) ;
#59828 = CARTESIAN_POINT ( 'NONE',  ( 170.2912665166379611, 270.8011127091891126, -16.89563538064900428 ) ) ;
#59829 = DIRECTION ( 'NONE',  ( -0.6778389383370750920, -0.7352104281592222179, 0.000000000000000000 ) ) ;
#59830 = CARTESIAN_POINT ( 'NONE',  ( -22.42236680055709641, 157.8615022471902591, 0.000000000000000000 ) ) ;
#59832 = CARTESIAN_POINT ( 'NONE',  ( 75.78130554586795142, 207.8927522451417929, -10.00000000000009059 ) ) ;
#59831 = CARTESIAN_POINT ( 'NONE',  ( 21.22170510744830096, 176.3927522451418213, -10.00000000000009237 ) ) ;
#59833 = CARTESIAN_POINT ( 'NONE',  ( 176.7457436420401677, 254.2668712825680188, -3.870637407069959401 ) ) ;
#59834 = CARTESIAN_POINT ( 'NONE',  ( 198.5386315514599858, 286.7679982181109608, 17.03868888912368718 ) ) ;
#59835 = EDGE_CURVE ( 'NONE', #95312, #8176, #38982, .T. ) ;
#59836 = AXIS2_PLACEMENT_3D ( 'NONE', #54958, #95016, #17467 ) ;
#59837 = CARTESIAN_POINT ( 'NONE',  ( 60.28305926085685229, 195.6115022471902023, -5.000000000000041744 ) ) ;
#59838 = CARTESIAN_POINT ( 'NONE',  ( -13.11024591527734451, 0.000000000000000000, 45.00000000000000000 ) ) ;
#59839 = CARTESIAN_POINT ( 'NONE',  ( 119.0307608796806278, 227.9824982072973683, 3.021315404115420679E-15 ) ) ;
#59840 = CARTESIAN_POINT ( 'NONE',  ( 17.65854496445001232, 174.8768266524159856, -9.188101187500091527 ) ) ;
#59841 = CARTESIAN_POINT ( 'NONE',  ( 167.7210762313646910, 287.2684685992639402, 4.983143766097549943 ) ) ;
#59842 = EDGE_CURVE ( 'NONE', #18980, #13449, #77584, .T. ) ;
#59843 = CARTESIAN_POINT ( 'NONE',  ( 192.6797324865049745, 296.9159090750308110, 12.42053959885222625 ) ) ;
#59844 = CARTESIAN_POINT ( 'NONE',  ( 45.61829935282815995, 28.19860640527296525, 2.839279412974134775 ) ) ;
#59845 = CARTESIAN_POINT ( 'NONE',  ( 165.9969153545198708, 246.1123342570000716, -1.176638740111072723 ) ) ;
#59846 = CARTESIAN_POINT ( 'NONE',  ( 207.4764081617721843, 271.2873150223495600, 6.359972247200924578 ) ) ;
#59847 = CARTESIAN_POINT ( 'NONE',  ( 186.8874022707183826, 267.3628004192088383, 13.25673146551773129 ) ) ;
#59848 = CARTESIAN_POINT ( 'NONE',  ( 153.2978239650968533, 265.5538651647430584, -16.15457164513478006 ) ) ;
#59849 = CARTESIAN_POINT ( 'NONE',  ( 160.1502792044530850, 280.1323723417889369, 9.307031849721941086 ) ) ;
#59850 = CARTESIAN_POINT ( 'NONE',  ( 17.37926562425035826, 12.96004757982088762, -5.678558825948276656 ) ) ;
#59851 = CARTESIAN_POINT ( 'NONE',  ( -12.68721568607400485, 24.67147432707382748, 10.00000000000000000 ) ) ;
#59852 = CARTESIAN_POINT ( 'NONE',  ( -22.42236680055709641, 157.8615022471902591, 0.000000000000000000 ) ) ;
#59853 = AXIS2_PLACEMENT_3D ( 'NONE', #34779, #27202, #58090 ) ;
#59854 = CARTESIAN_POINT ( 'NONE',  ( 71.41016749218992743, 59.45273978182969188, 15.19346469599747174 ) ) ;
#59855 = CARTESIAN_POINT ( 'NONE',  ( 194.3799873100184641, 293.9709813348915191, 15.33105633561973669 ) ) ;
#59856 = ORIENTED_EDGE ( 'NONE', *, *, #31778, .F. ) ;
#59857 = CARTESIAN_POINT ( 'NONE',  ( 183.4752222048318515, 289.9104771362203792, 12.19711425367773394 ) ) ;
#59858 = CARTESIAN_POINT ( 'NONE',  ( 174.5885488454506174, 256.4458599265808516, 12.05082362884263425 ) ) ;
#59859 = CARTESIAN_POINT ( 'NONE',  ( 81.14314822843688546, 42.42749270467351153, 7.695795501257847171 ) ) ;
#59860 = ORIENTED_EDGE ( 'NONE', *, *, #32475, .F. ) ;
#59861 = CARTESIAN_POINT ( 'NONE',  ( -23.47208873469913115, 24.42380372261332155, 10.00000000000000000 ) ) ;
#59862 = CARTESIAN_POINT ( 'NONE',  ( -13.11024591527734451, 27.99999999999999645, 48.00000000000000000 ) ) ;
#59863 = CARTESIAN_POINT ( 'NONE',  ( 76.70949559664001072, 63.86342103896397759, 14.86793590975532631 ) ) ;
#59864 = CARTESIAN_POINT ( 'NONE',  ( 203.1705638993064156, 278.7452560544191442, -15.08126533799095093 ) ) ;
#59865 = EDGE_LOOP ( 'NONE', ( #67477, #93891, #76224, #84592 ) ) ;
#59866 = ORIENTED_EDGE ( 'NONE', *, *, #91965, .T. ) ;
#59868 = CARTESIAN_POINT ( 'NONE',  ( -23.47208873469913470, 24.42380372261331800, -10.00000000000000000 ) ) ;
#59867 = DIRECTION ( 'NONE',  ( 0.4924038765061026779, -0.8528685319524446085, -0.1736481776669273058 ) ) ;
#59869 = CARTESIAN_POINT ( 'NONE',  ( 152.6992418905140028, 266.1641500988167763, 17.27767170937316621 ) ) ;
#59870 = ORIENTED_EDGE ( 'NONE', *, *, #20842, .T. ) ;
#59871 = CARTESIAN_POINT ( 'NONE',  ( 190.7779368023172708, 300.2099158256590385, 8.142228434510803581 ) ) ;
#59872 = CARTESIAN_POINT ( 'NONE',  ( 80.25077290097513583, 58.18867766503439043, -16.60702595570231566 ) ) ;
#59873 = PLANE ( 'NONE',  #45102 ) ;
#59874 = EDGE_LOOP ( 'NONE', ( #34649, #1947, #76716, #42217 ) ) ;
#59875 = CARTESIAN_POINT ( 'NONE',  ( 78.04299808706751662, 61.03337783168321096, -15.88841590149242222 ) ) ;
#59876 = ADVANCED_FACE ( 'NONE', ( #19098 ), #82177, .T. ) ;
#59877 = CARTESIAN_POINT ( 'NONE',  ( 81.08217831220640903, 43.07020448918126476, 9.543463939025171427 ) ) ;
#59878 = EDGE_LOOP ( 'NONE', ( #62372, #4187, #35096, #65609 ) ) ;
#59879 = CARTESIAN_POINT ( 'NONE',  ( 13.90223112049948639, 33.06302660730328569, -10.00000000000000000 ) ) ;
#59880 = LINE ( 'NONE', #21400, #10590 ) ;
#59881 = VERTEX_POINT ( 'NONE', #44845 ) ;
#59882 = CARTESIAN_POINT ( 'NONE',  ( 177.5916152172162299, 279.2165670549423453, -16.08229183096581139 ) ) ;
#59883 = CARTESIAN_POINT ( 'NONE',  ( 172.1850212007017262, 264.1675647692185294, -16.02513241725109339 ) ) ;
#59884 = VERTEX_POINT ( 'NONE', #99077 ) ;
#59885 = EDGE_CURVE ( 'NONE', #1543, #39441, #85735, .T. ) ;
#59886 = CARTESIAN_POINT ( 'NONE',  ( 158.5760999176972632, 274.9853568892722819, -13.72891502304694633 ) ) ;
#59887 = DIRECTION ( 'NONE',  ( -0.8660254037844378194, -0.5000000000000013323, -0.000000000000000000 ) ) ;
#59888 = PLANE ( 'NONE',  #14304 ) ;
#59889 = ORIENTED_EDGE ( 'NONE', *, *, #84509, .T. ) ;
#59890 = EDGE_CURVE ( 'NONE', #76483, #89630, #6086, .T. ) ;
#59891 = CARTESIAN_POINT ( 'NONE',  ( 156.6755709933906076, 266.6679220207594767, -16.20175030095106905 ) ) ;
#59892 = CARTESIAN_POINT ( 'NONE',  ( 147.2494378675467033, 275.6034875578896504, 3.639370109197119341 ) ) ;
#59893 = CARTESIAN_POINT ( 'NONE',  ( 206.9942764641839688, 270.1223916185117560, -3.431663675821580828 ) ) ;
#59894 = CARTESIAN_POINT ( 'NONE',  ( 190.0607312434325138, 301.4521522931182176, 3.538147641957853473 ) ) ;
#59895 = CARTESIAN_POINT ( 'NONE',  ( 192.6470966816805230, 296.9724359471326807, 11.11268290051284424 ) ) ;
#59897 = CARTESIAN_POINT ( 'NONE',  ( 191.8398273019305691, 298.3706675282543301, 9.207119386290592900 ) ) ;
#59896 = VECTOR ( 'NONE', #67210, 1000.000000000000114 ) ;
#59898 = CARTESIAN_POINT ( 'NONE',  ( 147.0660117096331874, 275.9211909828330249, -0.7354350123930680772 ) ) ;
#59899 = ORIENTED_EDGE ( 'NONE', *, *, #64637, .T. ) ;
#59900 = CARTESIAN_POINT ( 'NONE',  ( 74.38854607822595710, 57.91757908437448776, -15.94610812356584262 ) ) ;
#59901 = CARTESIAN_POINT ( 'NONE',  ( 164.9103019330012216, 245.0139736909548560, 2.841678961959298810 ) ) ;
#59902 = PLANE ( 'NONE',  #75845 ) ;
#59903 = CARTESIAN_POINT ( 'NONE',  ( -17.42236680055705023, 149.2012482093457777, 0.000000000000000000 ) ) ;
#59904 = CARTESIAN_POINT ( 'NONE',  ( 168.0314348872740311, 286.7485367448098827, 3.530950783189123587 ) ) ;
#59905 = DIRECTION ( 'NONE',  ( 0.000000000000000000, 0.000000000000000000, 1.000000000000000000 ) ) ;
#59906 = VERTEX_POINT ( 'NONE', #84392 ) ;
#59907 = CARTESIAN_POINT ( 'NONE',  ( 149.1183742800849643, 272.3663947352575860, -12.92061183374618238 ) ) ;
#59908 = CARTESIAN_POINT ( 'NONE',  ( 76.40818250836743175, 54.09807576519859396, -16.06719028116590309 ) ) ;
#59909 = CARTESIAN_POINT ( 'NONE',  ( 148.9047129658783319, 273.1746572624253986, 9.419085927755277865 ) ) ;
#59910 = CARTESIAN_POINT ( 'NONE',  ( 79.49157516048417449, 46.35107416014648152, 12.69267528992099869 ) ) ;
#59911 = CARTESIAN_POINT ( 'NONE',  ( 182.4816129607276025, 284.1573356931687044, -15.00314700627625975 ) ) ;
#59912 = CARTESIAN_POINT ( 'NONE',  ( 76.20052385246813742, 55.90692255230084129, -16.60794131075797608 ) ) ;
#59913 = VECTOR ( 'NONE', #12229, 1000.000000000000000 ) ;
#59914 = ORIENTED_EDGE ( 'NONE', *, *, #34381, .F. ) ;
#59915 = CARTESIAN_POINT ( 'NONE',  ( 163.4139553296302267, 247.6057220337265505, -10.31482883765270842 ) ) ;
#59916 = CARTESIAN_POINT ( 'NONE',  ( 83.34650525046124869, 42.68055930881851623, 6.999721904327397937 ) ) ;
#59917 = EDGE_CURVE ( 'NONE', #82871, #68558, #64970, .T. ) ;
#59918 = CARTESIAN_POINT ( 'NONE',  ( 155.3072241301414067, 262.2133070116863109, 17.03827534033916535 ) ) ;
#59919 = CARTESIAN_POINT ( 'NONE',  ( 56.22356517706937495, 193.2677522451418213, -5.000000000000041744 ) ) ;
#59920 = CARTESIAN_POINT ( 'NONE',  ( 112.6505328941731108, 235.8458772461660544, 9.188101187500095079 ) ) ;
#59921 = CARTESIAN_POINT ( 'NONE',  ( 199.0756812798354645, 285.8378008023734083, -18.45377816087746936 ) ) ;
#59922 = LINE ( 'NONE', #92370, #48124 ) ;
#59923 = CARTESIAN_POINT ( 'NONE',  ( -23.32062891409032090, 78.77562236714182120, 59.99999999999999289 ) ) ;
#59924 = CARTESIAN_POINT ( 'NONE',  ( 33.92367135321775606, 181.2048013555409796, 4.594050593750051981 ) ) ;
#59925 = DIRECTION ( 'NONE',  ( 0.000000000000000000, -0.000000000000000000, -1.000000000000000000 ) ) ;
#59926 = ORIENTED_EDGE ( 'NONE', *, *, #16721, .T. ) ;
#59927 = CARTESIAN_POINT ( 'NONE',  ( 195.1474640768281290, 265.6393084148356252, -8.887799905196541062 ) ) ;
#59928 = CARTESIAN_POINT ( 'NONE',  ( 181.5271692362856015, 267.5257140134757492, 14.92964428755297135 ) ) ;
#59929 =( BOUNDED_SURFACE ( )  B_SPLINE_SURFACE ( 1, 2, ( 
 ( #89052, #90518, #5371, #12993, #37737, #44350, #29172, #82907, #75781, #52451, #38227, #22555, #7345, #76277, #22052, #91489, #51461, #52952, #60536, #14464, #45828, #69143, #45346, #100072, #59539, #53440, #74793, #30659, #6851, #30150, #61542, #67157, #51967, #36254, #76751, #21090, #13479, #68647, #75281, #13965, #68150, #99567, #61035, #84391, #5865, #36750, #92008, #92485, #83902, #82427, #14937, #67659, #98078, #43852, #28656, #98589, #60040, #91006, #6367, #83396, #21568, #44844, #37251, #99076, #29659, #63048, #23032, #93992, #32140, #86409, #17450, #79306, #16940, #40733, #31132, #94485, #46326, #9875, #47826, #1769, #71678, #38738, #23530, #7859, #48358, #62025, #54421, #40230, #85398, #85918, #39715, #78765, #9352, #55920, #92976, #8355, #63544, #2269, #24542, #33151, #55422, #15945, #71172, #53925, #32648, #64051, #86913, #16444, #8845, #25044, #1258, #39224, #84888, #15428, #77251, #47340, #69644, #252, #62527, #46848, #77770, #70131, #744, #31628, #93488, #24046, #54941, #78264, #70643, #57944, #73174, #27062, #74170, #26563, #64558, #88927, #42235, #4762, #96492, #72686, #56446, #66051, #34646, #65546, #96999, #96003, #3278, #41741, #18976, #80295, #49850, #81295, #48867, #11868, #10365, #87439, #3764, #80812, #17972, #57439, #42724, #79800, #41233, #19487, #50343, #73662, #72172, #2778, #4240, #95517, #35644, #33666, #11385, #58434, #35140, #26063, #94995, #88416, #34161, #43228, #56940, #25558, #87926, #27568, #10866, #89409, #18468, #49355, #19960, #50837, #65053, #81787, #12362, #28532, #84281, #68036, #6235, #98957, #59415, #82301, #59924, #37619, #75162, #7223, #5250, #76165, #5737, #45228, #99453, #36624, #67033, #29541, #60413, #76638, #83271, #29056, #91880, #91369, #21932, #52822, #30029, #45715, #83778, #60913, #68530, #66545, #13839, #22433, #37129, #98462, #43730, #53325, #67533, #14339, #90894, #13359, #6742, #14826, #97473, #28039, #89885, #44715, #90395, #58914, #20459, #51333, #21444, #12871, #74673, #36130, #20970, #52330, #51852, #82793, #44224, #75649, #94371, #22921, #63433, #79177, #92862, #54820, #46725, #139, #38107, #31515, #39105, #78146, #32539, #69020, #55309, #17325, #31022, #85800, #40113, #92373, #1140, #8732, #9233, #30534, #47712, #24926, #24434, #61914, #23416, #48231, #15821, #71052, #46207, #99950, #61421, #54306, #1654, #39604, #7731, #32017, #69528, #62926, #70524, #77124, #85274, #84772, #53808, #15308, #55800, #38619, #77653, #8239, #86792, #70019, #635, #62409, #93365, #23922, #16330, #47224, #93877, #86291, #16825, #78650, #49725, #5499, #9756, #28286, #90650, #72045, #57320, #13116, #63927, #74427, #80682, #82551, #2146, #20710, #36382, #97718, #33536, #2649, #21208, #87806, #43975, #17847, #52088, #40616, #64435, #74917, #11257, #79679, #5011, #41111, #35891, #43483, #48748, #95395, #56319, #94866, #71550, #67286, #10741, #18348, #59677, #10242, #33027, #25950, #98213, #56823, #66793, #25424, #87313, #72561, #59162, #49241, #80176, #90136, #41616, #28797, #51597, #3164, #34050, #64939, #95883, #26444, #88292, #18846, #23666, #21696, #92624, #91622, #61674, #15565, #22192, #83533, #15074, #45963, #93114, #99702, #45477, #8001, #76880, #7476, #69284, #46468, #62165, #84530, #77398, #85021, #83034, #30290, #38876, #53575, #14598, #60167, #54066, #53086, #30795, #84040, #29791, #100209, #69780, #13605, #23174, #5993, #61178, #14097, #44478, #22698, #38371, #76411, #98721, #389, #75409, #31277, #6984, #92145, #68284, #36887, #67796, #29305, #37869, #91132, #52579, #68779, #44979, #75920, #6501, #37378, #99205, #60663, #87053, #95135, #94126, #78403, #17588, #32777, #48494, #64694, #86547, #24188, #79435, #1897, #95646, #56060, #32279, #16083, #25700, #94623, #25180, #56580, #55563, #63183, #1400, #78914, #39855, #9500, #40862, #8491, #71809, #70275, #46989, #63686, #40366, #77905, #17078, #2406, #39361, #886, #10000, #33284, #64186, #31765, #62669, #87567, #55071, #54558, #93621, #71305, #48994, #79930, #86057, #85542, #2918, #10490, #16583, #47479, #8984, #41372, #70790, #24681, #47968, #72311, #27195, #13006, #97610, #82443, #50972, #97133, #66187, #26193, #27700, #35281, #89540, #20593, #43866, #20101, #74808, #34287, #28178, #49480, #5386, #81924, #4898, #36272, #41883, #26686, #11010, #51476, #65184, #57574, #43369, #88547, #89064, #42856, #12500, #74316, #59049, #96132, #11512, #66676, #67171, #58568, #57072, #35782, #19113, #90021, #88053, #18601, #80436, #72821, #19616, #11999, #3413, #49989, #80944, #42366, #73300, #3891, #34773, #65674, #73792, #96629, #58084, #50474, #81427, #4381, #14951, #36765, #51981, #59555, #84406, #91018, #75796, #29187, #22071, #99090, #84901, #69157, #53943, #22569, #68659, #37754, #98094, #99582, #6864, #61050, #92500, #15442, #92023, #46341, #5879, #100087, #82920, #77264, #53455, #76763, #7876, #13496, #98604, #44366, #23045, #67675, #60055, #45841, #21581, #60549, #14479, #7358, #38242, #30674, #52466, #83411, #61554, #38753, #30166, #28672, #90532, #13981, #75298, #44856, #6382, #37265, #68164, #91506, #83917, #29674, #76292, #52966, #45360, #85410, #46862, #23544, #77784, #15959, #92990, #8371, #265, #69656, #31146, #62037, #54435, #97220, #4997, #3984, #88649, #27789, #42953, #58662, #43961, #96728, #34386, #89634, #12091, #74899, #66287, #42464, #26295, #35874, #4482, #35376, #66778, #65770, #73398, #11605, #89160, #50085, #19706, #51066, #18698, #82026, #80532, #57170, #73893, #50572, #88150, #27293, #12601, #49579, #11112, #20196, #43468, #34870, #74412, #58175, #81522, #97703, #90117, #5484, #28271, #41981, #59147, #96225, #64797, #20691, #51580, #82537, #72918, #13101, #95742, #3509, #65284, #26789, #81042, #57671, #19215, #55094, #84065, #24213, #41264, #53597, #15591, #7498, #61199, #99226, #92647, #100229, #38898, #93648, #29813, #16110, #79827, #92167, #46492, #912, #53109, #62189, #69802, #70301, #91644, #8515, #86081, #85566, #22718, #84555, #10395, #76900, #31790 ),
 ( #54584, #38396, #60686, #76431, #62692, #22211, #93140, #18001, #31301, #39384, #69308, #15094, #23689, #77426, #47009, #14619, #30815, #68799, #77923, #8025, #45498, #412, #61695, #7004, #48893, #37891, #99727, #30313, #23196, #54088, #45984, #85042, #57466, #27095, #58464, #26094, #89436, #87953, #33700, #81328, #57978, #64593, #3793, #19990, #95545, #56968, #11898, #97029, #35172, #18498, #49384, #65081, #82334, #49883, #74206, #80329, #12903, #72207, #26593, #43261, #73689, #41773, #66083, #3310, #27598, #4273, #10896, #96031, #72719, #34189, #2811, #66578, #73199, #80842, #20495, #88450, #19009, #11412, #4796, #42266, #42757, #34675, #65577, #96525, #50870, #88960, #19515, #81820, #50375, #89915, #12395, #35677, #97502, #28071, #58944, #51367, #14858, #52363, #84802, #82823, #53361, #83309, #22467, #76669, #13871, #44261, #76195, #6771, #53842, #60448, #6271, #69057, #37650, #68560, #30064, #7257, #22953, #45260, #38140, #45745, #43762, #91402, #99985, #14377, #75684, #21001, #30570, #44751, #91911, #37166, #90926, #60953, #61455, #74706, #84311, #67065, #21967, #75194, #5283, #83810, #99486, #68064, #59447, #92405, #36161, #97989, #98988, #90429, #29088, #5769, #28568, #51882, #13390, #36658, #67564, #98498, #52860, #29571, #59954, #21476, #8765, #16364, #55343, #9786, #15342, #32567, #94898, #77688, #62959, #17357, #69562, #78681, #86320, #86825, #7764, #24954, #40646, #1683, #39136, #47255, #85309, #9270, #93909, #25460, #16857, #93403, #77164, #48264, #47744, #40142, #79212, #78176, #23952, #62438, #39634, #664, #70556, #63464, #169, #94400, #31053, #38659, #24463, #1172, #61942, #32046, #55830, #92894, #23447, #71084, #71584, #2179, #54337, #15855, #33061, #46762, #56349, #8271, #63956, #46238, #70049, #31549, #54856, #85834, #4150, #25980, #41142, #48777, #73567, #80207, #64971, #18375, #11290, #88326, #74071, #58344, #43130, #11777, #57849, #26968, #87350, #88829, #96399, #50253, #81697, #4661, #81206, #35553, #95427, #89320, #10272, #66454, #42638, #65953, #97379, #2681, #87836, #72080, #12270, #56850, #49271, #35047, #10775, #49761, #3678, #96905, #27476, #19874, #41649, #72591, #50743, #27946, #19394, #17879, #79709, #3197, #33571, #64465, #34081, #95914, #26474, #80715, #73084, #57350, #65457, #18881, #42149, #34557, #37526, #83184, #60815, #14248, #98369, #99853, #36038, #29941, #51239, #52726, #45622, #91278, #99361, #28958, #82704, #21844, #37038, #83688, #38017, #58828, #13271, #91777, #60322, #28441, #45135, #90301, #76075, #6652, #66939, #51762, #5159, #12776, #89792, #53238, #59837, #36536, #7130, #97869, #20366, #59321, #22341, #75067, #98867, #68928, #43642, #21355, #68432, #20871, #67441, #84193, #44133, #76551, #14740, #29445, #82205, #5646, #74580, #52240, #90800, #13744, #44624, #75558, #6144, #67949, #9142, #63339, #69926, #30935, #62827, #93784, #40524, #47129, #93270, #55706, #24344, #55218, #16737, #94277, #9662, #31924, #24832, #32443, #71459, #78052, #86696, #1045, #62317, #7637, #1558, #543, #78557, #31425, #77556, #47627, #17229, #30437, #40017, #53720, #8641, #61820, #61326, #70435, #86199, #23826, #46115, #48136, #92287, #70955, #39018, #77031, #15728, #92771, #79081, #22836, #15220, #84680, #38528, #85180, #39510, #54720, #23326, #69435, #85702, #16238, #52, #54213, #46630, #8145, #81575, #64339, #49631, #4035, #56224, #65338, #42033, #73452, #94774, #11656, #27345, #88700, #25858, #95302, #12146, #80084, #34924, #10151, #43008, #81090, #26349, #65820, #57721, #41527, #2050, #79587, #96785, #25334, #96276, #89207, #34439, #42517, #72470, #56735, #26846, #80588, #19271, #32932, #33963, #71955, #50137, #11165, #63836, #3558, #10651, #87218, #58226, #72969, #19755, #50623, #3075, #64848, #49149, #57225, #87717, #88201, #17753, #48654, #41017, #2558, #33441, #18253, #18752, #95795, #5534, #91164, #35432, #27835, #13640, #98756, #36922, #66335, #89688, #83571, #74463, #84081, #82084, #59719, #37412, #44513, #58712, #14632, #22224, #21729, #12656, #20246, #97268, #60203, #66826, #51638, #5044, #98249, #74950, #60700, #45018, #29828, #29339, #75444, #6028, #73946, #67836, #83069, #52613, #68318, #91661, #14132, #53124, #43525, #75961, #51122, #4532, #6537, #99243, #35924, #97754, #28324, #59200, #90176, #20751, #82588, #13153, #44007, #36418, #90685, #67325, #28839, #21242, #52119, #30828, #86096, #1443, #85585, #55600, #47024, #7517, #16126, #45513, #931, #94166, #78445, #38912, #31316, #55108, #23707, #61714, #9026, #39402, #77941, #8530, #38410, #61217, #69818, #16621, #54103, #86585, #84569, #47518, #85060, #24230, #39899, #15608, #45999, #70317, #31806, #76444, #62205, #8040, #70831, #62707, #93666, #32323, #63224, #24717, #7020, #37905, #68815, #99742, #93157, #30327, #92181, #77444, #22734, #53612, #46506, #15107, #429, #92660, #76918, #69325, #100246, #23213, #54601, #95689, #48535, #58119, #57111, #41923, #49036, #32820, #34810, #96665, #80475, #25744, #63727, #2447, #17636, #50028, #73340, #1934, #42405, #17120, #71849, #33855, #56624, #79474, #48015, #10537, #18135, #88093, #11547, #78959, #34327, #27234, #10038, #64738, #19153, #71343, #11045, #18642, #88591, #9548, #26728, #3927, #3447, #40901, #33327, #40410, #95175, #80981, #25221, #94663, #56108, #64225, #65711, #49522, #87097, #72859, #87607, #65224, #96167, #79969, #41412, #72357, #2961, #26236, #57612, #90064, #66715, #37306, #27732, #89100, #58600, #91061, #4941, #28723, #99132, #73831, #51518, #90576, #20138, #97649, #75337, #51010, #6429, #21143, #35820, #5920, #14021, #29717, #36809, #12038, #67215, #81961, #19650, #59597, #13536, #20633, #4420, #68206, #50512, #52022, #28216, #35316, #74356, #89575, #21625, #44900, #66229, #75841, #81463, #43409, #5428, #59090, #12536, #42891, #82483, #13047, #82962, #83455, #97165, #67721, #43908, #74847, #36310, #52507, #98138, #44406, #98646, #60096, #29229, #70192, #85977, #46906, #84456, #53501, #70704, #38294, #62587, #68703 ) ),
 .UNSPECIFIED., .F., .F., .T. ) 
 B_SPLINE_SURFACE_WITH_KNOTS ( ( 2, 2 ),
 ( 3, 2, 2, 2, 2, 2, 2, 2, 2, 2, 2, 2, 2, 2, 2, 2, 2, 2, 2, 2, 2, 2, 2, 2, 2, 2, 2, 2, 2, 2, 2, 2, 2, 2, 2, 2, 2, 2, 2, 2, 2, 2, 2, 2, 2, 2, 2, 2, 2, 2, 2, 2, 2, 2, 2, 2, 2, 2, 2, 2, 2, 2, 2, 2, 2, 2, 2, 2, 2, 2, 2, 2, 2, 2, 2, 2, 2, 2, 2, 2, 2, 2, 2, 2, 2, 2, 2, 2, 2, 2, 2, 2, 2, 2, 2, 2, 2, 2, 2, 2, 2, 2, 2, 2, 2, 2, 2, 2, 2, 2, 2, 2, 2, 2, 2, 2, 2, 2, 2, 2, 2, 2, 2, 2, 2, 2, 2, 2, 2, 2, 2, 2, 2, 2, 2, 2, 2, 2, 2, 2, 2, 2, 2, 2, 2, 2, 2, 2, 2, 2, 2, 2, 2, 2, 2, 2, 2, 2, 2, 2, 2, 2, 2, 2, 2, 2, 2, 2, 2, 2, 2, 2, 2, 2, 2, 2, 2, 2, 2, 2, 2, 2, 2, 2, 2, 2, 2, 2, 2, 2, 2, 2, 2, 2, 2, 2, 2, 2, 2, 2, 2, 2, 2, 2, 2, 2, 2, 2, 2, 2, 2, 2, 2, 2, 2, 2, 2, 2, 2, 2, 2, 2, 2, 2, 2, 2, 2, 2, 2, 2, 2, 2, 2, 2, 2, 2, 2, 2, 2, 2, 2, 2, 2, 2, 2, 2, 2, 2, 2, 2, 2, 2, 2, 2, 2, 2, 2, 2, 2, 2, 2, 2, 2, 2, 2, 2, 2, 2, 2, 2, 2, 2, 2, 2, 2, 2, 2, 2, 2, 2, 2, 2, 2, 2, 2, 2, 2, 2, 2, 2, 2, 2, 2, 2, 2, 2, 2, 2, 2, 2, 2, 2, 2, 2, 2, 2, 2, 2, 2, 2, 2, 2, 2, 2, 2, 2, 2, 2, 2, 2, 2, 2, 2, 2, 2, 2, 2, 2, 2, 2, 2, 2, 2, 2, 2, 2, 2, 2, 2, 2, 2, 2, 2, 2, 2, 2, 2, 2, 2, 2, 2, 2, 2, 2, 2, 2, 2, 2, 2, 2, 2, 2, 2, 2, 2, 2, 2, 2, 2, 2, 2, 2, 3 ),
 ( 0.000000000000000000, 1.000000000000000000 ),
 ( 0.000000000000000000, 0.002688172043010752903, 0.005376344086021505805, 0.008064516129032257841, 0.01075268817204301161, 0.01344086021505376365, 0.01612903225806451568, 0.01881720430107526945, 0.02150537634408602322, 0.02419354838709677352, 0.02688172043010752729, 0.02956989247311828106, 0.03225806451612903136, 0.03494623655913978166, 0.03763440860215053890, 0.04032258064516128920, 0.04301075268817204644, 0.04569892473118279674, 0.04838709677419354704, 0.05107526881720430428, 0.05376344086021505458, 0.05645161290322580488, 0.05913978494623656212, 0.06182795698924731242, 0.06451612903225806273, 0.06720430107526881303, 0.06989247311827956333, 0.07258064516129032751, 0.07526881720430107781, 0.07795698924731182811, 0.08064516129032257841, 0.08333333333333332871, 0.08602150537634409289, 0.08870967741935484319, 0.09139784946236559349, 0.09408602150537634379, 0.09677419354838709409, 0.09946236559139784439, 0.1021505376344086086, 0.1048387096774193589, 0.1075268817204301092, 0.1102150537634408595, 0.1129032258064516098, 0.1155913978494623601, 0.1182795698924731242, 0.1209677419354838745, 0.1236559139784946248, 0.1263440860215053752, 0.1290322580645161255, 0.1317204301075268758, 0.1344086021505376261, 0.1370967741935483764, 0.1397849462365591267, 0.1424731182795699047, 0.1451612903225806550, 0.1478494623655914053, 0.1505376344086021556, 0.1532258064516129059, 0.1559139784946236562, 0.1586021505376344065, 0.1612903225806451568, 0.1639784946236559071, 0.1666666666666666574, 0.1693548387096774077, 0.1720430107526881858, 0.1747311827956989361, 0.1774193548387096864, 0.1801075268817204367, 0.1827956989247311870, 0.1854838709677419373, 0.1881720430107526876, 0.1908602150537634379, 0.1935483870967741882, 0.1962365591397849385, 0.1989247311827956888, 0.2016129032258064391, 0.2043010752688172171, 0.2069892473118279674, 0.2096774193548387177, 0.2123655913978494680, 0.2150537634408602183, 0.2177419354838709686, 0.2204301075268817189, 0.2231182795698924692, 0.2258064516129032195, 0.2284946236559139698, 0.2311827956989247201, 0.2338709677419354704, 0.2365591397849462485, 0.2392473118279569988, 0.2419354838709677491, 0.2446236559139784994, 0.2473118279569892497, 0.2500000000000000000, 0.2526881720430107503, 0.2553763440860215006, 0.2580645161290322509, 0.2607526881720430012, 0.2634408602150537515, 0.2661290322580645018, 0.2688172043010752521, 0.2715053763440860024, 0.2741935483870967527, 0.2768817204301075030, 0.2795698924731182533, 0.2822580645161290591, 0.2849462365591398094, 0.2876344086021505597, 0.2903225806451613100, 0.2930107526881720603, 0.2956989247311828106, 0.2983870967741935609, 0.3010752688172043112, 0.3037634408602150615, 0.3064516129032258118, 0.3091397849462365621, 0.3118279569892473124, 0.3145161290322580627, 0.3172043010752688130, 0.3198924731182795633, 0.3225806451612903136, 0.3252688172043010639, 0.3279569892473118142, 0.3306451612903225645, 0.3333333333333333148, 0.3360215053763440651, 0.3387096774193548154, 0.3413978494623655657, 0.3440860215053763715, 0.3467741935483871218, 0.3494623655913978721, 0.3521505376344086224, 0.3548387096774193727, 0.3575268817204301230, 0.3602150537634408733, 0.3629032258064516236, 0.3655913978494623739, 0.3682795698924731242, 0.3709677419354838745, 0.3736559139784946248, 0.3763440860215053752, 0.3790322580645161255, 0.3817204301075268758, 0.3844086021505376261, 0.3870967741935483764, 0.3897849462365591267, 0.3924731182795698770, 0.3951612903225806273, 0.3978494623655913776, 0.4005376344086021279, 0.4032258064516128782, 0.4059139784946236285, 0.4086021505376344343, 0.4112903225806451846, 0.4139784946236559349, 0.4166666666666666852, 0.4193548387096774355, 0.4220430107526881858, 0.4247311827956989361, 0.4274193548387096864, 0.4301075268817204367, 0.4327956989247311870, 0.4354838709677419373, 0.4381720430107526876, 0.4408602150537634379, 0.4435483870967741882, 0.4462365591397849385, 0.4489247311827956888, 0.4516129032258064391, 0.4543010752688171894, 0.4569892473118279397, 0.4596774193548386900, 0.4623655913978494403, 0.4650537634408601906, 0.4677419354838709409, 0.4704301075268817467, 0.4731182795698924970, 0.4758064516129032473, 0.4784946236559139976, 0.4811827956989247479, 0.4838709677419354982, 0.4865591397849462485, 0.4892473118279569988, 0.4919354838709677491, 0.4946236559139784994, 0.4973118279569892497, 0.5000000000000000000, 0.5026881720430107503, 0.5053763440860215006, 0.5080645161290322509, 0.5107526881720430012, 0.5134408602150537515, 0.5161290322580645018, 0.5188172043010752521, 0.5215053763440860024, 0.5241935483870967527, 0.5268817204301075030, 0.5295698924731182533, 0.5322580645161290036, 0.5349462365591397539, 0.5376344086021505042, 0.5403225806451612545, 0.5430107526881720048, 0.5456989247311827551, 0.5483870967741935054, 0.5510752688172042557, 0.5537634408602150060, 0.5564516129032257563, 0.5591397849462365066, 0.5618279569892472569, 0.5645161290322581182, 0.5672043010752688685, 0.5698924731182796188, 0.5725806451612903691, 0.5752688172043011194, 0.5779569892473118697, 0.5806451612903226200, 0.5833333333333333703, 0.5860215053763441206, 0.5887096774193548709, 0.5913978494623656212, 0.5940860215053763715, 0.5967741935483871218, 0.5994623655913978721, 0.6021505376344086224, 0.6048387096774193727, 0.6075268817204301230, 0.6102150537634408733, 0.6129032258064516236, 0.6155913978494623739, 0.6182795698924731242, 0.6209677419354838745, 0.6236559139784946248, 0.6263440860215053752, 0.6290322580645161255, 0.6317204301075268758, 0.6344086021505376261, 0.6370967741935483764, 0.6397849462365591267, 0.6424731182795698770, 0.6451612903225806273, 0.6478494623655913776, 0.6505376344086021279, 0.6532258064516128782, 0.6559139784946236285, 0.6586021505376343788, 0.6612903225806451291, 0.6639784946236558794, 0.6666666666666666297, 0.6693548387096773800, 0.6720430107526881303, 0.6747311827956988806, 0.6774193548387096309, 0.6801075268817203812, 0.6827956989247311315, 0.6854838709677418818, 0.6881720430107527431, 0.6908602150537634934, 0.6935483870967742437, 0.6962365591397849940, 0.6989247311827957443, 0.7016129032258064946, 0.7043010752688172449, 0.7069892473118279952, 0.7096774193548387455, 0.7123655913978494958, 0.7150537634408602461, 0.7177419354838709964, 0.7204301075268817467, 0.7231182795698924970, 0.7258064516129032473, 0.7284946236559139976, 0.7311827956989247479, 0.7338709677419354982, 0.7365591397849462485, 0.7392473118279569988, 0.7419354838709677491, 0.7446236559139784994, 0.7473118279569892497, 0.7500000000000000000, 0.7526881720430107503, 0.7553763440860215006, 0.7580645161290322509, 0.7607526881720430012, 0.7634408602150537515, 0.7661290322580645018, 0.7688172043010752521, 0.7715053763440860024, 0.7741935483870967527, 0.7768817204301075030, 0.7795698924731182533, 0.7822580645161290036, 0.7849462365591397539, 0.7876344086021505042, 0.7903225806451612545, 0.7930107526881720048, 0.7956989247311827551, 0.7983870967741935054, 0.8010752688172042557, 0.8037634408602150060, 0.8064516129032257563, 0.8091397849462365066, 0.8118279569892472569, 0.8145161290322581182, 0.8172043010752688685, 0.8198924731182796188, 0.8225806451612903691, 0.8252688172043011194, 0.8279569892473118697, 0.8306451612903226200, 0.8333333333333333703, 0.8360215053763441206, 0.8387096774193548709, 0.8413978494623656212, 0.8440860215053763715, 0.8467741935483871218, 0.8494623655913978721, 0.8521505376344086224, 0.8548387096774193727, 0.8575268817204301230, 0.8602150537634408733, 0.8629032258064516236, 0.8655913978494623739, 0.8682795698924731242, 0.8709677419354838745, 0.8736559139784946248, 0.8763440860215053752, 0.8790322580645161255, 0.8817204301075268758, 0.8844086021505376261, 0.8870967741935483764, 0.8897849462365591267, 0.8924731182795698770, 0.8951612903225806273, 0.8978494623655913776, 0.9005376344086021279, 0.9032258064516128782, 0.9059139784946236285, 0.9086021505376343788, 0.9112903225806451291, 0.9139784946236558794, 0.9166666666666666297, 0.9193548387096773800, 0.9220430107526881303, 0.9247311827956988806, 0.9274193548387096309, 0.9301075268817203812, 0.9327956989247311315, 0.9354838709677418818, 0.9381720430107527431, 0.9408602150537634934, 0.9435483870967742437, 0.9462365591397849940, 0.9489247311827957443, 0.9516129032258064946, 0.9543010752688172449, 0.9569892473118279952, 0.9596774193548387455, 0.9623655913978494958, 0.9650537634408602461, 0.9677419354838709964, 0.9704301075268817467, 0.9731182795698924970, 0.9758064516129032473, 0.9784946236559139976, 0.9811827956989247479, 0.9838709677419354982, 0.9865591397849462485, 0.9892473118279569988, 0.9919354838709677491, 0.9946236559139784994, 0.9973118279569892497, 1.000000000000000000 ),
 .UNSPECIFIED. ) 
 GEOMETRIC_REPRESENTATION_ITEM ( )  RATIONAL_B_SPLINE_SURFACE ( (
 ( 1.000000000000000000, 0.8660254037844387076, 1.000000000000000000, 0.8660254037844387076, 1.000000000000000000, 0.8660254037844387076, 1.000000000000000000, 0.8660254037844387076, 1.000000000000000000, 0.8660254037844387076, 1.000000000000000000, 0.8660254037844387076, 1.000000000000000000, 0.8660254037844387076, 1.000000000000000000, 0.8660254037844387076, 1.000000000000000000, 0.8660254037844387076, 1.000000000000000000, 0.8660254037844387076, 1.000000000000000000, 0.8660254037844387076, 1.000000000000000000, 0.8660254037844387076, 1.000000000000000000, 0.8660254037844387076, 1.000000000000000000, 0.8660254037844387076, 1.000000000000000000, 0.8660254037844387076, 1.000000000000000000, 0.8660254037844387076, 1.000000000000000000, 0.8660254037844387076, 1.000000000000000000, 0.8660254037844387076, 1.000000000000000000, 0.8660254037844387076, 1.000000000000000000, 0.8660254037844387076, 1.000000000000000000, 0.8660254037844387076, 1.000000000000000000, 0.8660254037844387076, 1.000000000000000000, 0.8660254037844387076, 1.000000000000000000, 0.8660254037844387076, 1.000000000000000000, 0.8660254037844387076, 1.000000000000000000, 0.8660254037844387076, 1.000000000000000000, 0.8660254037844387076, 1.000000000000000000, 0.8660254037844387076, 1.000000000000000000, 0.8660254037844387076, 1.000000000000000000, 0.8660254037844387076, 1.000000000000000000, 0.8660254037844387076, 1.000000000000000000, 0.8660254037844387076, 1.000000000000000000, 0.8660254037844387076, 1.000000000000000000, 0.8660254037844387076, 1.000000000000000000, 0.8660254037844387076, 1.000000000000000000, 0.8660254037844387076, 1.000000000000000000, 0.8660254037844387076, 1.000000000000000000, 0.8660254037844387076, 1.000000000000000000, 0.8660254037844387076, 1.000000000000000000, 0.8660254037844387076, 1.000000000000000000, 0.8660254037844387076, 1.000000000000000000, 0.8660254037844387076, 1.000000000000000000, 0.8660254037844387076, 1.000000000000000000, 0.8660254037844387076, 1.000000000000000000, 0.8660254037844387076, 1.000000000000000000, 0.8660254037844387076, 1.000000000000000000, 0.8660254037844387076, 1.000000000000000000, 0.8660254037844387076, 1.000000000000000000, 0.8660254037844387076, 1.000000000000000000, 0.8660254037844387076, 1.000000000000000000, 0.8660254037844387076, 1.000000000000000000, 0.8660254037844387076, 1.000000000000000000, 0.8660254037844387076, 1.000000000000000000, 0.8660254037844387076, 1.000000000000000000, 0.8660254037844387076, 1.000000000000000000, 0.8660254037844387076, 1.000000000000000000, 0.8660254037844387076, 1.000000000000000000, 0.8660254037844387076, 1.000000000000000000, 0.8660254037844387076, 1.000000000000000000, 0.8660254037844387076, 1.000000000000000000, 0.8660254037844387076, 1.000000000000000000, 0.8660254037844387076, 1.000000000000000000, 0.8660254037844387076, 1.000000000000000000, 0.8660254037844387076, 1.000000000000000000, 0.8660254037844387076, 1.000000000000000000, 0.8660254037844387076, 1.000000000000000000, 0.8660254037844387076, 1.000000000000000000, 0.8660254037844387076, 1.000000000000000000, 0.8660254037844387076, 1.000000000000000000, 0.8660254037844387076, 1.000000000000000000, 0.8660254037844387076, 1.000000000000000000, 0.8660254037844387076, 1.000000000000000000, 0.8660254037844387076, 1.000000000000000000, 0.8660254037844387076, 1.000000000000000000, 0.8660254037844387076, 1.000000000000000000, 0.8660254037844387076, 1.000000000000000000, 0.8660254037844387076, 1.000000000000000000, 0.8660254037844387076, 1.000000000000000000, 0.8660254037844387076, 1.000000000000000000, 0.8660254037844387076, 1.000000000000000000, 0.8660254037844387076, 1.000000000000000000, 0.8660254037844387076, 1.000000000000000000, 0.8660254037844387076, 1.000000000000000000, 0.8660254037844387076, 1.000000000000000000, 0.8660254037844387076, 1.000000000000000000, 0.8660254037844387076, 1.000000000000000000, 0.8660254037844387076, 1.000000000000000000, 0.8660254037844387076, 1.000000000000000000, 0.8660254037844387076, 1.000000000000000000, 0.8660254037844387076, 1.000000000000000000, 0.8660254037844387076, 1.000000000000000000, 0.8660254037844387076, 1.000000000000000000, 0.8660254037844387076, 1.000000000000000000, 0.8660254037844387076, 1.000000000000000000, 0.8660254037844387076, 1.000000000000000000, 0.8660254037844387076, 1.000000000000000000, 0.8660254037844387076, 1.000000000000000000, 0.8660254037844387076, 1.000000000000000000, 0.8660254037844387076, 1.000000000000000000, 0.8660254037844387076, 1.000000000000000000, 0.8660254037844387076, 1.000000000000000000, 0.8660254037844387076, 1.000000000000000000, 0.8660254037844387076, 1.000000000000000000, 0.8660254037844387076, 1.000000000000000000, 0.8660254037844387076, 1.000000000000000000, 0.8660254037844387076, 1.000000000000000000, 0.8660254037844387076, 1.000000000000000000, 0.8660254037844387076, 1.000000000000000000, 0.8660254037844387076, 1.000000000000000000, 0.8660254037844387076, 1.000000000000000000, 0.8660254037844387076, 1.000000000000000000, 0.8660254037844387076, 1.000000000000000000, 0.8660254037844387076, 1.000000000000000000, 0.8660254037844387076, 1.000000000000000000, 0.8660254037844387076, 1.000000000000000000, 0.8660254037844387076, 1.000000000000000000, 0.8660254037844387076, 1.000000000000000000, 0.8660254037844387076, 1.000000000000000000, 0.8660254037844387076, 1.000000000000000000, 0.8660254037844387076, 1.000000000000000000, 0.8660254037844387076, 1.000000000000000000, 0.8660254037844387076, 1.000000000000000000, 0.8660254037844387076, 1.000000000000000000, 0.8660254037844387076, 1.000000000000000000, 0.8660254037844387076, 1.000000000000000000, 0.8660254037844387076, 1.000000000000000000, 0.8660254037844387076, 1.000000000000000000, 0.8660254037844387076, 1.000000000000000000, 0.8660254037844387076, 1.000000000000000000, 0.8660254037844387076, 1.000000000000000000, 0.8660254037844387076, 1.000000000000000000, 0.8660254037844387076, 1.000000000000000000, 0.8660254037844387076, 1.000000000000000000, 0.8660254037844387076, 1.000000000000000000, 0.8660254037844387076, 1.000000000000000000, 0.8660254037844387076, 1.000000000000000000, 0.8660254037844387076, 1.000000000000000000, 0.8660254037844387076, 1.000000000000000000, 0.8660254037844387076, 1.000000000000000000, 0.8660254037844387076, 1.000000000000000000, 0.8660254037844387076, 1.000000000000000000, 0.8660254037844387076, 1.000000000000000000, 0.8660254037844387076, 1.000000000000000000, 0.8660254037844387076, 1.000000000000000000, 0.8660254037844387076, 1.000000000000000000, 0.8660254037844387076, 1.000000000000000000, 0.8660254037844387076, 1.000000000000000000, 0.8660254037844387076, 1.000000000000000000, 0.8660254037844387076, 1.000000000000000000, 0.8660254037844387076, 1.000000000000000000, 0.8660254037844387076, 1.000000000000000000, 0.8660254037844387076, 1.000000000000000000, 0.8660254037844387076, 1.000000000000000000, 0.8660254037844387076, 1.000000000000000000, 0.8660254037844387076, 1.000000000000000000, 0.8660254037844387076, 1.000000000000000000, 0.8660254037844387076, 1.000000000000000000, 0.8660254037844387076, 1.000000000000000000, 0.8660254037844387076, 1.000000000000000000, 0.8660254037844387076, 1.000000000000000000, 0.8660254037844387076, 1.000000000000000000, 0.8660254037844387076, 1.000000000000000000, 0.8660254037844387076, 1.000000000000000000, 0.8660254037844387076, 1.000000000000000000, 0.8660254037844387076, 1.000000000000000000, 0.8660254037844387076, 1.000000000000000000, 0.8660254037844387076, 1.000000000000000000, 0.8660254037844387076, 1.000000000000000000, 0.8660254037844387076, 1.000000000000000000, 0.8660254037844387076, 1.000000000000000000, 0.8660254037844387076, 1.000000000000000000, 0.8660254037844387076, 1.000000000000000000, 0.8660254037844387076, 1.000000000000000000, 0.8660254037844387076, 1.000000000000000000, 0.8660254037844387076, 1.000000000000000000, 0.8660254037844387076, 1.000000000000000000, 0.8660254037844387076, 1.000000000000000000, 0.8660254037844387076, 1.000000000000000000, 0.8660254037844387076, 1.000000000000000000, 0.8660254037844387076, 1.000000000000000000, 0.8660254037844387076, 1.000000000000000000, 0.8660254037844387076, 1.000000000000000000, 0.8660254037844387076, 1.000000000000000000, 0.8660254037844387076, 1.000000000000000000, 0.8660254037844387076, 1.000000000000000000, 0.8660254037844387076, 1.000000000000000000, 0.8660254037844387076, 1.000000000000000000, 0.8660254037844387076, 1.000000000000000000, 0.8660254037844387076, 1.000000000000000000, 0.8660254037844387076, 1.000000000000000000, 0.8660254037844387076, 1.000000000000000000, 0.8660254037844387076, 1.000000000000000000, 0.8660254037844387076, 1.000000000000000000, 0.8660254037844387076, 1.000000000000000000, 0.8660254037844387076, 1.000000000000000000, 0.8660254037844387076, 1.000000000000000000, 0.8660254037844387076, 1.000000000000000000, 0.8660254037844387076, 1.000000000000000000, 0.8660254037844387076, 1.000000000000000000, 0.8660254037844387076, 1.000000000000000000, 0.8660254037844387076, 1.000000000000000000, 0.8660254037844387076, 1.000000000000000000, 0.8660254037844387076, 1.000000000000000000, 0.8660254037844387076, 1.000000000000000000, 0.8660254037844387076, 1.000000000000000000, 0.8660254037844387076, 1.000000000000000000, 0.8660254037844387076, 1.000000000000000000, 0.8660254037844387076, 1.000000000000000000, 0.8660254037844387076, 1.000000000000000000, 0.8660254037844387076, 1.000000000000000000, 0.8660254037844387076, 1.000000000000000000, 0.8660254037844387076, 1.000000000000000000, 0.8660254037844387076, 1.000000000000000000, 0.8660254037844387076, 1.000000000000000000, 0.8660254037844387076, 1.000000000000000000, 0.8660254037844387076, 1.000000000000000000, 0.8660254037844387076, 1.000000000000000000, 0.8660254037844387076, 1.000000000000000000, 0.8660254037844387076, 1.000000000000000000, 0.8660254037844387076, 1.000000000000000000, 0.8660254037844387076, 1.000000000000000000, 0.8660254037844387076, 1.000000000000000000, 0.8660254037844387076, 1.000000000000000000, 0.8660254037844387076, 1.000000000000000000, 0.8660254037844387076, 1.000000000000000000, 0.8660254037844387076, 1.000000000000000000, 0.8660254037844387076, 1.000000000000000000, 0.8660254037844387076, 1.000000000000000000, 0.8660254037844387076, 1.000000000000000000, 0.8660254037844387076, 1.000000000000000000, 0.8660254037844387076, 1.000000000000000000, 0.8660254037844387076, 1.000000000000000000, 0.8660254037844387076, 1.000000000000000000, 0.8660254037844387076, 1.000000000000000000, 0.8660254037844387076, 1.000000000000000000, 0.8660254037844387076, 1.000000000000000000, 0.8660254037844387076, 1.000000000000000000, 0.8660254037844387076, 1.000000000000000000, 0.8660254037844387076, 1.000000000000000000, 0.8660254037844387076, 1.000000000000000000, 0.8660254037844387076, 1.000000000000000000, 0.8660254037844387076, 1.000000000000000000, 0.8660254037844387076, 1.000000000000000000, 0.8660254037844387076, 1.000000000000000000, 0.8660254037844387076, 1.000000000000000000, 0.8660254037844387076, 1.000000000000000000, 0.8660254037844387076, 1.000000000000000000, 0.8660254037844387076, 1.000000000000000000, 0.8660254037844387076, 1.000000000000000000, 0.8660254037844387076, 1.000000000000000000, 0.8660254037844387076, 1.000000000000000000, 0.8660254037844387076, 1.000000000000000000, 0.8660254037844387076, 1.000000000000000000, 0.8660254037844387076, 1.000000000000000000, 0.8660254037844387076, 1.000000000000000000, 0.8660254037844387076, 1.000000000000000000, 0.8660254037844387076, 1.000000000000000000, 0.8660254037844387076, 1.000000000000000000, 0.8660254037844387076, 1.000000000000000000, 0.8660254037844387076, 1.000000000000000000, 0.8660254037844387076, 1.000000000000000000, 0.8660254037844387076, 1.000000000000000000, 0.8660254037844387076, 1.000000000000000000, 0.8660254037844387076, 1.000000000000000000, 0.8660254037844387076, 1.000000000000000000, 0.8660254037844387076, 1.000000000000000000, 0.8660254037844387076, 1.000000000000000000, 0.8660254037844387076, 1.000000000000000000, 0.8660254037844387076, 1.000000000000000000, 0.8660254037844387076, 1.000000000000000000, 0.8660254037844387076, 1.000000000000000000, 0.8660254037844387076, 1.000000000000000000, 0.8660254037844387076, 1.000000000000000000, 0.8660254037844387076, 1.000000000000000000, 0.8660254037844387076, 1.000000000000000000, 0.8660254037844387076, 1.000000000000000000, 0.8660254037844387076, 1.000000000000000000, 0.8660254037844387076, 1.000000000000000000, 0.8660254037844387076, 1.000000000000000000, 0.8660254037844387076, 1.000000000000000000, 0.8660254037844387076, 1.000000000000000000, 0.8660254037844387076, 1.000000000000000000, 0.8660254037844387076, 1.000000000000000000, 0.8660254037844387076, 1.000000000000000000, 0.8660254037844387076, 1.000000000000000000, 0.8660254037844387076, 1.000000000000000000, 0.8660254037844387076, 1.000000000000000000, 0.8660254037844387076, 1.000000000000000000, 0.8660254037844387076, 1.000000000000000000, 0.8660254037844387076, 1.000000000000000000, 0.8660254037844387076, 1.000000000000000000, 0.8660254037844387076, 1.000000000000000000, 0.8660254037844387076, 1.000000000000000000, 0.8660254037844387076, 1.000000000000000000, 0.8660254037844387076, 1.000000000000000000, 0.8660254037844387076, 1.000000000000000000, 0.8660254037844387076, 1.000000000000000000, 0.8660254037844387076, 1.000000000000000000, 0.8660254037844387076, 1.000000000000000000, 0.8660254037844387076, 1.000000000000000000, 0.8660254037844387076, 1.000000000000000000, 0.8660254037844387076, 1.000000000000000000, 0.8660254037844387076, 1.000000000000000000, 0.8660254037844387076, 1.000000000000000000, 0.8660254037844387076, 1.000000000000000000, 0.8660254037844387076, 1.000000000000000000, 0.8660254037844387076, 1.000000000000000000, 0.8660254037844387076, 1.000000000000000000, 0.8660254037844387076, 1.000000000000000000, 0.8660254037844387076, 1.000000000000000000, 0.8660254037844387076, 1.000000000000000000, 0.8660254037844387076, 1.000000000000000000, 0.8660254037844387076, 1.000000000000000000, 0.8660254037844387076, 1.000000000000000000, 0.8660254037844387076, 1.000000000000000000, 0.8660254037844387076, 1.000000000000000000, 0.8660254037844387076, 1.000000000000000000, 0.8660254037844387076, 1.000000000000000000, 0.8660254037844387076, 1.000000000000000000, 0.8660254037844387076, 1.000000000000000000, 0.8660254037844387076, 1.000000000000000000, 0.8660254037844387076, 1.000000000000000000, 0.8660254037844387076, 1.000000000000000000, 0.8660254037844387076, 1.000000000000000000, 0.8660254037844387076, 1.000000000000000000, 0.8660254037844387076, 1.000000000000000000, 0.8660254037844387076, 1.000000000000000000, 0.8660254037844387076, 1.000000000000000000, 0.8660254037844387076, 1.000000000000000000, 0.8660254037844387076, 1.000000000000000000, 0.8660254037844387076, 1.000000000000000000, 0.8660254037844387076, 1.000000000000000000, 0.8660254037844387076, 1.000000000000000000, 0.8660254037844387076, 1.000000000000000000, 0.8660254037844387076, 1.000000000000000000, 0.8660254037844387076, 1.000000000000000000, 0.8660254037844387076, 1.000000000000000000, 0.8660254037844387076, 1.000000000000000000, 0.8660254037844387076, 1.000000000000000000, 0.8660254037844387076, 1.000000000000000000, 0.8660254037844387076, 1.000000000000000000, 0.8660254037844387076, 1.000000000000000000, 0.8660254037844387076, 1.000000000000000000, 0.8660254037844387076, 1.000000000000000000, 0.8660254037844387076, 1.000000000000000000, 0.8660254037844387076, 1.000000000000000000, 0.8660254037844387076, 1.000000000000000000, 0.8660254037844387076, 1.000000000000000000, 0.8660254037844387076, 1.000000000000000000, 0.8660254037844387076, 1.000000000000000000, 0.8660254037844387076, 1.000000000000000000, 0.8660254037844387076, 1.000000000000000000, 0.8660254037844387076, 1.000000000000000000, 0.8660254037844387076, 1.000000000000000000, 0.8660254037844387076, 1.000000000000000000, 0.8660254037844387076, 1.000000000000000000, 0.8660254037844387076, 1.000000000000000000, 0.8660254037844387076, 1.000000000000000000, 0.8660254037844387076, 1.000000000000000000, 0.8660254037844387076, 1.000000000000000000, 0.8660254037844387076, 1.000000000000000000, 0.8660254037844387076, 1.000000000000000000, 0.8660254037844387076, 1.000000000000000000, 0.8660254037844387076, 1.000000000000000000, 0.8660254037844387076, 1.000000000000000000, 0.8660254037844387076, 1.000000000000000000, 0.8660254037844387076, 1.000000000000000000, 0.8660254037844387076, 1.000000000000000000, 0.8660254037844387076, 1.000000000000000000, 0.8660254037844387076, 1.000000000000000000, 0.8660254037844387076, 1.000000000000000000, 0.8660254037844387076, 1.000000000000000000),
 ( 1.000000000000000000, 0.8660254037844387076, 1.000000000000000000, 0.8660254037844387076, 1.000000000000000000, 0.8660254037844387076, 1.000000000000000000, 0.8660254037844387076, 1.000000000000000000, 0.8660254037844387076, 1.000000000000000000, 0.8660254037844387076, 1.000000000000000000, 0.8660254037844387076, 1.000000000000000000, 0.8660254037844387076, 1.000000000000000000, 0.8660254037844387076, 1.000000000000000000, 0.8660254037844387076, 1.000000000000000000, 0.8660254037844387076, 1.000000000000000000, 0.8660254037844387076, 1.000000000000000000, 0.8660254037844387076, 1.000000000000000000, 0.8660254037844387076, 1.000000000000000000, 0.8660254037844387076, 1.000000000000000000, 0.8660254037844387076, 1.000000000000000000, 0.8660254037844387076, 1.000000000000000000, 0.8660254037844387076, 1.000000000000000000, 0.8660254037844387076, 1.000000000000000000, 0.8660254037844387076, 1.000000000000000000, 0.8660254037844387076, 1.000000000000000000, 0.8660254037844387076, 1.000000000000000000, 0.8660254037844387076, 1.000000000000000000, 0.8660254037844387076, 1.000000000000000000, 0.8660254037844387076, 1.000000000000000000, 0.8660254037844387076, 1.000000000000000000, 0.8660254037844387076, 1.000000000000000000, 0.8660254037844387076, 1.000000000000000000, 0.8660254037844387076, 1.000000000000000000, 0.8660254037844387076, 1.000000000000000000, 0.8660254037844387076, 1.000000000000000000, 0.8660254037844387076, 1.000000000000000000, 0.8660254037844387076, 1.000000000000000000, 0.8660254037844387076, 1.000000000000000000, 0.8660254037844387076, 1.000000000000000000, 0.8660254037844387076, 1.000000000000000000, 0.8660254037844387076, 1.000000000000000000, 0.8660254037844387076, 1.000000000000000000, 0.8660254037844387076, 1.000000000000000000, 0.8660254037844387076, 1.000000000000000000, 0.8660254037844387076, 1.000000000000000000, 0.8660254037844387076, 1.000000000000000000, 0.8660254037844387076, 1.000000000000000000, 0.8660254037844387076, 1.000000000000000000, 0.8660254037844387076, 1.000000000000000000, 0.8660254037844387076, 1.000000000000000000, 0.8660254037844387076, 1.000000000000000000, 0.8660254037844387076, 1.000000000000000000, 0.8660254037844387076, 1.000000000000000000, 0.8660254037844387076, 1.000000000000000000, 0.8660254037844387076, 1.000000000000000000, 0.8660254037844387076, 1.000000000000000000, 0.8660254037844387076, 1.000000000000000000, 0.8660254037844387076, 1.000000000000000000, 0.8660254037844387076, 1.000000000000000000, 0.8660254037844387076, 1.000000000000000000, 0.8660254037844387076, 1.000000000000000000, 0.8660254037844387076, 1.000000000000000000, 0.8660254037844387076, 1.000000000000000000, 0.8660254037844387076, 1.000000000000000000, 0.8660254037844387076, 1.000000000000000000, 0.8660254037844387076, 1.000000000000000000, 0.8660254037844387076, 1.000000000000000000, 0.8660254037844387076, 1.000000000000000000, 0.8660254037844387076, 1.000000000000000000, 0.8660254037844387076, 1.000000000000000000, 0.8660254037844387076, 1.000000000000000000, 0.8660254037844387076, 1.000000000000000000, 0.8660254037844387076, 1.000000000000000000, 0.8660254037844387076, 1.000000000000000000, 0.8660254037844387076, 1.000000000000000000, 0.8660254037844387076, 1.000000000000000000, 0.8660254037844387076, 1.000000000000000000, 0.8660254037844387076, 1.000000000000000000, 0.8660254037844387076, 1.000000000000000000, 0.8660254037844387076, 1.000000000000000000, 0.8660254037844387076, 1.000000000000000000, 0.8660254037844387076, 1.000000000000000000, 0.8660254037844387076, 1.000000000000000000, 0.8660254037844387076, 1.000000000000000000, 0.8660254037844387076, 1.000000000000000000, 0.8660254037844387076, 1.000000000000000000, 0.8660254037844387076, 1.000000000000000000, 0.8660254037844387076, 1.000000000000000000, 0.8660254037844387076, 1.000000000000000000, 0.8660254037844387076, 1.000000000000000000, 0.8660254037844387076, 1.000000000000000000, 0.8660254037844387076, 1.000000000000000000, 0.8660254037844387076, 1.000000000000000000, 0.8660254037844387076, 1.000000000000000000, 0.8660254037844387076, 1.000000000000000000, 0.8660254037844387076, 1.000000000000000000, 0.8660254037844387076, 1.000000000000000000, 0.8660254037844387076, 1.000000000000000000, 0.8660254037844387076, 1.000000000000000000, 0.8660254037844387076, 1.000000000000000000, 0.8660254037844387076, 1.000000000000000000, 0.8660254037844387076, 1.000000000000000000, 0.8660254037844387076, 1.000000000000000000, 0.8660254037844387076, 1.000000000000000000, 0.8660254037844387076, 1.000000000000000000, 0.8660254037844387076, 1.000000000000000000, 0.8660254037844387076, 1.000000000000000000, 0.8660254037844387076, 1.000000000000000000, 0.8660254037844387076, 1.000000000000000000, 0.8660254037844387076, 1.000000000000000000, 0.8660254037844387076, 1.000000000000000000, 0.8660254037844387076, 1.000000000000000000, 0.8660254037844387076, 1.000000000000000000, 0.8660254037844387076, 1.000000000000000000, 0.8660254037844387076, 1.000000000000000000, 0.8660254037844387076, 1.000000000000000000, 0.8660254037844387076, 1.000000000000000000, 0.8660254037844387076, 1.000000000000000000, 0.8660254037844387076, 1.000000000000000000, 0.8660254037844387076, 1.000000000000000000, 0.8660254037844387076, 1.000000000000000000, 0.8660254037844387076, 1.000000000000000000, 0.8660254037844387076, 1.000000000000000000, 0.8660254037844387076, 1.000000000000000000, 0.8660254037844387076, 1.000000000000000000, 0.8660254037844387076, 1.000000000000000000, 0.8660254037844387076, 1.000000000000000000, 0.8660254037844387076, 1.000000000000000000, 0.8660254037844387076, 1.000000000000000000, 0.8660254037844387076, 1.000000000000000000, 0.8660254037844387076, 1.000000000000000000, 0.8660254037844387076, 1.000000000000000000, 0.8660254037844387076, 1.000000000000000000, 0.8660254037844387076, 1.000000000000000000, 0.8660254037844387076, 1.000000000000000000, 0.8660254037844387076, 1.000000000000000000, 0.8660254037844387076, 1.000000000000000000, 0.8660254037844387076, 1.000000000000000000, 0.8660254037844387076, 1.000000000000000000, 0.8660254037844387076, 1.000000000000000000, 0.8660254037844387076, 1.000000000000000000, 0.8660254037844387076, 1.000000000000000000, 0.8660254037844387076, 1.000000000000000000, 0.8660254037844387076, 1.000000000000000000, 0.8660254037844387076, 1.000000000000000000, 0.8660254037844387076, 1.000000000000000000, 0.8660254037844387076, 1.000000000000000000, 0.8660254037844387076, 1.000000000000000000, 0.8660254037844387076, 1.000000000000000000, 0.8660254037844387076, 1.000000000000000000, 0.8660254037844387076, 1.000000000000000000, 0.8660254037844387076, 1.000000000000000000, 0.8660254037844387076, 1.000000000000000000, 0.8660254037844387076, 1.000000000000000000, 0.8660254037844387076, 1.000000000000000000, 0.8660254037844387076, 1.000000000000000000, 0.8660254037844387076, 1.000000000000000000, 0.8660254037844387076, 1.000000000000000000, 0.8660254037844387076, 1.000000000000000000, 0.8660254037844387076, 1.000000000000000000, 0.8660254037844387076, 1.000000000000000000, 0.8660254037844387076, 1.000000000000000000, 0.8660254037844387076, 1.000000000000000000, 0.8660254037844387076, 1.000000000000000000, 0.8660254037844387076, 1.000000000000000000, 0.8660254037844387076, 1.000000000000000000, 0.8660254037844387076, 1.000000000000000000, 0.8660254037844387076, 1.000000000000000000, 0.8660254037844387076, 1.000000000000000000, 0.8660254037844387076, 1.000000000000000000, 0.8660254037844387076, 1.000000000000000000, 0.8660254037844387076, 1.000000000000000000, 0.8660254037844387076, 1.000000000000000000, 0.8660254037844387076, 1.000000000000000000, 0.8660254037844387076, 1.000000000000000000, 0.8660254037844387076, 1.000000000000000000, 0.8660254037844387076, 1.000000000000000000, 0.8660254037844387076, 1.000000000000000000, 0.8660254037844387076, 1.000000000000000000, 0.8660254037844387076, 1.000000000000000000, 0.8660254037844387076, 1.000000000000000000, 0.8660254037844387076, 1.000000000000000000, 0.8660254037844387076, 1.000000000000000000, 0.8660254037844387076, 1.000000000000000000, 0.8660254037844387076, 1.000000000000000000, 0.8660254037844387076, 1.000000000000000000, 0.8660254037844387076, 1.000000000000000000, 0.8660254037844387076, 1.000000000000000000, 0.8660254037844387076, 1.000000000000000000, 0.8660254037844387076, 1.000000000000000000, 0.8660254037844387076, 1.000000000000000000, 0.8660254037844387076, 1.000000000000000000, 0.8660254037844387076, 1.000000000000000000, 0.8660254037844387076, 1.000000000000000000, 0.8660254037844387076, 1.000000000000000000, 0.8660254037844387076, 1.000000000000000000, 0.8660254037844387076, 1.000000000000000000, 0.8660254037844387076, 1.000000000000000000, 0.8660254037844387076, 1.000000000000000000, 0.8660254037844387076, 1.000000000000000000, 0.8660254037844387076, 1.000000000000000000, 0.8660254037844387076, 1.000000000000000000, 0.8660254037844387076, 1.000000000000000000, 0.8660254037844387076, 1.000000000000000000, 0.8660254037844387076, 1.000000000000000000, 0.8660254037844387076, 1.000000000000000000, 0.8660254037844387076, 1.000000000000000000, 0.8660254037844387076, 1.000000000000000000, 0.8660254037844387076, 1.000000000000000000, 0.8660254037844387076, 1.000000000000000000, 0.8660254037844387076, 1.000000000000000000, 0.8660254037844387076, 1.000000000000000000, 0.8660254037844387076, 1.000000000000000000, 0.8660254037844387076, 1.000000000000000000, 0.8660254037844387076, 1.000000000000000000, 0.8660254037844387076, 1.000000000000000000, 0.8660254037844387076, 1.000000000000000000, 0.8660254037844387076, 1.000000000000000000, 0.8660254037844387076, 1.000000000000000000, 0.8660254037844387076, 1.000000000000000000, 0.8660254037844387076, 1.000000000000000000, 0.8660254037844387076, 1.000000000000000000, 0.8660254037844387076, 1.000000000000000000, 0.8660254037844387076, 1.000000000000000000, 0.8660254037844387076, 1.000000000000000000, 0.8660254037844387076, 1.000000000000000000, 0.8660254037844387076, 1.000000000000000000, 0.8660254037844387076, 1.000000000000000000, 0.8660254037844387076, 1.000000000000000000, 0.8660254037844387076, 1.000000000000000000, 0.8660254037844387076, 1.000000000000000000, 0.8660254037844387076, 1.000000000000000000, 0.8660254037844387076, 1.000000000000000000, 0.8660254037844387076, 1.000000000000000000, 0.8660254037844387076, 1.000000000000000000, 0.8660254037844387076, 1.000000000000000000, 0.8660254037844387076, 1.000000000000000000, 0.8660254037844387076, 1.000000000000000000, 0.8660254037844387076, 1.000000000000000000, 0.8660254037844387076, 1.000000000000000000, 0.8660254037844387076, 1.000000000000000000, 0.8660254037844387076, 1.000000000000000000, 0.8660254037844387076, 1.000000000000000000, 0.8660254037844387076, 1.000000000000000000, 0.8660254037844387076, 1.000000000000000000, 0.8660254037844387076, 1.000000000000000000, 0.8660254037844387076, 1.000000000000000000, 0.8660254037844387076, 1.000000000000000000, 0.8660254037844387076, 1.000000000000000000, 0.8660254037844387076, 1.000000000000000000, 0.8660254037844387076, 1.000000000000000000, 0.8660254037844387076, 1.000000000000000000, 0.8660254037844387076, 1.000000000000000000, 0.8660254037844387076, 1.000000000000000000, 0.8660254037844387076, 1.000000000000000000, 0.8660254037844387076, 1.000000000000000000, 0.8660254037844387076, 1.000000000000000000, 0.8660254037844387076, 1.000000000000000000, 0.8660254037844387076, 1.000000000000000000, 0.8660254037844387076, 1.000000000000000000, 0.8660254037844387076, 1.000000000000000000, 0.8660254037844387076, 1.000000000000000000, 0.8660254037844387076, 1.000000000000000000, 0.8660254037844387076, 1.000000000000000000, 0.8660254037844387076, 1.000000000000000000, 0.8660254037844387076, 1.000000000000000000, 0.8660254037844387076, 1.000000000000000000, 0.8660254037844387076, 1.000000000000000000, 0.8660254037844387076, 1.000000000000000000, 0.8660254037844387076, 1.000000000000000000, 0.8660254037844387076, 1.000000000000000000, 0.8660254037844387076, 1.000000000000000000, 0.8660254037844387076, 1.000000000000000000, 0.8660254037844387076, 1.000000000000000000, 0.8660254037844387076, 1.000000000000000000, 0.8660254037844387076, 1.000000000000000000, 0.8660254037844387076, 1.000000000000000000, 0.8660254037844387076, 1.000000000000000000, 0.8660254037844387076, 1.000000000000000000, 0.8660254037844387076, 1.000000000000000000, 0.8660254037844387076, 1.000000000000000000, 0.8660254037844387076, 1.000000000000000000, 0.8660254037844387076, 1.000000000000000000, 0.8660254037844387076, 1.000000000000000000, 0.8660254037844387076, 1.000000000000000000, 0.8660254037844387076, 1.000000000000000000, 0.8660254037844387076, 1.000000000000000000, 0.8660254037844387076, 1.000000000000000000, 0.8660254037844387076, 1.000000000000000000, 0.8660254037844387076, 1.000000000000000000, 0.8660254037844387076, 1.000000000000000000, 0.8660254037844387076, 1.000000000000000000, 0.8660254037844387076, 1.000000000000000000, 0.8660254037844387076, 1.000000000000000000, 0.8660254037844387076, 1.000000000000000000, 0.8660254037844387076, 1.000000000000000000, 0.8660254037844387076, 1.000000000000000000, 0.8660254037844387076, 1.000000000000000000, 0.8660254037844387076, 1.000000000000000000, 0.8660254037844387076, 1.000000000000000000, 0.8660254037844387076, 1.000000000000000000, 0.8660254037844387076, 1.000000000000000000, 0.8660254037844387076, 1.000000000000000000, 0.8660254037844387076, 1.000000000000000000, 0.8660254037844387076, 1.000000000000000000, 0.8660254037844387076, 1.000000000000000000, 0.8660254037844387076, 1.000000000000000000, 0.8660254037844387076, 1.000000000000000000, 0.8660254037844387076, 1.000000000000000000, 0.8660254037844387076, 1.000000000000000000, 0.8660254037844387076, 1.000000000000000000, 0.8660254037844387076, 1.000000000000000000, 0.8660254037844387076, 1.000000000000000000, 0.8660254037844387076, 1.000000000000000000, 0.8660254037844387076, 1.000000000000000000, 0.8660254037844387076, 1.000000000000000000, 0.8660254037844387076, 1.000000000000000000, 0.8660254037844387076, 1.000000000000000000, 0.8660254037844387076, 1.000000000000000000, 0.8660254037844387076, 1.000000000000000000, 0.8660254037844387076, 1.000000000000000000, 0.8660254037844387076, 1.000000000000000000, 0.8660254037844387076, 1.000000000000000000, 0.8660254037844387076, 1.000000000000000000, 0.8660254037844387076, 1.000000000000000000, 0.8660254037844387076, 1.000000000000000000, 0.8660254037844387076, 1.000000000000000000, 0.8660254037844387076, 1.000000000000000000, 0.8660254037844387076, 1.000000000000000000, 0.8660254037844387076, 1.000000000000000000, 0.8660254037844387076, 1.000000000000000000, 0.8660254037844387076, 1.000000000000000000, 0.8660254037844387076, 1.000000000000000000, 0.8660254037844387076, 1.000000000000000000, 0.8660254037844387076, 1.000000000000000000, 0.8660254037844387076, 1.000000000000000000, 0.8660254037844387076, 1.000000000000000000, 0.8660254037844387076, 1.000000000000000000, 0.8660254037844387076, 1.000000000000000000, 0.8660254037844387076, 1.000000000000000000, 0.8660254037844387076, 1.000000000000000000, 0.8660254037844387076, 1.000000000000000000, 0.8660254037844387076, 1.000000000000000000, 0.8660254037844387076, 1.000000000000000000, 0.8660254037844387076, 1.000000000000000000, 0.8660254037844387076, 1.000000000000000000, 0.8660254037844387076, 1.000000000000000000, 0.8660254037844387076, 1.000000000000000000, 0.8660254037844387076, 1.000000000000000000, 0.8660254037844387076, 1.000000000000000000, 0.8660254037844387076, 1.000000000000000000, 0.8660254037844387076, 1.000000000000000000, 0.8660254037844387076, 1.000000000000000000, 0.8660254037844387076, 1.000000000000000000, 0.8660254037844387076, 1.000000000000000000, 0.8660254037844387076, 1.000000000000000000, 0.8660254037844387076, 1.000000000000000000, 0.8660254037844387076, 1.000000000000000000, 0.8660254037844387076, 1.000000000000000000, 0.8660254037844387076, 1.000000000000000000, 0.8660254037844387076, 1.000000000000000000, 0.8660254037844387076, 1.000000000000000000, 0.8660254037844387076, 1.000000000000000000, 0.8660254037844387076, 1.000000000000000000, 0.8660254037844387076, 1.000000000000000000, 0.8660254037844387076, 1.000000000000000000, 0.8660254037844387076, 1.000000000000000000, 0.8660254037844387076, 1.000000000000000000, 0.8660254037844387076, 1.000000000000000000, 0.8660254037844387076, 1.000000000000000000, 0.8660254037844387076, 1.000000000000000000, 0.8660254037844387076, 1.000000000000000000, 0.8660254037844387076, 1.000000000000000000, 0.8660254037844387076, 1.000000000000000000, 0.8660254037844387076, 1.000000000000000000, 0.8660254037844387076, 1.000000000000000000) ) ) 
 REPRESENTATION_ITEM ( '' )  SURFACE ( )  );
#59930 = CARTESIAN_POINT ( 'NONE',  ( 147.5693121967435957, 275.0494489676833041, 4.210973343677100189 ) ) ;
#59931 = CARTESIAN_POINT ( 'NONE',  ( 81.85611950375817969, 41.21271484795168760, -5.731628893815098102 ) ) ;
#59932 = CARTESIAN_POINT ( 'NONE',  ( -19.65312891409030271, 93.06504152958497400, 59.99999999999999289 ) ) ;
#59933 = CYLINDRICAL_SURFACE ( 'NONE', #17441, 1.449999999999993072 ) ;
#59934 = DIRECTION ( 'NONE',  ( 0.000000000000000000, -1.000000000000000000, 1.060575238724906175E-16 ) ) ;
#59935 = CARTESIAN_POINT ( 'NONE',  ( 100.3908607700757187, 228.7677522451418497, 10.00000000000009592 ) ) ;
#59936 = ORIENTED_EDGE ( 'NONE', *, *, #27387, .F. ) ;
#59937 = CARTESIAN_POINT ( 'NONE',  ( 79.26974131400612578, 59.52036692680489693, -16.53359576550785803 ) ) ;
#59938 = CARTESIAN_POINT ( 'NONE',  ( 162.6220573360242270, 248.9773295930640131, 10.49878733418918486 ) ) ;
#59939 = CARTESIAN_POINT ( 'NONE',  ( 80.18492040316456837, 47.57055350794450987, -13.79677460666521149 ) ) ;
#59940 = ADVANCED_FACE ( 'NONE', ( #92009 ), #66761, .T. ) ;
#59941 = CARTESIAN_POINT ( 'NONE',  ( 12.94935828348961593, 178.2833772461660544, -9.188101187500095079 ) ) ;
#59942 = CARTESIAN_POINT ( 'NONE',  ( 66.18968672761215544, 68.49487770601442094, -4.881532527435783919 ) ) ;
#59943 = CARTESIAN_POINT ( 'NONE',  ( 193.3216912985990916, 272.5173147653680417, 14.22613245673542259 ) ) ;
#59944 = CARTESIAN_POINT ( 'NONE',  ( 192.4335622838504207, 297.3422883733380786, -12.83044365323471325 ) ) ;
#59945 = CARTESIAN_POINT ( 'NONE',  ( 50.20806676147353187, 85.59215312471712878, -10.00000000000000000 ) ) ;
#59947 = CARTESIAN_POINT ( 'NONE',  ( 64.36996372895568186, 195.7202760586659167, -5.415160957724236172E-17 ) ) ;
#59946 = CARTESIAN_POINT ( 'NONE',  ( 175.0941756799416567, 286.4970703408308736, 10.49273659814999604 ) ) ;
#59948 = CARTESIAN_POINT ( 'NONE',  ( 207.6471633721571379, 270.9915583223058206, 2.196965492132801678 ) ) ;
#59949 = CARTESIAN_POINT ( 'NONE',  ( 203.9641523903856353, 276.3974457028200504, 13.34757937729907873 ) ) ;
#59950 = CARTESIAN_POINT ( 'NONE',  ( 70.58107171170311744, 70.42171057263509226, 5.244054101350007713 ) ) ;
#59951 = CARTESIAN_POINT ( 'NONE',  ( 66.41207382487917243, 68.05599230888550721, -4.871615717380384680 ) ) ;
#59952 = EDGE_LOOP ( 'NONE', ( #31563, #52957, #99823, #68014, #46416 ) ) ;
#59953 = CARTESIAN_POINT ( 'NONE',  ( 164.8638179515183424, 269.0684537314152749, 17.58025323075393587 ) ) ;
#59954 = CARTESIAN_POINT ( 'NONE',  ( 16.11576366785039127, 190.1115022471903160, -5.000000000000047962 ) ) ;
#59955 = CARTESIAN_POINT ( 'NONE',  ( 207.6932907333322191, 270.9116633891313199, 2.120963121341169710 ) ) ;
#59956 = CARTESIAN_POINT ( 'NONE',  ( 142.8531688511554307, 253.2833772461660544, -9.188101187500095079 ) ) ;
#59957 = CARTESIAN_POINT ( 'NONE',  ( 24.17276070933917609, 32.14336893147756768, 7.433330006724141015 ) ) ;
#59958 = CARTESIAN_POINT ( 'NONE',  ( 164.2980929276580468, 246.0743507930604608, 1.884825537327208478 ) ) ;
#59959 = CARTESIAN_POINT ( 'NONE',  ( 85.33699565288863198, 48.33901173460944278, -12.30238903177781395 ) ) ;
#59960 = CARTESIAN_POINT ( 'NONE',  ( 176.6558404752379090, 252.2237374370411942, -0.2705739152901737166 ) ) ;
#59962 = CARTESIAN_POINT ( 'NONE',  ( 189.5765870809536580, 289.5964489643898219, 15.12308329164838128 ) ) ;
#59961 = CARTESIAN_POINT ( 'NONE',  ( 88.21274111123641148, 43.92339361237885953, 2.502205135834638217 ) ) ;
#59963 = CARTESIAN_POINT ( 'NONE',  ( 68.83067416445564390, 64.29043214222643599, 12.51914382770813461 ) ) ;
#59964 = VERTEX_POINT ( 'NONE', #71173 ) ;
#59965 = DIRECTION ( 'NONE',  ( 0.9994538543569184696, -0.03304531753667278027, 0.000000000000000000 ) ) ;
#59966 = CARTESIAN_POINT ( 'NONE',  ( 163.9377421930003607, 246.6984965740322480, 8.856459175406742546 ) ) ;
#59967 = CARTESIAN_POINT ( 'NONE',  ( 192.7686961758011250, 263.9209412561240811, -8.347089341778378468 ) ) ;
#59968 = CARTESIAN_POINT ( 'NONE',  ( 169.1830573458304627, 254.2960580516546827, 12.91860015404840389 ) ) ;
#59969 = CARTESIAN_POINT ( 'NONE',  ( 197.2578275771767551, 273.1615466810303587, -13.38357264611757103 ) ) ;
#59970 = ORIENTED_EDGE ( 'NONE', *, *, #15181, .T. ) ;
#59971 = DIRECTION ( 'NONE',  ( -0.8660254037844387076, -0.4999999999999998890, -0.000000000000000000 ) ) ;
#59972 = CARTESIAN_POINT ( 'NONE',  ( 170.1929779583345237, 284.3448978393517450, -11.77788885849169453 ) ) ;
#59973 = CARTESIAN_POINT ( 'NONE',  ( 71.64147408072075507, 72.45736481867632506, 0.9627058344235318588 ) ) ;
#59974 = DIRECTION ( 'NONE',  ( -0.4972609476841356457, 0.8612812260087758798, 0.1045284632676436315 ) ) ;
#59975 = CARTESIAN_POINT ( 'NONE',  ( 203.2757866645317222, 269.5093088776978334, -7.514607224931010521 ) ) ;
#59976 = DIRECTION ( 'NONE',  ( 0.4999999999999992784, -0.8660254037844390407, 0.000000000000000000 ) ) ;
#59977 = CARTESIAN_POINT ( 'NONE',  ( 68.57078111580027269, 69.83554316562776876, 3.250710778096809417 ) ) ;
#59978 = VECTOR ( 'NONE', #53323, 1000.000000000000000 ) ;
#59979 = CARTESIAN_POINT ( 'NONE',  ( -46.49770490450612215, 29.77544742692501600, 10.00000000000000000 ) ) ;
#59980 = ORIENTED_EDGE ( 'NONE', *, *, #18521, .T. ) ;
#59981 = DIRECTION ( 'NONE',  ( 0.4999999999999992784, -0.8660254037844390407, 0.000000000000000000 ) ) ;
#59982 = CARTESIAN_POINT ( 'NONE',  ( 19.88154021482007749, 11.28848085856230377, 1.475505719884397138E-15 ) ) ;
#59983 = CARTESIAN_POINT ( 'NONE',  ( 84.09923392499968031, 48.62025565107681047, 13.03358251092844000 ) ) ;
#59984 = EDGE_LOOP ( 'NONE', ( #49457, #37432, #56757, #17016 ) ) ;
#59985 = DIRECTION ( 'NONE',  ( -0.8660254037844387076, -0.4999999999999998890, -0.000000000000000000 ) ) ;
#59986 = CARTESIAN_POINT ( 'NONE',  ( 86.15665200708443194, 46.94614013873178493, -10.61509939557872073 ) ) ;
#59987 = CARTESIAN_POINT ( 'NONE',  ( 84.69910869649594076, 45.11611167524748822, -8.770891836413943210 ) ) ;
#59988 = ORIENTED_EDGE ( 'NONE', *, *, #1667, .F. ) ;
#59989 = CARTESIAN_POINT ( 'NONE',  ( 191.7187529716733820, 298.5803744197520473, -8.487597704798396592 ) ) ;
#59990 = CARTESIAN_POINT ( 'NONE',  ( 79.42275183545125117, 59.70681295713441727, -16.17365378312262436 ) ) ;
#59991 = CARTESIAN_POINT ( 'NONE',  ( 204.8189571845487080, 275.8901551335242175, 13.43702398685204358 ) ) ;
#59992 = CARTESIAN_POINT ( 'NONE',  ( 87.34642337659644795, 43.20430561321286689, -4.696387144280492735E-07 ) ) ;
#59993 = CARTESIAN_POINT ( 'NONE',  ( 69.35253854973147725, 63.01665765329197910, 13.58811665792164014 ) ) ;
#59994 = ORIENTED_EDGE ( 'NONE', *, *, #97722, .F. ) ;
#59995 = CARTESIAN_POINT ( 'NONE',  ( 87.34609280552280097, 230.4244531367911009, -4.594050593750046652 ) ) ;
#59996 = CARTESIAN_POINT ( 'NONE',  ( 198.7838390185755770, 282.9248331187500298, 17.36760380735526610 ) ) ;
#59997 = CARTESIAN_POINT ( 'NONE',  ( 68.62032050481585088, 70.74532250035436221, 0.7225376792652218327 ) ) ;
#59998 = CARTESIAN_POINT ( 'NONE',  ( 81.60031397647219364, 42.64669660525676420, -7.620194330344577160 ) ) ;
#59999 = ORIENTED_EDGE ( 'NONE', *, *, #91252, .T. ) ;
#60000 = ORIENTED_EDGE ( 'NONE', *, *, #55161, .T. ) ;
#60001 = EDGE_CURVE ( 'NONE', #52454, #70967, #253, .T. ) ;
#60002 = CARTESIAN_POINT ( 'NONE',  ( 207.1548490022400415, 270.0363760279268490, 1.710376025867456962 ) ) ;
#60003 = ORIENTED_EDGE ( 'NONE', *, *, #34434, .F. ) ;
#60004 = CARTESIAN_POINT ( 'NONE',  ( 81.56554115986412512, 50.74390853957432057, 14.52805404999391214 ) ) ;
#60006 = ORIENTED_EDGE ( 'NONE', *, *, #93688, .F. ) ;
#60005 = B_SPLINE_CURVE_WITH_KNOTS ( 'NONE', 3,
 ( #58296, #29402, #31382, #52679 ),
 .UNSPECIFIED., .F., .F.,
 ( 4, 4 ),
 ( 0.003581673450268924204, 0.009034217805257406531 ),
 .UNSPECIFIED. ) ;
#60007 = EDGE_CURVE ( 'NONE', #50040, #91566, #54403, .T. ) ;
#60008 = CARTESIAN_POINT ( 'NONE',  ( 203.9697818395143258, 267.9997349688208601, 0.5926888351516317321 ) ) ;
#60009 = ORIENTED_EDGE ( 'NONE', *, *, #58199, .T. ) ;
#60010 = CARTESIAN_POINT ( 'NONE',  ( 164.6921227768849008, 245.3918710745008127, 2.498195641553966340 ) ) ;
#60011 = EDGE_CURVE ( 'NONE', #62487, #36092, #86914, .T. ) ;
#60012 = B_SPLINE_CURVE_WITH_KNOTS ( 'NONE', 3,
 ( #22814, #84651, #7108, #78025 ),
 .UNSPECIFIED., .F., .F.,
 ( 4, 4 ),
 ( 0.03712676085629124101, 0.04575313303586313329 ),
 .UNSPECIFIED. ) ;
#60013 = DIRECTION ( 'NONE',  ( -0.9514785060800223793, 0.3077152132536332130, 0.000000000000000000 ) ) ;
#60014 = ADVANCED_FACE ( 'NONE', ( #9876 ), #40734, .T. ) ;
#60015 = CARTESIAN_POINT ( 'NONE',  ( 82.81701024667485456, 53.37631690731208778, -15.29776186725079334 ) ) ;
#60016 = CARTESIAN_POINT ( 'NONE',  ( 164.8146514257492186, 264.9101748124866162, -16.65136860934597252 ) ) ;
#60017 = ORIENTED_EDGE ( 'NONE', *, *, #62596, .T. ) ;
#60018 = CARTESIAN_POINT ( 'NONE',  ( 76.68531899032339538, 59.74883463824316010, 15.90439264542311726 ) ) ;
#60019 = CARTESIAN_POINT ( 'NONE',  ( 7.668962567711002265, 16.37878583063838533, 9.188101187500006262 ) ) ;
#60020 = ORIENTED_EDGE ( 'NONE', *, *, #15064, .F. ) ;
#60021 = CARTESIAN_POINT ( 'NONE',  ( 164.9015738923758079, 282.0469085907977274, 8.845953399109694359 ) ) ;
#60023 = EDGE_LOOP ( 'NONE', ( #39096, #98813, #40072, #62361 ) ) ;
#60022 = CARTESIAN_POINT ( 'NONE',  ( 206.9022815319215738, 270.8307493124123084, 4.969621876343158107 ) ) ;
#60024 = CARTESIAN_POINT ( 'NONE',  ( 202.9689790241539242, 279.0944113002206564, 15.85114608332523289 ) ) ;
#60025 = CARTESIAN_POINT ( 'NONE',  ( 184.9789842570080793, 258.2806869971382184, 2.961155574049133765 ) ) ;
#60026 = CARTESIAN_POINT ( 'NONE',  ( 157.9648834242245528, 279.9874070561871804, -6.790362339845969153 ) ) ;
#60027 = PLANE ( 'NONE',  #74895 ) ;
#60028 = CARTESIAN_POINT ( 'NONE',  ( 192.7517790942337683, 292.1482192696278162, -14.59390454542270099 ) ) ;
#60029 = CARTESIAN_POINT ( 'NONE',  ( 85.73939067079162157, 43.09395395977590226, 3.031127533106598548 ) ) ;
#60030 = CARTESIAN_POINT ( 'NONE',  ( 194.6806917771430392, 263.4467307442432684, -0.7818862912174471269 ) ) ;
#60031 = ORIENTED_EDGE ( 'NONE', *, *, #40157, .T. ) ;
#60032 = CARTESIAN_POINT ( 'NONE',  ( 181.6970786337707864, 271.3723858492330123, -15.97957702204227282 ) ) ;
#60033 = CARTESIAN_POINT ( 'NONE',  ( 160.6790552449755864, 275.7503919994865100, 12.80081933329241473 ) ) ;
#60034 = CARTESIAN_POINT ( 'NONE',  ( 14.65434579541631521, 169.2677522451417929, -5.000000000000041744 ) ) ;
#60035 = CARTESIAN_POINT ( 'NONE',  ( 196.1195291313601672, 269.4854874125175570, -10.82207891638150521 ) ) ;
#60036 = CARTESIAN_POINT ( 'NONE',  ( 175.0419018616888991, 281.4530265013858070, -14.15648744962207672 ) ) ;
#60037 = CARTESIAN_POINT ( 'NONE',  ( 163.6328441044221620, 247.2265955545804275, -8.943872350901562740 ) ) ;
#60038 = DIRECTION ( 'NONE',  ( -0.000000000000000000, 1.000000000000000000, -0.000000000000000000 ) ) ;
#60039 = CARTESIAN_POINT ( 'NONE',  ( 164.7062239463616606, 274.2877436771660200, 14.86310344068559885 ) ) ;
#60041 = CARTESIAN_POINT ( 'NONE',  ( 33.32252067603396029, 20.20801979619930577, -3.090169943749474069 ) ) ;
#60040 = CARTESIAN_POINT ( 'NONE',  ( 2.746756816977958593, 163.2048013555410080, 4.594050593750051981 ) ) ;
#60042 = CARTESIAN_POINT ( 'NONE',  ( 164.0651280066704771, 248.4778578725967861, 9.975266483072225299 ) ) ;
#60043 = VERTEX_POINT ( 'NONE', #75594 ) ;
#60044 = EDGE_LOOP ( 'NONE', ( #52554, #72628, #68857, #78076 ) ) ;
#60045 = PLANE ( 'NONE',  #57961 ) ;
#60046 = CARTESIAN_POINT ( 'NONE',  ( 127.4000280541508516, 234.3615022471901739, 5.000000000000051514 ) ) ;
#60047 = CARTESIAN_POINT ( 'NONE',  ( 171.7465271196784897, 289.8775964799340841, 2.715013937588829140 ) ) ;
#60048 = FACE_OUTER_BOUND ( 'NONE', #94584, .T. ) ;
#60049 = AXIS2_PLACEMENT_3D ( 'NONE', #96918, #81709, #5170 ) ;
#60050 = CARTESIAN_POINT ( 'NONE',  ( 203.4435754520237651, 276.2723861740593634, 14.48166091637323483 ) ) ;
#60051 = CARTESIAN_POINT ( 'NONE',  ( 84.82223274050802786, 47.96708222389427334, 11.74877015797738622 ) ) ;
#60052 = CARTESIAN_POINT ( 'NONE',  ( 150.2121420128144678, 276.5610649638679774, 3.689409684367604303 ) ) ;
#60053 = B_SPLINE_CURVE_WITH_KNOTS ( 'NONE', 3,
 ( #39185, #77217, #6820, #14431 ),
 .UNSPECIFIED., .F., .F.,
 ( 4, 4 ),
 ( 0.04707519336486235689, 0.04887066958154942520 ),
 .UNSPECIFIED. ) ;
#60054 = CARTESIAN_POINT ( 'NONE',  ( 23.50386934422995822, 190.5024278399160949, -9.188101187500093303 ) ) ;
#60055 = CARTESIAN_POINT ( 'NONE',  ( 122.6912752411227103, 232.4548013555409796, -4.594050593750042211 ) ) ;
#60056 = CARTESIAN_POINT ( 'NONE',  ( 87.84668905185571930, 44.44462267732798466, -3.943169391390685341 ) ) ;
#60057 = CARTESIAN_POINT ( 'NONE',  ( 183.2120991357361106, 257.6510318301264419, -2.908943044801409972 ) ) ;
#60058 = CARTESIAN_POINT ( 'NONE',  ( 79.27428326626197475, 58.12688789515522103, 16.22428513376493342 ) ) ;
#60059 = CARTESIAN_POINT ( 'NONE',  ( 48.87252615048947746, 107.3561085985702874, 177.5919119679930134 ) ) ;
#60060 = EDGE_CURVE ( 'NONE', #13198, #49332, #60356, .T. ) ;
#60061 = CARTESIAN_POINT ( 'NONE',  ( 78.47336120520917291, 54.13984261423279776, -15.94495912723520625 ) ) ;
#60062 = CARTESIAN_POINT ( 'NONE',  ( 185.4206969650253711, 260.4038640631882231, 9.453313016594156792 ) ) ;
#60063 = CARTESIAN_POINT ( 'NONE',  ( 161.8807657183444064, 250.2612843381103573, -13.52770735624900311 ) ) ;
#60064 = DIRECTION ( 'NONE',  ( 0.6313854049612632746, 0.7754691937155863135, 0.000000000000000000 ) ) ;
#60065 = LINE ( 'NONE', #21592, #70812 ) ;
#60066 = DIRECTION ( 'NONE',  ( -0.7080737730998298840, 0.7061384650677022812, 0.000000000000000000 ) ) ;
#60067 = CARTESIAN_POINT ( 'NONE',  ( 196.5634515809505842, 266.6633299776104309, 8.168478504490389369 ) ) ;
#60068 = FACE_OUTER_BOUND ( 'NONE', #63627, .T. ) ;
#60069 = CARTESIAN_POINT ( 'NONE',  ( 184.4468480456720840, 268.5537564916724023, -15.62460610151881291 ) ) ;
#60070 = CYLINDRICAL_SURFACE ( 'NONE', #62650, 17.82106496071139645 ) ;
#60071 = CARTESIAN_POINT ( 'NONE',  ( 188.1412547211656943, 273.5593357346770063, 17.08033167198486879 ) ) ;
#60072 = EDGE_CURVE ( 'NONE', #37857, #55385, #20901, .T. ) ;
#60073 = CARTESIAN_POINT ( 'NONE',  ( 102.8537940617441819, 224.0643266524160140, 9.188101187500095079 ) ) ;
#60074 = CARTESIAN_POINT ( 'NONE',  ( 9.573022157908470220, 14.03085787977760646, 9.188101187500006262 ) ) ;
#60075 = CARTESIAN_POINT ( 'NONE',  ( 191.0170959869219303, 299.7956799668270946, 7.353346939903929069 ) ) ;
#60076 = CARTESIAN_POINT ( 'NONE',  ( 159.1113560326100753, 259.2834188555653441, -17.54322067557006903 ) ) ;
#60078 = CARTESIAN_POINT ( 'NONE',  ( 151.9298993999875904, 267.4966903808301026, 16.91367899156788468 ) ) ;
#60077 = CARTESIAN_POINT ( 'NONE',  ( 157.0935036675524827, 258.5530654392286465, 17.32636058289560665 ) ) ;
#60079 = DIRECTION ( 'NONE',  ( 0.5000000000000048850, -0.8660254037844358210, 0.000000000000000000 ) ) ;
#60080 = CARTESIAN_POINT ( 'NONE',  ( 198.4860348845112981, 286.8590983175747056, -18.20461732983060088 ) ) ;
#60081 = CARTESIAN_POINT ( 'NONE',  ( -19.65312891409030271, 9.999999999999994671, 54.99999999999999289 ) ) ;
#60082 = CARTESIAN_POINT ( 'NONE',  ( 42.15419773769040290, 26.19860640527295814, 2.839279412974134775 ) ) ;
#60083 = CARTESIAN_POINT ( 'NONE',  ( 193.2100161762185735, 295.9974307820218087, -12.46499585622781758 ) ) ;
#60084 = FACE_BOUND ( 'NONE', #11035, .T. ) ;
#60085 = ORIENTED_EDGE ( 'NONE', *, *, #26577, .F. ) ;
#60086 = CARTESIAN_POINT ( 'NONE',  ( 23.51121325743158508, 19.28920272979927120, -7.433330006724141015 ) ) ;
#60087 = DIRECTION ( 'NONE',  ( -0.8660254037844387076, -0.4999999999999998890, -0.000000000000000000 ) ) ;
#60088 = DIRECTION ( 'NONE',  ( -0.7763215174174871169, 0.6303371332823493045, 0.000000000000000000 ) ) ;
#60089 = CARTESIAN_POINT ( 'NONE',  ( 196.9319848161575806, 289.5507919934690335, -17.64330560362266453 ) ) ;
#60090 = B_SPLINE_CURVE_WITH_KNOTS ( 'NONE', 3,
 ( #61241, #51671, #59745, #13183, #29857, #75989, #44039, #36449, #7546, #75473, #6058, #91689, #45538, #14662, #74979, #67352, #30356, #36952, #20780, #67863, #6566, #46029, #5560, #37931, #98281, #99274, #38438, #37439, #76470, #53154, #7050, #53639, #69352, #100271, #84594, #959, #38940, #77966, #9059, #25250, #48561, #55629, #10063, #70863, #23737, #8561, #79502, #86614, #40928, #458 ),
 .UNSPECIFIED., .F., .F.,
 ( 4, 2, 2, 2, 2, 2, 2, 2, 2, 2, 2, 2, 2, 2, 2, 2, 2, 2, 2, 2, 2, 2, 2, 2, 4 ),
 ( 0.0003281754202554149351, 0.0008006094400505323408, 0.001273043459845649584, 0.001509260469743186088, 0.001627368974692035329, 0.001745477479640884571, 0.001981694489538647890, 0.002217911499436411426, 0.002690345519231964518, 0.003162779539027517611, 0.004107647578618566983, 0.005052515618209615922, 0.005524949638005215852, 0.005761166647903014949, 0.005879275152851915799, 0.005938329405326366224, 0.005997383657800815782, 0.006056437910275266207, 0.006115492162749716631, 0.006233600667698616614, 0.006469817677596420916, 0.006942251697392027784, 0.007414685717187633786, 0.007650902727085504007, 0.007887119736983375096 ),
 .UNSPECIFIED. ) ;
#60091 = VERTEX_POINT ( 'NONE', #23359 ) ;
#60092 = CARTESIAN_POINT ( 'NONE',  ( 70.80219251493628008, 60.87566219113961807, 14.54675205938061744 ) ) ;
#60093 = CARTESIAN_POINT ( 'NONE',  ( 159.7897726928491409, 253.8829904965402875, 16.83923858130328810 ) ) ;
#60094 = CARTESIAN_POINT ( 'NONE',  ( 157.7660523726510462, 268.4465589492402842, 16.76385752021615261 ) ) ;
#60095 = DIRECTION ( 'NONE',  ( 0.8660254037844379305, 0.5000000000000011102, 0.000000000000000000 ) ) ;
#60096 = CARTESIAN_POINT ( 'NONE',  ( 140.8234218128095847, 262.1115022471903444, -5.000000000000047962 ) ) ;
#60097 = VERTEX_POINT ( 'NONE', #7676 ) ;
#60098 = CARTESIAN_POINT ( 'NONE',  ( 70.27693386828532596, 63.84783520667136258, 13.41007760784634151 ) ) ;
#60099 = EDGE_LOOP ( 'NONE', ( #53431, #57518, #85736, #25020, #49179, #80907, #34061, #58413, #80109, #12875, #36441, #36110, #72665, #78379, #28637, #1840, #24867, #74978, #41854, #46695 ) ) ;
#60100 = CARTESIAN_POINT ( 'NONE',  ( 195.7229849017213610, 265.1195584955938216, -4.418747677595802337 ) ) ;
#60101 = CARTESIAN_POINT ( 'NONE',  ( 82.87596643829704135, 41.15858874971023340, 0.1873015203630768732 ) ) ;
#60102 = ORIENTED_EDGE ( 'NONE', *, *, #68341, .F. ) ;
#60103 = CARTESIAN_POINT ( 'NONE',  ( 185.2143418923794798, 292.5124672671021244, -10.69479488396104827 ) ) ;
#60104 = ORIENTED_EDGE ( 'NONE', *, *, #30205, .T. ) ;
#60105 = CARTESIAN_POINT ( 'NONE',  ( 86.43879872498249028, 47.50144577818752367, -11.01113278173270693 ) ) ;
#60106 = CARTESIAN_POINT ( 'NONE',  ( 206.2356669332361605, 273.4363418692194045, 11.05590195897326922 ) ) ;
#60107 = CARTESIAN_POINT ( 'NONE',  ( 190.6061379745418094, 278.8388338309181904, -16.51655004129774795 ) ) ;
#60108 = FACE_OUTER_BOUND ( 'NONE', #33198, .T. ) ;
#60109 = CARTESIAN_POINT ( 'NONE',  ( 152.7295469705997277, 266.1116601603806657, -17.40211458100010589 ) ) ;
#60110 = DIRECTION ( 'NONE',  ( 0.4737039832092511671, 0.8806841296921895657, 0.000000000000000000 ) ) ;
#60111 = CARTESIAN_POINT ( 'NONE',  ( 35.31444455405989657, 43.49540643055190969, 3.479690158560446702E-15 ) ) ;
#60112 = PLANE ( 'NONE',  #42944 ) ;
#60113 = EDGE_CURVE ( 'NONE', #5348, #61424, #10844, .T. ) ;
#60114 = DIRECTION ( 'NONE',  ( 0.000000000000000000, 0.000000000000000000, 1.000000000000000000 ) ) ;
#60115 = CARTESIAN_POINT ( 'NONE',  ( 72.84042761573121538, 202.8615022471901739, 5.000000000000051514 ) ) ;
#60116 = ORIENTED_EDGE ( 'NONE', *, *, #64577, .T. ) ;
#60117 = AXIS2_PLACEMENT_3D ( 'NONE', #21502, #28589, #91426 ) ;
#60118 = ORIENTED_EDGE ( 'NONE', *, *, #46263, .F. ) ;
#60119 = CARTESIAN_POINT ( 'NONE',  ( 205.2391015854675516, 275.1624436846170738, -14.01434138479280911 ) ) ;
#60120 = CARTESIAN_POINT ( 'NONE',  ( 182.5892408154444695, 296.6611350254266313, 0.3217610282793219589 ) ) ;
#60122 = CARTESIAN_POINT ( 'NONE',  ( 194.1789525331299728, 294.3191837825503967, -15.34533909744314961 ) ) ;
#60121 = CARTESIAN_POINT ( 'NONE',  ( 174.1046625087539894, 257.2888617342148336, -11.85904880942999107 ) ) ;
#60123 = DIRECTION ( 'NONE',  ( 0.000000000000000000, 0.000000000000000000, 1.000000000000000000 ) ) ;
#60124 = CARTESIAN_POINT ( 'NONE',  ( 197.9761018079605606, 272.1676159484598543, -13.70813156040953729 ) ) ;
#60125 = CARTESIAN_POINT ( 'NONE',  ( 13.75631770279071020, 31.55236904046464375, -10.00000000000000000 ) ) ;
#60126 = CARTESIAN_POINT ( 'NONE',  ( 82.48576119632784298, 40.42786996717531167, 0.9267432163235941323 ) ) ;
#60127 = CARTESIAN_POINT ( 'NONE',  ( 170.5330744639767033, 287.4519228453978599, -4.620264690464154889 ) ) ;
#60128 = EDGE_CURVE ( 'NONE', #12155, #14695, #75338, .T. ) ;
#60129 = CARTESIAN_POINT ( 'NONE',  ( 77.31442247797616574, 63.22349627092265223, -15.21530826047764862 ) ) ;
#60130 = CARTESIAN_POINT ( 'NONE',  ( 186.7687816609699212, 286.9689498124462261, -15.64156219619770560 ) ) ;
#60131 = B_SPLINE_CURVE_WITH_KNOTS ( 'NONE', 3,
 ( #4072, #37820, #91082, #14046, #45910, #15019, #96822, #84477, #89243, #91568, #27380, #58266, #19793, #76359, #50661, #68729, #60613, #61118 ),
 .UNSPECIFIED., .F., .F.,
 ( 4, 2, 2, 2, 2, 2, 2, 2, 4 ),
 ( 0.0001987964186102976830, 0.0003140683529223511493, 0.0003717043200783778554, 0.0004293402872344046156, 0.0004581582708124750519, 0.0004869762543905454882, 0.0005446122215466848429, 0.0006598841558589985720, 0.001120971893108076763 ),
 .UNSPECIFIED. ) ;
#60132 = CARTESIAN_POINT ( 'NONE',  ( 118.1174918034448922, 232.8768266524160140, 9.188101187500098632 ) ) ;
#60133 = ORIENTED_EDGE ( 'NONE', *, *, #50506, .T. ) ;
#60134 = CARTESIAN_POINT ( 'NONE',  ( 184.0739800145211120, 260.1317561499213298, -9.673630312158074673 ) ) ;
#60135 = CARTESIAN_POINT ( 'NONE',  ( 27.20206195878591870, 37.74646525600392266, 2.839279412974139660 ) ) ;
#60136 = DIRECTION ( 'NONE',  ( 0.000000000000000000, 0.000000000000000000, 1.000000000000000000 ) ) ;
#60137 = EDGE_LOOP ( 'NONE', ( #22661, #15368, #82519 ) ) ;
#60138 = EDGE_LOOP ( 'NONE', ( #66904, #59138, #77867, #2471 ) ) ;
#60139 = CARTESIAN_POINT ( 'NONE',  ( 74.18796447308154995, 68.76651203251665834, -11.36463150814737766 ) ) ;
#60140 = CARTESIAN_POINT ( 'NONE',  ( 164.4902401177012337, 246.2554029907234678, -2.428734258964198034 ) ) ;
#60141 = CARTESIAN_POINT ( 'NONE',  ( 195.9359860111818250, 291.2759125279654882, 17.49638312768267312 ) ) ;
#60142 = CARTESIAN_POINT ( 'NONE',  ( 31.58830253577720626, 26.43677371833803136, -10.00000000000000355 ) ) ;
#60143 = CARTESIAN_POINT ( 'NONE',  ( 15.16022976130349065, 27.49103043416548431, -8.090169943749479842 ) ) ;
#60144 = EDGE_LOOP ( 'NONE', ( #3057, #12581, #50282, #19075 ) ) ;
#60145 = CARTESIAN_POINT ( 'NONE',  ( 195.5149407638684522, 292.0051842885976043, 15.88854587925930772 ) ) ;
#60146 = ORIENTED_EDGE ( 'NONE', *, *, #69288, .T. ) ;
#60147 = CARTESIAN_POINT ( 'NONE',  ( 30.34687108590969373, 93.06504152958497400, 60.00000000000000000 ) ) ;
#60148 = VERTEX_POINT ( 'NONE', #45172 ) ;
#60149 = CARTESIAN_POINT ( 'NONE',  ( 35.47817891544688251, 110.9002400656976022, 59.99999999999999289 ) ) ;
#60150 = CARTESIAN_POINT ( 'NONE',  ( 192.7079119722239113, 262.6034417676851263, 4.671215074061198180 ) ) ;
#60151 = CARTESIAN_POINT ( 'NONE',  ( 155.5311623832600958, 261.6886619413561448, 17.00987194985870943 ) ) ;
#60152 = CARTESIAN_POINT ( 'NONE',  ( 83.76918405636864406, 48.70819753632389393, 12.74357695574461147 ) ) ;
#60154 = CARTESIAN_POINT ( 'NONE',  ( 69.82388864200702017, 62.78505363333596279, -13.30987185219257718 ) ) ;
#60153 = PLANE ( 'NONE',  #4772 ) ;
#60155 = CARTESIAN_POINT ( 'NONE',  ( 200.7134601498536028, 283.0010845879393742, -16.98649239173277792 ) ) ;
#60156 = ORIENTED_EDGE ( 'NONE', *, *, #32497, .F. ) ;
#60157 = DIRECTION ( 'NONE',  ( -0.4999999999999987788, 0.8660254037844392627, 0.000000000000000000 ) ) ;
#60158 = CARTESIAN_POINT ( 'NONE',  ( 82.14295211724746082, 50.23227492270505223, 14.12545005886346772 ) ) ;
#60159 = CARTESIAN_POINT ( 'NONE',  ( 82.10416747357091083, 41.15855318747237135, -3.445724401907877432 ) ) ;
#60160 = DIRECTION ( 'NONE',  ( 0.000000000000000000, 0.000000000000000000, 1.000000000000000000 ) ) ;
#60161 = CARTESIAN_POINT ( 'NONE',  ( 189.0232759416005877, 269.9725822948850578, -14.03890638026795301 ) ) ;
#60162 = DIRECTION ( 'NONE',  ( 0.5000000000000014433, -0.8660254037844378194, 0.000000000000000000 ) ) ;
#60163 = CARTESIAN_POINT ( 'NONE',  ( -19.52110968745198250, 93.01322780128255374, 59.99999999999999289 ) ) ;
#60164 = DIRECTION ( 'NONE',  ( 0.000000000000000000, -0.000000000000000000, 1.000000000000000000 ) ) ;
#60165 = CARTESIAN_POINT ( 'NONE',  ( 23.57265107556306916, 195.9637435831424739, 2.679491924311251605 ) ) ;
#60166 = CARTESIAN_POINT ( 'NONE',  ( 72.06082664650362801, 70.73905283940008815, -6.476476296684364975 ) ) ;
#60167 = CARTESIAN_POINT ( 'NONE',  ( 70.32319418844367931, 223.6589784336661921, -6.496448406907675876E-16 ) ) ;
#60168 = CARTESIAN_POINT ( 'NONE',  ( 206.1615484827472358, 273.5647187912443314, -9.556459874778100883 ) ) ;
#60169 = DIRECTION ( 'NONE',  ( -1.000000000000000000, 0.000000000000000000, 0.000000000000000000 ) ) ;
#60170 = CARTESIAN_POINT ( 'NONE',  ( 208.3586375946586315, 269.7592488206576604, -1.970210487958146128 ) ) ;
#60171 = CARTESIAN_POINT ( 'NONE',  ( 13.90223112049948639, 33.06302660730329279, -10.00000000000000000 ) ) ;
#60172 = EDGE_CURVE ( 'NONE', #60539, #12691, #8181, .T. ) ;
#60173 = CARTESIAN_POINT ( 'NONE',  ( 161.2133744761260061, 251.4172398781588811, -14.30368667312104058 ) ) ;
#60174 = CARTESIAN_POINT ( 'NONE',  ( -58.10760318826260118, 36.06970723555270553, -10.00000000000000000 ) ) ;
#60175 = CARTESIAN_POINT ( 'NONE',  ( -20.81253355169515018, 95.09634674671917764, 45.19948544083312214 ) ) ;
#60176 = CARTESIAN_POINT ( 'NONE',  ( 116.1416978049531110, 237.8615022471902307, -10.00000000000009592 ) ) ;
#60177 = ADVANCED_FACE ( 'NONE', ( #84228 ), #84714, .T. ) ;
#60178 = CARTESIAN_POINT ( 'NONE',  ( 37.05984716305037807, 40.13478043621391578, 8.090169943749478065 ) ) ;
#60179 = CARTESIAN_POINT ( 'NONE',  ( -46.49770490450612215, 29.77544742692501600, -10.00000000000000000 ) ) ;
#60180 = CARTESIAN_POINT ( 'NONE',  ( 82.78345634833958400, 53.69061190982763776, 15.38144188222361386 ) ) ;
#60181 = CARTESIAN_POINT ( 'NONE',  ( 71.72870690310715247, 72.16142621409359492, 3.283488654313290844 ) ) ;
#60182 = CARTESIAN_POINT ( 'NONE',  ( 24.64070123457955219, 185.0333772461660544, 9.188101187500095079 ) ) ;
#60183 = B_SPLINE_CURVE_WITH_KNOTS ( 'NONE', 3,
 ( #34538, #65436, #98352, #74563, #20854, #27452, #21334, #29429, #13729, #59303, #12759, #20348, #27928, #21825, #4640, #52218, #58326, #83164, #82687, #5627, #98853, #90784, #28941, #36520, #67421, #97362, #28423, #51219, #73549, #82187, #35025, #44606, #13254, #43622, #36021, #4132, #52711, #59817, #35533, #44112, #37023, #66922, #60303, #75540, #6126, #58811, #51745, #67931 ),
 .UNSPECIFIED., .F., .F.,
 ( 4, 2, 2, 2, 2, 2, 2, 2, 2, 2, 2, 2, 2, 2, 2, 2, 2, 2, 2, 2, 2, 2, 2, 4 ),
 ( 0.0004489931541215139068, 0.001462873357728531861, 0.001969813459531987061, 0.002223283510433714770, 0.002350018535884506633, 0.002476753561335297629, 0.002730223612236896968, 0.002983693663138495440, 0.003490633764941693251, 0.004504513968548151323, 0.005518394172154609395, 0.006025334273957838431, 0.006278804324859453383, 0.006532274375761068334, 0.006595641888486466868, 0.006659009401211866269, 0.006722376913937264803, 0.006785744426662664204, 0.007039214477564325126, 0.007546154579367791819, 0.007799624630269523864, 0.008053094681171255043, 0.008306564732072987955, 0.008560034782974719134 ),
 .UNSPECIFIED. ) ;
#60184 = ADVANCED_FACE ( 'NONE', ( #44659 ), #92806, .F. ) ;
#60185 = CARTESIAN_POINT ( 'NONE',  ( 171.9695299662907360, 276.3046275190319534, -16.98996149290084645 ) ) ;
#60186 = CARTESIAN_POINT ( 'NONE',  ( 43.71265818875933462, 33.43677371833805267, -10.00000000000000355 ) ) ;
#60187 = CARTESIAN_POINT ( 'NONE',  ( 164.1654149204426858, 248.3041558426086226, -9.671695341034215687 ) ) ;
#60188 = CARTESIAN_POINT ( 'NONE',  ( 71.70482085610929346, 72.04085231235103493, -1.605959201768876410 ) ) ;
#60189 = CARTESIAN_POINT ( 'NONE',  ( 59.90443346675090908, 196.2048013555409796, 4.594050593750051981 ) ) ;
#60190 = CARTESIAN_POINT ( 'NONE',  ( 21.14648969749996965, 33.18502408145592142, 5.678558825948276656 ) ) ;
#60191 = CARTESIAN_POINT ( 'NONE',  ( 198.8157103782086210, 286.2880836124806478, -18.60729372713428020 ) ) ;
#60192 = DIRECTION ( 'NONE',  ( 0.8755176446346986108, -0.4831861483251662648, 0.000000000000000000 ) ) ;
#60193 = CARTESIAN_POINT ( 'NONE',  ( 44.08964769951546714, 27.58380873178791148, 6.180339887498953466 ) ) ;
#60194 = CARTESIAN_POINT ( 'NONE',  ( 9.830230629461709668, 30.95267373526311516, -10.00000000000000000 ) ) ;
#60195 = CARTESIAN_POINT ( 'NONE',  ( 202.9470114082288319, 270.0688303170933864, -6.543538759376999359 ) ) ;
#60196 = CARTESIAN_POINT ( 'NONE',  ( 175.4799100621144134, 291.2742715687741679, 2.018303699312502086 ) ) ;
#60197 = CARTESIAN_POINT ( 'NONE',  ( 176.8361213315729117, 275.2114496154293306, 16.59131570778482256 ) ) ;
#60198 = CARTESIAN_POINT ( 'NONE',  ( 73.54743893589137826, 64.98868938413073693, 13.35376214375427217 ) ) ;
#60199 = CARTESIAN_POINT ( 'NONE',  ( 70.04496804106824470, 67.88492258065853946, -9.012774590751471138 ) ) ;
#60200 = DIRECTION ( 'NONE',  ( 0.4999999999999998890, -0.8660254037844385966, 0.000000000000000000 ) ) ;
#60201 = EDGE_CURVE ( 'NONE', #14882, #26754, #46668, .T. ) ;
#60202 = CARTESIAN_POINT ( 'NONE',  ( 35.32845566053276087, 49.32197259295687530, -10.00000000000000000 ) ) ;
#60204 =( BOUNDED_CURVE ( )  B_SPLINE_CURVE ( 2, ( #59159, #82040, #90646, #43972, #90133, #35389, #67792, #43479, #98716 ),
 .UNSPECIFIED., .F., .T. ) 
 B_SPLINE_CURVE_WITH_KNOTS ( ( 3, 2, 2, 2, 3 ),
 ( 0.9556451612903226200, 0.9569892473118279952, 0.9596774193548387455, 0.9623655913978494958, 0.9637096774193548709 ),
 .UNSPECIFIED. ) 
 CURVE ( )  GEOMETRIC_REPRESENTATION_ITEM ( )  RATIONAL_B_SPLINE_CURVE ( ( 0.9330127018922194093, 0.9330127018922194093, 1.000000000000000000, 0.8660254037844387076, 1.000000000000000000, 0.8660254037844387076, 1.000000000000000000, 0.9330127018922194093, 0.9330127018922194093 ) ) 
 REPRESENTATION_ITEM ( '' )  );
#60203 = CARTESIAN_POINT ( 'NONE',  ( 98.02733310912863374, 220.7365022471901739, -10.00000000000009059 ) ) ;
#60205 = DIRECTION ( 'NONE',  ( 0.4999999999999992784, -0.8660254037844390407, 0.000000000000000000 ) ) ;
#60206 = LINE ( 'NONE', #21731, #72527 ) ;
#60207 = EDGE_LOOP ( 'NONE', ( #16762, #80857, #64283, #39151 ) ) ;
#60208 = CARTESIAN_POINT ( 'NONE',  ( 58.44249495421716745, 213.7369531367911293, -4.594050593750048428 ) ) ;
#60209 = ORIENTED_EDGE ( 'NONE', *, *, #25364, .F. ) ;
#60210 = CARTESIAN_POINT ( 'NONE',  ( 166.2774799739476066, 265.1959323007807257, 16.57056821886706288 ) ) ;
#60211 = CARTESIAN_POINT ( 'NONE',  ( 190.7908437487391780, 300.1875603386860689, -4.317984972589949955 ) ) ;
#60212 = DIRECTION ( 'NONE',  ( -0.000000000000000000, 0.000000000000000000, -1.000000000000000000 ) ) ;
#60213 = ORIENTED_EDGE ( 'NONE', *, *, #3885, .F. ) ;
#60214 = DIRECTION ( 'NONE',  ( 1.000000000000000000, 0.000000000000000000, 2.816764622163176013E-16 ) ) ;
#60215 = CARTESIAN_POINT ( 'NONE',  ( 79.21691572551614513, 45.75049196499858084, -12.99762880459370784 ) ) ;
#60216 = CARTESIAN_POINT ( 'NONE',  ( 193.5629084239263307, 292.5061527191514870, -15.60167767085171242 ) ) ;
#60217 = CARTESIAN_POINT ( 'NONE',  ( 73.10684881258417533, 70.60603909402131251, -7.845798253817742207 ) ) ;
#60218 = CARTESIAN_POINT ( 'NONE',  ( 206.6742118400747756, 271.5744752743144659, -6.599374785183829140 ) ) ;
#60219 = CARTESIAN_POINT ( 'NONE',  ( 115.9793180381956716, 227.7677522451417929, -5.000000000000041744 ) ) ;
#60221 = VERTEX_POINT ( 'NONE', #69962 ) ;
#60220 = VECTOR ( 'NONE', #34692, 1000.000000000000114 ) ;
#60222 = CARTESIAN_POINT ( 'NONE',  ( 20.65934362447757167, 23.87878583063841376, -9.188101187500006262 ) ) ;
#60223 = CARTESIAN_POINT ( 'NONE',  ( 75.61128893809926410, 57.78454237761125256, 16.06483355829618986 ) ) ;
#60224 = CARTESIAN_POINT ( 'NONE',  ( 67.76226342272079251, 69.50789913810500309, -2.504574930950261624 ) ) ;
#60225 = CARTESIAN_POINT ( 'NONE',  ( 167.9496373820661290, 248.6204696539478789, -6.517719931589019744 ) ) ;
#60226 = ADVANCED_FACE ( 'NONE', ( #83216 ), #577, .T. ) ;
#60227 = EDGE_CURVE ( 'NONE', #30330, #9173, #49649, .T. ) ;
#60228 = ORIENTED_EDGE ( 'NONE', *, *, #73902, .F. ) ;
#60229 = CARTESIAN_POINT ( 'NONE',  ( 182.6429660890904074, 283.7719756040974062, 15.79391243952982649 ) ) ;
#60230 = CARTESIAN_POINT ( 'NONE',  ( 206.6912923161529818, 272.6471755567893638, -9.325620632947922317 ) ) ;
#60231 = ORIENTED_EDGE ( 'NONE', *, *, #28811, .T. ) ;
#60232 = EDGE_CURVE ( 'NONE', #1644, #84697, #49186, .T. ) ;
#60234 = DIRECTION ( 'NONE',  ( 0.9646071681523454844, -0.2636911283094535152, 0.000000000000000000 ) ) ;
#60233 = DIRECTION ( 'NONE',  ( -1.000000000000000000, 0.000000000000000000, 0.000000000000000000 ) ) ;
#60235 = CARTESIAN_POINT ( 'NONE',  ( 162.7007457333762090, 248.8410372908842021, -10.94671474643812914 ) ) ;
#60236 = CARTESIAN_POINT ( 'NONE',  ( 204.9432097630379417, 275.6749433546094679, 13.74700047688257776 ) ) ;
#60237 = CARTESIAN_POINT ( 'NONE',  ( 190.0667283601964357, 259.9641452334862493, -5.090329199819447104E-14 ) ) ;
#60238 = CARTESIAN_POINT ( 'NONE',  ( 81.53661897590532703, 55.80016554358400072, 16.37044094275388417 ) ) ;
#60239 = CARTESIAN_POINT ( 'NONE',  ( 161.0844399624414507, 263.0064568173025350, -17.38383432207021784 ) ) ;
#60240 = CARTESIAN_POINT ( 'NONE',  ( 125.2075541532825014, 255.3464784336661353, 1.353441290958777525E-15 ) ) ;
#60241 = EDGE_CURVE ( 'NONE', #16392, #33130, #66623, .T. ) ;
#60242 = VECTOR ( 'NONE', #97944, 1000.000000000000114 ) ;
#60243 = CARTESIAN_POINT ( 'NONE',  ( 81.74442484449845381, 211.8768266524159856, 9.188101187500098632 ) ) ;
#60244 = ORIENTED_EDGE ( 'NONE', *, *, #9599, .T. ) ;
#60245 = CARTESIAN_POINT ( 'NONE',  ( 174.1398777777984037, 265.6557655336882249, 16.43872977299918503 ) ) ;
#60246 = CARTESIAN_POINT ( 'NONE',  ( 1.638219116881074022, 26.38162155862025671, 10.00000000000000000 ) ) ;
#60247 = EDGE_LOOP ( 'NONE', ( #32452, #10434, #20423, #92227 ) ) ;
#60248 = CARTESIAN_POINT ( 'NONE',  ( 160.2539783940571851, 253.8594209733300318, 15.13163501824758228 ) ) ;
#60249 = ORIENTED_EDGE ( 'NONE', *, *, #11054, .F. ) ;
#60250 = ORIENTED_EDGE ( 'NONE', *, *, #32562, .F. ) ;
#60251 = EDGE_CURVE ( 'NONE', #72476, #45307, #60916, .T. ) ;
#60252 = DIRECTION ( 'NONE',  ( -0.000000000000000000, 0.000000000000000000, -1.000000000000000000 ) ) ;
#60253 = CARTESIAN_POINT ( 'NONE',  ( 66.62639878018896411, 67.83600655791506995, 6.946500236981309584 ) ) ;
#60254 = EDGE_CURVE ( 'NONE', #44553, #49678, #40044, .T. ) ;
#60255 = CARTESIAN_POINT ( 'NONE',  ( 196.9422331689194152, 286.2628525950418634, 16.90547485990039789 ) ) ;
#60256 = B_SPLINE_CURVE_WITH_KNOTS ( 'NONE', 3,
 ( #18555, #43321, #27652, #74267, #42323, #26146, #58036, #33758, #73744, #97083 ),
 .UNSPECIFIED., .F., .F.,
 ( 4, 2, 2, 2, 4 ),
 ( 0.000000000000000000, 0.2500000000000000000, 0.5000000000000000000, 0.7500000000000000000, 1.000000000000000000 ),
 .UNSPECIFIED. ) ;
#60257 = CARTESIAN_POINT ( 'NONE',  ( -32.94356256989595977, 94.88921800892812541, 10.61543114587583503 ) ) ;
#60258 = CARTESIAN_POINT ( 'NONE',  ( 81.46866702687000839, 55.81909161095428829, 16.37896761046575378 ) ) ;
#60259 = CARTESIAN_POINT ( 'NONE',  ( 193.9966098916996771, 294.6350105018939871, 13.97117019253516013 ) ) ;
#60260 = CARTESIAN_POINT ( 'NONE',  ( 71.11923220532735002, 65.88429979018354743, 11.70261362563623386 ) ) ;
#60261 = CARTESIAN_POINT ( 'NONE',  ( 182.5067194347547854, 257.1923330838238826, -6.222426465989368438 ) ) ;
#60262 = ORIENTED_EDGE ( 'NONE', *, *, #89430, .F. ) ;
#60263 = CARTESIAN_POINT ( 'NONE',  ( -19.65312891409030271, 93.06504152958497400, -10.00000000000000888 ) ) ;
#60264 = DIRECTION ( 'NONE',  ( -0.6647600172776847449, 0.7470569720101488675, 0.000000000000000000 ) ) ;
#60265 = ORIENTED_EDGE ( 'NONE', *, *, #38061, .F. ) ;
#60266 = B_SPLINE_CURVE_WITH_KNOTS ( 'NONE', 3,
 ( #25459, #87349, #1171, #18374, #79708, #26967, #20365, #75066, #65952, #43129, #52239, #13270, #82204, #12775, #20870, #51761, #5645, #67440, #73083, #57848, #28957, #83183, #34556, #65456, #29940, #76074, #51, #14739, #92770, #91776, #38016, #30436, #53719, #67948, #61325, #84679, #60321, #46629, #69925, #542, #15219, #77030, #38527, #29444, #80083, #2049, #41526, #33962 ),
 .UNSPECIFIED., .F., .F.,
 ( 4, 2, 2, 2, 2, 2, 2, 2, 2, 2, 2, 2, 2, 2, 2, 2, 2, 2, 2, 2, 2, 2, 2, 4 ),
 ( 0.002098688353426452196, 0.002534572199440611722, 0.002752514122447782992, 0.002970456045454953828, 0.003079427006958539680, 0.003188397968462125531, 0.003297368929965711383, 0.003406339891469296801, 0.003624281814476544399, 0.003842223737483791562, 0.004713991429512820117, 0.005585759121541849538, 0.006457526813570877225, 0.006893410659585395839, 0.007329294505599914453, 0.007438265467103608725, 0.007492750947855422033, 0.007547236428607235342, 0.007656207390110858491, 0.007765178351614485108, 0.008201062197628897904, 0.008636946043643310700, 0.008854887966650496281, 0.009072829889657683597 ),
 .UNSPECIFIED. ) ;
#60267 = CARTESIAN_POINT ( 'NONE',  ( 76.12238913165759868, 51.10370791208713115, -15.58940357410317468 ) ) ;
#60268 = CARTESIAN_POINT ( 'NONE',  ( 173.9990153864150670, 253.4041716863320062, -7.605893656024731442 ) ) ;
#60269 = CARTESIAN_POINT ( 'NONE',  ( 186.8006684768011212, 276.5875442340776544, 17.70268152755913604 ) ) ;
#60270 = CARTESIAN_POINT ( 'NONE',  ( 196.3507576896697344, 290.5575069072837664, -17.68249398312240928 ) ) ;
#60271 = DIRECTION ( 'NONE',  ( 0.000000000000000000, 0.000000000000000000, 1.000000000000000000 ) ) ;
#60272 = CYLINDRICAL_SURFACE ( 'NONE', #51259, 70.00000000000002842 ) ;
#60273 = CARTESIAN_POINT ( 'NONE',  ( 140.0928864244750685, 245.5643266524160424, -9.188101187500093303 ) ) ;
#60274 = EDGE_LOOP ( 'NONE', ( #38695, #90963, #5177, #53406 ) ) ;
#60275 = CARTESIAN_POINT ( 'NONE',  ( 80.09120749856197108, 44.41673742825524585, -10.86461196121644157 ) ) ;
#60276 = CARTESIAN_POINT ( 'NONE',  ( 182.9163764445669642, 258.7192441424419371, 6.406310776454488654 ) ) ;
#60277 = CARTESIAN_POINT ( 'NONE',  ( 155.9683004480747286, 261.9866473075522322, -16.96465910183697900 ) ) ;
#60278 = CARTESIAN_POINT ( 'NONE',  ( 73.06696598015496136, 70.66213948254207367, 7.705144097525488789 ) ) ;
#60279 = CARTESIAN_POINT ( 'NONE',  ( 73.78116818605872140, 66.73777287303562389, -12.34320005290799394 ) ) ;
#60280 = ORIENTED_EDGE ( 'NONE', *, *, #11007, .T. ) ;
#60281 = CARTESIAN_POINT ( 'NONE',  ( 77.51198627597376856, 60.98384281500086956, 15.82258133188943106 ) ) ;
#60282 = CARTESIAN_POINT ( 'NONE',  ( 182.1414478339540040, 275.7655165773919634, -16.43324961048260846 ) ) ;
#60283 = FACE_OUTER_BOUND ( 'NONE', #52658, .T. ) ;
#60284 = DIRECTION ( 'NONE',  ( 0.8606332181800098180, -0.5092253565614340838, 0.000000000000000000 ) ) ;
#60285 = CARTESIAN_POINT ( 'NONE',  ( 81.13117295687578689, 52.04838968429105250, 15.10467803161753331 ) ) ;
#60286 = CARTESIAN_POINT ( 'NONE',  ( 202.5535515909786000, 267.2301142524262332, 0.8809907921587507573 ) ) ;
#60287 = CARTESIAN_POINT ( 'NONE',  ( 198.4976171291946514, 266.2161181449658898, 0.6785798567533030123 ) ) ;
#60288 = CARTESIAN_POINT ( 'NONE',  ( 190.9380839614473473, 299.9325328093580652, -5.232187664503159752 ) ) ;
#60289 = CARTESIAN_POINT ( 'NONE',  ( 184.2669327163933986, 281.3015570470274724, 16.28411061875366173 ) ) ;
#60290 = AXIS2_PLACEMENT_3D ( 'NONE', #64329, #38652, #87707 ) ;
#60291 = EDGE_CURVE ( 'NONE', #5719, #21768, #72319, .T. ) ;
#60292 = CARTESIAN_POINT ( 'NONE',  ( 193.0780078417625703, 268.7414322461000893, 12.24939826239815055 ) ) ;
#60293 = CIRCLE ( 'NONE', #73291, 17.82106496071138935 ) ;
#60294 = ADVANCED_FACE ( 'NONE', ( #62352 ), #93820, .T. ) ;
#60295 = B_SPLINE_SURFACE_WITH_KNOTS ( 'NONE', 3, 1, ( 
 ( #38931, #69836 ),
 ( #448, #62223 ),
 ( #23727, #16144 ),
 ( #6048, #67855 ),
 ( #98776, #94185 ),
 ( #71361, #93685 ),
 ( #17655, #71867 ),
 ( #78463, #57129 ),
 ( #950, #55621 ),
 ( #56641, #39917 ),
 ( #8550, #18153 ),
 ( #2465, #24738 ),
 ( #63748, #64244 ),
 ( #49052, #79988 ),
 ( #41432, #38312 ),
 ( #60606, #69221 ),
 ( #61612, #77331 ),
 ( #38813, #325 ),
 ( #62101, #29245 ),
 ( #52039, #13553 ),
 ( #78340, #78846 ),
 ( #94066, #95073 ),
 ( #70211, #40304 ),
 ( #71747, #63621 ),
 ( #48932, #24125 ),
 ( #1837, #54497 ),
 ( #79871, #25114 ),
 ( #25636, #41305 ),
 ( #56518, #87506 ),
 ( #72248, #85476 ),
 ( #3831, #35719 ) ),
 .UNSPECIFIED., .F., .F., .F.,
 ( 4, 3, 3, 3, 3, 3, 3, 3, 3, 3, 4 ),
 ( 2, 2 ),
 ( 0.000000000000000000, 0.1122669598086740300, 0.2243161639709581601, 0.3396355846219040742, 0.4553962076585059138, 0.5677860799922319623, 0.6749047109689451096, 0.7773884377078192909, 0.8775581155834162317, 0.9782364162377708006, 1.000000000000000000 ),
 ( 0.000000000000000000, 1.000000000000000000 ),
 .UNSPECIFIED. ) ;
#60296 = CARTESIAN_POINT ( 'NONE',  ( 26.29472225869274382, 23.38052372038642091, 10.00000000000000533 ) ) ;
#60297 = DIRECTION ( 'NONE',  ( -0.4999999999999982792, 0.8660254037844398178, 0.000000000000000000 ) ) ;
#60298 = CARTESIAN_POINT ( 'NONE',  ( 205.3385343418334230, 274.5435030208487319, 11.21992643350996843 ) ) ;
#60299 = CARTESIAN_POINT ( 'NONE',  ( 67.28775127781241849, 69.02525132645125439, -5.181563858835234626 ) ) ;
#60300 = CARTESIAN_POINT ( 'NONE',  ( 198.6587626159274294, 286.5599251108861267, 17.99840276545888784 ) ) ;
#60301 = CARTESIAN_POINT ( 'NONE',  ( 193.0758421513005487, 292.7688076435337621, 15.33214366454828692 ) ) ;
#60302 = CARTESIAN_POINT ( 'NONE',  ( 149.3212960838965557, 247.0177522451417644, 5.000000000000051514 ) ) ;
#60303 = CARTESIAN_POINT ( 'NONE',  ( 175.4720935967913533, 286.3835187628145036, -12.16069689870089121 ) ) ;
#60304 = ORIENTED_EDGE ( 'NONE', *, *, #60787, .F. ) ;
#60305 = ADVANCED_FACE ( 'NONE', ( #87256 ), #40559, .F. ) ;
#60307 = CARTESIAN_POINT ( 'NONE',  ( 66.49880604618508073, 67.93642891560753583, -6.609368650527830624 ) ) ;
#60306 = VECTOR ( 'NONE', #30221, 1000.000000000000114 ) ;
#60308 = CARTESIAN_POINT ( 'NONE',  ( 72.45751905151222161, 70.67373443742414452, -7.865264308201653343 ) ) ;
#60309 = CARTESIAN_POINT ( 'NONE',  ( 150.6438662863770332, 269.7241650738195631, -14.92510732909997628 ) ) ;
#60310 = CARTESIAN_POINT ( 'NONE',  ( -0.2035760843690503918, 176.8149278399160949, -9.188101187500095079 ) ) ;
#60311 = CARTESIAN_POINT ( 'NONE',  ( 30.57965140047823738, 19.78380873178787880, -6.180339887498949025 ) ) ;
#60312 = CARTESIAN_POINT ( 'NONE',  ( 85.51397903554266122, 48.65227260402726017, 12.46570927396283146 ) ) ;
#60313 = CARTESIAN_POINT ( 'NONE',  ( 65.24466313315720356, 215.1427522451419065, -10.00000000000009592 ) ) ;
#60314 = CARTESIAN_POINT ( 'NONE',  ( 71.87910863004675832, 71.70566666627038899, -3.826659594235088946 ) ) ;
#60315 = CARTESIAN_POINT ( 'NONE',  ( 78.14015596324891533, 47.79605781560269406, 14.53813849190288465 ) ) ;
#60316 = B_SPLINE_SURFACE_WITH_KNOTS ( 'NONE', 3, 1, ( 
 ( #84694, #91791 ),
 ( #13759, #62334 ),
 ( #38032, #68448 ),
 ( #61838, #37056 ),
 ( #98881, #37542 ),
 ( #93285, #29955 ),
 ( #92785, #44638 ),
 ( #15235, #85194 ),
 ( #99376, #46646 ),
 ( #15738, #68942 ),
 ( #77571, #22356 ),
 ( #53253, #8159 ),
 ( #67963, #45636 ),
 ( #558, #92302 ),
 ( #45152, #6160 ),
 ( #14754, #52740 ),
 ( #76564, #29461 ),
 ( #30453, #60336 ),
 ( #91293, #61343 ),
 ( #21858, #83702 ),
 ( #6665, #36342 ),
 ( #13567, #76366 ),
 ( #6456, #37334 ),
 ( #91089, #52536 ),
 ( #53037, #30245 ),
 ( #6938, #21654 ),
 ( #28246, #22147 ),
 ( #99160, #90605 ),
 ( #14557, #83487 ),
 ( #92103, #99659 ),
 ( #90094, #4969 ),
 ( #82990, #66745 ),
 ( #61126, #14053 ),
 ( #97680, #67244 ) ),
 .UNSPECIFIED., .T., .F., .F.,
 ( 4, 2, 2, 2, 2, 2, 2, 2, 2, 2, 2, 2, 2, 2, 2, 2, 4 ),
 ( 2, 2 ),
 ( 0.000000000000000000, 0.06250000000000000000, 0.1250000000000000000, 0.1875000000000000000, 0.2500000000000000000, 0.3125000000000000000, 0.3750000000000000000, 0.4375000000000000000, 0.5000000000000000000, 0.5625000000000000000, 0.6250000000000000000, 0.6875000000000000000, 0.7500000000000000000, 0.8125000000000000000, 0.8750000000000000000, 0.9375000000000000000, 1.000000000000000000 ),
 ( 0.000000000000000000, 1.000000000000000000 ),
 .UNSPECIFIED. ) ;
#60317 = DIRECTION ( 'NONE',  ( 0.8660254037844399289, 0.4999999999999977240, -0.000000000000000000 ) ) ;
#60318 = EDGE_CURVE ( 'NONE', #10254, #7154, #62864, .T. ) ;
#60319 = CARTESIAN_POINT ( 'NONE',  ( 198.6701036545953230, 286.5402818557027445, 17.25253558010639310 ) ) ;
#60320 = EDGE_CURVE ( 'NONE', #10093, #60091, #76330, .T. ) ;
#60321 = CARTESIAN_POINT ( 'NONE',  ( 183.1064801743427211, 295.7402259981610655, 1.177175515638812398 ) ) ;
#60322 = CARTESIAN_POINT ( 'NONE',  ( 57.68498304950353628, 194.1115022471902023, -5.000000000000041744 ) ) ;
#60323 = FACE_OUTER_BOUND ( 'NONE', #46950, .T. ) ;
#60324 = CARTESIAN_POINT ( 'NONE',  ( 147.8503508990560533, 274.5626756563852950, 7.845851077393495743 ) ) ;
#60325 = CARTESIAN_POINT ( 'NONE',  ( 16.79251956066557128, 174.3768266524160140, 9.188101187500098632 ) ) ;
#60326 = CARTESIAN_POINT ( 'NONE',  ( 164.3787126659294131, 284.8162412357542621, 4.248981773088212677 ) ) ;
#60327 = CARTESIAN_POINT ( 'NONE',  ( 153.0070714074088016, 265.6309737354857248, 17.74442213480098474 ) ) ;
#60328 = CARTESIAN_POINT ( 'NONE',  ( 44.05945362601616466, 27.29860640527295956, -2.839279412974138328 ) ) ;
#60329 = CARTESIAN_POINT ( 'NONE',  ( 201.2339362457151992, 280.2550766807431160, -16.75742611627472911 ) ) ;
#60330 = CYLINDRICAL_SURFACE ( 'NONE', #35329, 17.82106496071139645 ) ;
#60331 = CARTESIAN_POINT ( 'NONE',  ( 189.1997833930358013, 268.1800545106789286, 13.86060302672411382 ) ) ;
#60332 = CARTESIAN_POINT ( 'NONE',  ( 149.1653648461108617, 275.5304674000249179, 7.618651205328232479 ) ) ;
#60333 = CARTESIAN_POINT ( 'NONE',  ( 164.0858594112551430, 281.5537891919451567, 8.872571969112266643 ) ) ;
#60334 = PRODUCT_CONTEXT ( 'NONE', #46600, 'mechanical' ) ;
#60335 = CARTESIAN_POINT ( 'NONE',  ( 20.93478768117288524, 17.80170272979926338, 7.433330006724137462 ) ) ;
#60336 = CARTESIAN_POINT ( 'NONE',  ( 148.3837145175834280, 273.6388627701866767, 8.841971351370922605 ) ) ;
#60337 = CARTESIAN_POINT ( 'NONE',  ( 71.84836080304555139, 59.06364556286701628, 15.37505501383178519 ) ) ;
#60338 = CARTESIAN_POINT ( 'NONE',  ( 194.4263876777154394, 293.8906135405502482, 15.23185943445137802 ) ) ;
#60339 = EDGE_LOOP ( 'NONE', ( #96005, #59713, #21532, #57403 ) ) ;
#60340 = CARTESIAN_POINT ( 'NONE',  ( 86.19897734768302655, 45.52340696477872939, -8.150747010710539087 ) ) ;
#60341 = CARTESIAN_POINT ( 'NONE',  ( 85.27924949840783597, 45.45504446614027927, -9.497384621978497421 ) ) ;
#60342 = CARTESIAN_POINT ( 'NONE',  ( 75.10336920942704353, 53.49933058092891258, -16.05324734149355237 ) ) ;
#60343 = CARTESIAN_POINT ( 'NONE',  ( 88.25515730755107313, 44.35562341810459941, 2.525333633695516333 ) ) ;
#60344 = EDGE_LOOP ( 'NONE', ( #68961, #7664, #31148, #77141 ) ) ;
#60345 = PLANE ( 'NONE',  #40855 ) ;
#60346 = CARTESIAN_POINT ( 'NONE',  ( 82.39721099668476256, 40.42262220707492304, 1.474573639734337860 ) ) ;
#60347 = CARTESIAN_POINT ( 'NONE',  ( 76.88576290890495102, 63.85744880123300504, 14.90658078946527354 ) ) ;
#60348 = CARTESIAN_POINT ( 'NONE',  ( 203.2187760522547819, 278.6617501559703101, -15.08675642319914978 ) ) ;
#60349 = VERTEX_POINT ( 'NONE', #94315 ) ;
#60350 = ORIENTED_EDGE ( 'NONE', *, *, #62585, .F. ) ;
#60351 = ADVANCED_FACE ( 'NONE', ( #59236 ), #95831, .F. ) ;
#60353 = CARTESIAN_POINT ( 'NONE',  ( 204.9103773355753617, 275.7318107871104189, 13.62808820451859937 ) ) ;
#60352 = CARTESIAN_POINT ( 'NONE',  ( 186.2856400130477539, 271.9584414235993677, -16.42190033998581811 ) ) ;
#60354 = ORIENTED_EDGE ( 'NONE', *, *, #99606, .F. ) ;
#60355 = CARTESIAN_POINT ( 'NONE',  ( 191.5544531425776427, 298.8649500714207647, 8.366689293739112188 ) ) ;
#60356 = LINE ( 'NONE', #37560, #23674 ) ;
#60357 = CARTESIAN_POINT ( 'NONE',  ( 80.29069729260778843, 58.15026982914754683, -16.60659103188077879 ) ) ;
#60358 = CARTESIAN_POINT ( 'NONE',  ( -40.67952639183666008, 27.60432558407079640, -10.00000000000000000 ) ) ;
#60359 = EDGE_LOOP ( 'NONE', ( #98189, #88116, #17393, #2289 ) ) ;
#60360 = CARTESIAN_POINT ( 'NONE',  ( 189.8147415777049218, 301.8782188922952514, -0.5019643756309712934 ) ) ;
#60361 = ADVANCED_FACE ( 'NONE', ( #81610 ), #74983, .F. ) ;
#60362 = AXIS2_PLACEMENT_3D ( 'NONE', #60583, #5419, #27725 ) ;
#60363 = ORIENTED_EDGE ( 'NONE', *, *, #34989, .F. ) ;
#60364 = CARTESIAN_POINT ( 'NONE',  ( 206.1215120922853146, 273.6340638536760821, 10.12238414215620885 ) ) ;
#60365 = EDGE_CURVE ( 'NONE', #98986, #77883, #34959, .T. ) ;
#60366 = CARTESIAN_POINT ( 'NONE',  ( 4.102725850843912170, 28.55253618238880620, -10.00000000000000000 ) ) ;
#60367 = ORIENTED_EDGE ( 'NONE', *, *, #43885, .T. ) ;
#60368 = CARTESIAN_POINT ( 'NONE',  ( 149.5633513747893346, 271.5956717990251832, 12.83777201928511325 ) ) ;
#60369 = FACE_OUTER_BOUND ( 'NONE', #63821, .T. ) ;
#60370 = AXIS2_PLACEMENT_3D ( 'NONE', #43526, #26350, #4533 ) ;
#60371 = ORIENTED_EDGE ( 'NONE', *, *, #1243, .T. ) ;
#60372 = CARTESIAN_POINT ( 'NONE',  ( -7.270353138567037021, 73.42010414804977358, 14.97951234254161257 ) ) ;
#60373 = CARTESIAN_POINT ( 'NONE',  ( 84.09875786492884231, 229.3615022471903160, 5.000000000000046185 ) ) ;
#60374 = CARTESIAN_POINT ( 'NONE',  ( 180.4054221593022476, 281.2366265252658764, 16.98216568542962435 ) ) ;
#60375 = DIRECTION ( 'NONE',  ( -0.8660254037844387076, -0.4999999999999998890, -0.000000000000000000 ) ) ;
#60376 = ORIENTED_EDGE ( 'NONE', *, *, #9792, .T. ) ;
#60377 = ORIENTED_EDGE ( 'NONE', *, *, #74348, .T. ) ;
#60378 = CARTESIAN_POINT ( 'NONE',  ( 73.41164147859498712, 69.84296063560688594, 9.177452858377941780 ) ) ;
#60380 = VECTOR ( 'NONE', #24333, 1000.000000000000000 ) ;
#60379 = CARTESIAN_POINT ( 'NONE',  ( 82.80579214661656806, 42.74001471116365991, -6.585052516728319816 ) ) ;
#60381 = CARTESIAN_POINT ( 'NONE',  ( 190.8957779480239765, 300.0058089740729770, -4.541438514207768229 ) ) ;
#60382 = CARTESIAN_POINT ( 'NONE',  ( 148.1634546024981205, 274.0203641339852538, 9.324875965062235039 ) ) ;
#60383 = CARTESIAN_POINT ( 'NONE',  ( 175.1455254742422767, 260.8290329488390853, -14.76850912927449322 ) ) ;
#60384 = CARTESIAN_POINT ( 'NONE',  ( 152.9489295551198893, 265.7316783776963121, 17.71675637597311237 ) ) ;
#60385 = B_SPLINE_CURVE_WITH_KNOTS ( 'NONE', 3,
 ( #32653, #7349, #23036, #53932 ),
 .UNSPECIFIED., .F., .F.,
 ( 4, 4 ),
 ( 0.0005560040454048003873, 0.001053805433886535097 ),
 .UNSPECIFIED. ) ;
#60386 = CARTESIAN_POINT ( 'NONE',  ( 147.2637475104381792, 275.5787025293629426, -0.3536082318825462534 ) ) ;
#60387 = CARTESIAN_POINT ( 'NONE',  ( 191.0724301404414689, 299.6998384015373063, -9.342134220577969828 ) ) ;
#60388 = AXIS2_PLACEMENT_3D ( 'NONE', #35089, #86863, #19435 ) ;
#60389 = CARTESIAN_POINT ( 'NONE',  ( 79.36418056962840240, 56.08893731827392770, -16.16201821102233183 ) ) ;
#60390 = DIRECTION ( 'NONE',  ( 0.000000000000000000, 0.000000000000000000, 1.000000000000000000 ) ) ;
#60391 = LINE ( 'NONE', #84746, #72594 ) ;
#60392 = CARTESIAN_POINT ( 'NONE',  ( 170.9795069520696700, 289.1314490031791706, 4.359428402176874329 ) ) ;
#60393 = CARTESIAN_POINT ( 'NONE',  ( 78.29855726973434571, 47.75006341431981127, 13.92167056375030043 ) ) ;
#60394 = ORIENTED_EDGE ( 'NONE', *, *, #8184, .T. ) ;
#60395 = CARTESIAN_POINT ( 'NONE',  ( 149.1230935109639972, 272.3582207876025336, -11.65754870978959268 ) ) ;
#60396 = CARTESIAN_POINT ( 'NONE',  ( 72.48280754011685190, 70.60311863597817705, 7.264376673680498442 ) ) ;
#60397 = CARTESIAN_POINT ( 'NONE',  ( 148.9880786965214838, 273.1702080067959173, 9.612489482347704950 ) ) ;
#60398 = CARTESIAN_POINT ( 'NONE',  ( 79.39828970323148383, 45.77552746013876828, 12.94240580742716240 ) ) ;
#60399 = CARTESIAN_POINT ( 'NONE',  ( -73.66720466879951346, 50.53642055324488780, 10.00000000000000000 ) ) ;
#60400 = CARTESIAN_POINT ( 'NONE',  ( 147.9357294667677252, 274.4147956392308174, -9.396937908507679182 ) ) ;
#60401 = CARTESIAN_POINT ( 'NONE',  ( 166.0155803056910315, 284.5441077266590355, -8.592831666274795666 ) ) ;
#60402 = ORIENTED_EDGE ( 'NONE', *, *, #40056, .F. ) ;
#60403 = CARTESIAN_POINT ( 'NONE',  ( 168.3577311645284453, 254.0536616052273473, -11.79086602269251571 ) ) ;
#60404 = CARTESIAN_POINT ( 'NONE',  ( 186.7063704226160326, 285.7974574491823319, -16.69995036437973468 ) ) ;
#60406 = ADVANCED_FACE ( 'NONE', ( #4069 ), #4569, .T. ) ;
#60405 = CARTESIAN_POINT ( 'NONE',  ( 71.99267133948018227, 71.58944556433895912, 5.550980660130568900 ) ) ;
#60407 = CARTESIAN_POINT ( 'NONE',  ( 54.99669585504140912, 195.8927522451418213, -10.00000000000009059 ) ) ;
#60408 = CARTESIAN_POINT ( 'NONE',  ( 114.9778026189612632, 243.3149278399160664, 9.188101187500093303 ) ) ;
#60409 = CARTESIAN_POINT ( 'NONE',  ( 151.2567985338353935, 268.6625352796243646, -15.71756535662528798 ) ) ;
#60410 = FACE_OUTER_BOUND ( 'NONE', #58127, .T. ) ;
#60411 = LINE ( 'NONE', #28037, #90714 ) ;
#60412 = CARTESIAN_POINT ( 'NONE',  ( 172.8311536199634588, 250.6280622661865607, -4.159570053950042201 ) ) ;
#60413 = CARTESIAN_POINT ( 'NONE',  ( 36.52174756457106497, 182.7048013555409796, 4.594050593750051981 ) ) ;
#60414 = CARTESIAN_POINT ( 'NONE',  ( 147.6458100276484799, 275.6668707137318393, -2.669052585738262096 ) ) ;
#60415 = B_SPLINE_CURVE_WITH_KNOTS ( 'NONE', 3,
 ( #65848, #96303, #19297, #12171 ),
 .UNSPECIFIED., .F., .F.,
 ( 4, 4 ),
 ( 0.04472034873244652015, 0.04887066958154942520 ),
 .UNSPECIFIED. ) ;
#60416 = EDGE_LOOP ( 'NONE', ( #3804, #975, #52163, #95478 ) ) ;
#60417 = CARTESIAN_POINT ( 'NONE',  ( 34.05451400132101014, 48.17084265633775431, 10.00000000000000000 ) ) ;
#60418 = CARTESIAN_POINT ( 'NONE',  ( 181.8935359714662923, 266.9004732347041795, 15.52955990709112122 ) ) ;
#60419 = B_SPLINE_CURVE_WITH_KNOTS ( 'NONE', 3,
 ( #53770, #60374, #45187, #98917 ),
 .UNSPECIFIED., .F., .F.,
 ( 4, 4 ),
 ( 0.02807627225634463583, 0.03726733138970944603 ),
 .UNSPECIFIED. ) ;
#60420 = LINE ( 'NONE', #14346, #90281 ) ;
#60421 = CARTESIAN_POINT ( 'NONE',  ( 146.9376205018946848, 276.1435710778808925, 5.066564108429441937 ) ) ;
#60422 = CARTESIAN_POINT ( 'NONE',  ( 99.01965388075032592, 234.6427522451419065, -10.00000000000009592 ) ) ;
#60423 = DIRECTION ( 'NONE',  ( 0.4851478631379963491, -0.8403007481384849875, 0.2419218955996714493 ) ) ;
#60424 = CARTESIAN_POINT ( 'NONE',  ( 64.18017357788677657, 207.8615022471902307, -10.00000000000009592 ) ) ;
#60425 = CARTESIAN_POINT ( 'NONE',  ( 164.1747640914098554, 250.0330537093315399, 10.26818566766051077 ) ) ;
#60426 = CARTESIAN_POINT ( 'NONE',  ( 108.6181021060278198, 243.5177522451419065, 5.000000000000046185 ) ) ;
#60427 = ORIENTED_EDGE ( 'NONE', *, *, #7646, .F. ) ;
#60428 = CARTESIAN_POINT ( 'NONE',  ( 198.7382248435485792, 267.5558359697628248, -8.259202697554929529 ) ) ;
#60429 = EDGE_CURVE ( 'NONE', #39044, #21, #99301, .T. ) ;
#60430 = CARTESIAN_POINT ( 'NONE',  ( 155.7386282512242985, 279.8610998479833825, -1.584717933846769400 ) ) ;
#60431 = CARTESIAN_POINT ( 'NONE',  ( 163.4218292706009095, 247.5920839679097014, -10.44611490715852042 ) ) ;
#60432 = VECTOR ( 'NONE', #99863, 1000.000000000000114 ) ;
#60433 = CARTESIAN_POINT ( 'NONE',  ( 16.49491010205593255, 171.1423013555409796, -4.594050593750043987 ) ) ;
#60434 = CARTESIAN_POINT ( 'NONE',  ( 14.64478397084458550, 10.58380873178785642, 6.180339887498953466 ) ) ;
#60435 = CARTESIAN_POINT ( 'NONE',  ( -15.45538172674451616, 105.8574260514038627, 44.07251632651297513 ) ) ;
#60436 = CARTESIAN_POINT ( 'NONE',  ( 71.61759974305658716, 58.94635126778479872, -15.37279249342744336 ) ) ;
#60437 = CARTESIAN_POINT ( 'NONE',  ( 73.07265265467388815, 69.63838777454593298, 9.188147135407486843 ) ) ;
#60439 = CARTESIAN_POINT ( 'NONE',  ( 61.79834339388186493, 215.6744531367911293, 4.594050593750047540 ) ) ;
#60438 = CARTESIAN_POINT ( 'NONE',  ( 174.7685907560459100, 286.3307797320127861, 10.46086992841393482 ) ) ;
#60440 = CARTESIAN_POINT ( 'NONE',  ( 163.7038023771459052, 247.1036922210055025, -6.448491958542482472 ) ) ;
#60441 = CARTESIAN_POINT ( 'NONE',  ( 73.11778380043915604, 57.33886984688226818, 15.89460713103382439 ) ) ;
#60442 = EDGE_CURVE ( 'NONE', #49563, #7148, #34472, .T. ) ;
#60443 = CARTESIAN_POINT ( 'NONE',  ( 64.77737111682257876, 68.52662068827326891, 0.000000000000000000 ) ) ;
#60444 = CARTESIAN_POINT ( 'NONE',  ( 66.40824058694533960, 68.21386763270049869, -4.392278699897152805 ) ) ;
#60445 = VERTEX_POINT ( 'NONE', #89240 ) ;
#60446 = ADVANCED_FACE ( 'NONE', ( #11200 ), #51389, .F. ) ;
#60447 = VECTOR ( 'NONE', #98786, 1000.000000000000114 ) ;
#60448 = CARTESIAN_POINT ( 'NONE',  ( 6.950328144465094837, 181.4865022471903160, -10.00000000000009415 ) ) ;
#60449 = CARTESIAN_POINT ( 'NONE',  ( 207.5290616128274337, 271.1961165699281651, 2.604679844609484984 ) ) ;
#60450 = AXIS2_PLACEMENT_3D ( 'NONE', #34781, #65683, #33295 ) ;
#60451 = CARTESIAN_POINT ( 'NONE',  ( 141.8249372320439647, 246.5643266524160140, 9.188101187500095079 ) ) ;
#60452 = CARTESIAN_POINT ( 'NONE',  ( 22.33066906249845118, 34.93396525600390845, 2.839279412974139660 ) ) ;
#60453 = CARTESIAN_POINT ( 'NONE',  ( 164.3691747484889163, 245.9512334678869365, 1.203589100610505724 ) ) ;
#60454 = CARTESIAN_POINT ( 'NONE',  ( 83.58592293191674116, 51.62412561587523641, -14.84978998814507989 ) ) ;
#60455 = CARTESIAN_POINT ( 'NONE',  ( -7.338644212303985448, 23.89290704711799052, 10.00000000000000000 ) ) ;
#60457 = CARTESIAN_POINT ( 'NONE',  ( 189.4564606193425789, 289.8033142756258940, 15.68452023909392956 ) ) ;
#60456 = CARTESIAN_POINT ( 'NONE',  ( 84.50387165700357173, 41.56312468464896170, -0.5288249497319834624 ) ) ;
#60458 = CARTESIAN_POINT ( 'NONE',  ( 68.96547873374085214, 64.13046873611052945, 12.06460432375195957 ) ) ;
#60459 = ORIENTED_EDGE ( 'NONE', *, *, #97229, .T. ) ;
#60460 = CARTESIAN_POINT ( 'NONE',  ( 81.50039046230392614, 52.51855974082073431, 15.62894985664426528 ) ) ;
#60461 = CARTESIAN_POINT ( 'NONE',  ( 73.03232164105139645, 66.66734575193103751, -12.55698212435192929 ) ) ;
#60462 = CARTESIAN_POINT ( 'NONE',  ( 155.9200296242932495, 280.3860598674420430, -5.539708607631867565 ) ) ;
#60463 = CARTESIAN_POINT ( 'NONE',  ( 197.2238629298283570, 273.4569059118221617, -14.28082208226903305 ) ) ;
#60464 = ORIENTED_EDGE ( 'NONE', *, *, #63113, .F. ) ;
#60465 = CARTESIAN_POINT ( 'NONE',  ( 206.5287971022838178, 272.9286255231971268, 9.140400389658188018 ) ) ;
#60466 = CARTESIAN_POINT ( 'NONE',  ( -41.62359735524142224, 26.60228115600144250, 177.5919119679930134 ) ) ;
#60467 = B_SPLINE_CURVE_WITH_KNOTS ( 'NONE', 3,
 ( #8471, #61657, #39342, #70257 ),
 .UNSPECIFIED., .F., .F.,
 ( 4, 4 ),
 ( 0.01270677793150105754, 0.02126268609028184389 ),
 .UNSPECIFIED. ) ;
#60468 = CARTESIAN_POINT ( 'NONE',  ( 153.4689407916852701, 266.8309924954582470, 16.62268559038933091 ) ) ;
#60469 = CARTESIAN_POINT ( 'NONE',  ( 192.7547114638438188, 293.9047809918118901, -14.59372857566467374 ) ) ;
#60470 = CARTESIAN_POINT ( 'NONE',  ( 71.98264401366868981, 72.39816763649429276, -2.869464145551841039 ) ) ;
#60471 = CARTESIAN_POINT ( 'NONE',  ( 67.94301448590864823, 69.19482911460316643, 4.205308713653838737 ) ) ;
#60472 = CARTESIAN_POINT ( 'NONE',  ( 200.6737073311291795, 283.0699384897140476, -17.61533935526990291 ) ) ;
#60473 = ADVANCED_FACE ( 'NONE', ( #37935 ), #45053, .F. ) ;
#60474 = CARTESIAN_POINT ( 'NONE',  ( 190.9874095833745002, 280.9743702084771826, 16.64962686899652411 ) ) ;
#60475 = CARTESIAN_POINT ( 'NONE',  ( 11.07908504951724282, 25.13478043621386959, 8.090169943749478065 ) ) ;
#60476 = CARTESIAN_POINT ( 'NONE',  ( 81.38228331512368641, 42.18052851754683275, 8.075145019496556387 ) ) ;
#60477 = ORIENTED_EDGE ( 'NONE', *, *, #78944, .T. ) ;
#60478 = CARTESIAN_POINT ( 'NONE',  ( 190.1519139143167081, 301.2942192743771557, 4.481136594690903863 ) ) ;
#60479 = CARTESIAN_POINT ( 'NONE',  ( 86.37020013017546205, 47.54260244662367541, -11.08968936411752715 ) ) ;
#60480 = CARTESIAN_POINT ( 'NONE',  ( 189.0720163204064477, 297.0724856426199949, 8.110046717386847348 ) ) ;
#60481 = VERTEX_POINT ( 'NONE', #76474 ) ;
#60482 = CARTESIAN_POINT ( 'NONE',  ( 191.8329718516215223, 298.3825415164982928, -8.871589506312979267 ) ) ;
#60483 = FACE_OUTER_BOUND ( 'NONE', #78652, .T. ) ;
#60484 = CARTESIAN_POINT ( 'NONE',  ( 163.9942050550062049, 246.6007000282974673, 5.791111691696777974 ) ) ;
#60485 = CARTESIAN_POINT ( 'NONE',  ( 70.02414138031360835, 62.78214778883172187, 13.38063900663788708 ) ) ;
#60486 = VERTEX_POINT ( 'NONE', #98789 ) ;
#60487 = CARTESIAN_POINT ( 'NONE',  ( 94.78875894111908451, 225.5333772461660544, 9.188101187500095079 ) ) ;
#60488 = CARTESIAN_POINT ( 'NONE',  ( 155.3513056799751553, 261.5706408705564741, 18.59020393050806064 ) ) ;
#60489 = CARTESIAN_POINT ( 'NONE',  ( 73.05863210132505969, 69.60576123971951290, -9.808587366596233537 ) ) ;
#60490 = CARTESIAN_POINT ( 'NONE',  ( 179.4722142099873565, 269.7276464518548096, -17.35046799866735157 ) ) ;
#60491 = CARTESIAN_POINT ( 'NONE',  ( 81.20776596464571639, 42.33569611896157880, -7.485437602881505725 ) ) ;
#60492 = VERTEX_POINT ( 'NONE', #60237 ) ;
#60493 = ADVANCED_FACE ( 'NONE', ( #67357 ), #91198, .T. ) ;
#60494 = VERTEX_POINT ( 'NONE', #28873 ) ;
#60495 = ORIENTED_EDGE ( 'NONE', *, *, #22663, .F. ) ;
#60496 = CARTESIAN_POINT ( 'NONE',  ( 82.02196949114711799, 53.52097756913676818, 15.46628681541728056 ) ) ;
#60497 = ORIENTED_EDGE ( 'NONE', *, *, #85085, .F. ) ;
#60498 = CARTESIAN_POINT ( 'NONE',  ( 68.27542981431423641, 68.50580704656320563, 6.393928382725774462 ) ) ;
#60499 = CARTESIAN_POINT ( 'NONE',  ( -11.40312891409031693, 78.77562236714182120, 52.49999999999999289 ) ) ;
#60500 = VERTEX_POINT ( 'NONE', #68353 ) ;
#60501 = CARTESIAN_POINT ( 'NONE',  ( 164.4678285797544106, 245.7803600197737524, -6.875991496205872799 ) ) ;
#60502 = CARTESIAN_POINT ( 'NONE',  ( 66.18968672761215544, 68.49487770601442094, -4.881532527435783919 ) ) ;
#60503 = CARTESIAN_POINT ( 'NONE',  ( 153.1983976505312626, 265.2995869615763809, -17.69657798691567763 ) ) ;
#60504 = DIRECTION ( 'NONE',  ( -1.000000000000000000, 0.000000000000000000, 0.000000000000000000 ) ) ;
#60505 = CARTESIAN_POINT ( 'NONE',  ( 82.84342636331510334, 53.76751615666388062, -15.40379040879673056 ) ) ;
#60506 = CARTESIAN_POINT ( 'NONE',  ( 165.0905872925919198, 264.4194027570436560, -17.26892763788675111 ) ) ;
#60507 = ORIENTED_EDGE ( 'NONE', *, *, #10312, .T. ) ;
#60508 = CARTESIAN_POINT ( 'NONE',  ( 76.97307773550161869, 61.50313384435956010, 15.60575781086138747 ) ) ;
#60509 = CARTESIAN_POINT ( 'NONE',  ( 13.01786573420820226, 22.91421378149917842, 9.188101187500008038 ) ) ;
#60510 = ORIENTED_EDGE ( 'NONE', *, *, #2518, .F. ) ;
#60511 = DIRECTION ( 'NONE',  ( -0.9985601716053730259, 0.05364311403570636710, 0.000000000000000000 ) ) ;
#60512 = CARTESIAN_POINT ( 'NONE',  ( 85.67692334825835587, 48.86287692480856748, 12.08569265371076185 ) ) ;
#60514 = ORIENTED_EDGE ( 'NONE', *, *, #92264, .T. ) ;
#60513 = CARTESIAN_POINT ( 'NONE',  ( 115.5259514080638468, 249.0530062829863311, -4.648177544792955347E-16 ) ) ;
#60515 = CARTESIAN_POINT ( 'NONE',  ( 163.1332433029523372, 248.0919295262283981, 11.24052392390482957 ) ) ;
#60516 = CARTESIAN_POINT ( 'NONE',  ( 185.4561098074771621, 258.8772088657420909, 2.911598623360981630 ) ) ;
#60517 = CARTESIAN_POINT ( 'NONE',  ( 157.8220056349055369, 279.9582903339057793, -6.810428219376026604 ) ) ;
#60518 = CARTESIAN_POINT ( 'NONE',  ( 165.5430083683156681, 246.8960659038277470, -2.170161657073390149 ) ) ;
#60519 =( BOUNDED_CURVE ( )  B_SPLINE_CURVE ( 2, ( #95323, #2581, #48676, #43028, #49652, #26370, #97289, #87737, #79608 ),
 .UNSPECIFIED., .F., .T. ) 
 B_SPLINE_CURVE_WITH_KNOTS ( ( 3, 2, 2, 2, 3 ),
 ( 0.2056451612903225923, 0.2069892473118279674, 0.2096774193548387177, 0.2123655913978494680, 0.2137096774193548432 ),
 .UNSPECIFIED. ) 
 CURVE ( )  GEOMETRIC_REPRESENTATION_ITEM ( )  RATIONAL_B_SPLINE_CURVE ( ( 0.9330127018922194093, 0.9330127018922194093, 1.000000000000000000, 0.8660254037844387076, 1.000000000000000000, 0.8660254037844387076, 1.000000000000000000, 0.9330127018922194093, 0.9330127018922194093 ) ) 
 REPRESENTATION_ITEM ( '' )  );
#60520 = CARTESIAN_POINT ( 'NONE',  ( -13.19378359325312466, 163.1896272461660544, -9.188101187500095079 ) ) ;
#60521 = AXIS2_PLACEMENT_3D ( 'NONE', #7496, #36904, #6010 ) ;
#60522 = EDGE_CURVE ( 'NONE', #50774, #59643, #86072, .T. ) ;
#60523 = CARTESIAN_POINT ( 'NONE',  ( 161.4396252346964218, 251.0253620690641299, 14.51972485405798885 ) ) ;
#60524 = CARTESIAN_POINT ( 'NONE',  ( 157.8800731348900399, 281.1895650486539466, 1.630747533558548401 ) ) ;
#60525 = ORIENTED_EDGE ( 'NONE', *, *, #62159, .T. ) ;
#60526 = CARTESIAN_POINT ( 'NONE',  ( 181.7865378082156553, 270.5830284917279869, -16.18448056385958722 ) ) ;
#60528 = EDGE_CURVE ( 'NONE', #38315, #77337, #20702, .T. ) ;
#60527 = CARTESIAN_POINT ( 'NONE',  ( 142.6123662252853421, 259.5780487066560340, -7.305945665944390655 ) ) ;
#60529 = CARTESIAN_POINT ( 'NONE',  ( 5.633247839328403117, 167.3927522451417929, -10.00000000000009059 ) ) ;
#60530 = VECTOR ( 'NONE', #47916, 1000.000000000000114 ) ;
#60531 = LINE ( 'NONE', #6361, #4128 ) ;
#60532 = CARTESIAN_POINT ( 'NONE',  ( 171.5710534622694752, 280.0502575882814540, -15.14474945027508213 ) ) ;
#60533 = CARTESIAN_POINT ( 'NONE',  ( 163.3599243854785641, 247.6993063741778940, -7.900958877154002025 ) ) ;
#60534 = LINE ( 'NONE', #86281, #73764 ) ;
#60535 = CARTESIAN_POINT ( 'NONE',  ( 72.62753967730402849, 70.91775434214520146, 7.625672695449470240 ) ) ;
#60537 = CARTESIAN_POINT ( 'NONE',  ( 76.04770329001843265, 65.50818618912236957, 13.94958420308868341 ) ) ;
#60536 = CARTESIAN_POINT ( 'NONE',  ( -9.459049039432731121, 165.3458772461660544, 9.188101187500095079 ) ) ;
#60538 = CARTESIAN_POINT ( 'NONE',  ( 162.8410080103373048, 248.9638863495861472, 10.02562058800860711 ) ) ;
#60539 = VERTEX_POINT ( 'NONE', #78476 ) ;
#60540 = EDGE_LOOP ( 'NONE', ( #47049, #66489, #41556, #21626 ) ) ;
#60541 = DIRECTION ( 'NONE',  ( -1.000000000000000000, 0.000000000000000000, 0.000000000000000000 ) ) ;
#60542 = DIRECTION ( 'NONE',  ( 0.6056412518070691808, 0.7957378174433877849, 0.000000000000000000 ) ) ;
#60543 = CARTESIAN_POINT ( 'NONE',  ( 172.6414858973122080, 289.5474176056248439, 2.599858645979187699 ) ) ;
#60544 = CARTESIAN_POINT ( 'NONE',  ( 86.39222172200696548, 43.37934728214441549, 2.793685208327149283 ) ) ;
#60545 = CARTESIAN_POINT ( 'NONE',  ( 162.4303591677746681, 249.3093605601900435, -10.83980511239089672 ) ) ;
#60546 = CARTESIAN_POINT ( 'NONE',  ( 83.55683262847328763, 44.73071775418808471, 9.087976461446411136 ) ) ;
#60547 = DIRECTION ( 'NONE',  ( -0.7511915808658203852, -0.6600842437418951159, 0.000000000000000000 ) ) ;
#60548 = CARTESIAN_POINT ( 'NONE',  ( 16.84647260051960060, 180.5333772461660544, 9.188101187500095079 ) ) ;
#60549 = CARTESIAN_POINT ( 'NONE',  ( 116.7098534265301595, 244.3149278399160949, -9.188101187500095079 ) ) ;
#60550 = FACE_OUTER_BOUND ( 'NONE', #85763, .T. ) ;
#60551 = CARTESIAN_POINT ( 'NONE',  ( 183.1253468672910287, 257.7788483971966684, -2.448293748885121968 ) ) ;
#60552 = CARTESIAN_POINT ( 'NONE',  ( 206.6967779005227328, 272.1534147736609270, -6.959009905159835974 ) ) ;
#60553 = CARTESIAN_POINT ( 'NONE',  ( 178.5250536166888935, 283.8345237224107791, -14.80487358518624497 ) ) ;
#60554 = CARTESIAN_POINT ( 'NONE',  ( 81.28829938836423707, 53.14541240262165900, -15.42935213604580014 ) ) ;
#60555 = CARTESIAN_POINT ( 'NONE',  ( 194.1493756275458793, 294.3704124857528655, 13.94613522129020744 ) ) ;
#60556 = CARTESIAN_POINT ( 'NONE',  ( 207.4218731373931632, 271.3817724553659332, -5.249531240730909154 ) ) ;
#60557 = FACE_OUTER_BOUND ( 'NONE', #29846, .T. ) ;
#60558 = CARTESIAN_POINT ( 'NONE',  ( 162.8931802014337791, 249.0911889412991229, -10.32038157250286048 ) ) ;
#60559 = CARTESIAN_POINT ( 'NONE',  ( 192.6020418108567469, 265.2366636836216003, 7.811029749084129392 ) ) ;
#60560 = EDGE_CURVE ( 'NONE', #8880, #59093, #13207, .T. ) ;
#60561 = CYLINDRICAL_SURFACE ( 'NONE', #62592, 10.00000000000010658 ) ;
#60562 = CARTESIAN_POINT ( 'NONE',  ( 183.7010204048396815, 267.9445264290289970, -15.94297069647373633 ) ) ;
#60563 = CARTESIAN_POINT ( 'NONE',  ( 53.96283019206333620, 190.4155109091896350, 2.679491924311254714 ) ) ;
#60564 = EDGE_CURVE ( 'NONE', #65477, #10093, #26798, .T. ) ;
#60566 = ADVANCED_FACE ( 'NONE', ( #62235 ), #16158, .F. ) ;
#60565 = CARTESIAN_POINT ( 'NONE',  ( 183.8043731368310603, 268.5938253857621589, 16.29461355553033997 ) ) ;
#60567 = ADVANCED_FACE ( 'NONE', ( #3957 ), #59120, .F. ) ;
#60568 = CARTESIAN_POINT ( 'NONE',  ( 95.05956542768421969, 219.5643266524160140, 9.188101187500095079 ) ) ;
#60569 = CARTESIAN_POINT ( 'NONE',  ( 4.462289544239296468, 25.68290643055184574, 3.479690158560446702E-15 ) ) ;
#60570 = B_SPLINE_CURVE_WITH_KNOTS ( 'NONE', 3,
 ( #88149, #48598, #72917, #33908, #18697, #19214, #88648, #27292, #81521, #71904, #2504, #34869, #73397, #3508, #72416, #49092, #50084, #58174, #33386, #94722, #25281, #87163, #81041, #3020, #17695, #80531, #11111, #11604, #65283, #3983, #89159, #40472, #71404, #64288, #25806, #90631, #91116, #37361, #83017, #20690, #53068, #83516, #52073, #90116, #74898, #12090 ),
 .UNSPECIFIED., .F., .F.,
 ( 4, 1, 2, 2, 1, 2, 2, 1, 1, 2, 2, 1, 1, 2, 2, 1, 1, 2, 2, 1, 1, 1, 2, 2, 1, 1, 1, 2, 2, 4 ),
 ( 0.000000000000000000, 0.06250000000000308087, 0.09375000000000487110, 0.1250000000000066613, 0.1875000000000102418, 0.2187500000000134059, 0.2500000000000165423, 0.3125000000000192624, 0.3437500000000203726, 0.3593750000000210387, 0.3750000000000217049, 0.4375000000000275890, 0.4687500000000319189, 0.4843750000000340838, 0.5000000000000363043, 0.5625000000000544009, 0.5937500000000636158, 0.6093750000000668354, 0.6250000000000700551, 0.6875000000000744960, 0.7187500000000768274, 0.7343750000000780487, 0.7421875000000773825, 0.7500000000000766054, 0.8125000000000563993, 0.8437500000000449640, 0.8593750000000376366, 0.8671875000000351941, 0.8750000000000327516, 1.000000000000000000 ),
 .UNSPECIFIED. ) ;
#60571 = CARTESIAN_POINT ( 'NONE',  ( 67.97445910463009966, 65.68506835540814848, 10.87894195494597405 ) ) ;
#60572 = DIRECTION ( 'NONE',  ( -0.9331105242498700658, 0.3595896960900473172, 0.000000000000000000 ) ) ;
#60574 = CARTESIAN_POINT ( 'NONE',  ( 83.53981050848499024, 42.15194584004071032, -4.113498934485630087 ) ) ;
#60573 = CARTESIAN_POINT ( 'NONE',  ( -22.42236680055709641, 157.8615022471902591, 0.000000000000000000 ) ) ;
#60575 = CARTESIAN_POINT ( 'NONE',  ( 201.2481467672282633, 270.6558803864813854, -9.957100446674763461 ) ) ;
#60576 = LINE ( 'NONE', #77299, #95711 ) ;
#60577 = CYLINDRICAL_SURFACE ( 'NONE', #73657, 17.82106496071139645 ) ;
#60578 = CARTESIAN_POINT ( 'NONE',  ( 35.16646543599519248, 35.70171378149922248, -9.188101187500004485 ) ) ;
#60579 = CARTESIAN_POINT ( 'NONE',  ( 147.5749551500760788, 275.0396750858066639, -4.254929048021584670 ) ) ;
#60580 = DIRECTION ( 'NONE',  ( 0.4999999999999998890, -0.8660254037844385966, 0.000000000000000000 ) ) ;
#60581 = ORIENTED_EDGE ( 'NONE', *, *, #21783, .F. ) ;
#60582 = CARTESIAN_POINT ( 'NONE',  ( 22.87854050506884462, 34.18502408145592852, 5.678558825948277544 ) ) ;
#60583 = CARTESIAN_POINT ( 'NONE',  ( 80.87517248313827167, 58.64441083166272506, 0.000000000000000000 ) ) ;
#60584 = CARTESIAN_POINT ( 'NONE',  ( 147.3236643320416022, 275.4749235501183193, -5.185334239426818037 ) ) ;
#60585 = CARTESIAN_POINT ( 'NONE',  ( 93.96857342517718337, 4.999999999999999112, 14.21260523776213347 ) ) ;
#60586 = ORIENTED_EDGE ( 'NONE', *, *, #91303, .T. ) ;
#60587 = CARTESIAN_POINT ( 'NONE',  ( 70.62030545033579187, 60.85430430480430886, 14.51265376387380357 ) ) ;
#60588 = CARTESIAN_POINT ( 'NONE',  ( 159.6610344727618269, 254.1059716346071866, 15.33388637456589620 ) ) ;
#60589 = AXIS2_PLACEMENT_3D ( 'NONE', #56424, #40205, #46828 ) ;
#60590 = CARTESIAN_POINT ( 'NONE',  ( 183.2995815306362033, 263.9961729758801994, -13.75453846732532526 ) ) ;
#60591 = CARTESIAN_POINT ( 'NONE',  ( 186.6673878995319455, 276.5074556901925007, 17.73048906045012529 ) ) ;
#60592 = PLANE ( 'NONE',  #43583 ) ;
#60593 = ORIENTED_EDGE ( 'NONE', *, *, #53101, .T. ) ;
#60594 = CARTESIAN_POINT ( 'NONE',  ( 186.5306968903125266, 298.6962994122694681, -3.433113405341845059 ) ) ;
#60595 = ORIENTED_EDGE ( 'NONE', *, *, #29949, .F. ) ;
#60596 = CARTESIAN_POINT ( 'NONE',  ( 78.34913526621272695, 61.55915279984171917, 16.16953766326405173 ) ) ;
#60597 = CARTESIAN_POINT ( 'NONE',  ( 87.56426860159915293, 44.18524048238309376, 3.435755015769986542 ) ) ;
#60599 = ORIENTED_EDGE ( 'NONE', *, *, #25802, .F. ) ;
#60598 = AXIS2_PLACEMENT_3D ( 'NONE', #12327, #97436, #29504 ) ;
#60600 = CARTESIAN_POINT ( 'NONE',  ( 204.3821110352445203, 268.7037507017955136, 3.837584713511939416 ) ) ;
#60601 = CARTESIAN_POINT ( 'NONE',  ( 159.4943857219621748, 255.4856773835659851, 16.13974565162016006 ) ) ;
#60602 = CARTESIAN_POINT ( 'NONE',  ( 190.7811490393836209, 278.9442883317611290, -16.52517045990749978 ) ) ;
#60603 = PLANE ( 'NONE',  #15360 ) ;
#60604 = CARTESIAN_POINT ( 'NONE',  ( 153.1627746953036535, 265.3612877299463548, -17.72069958822647351 ) ) ;
#60605 = CARTESIAN_POINT ( 'NONE',  ( 38.25529575686164208, 27.80170272979929535, 7.433330006724137462 ) ) ;
#60606 = CARTESIAN_POINT ( 'NONE',  ( 80.21439583186709399, 44.30090529131236110, 11.38393923939230312 ) ) ;
#60607 = CARTESIAN_POINT ( 'NONE',  ( 81.32801083308449108, 55.42016325551186640, -16.33050219934855107 ) ) ;
#60608 = CARTESIAN_POINT ( 'NONE',  ( -32.96890249059735112, 94.81157474915079320, 43.92482684459560005 ) ) ;
#60609 = B_SPLINE_CURVE_WITH_KNOTS ( 'NONE', 3,
 ( #4287, #82349, #59968, #67079 ),
 .UNSPECIFIED., .F., .F.,
 ( 4, 4 ),
 ( 0.002191032057283921405, 0.01012571542419986488 ),
 .UNSPECIFIED. ) ;
#60610 = CARTESIAN_POINT ( 'NONE',  ( 87.41510241510319190, 45.50646524919893920, 7.075312488460167692 ) ) ;
#60611 = EDGE_LOOP ( 'NONE', ( #85803, #54011, #4467, #1222 ) ) ;
#60612 = ORIENTED_EDGE ( 'NONE', *, *, #36373, .F. ) ;
#60613 = CARTESIAN_POINT ( 'NONE',  ( 198.1939553405634058, 286.4340473833234455, 17.13778683239836553 ) ) ;
#60614 = CARTESIAN_POINT ( 'NONE',  ( 164.2981700896163773, 253.9203781951923133, 14.63367134977796802 ) ) ;
#60616 = CARTESIAN_POINT ( 'NONE',  ( 189.6567408476656738, 300.3785186016523312, -3.371745498157157961 ) ) ;
#60615 = CARTESIAN_POINT ( 'NONE',  ( 164.4936379324916516, 245.7356569095223051, 6.719479797016231437 ) ) ;
#60617 = CYLINDRICAL_SURFACE ( 'NONE', #41720, 10.00000000000010658 ) ;
#60618 = CARTESIAN_POINT ( 'NONE',  ( 197.4991444394840130, 272.9982161165312959, -13.25291263813902809 ) ) ;
#60619 = CARTESIAN_POINT ( 'NONE',  ( 77.01186407997560934, 60.03506380231930706, -15.92001384120855434 ) ) ;
#60620 = CARTESIAN_POINT ( 'NONE',  ( 82.33327191752177043, 40.37251757887272419, 1.340760960699656001 ) ) ;
#60621 = CARTESIAN_POINT ( 'NONE',  ( 170.8271762237143321, 287.6167538513918203, -4.615125244751493661 ) ) ;
#60622 = CARTESIAN_POINT ( 'NONE',  ( 77.25443146841556086, 63.45523539686509196, -15.12022256747658133 ) ) ;
#60623 = CARTESIAN_POINT ( 'NONE',  ( 190.7059995949267659, 300.3345147238140385, 2.121218676196247634E-15 ) ) ;
#60624 =( REPRESENTATION_RELATIONSHIP ('NONE','NONE', #67038, #7571 ) REPRESENTATION_RELATIONSHIP_WITH_TRANSFORMATION ( #37053 )SHAPE_REPRESENTATION_RELATIONSHIP( ) );
#60625 = CARTESIAN_POINT ( 'NONE',  ( 121.5815934185826421, 234.8768266524159856, -9.188101187500091527 ) ) ;
#60626 = ORIENTED_EDGE ( 'NONE', *, *, #57718, .T. ) ;
#60627 = CARTESIAN_POINT ( 'NONE',  ( 183.3956148285660390, 260.2657049373422069, -9.373603463087153642 ) ) ;
#60628 = CARTESIAN_POINT ( 'NONE',  ( 44.74566838383860556, 28.76004757982093807, 5.678558825948272215 ) ) ;
#60629 = CARTESIAN_POINT ( 'NONE',  ( 188.1638898588698510, 273.5466134088359240, 15.69418637652080584 ) ) ;
#60630 = EDGE_CURVE ( 'NONE', #22676, #76712, #34840, .T. ) ;
#60631 = ORIENTED_EDGE ( 'NONE', *, *, #9358, .T. ) ;
#60632 = CIRCLE ( 'NONE', #62288, 10.00000000000007816 ) ;
#60633 = CARTESIAN_POINT ( 'NONE',  ( 86.85107213257295200, 45.77346519082802700, -8.718545132792499430 ) ) ;
#60634 = PLANE ( 'NONE',  #22104 ) ;
#60635 = CARTESIAN_POINT ( 'NONE',  ( 147.3848241166324158, 275.3689916958264803, 2.889551403030883758 ) ) ;
#60636 = CARTESIAN_POINT ( 'NONE',  ( 159.9770824720811220, 253.5585604421560788, -16.42166711341322483 ) ) ;
#60637 = CARTESIAN_POINT ( 'NONE',  ( 17.70578863690133886, 169.4824982072973967, 3.021315404115420679E-15 ) ) ;
#60638 = EDGE_LOOP ( 'NONE', ( #98394, #14889, #79994, #34101 ) ) ;
#60639 = CARTESIAN_POINT ( 'NONE',  ( 43.53192288983094471, 62.93782412512172186, 10.00000000000000000 ) ) ;
#60640 = ORIENTED_EDGE ( 'NONE', *, *, #14029, .F. ) ;
#60641 = CARTESIAN_POINT ( 'NONE',  ( 38.03703169759608471, 202.7677522451419350, -5.000000000000047962 ) ) ;
#60642 = EDGE_LOOP ( 'NONE', ( #46973, #8762, #26624, #6540 ) ) ;
#60644 = CARTESIAN_POINT ( 'NONE',  ( 65.36586985908989789, 182.5653022007868742, 0.000000000000000000 ) ) ;
#60643 = B_SPLINE_CURVE_WITH_KNOTS ( 'NONE', 3,
 ( #50229, #26940, #19851, #5136 ),
 .UNSPECIFIED., .F., .F.,
 ( 4, 4 ),
 ( 2.841188977517477842E-17, 0.006553300831967987308 ),
 .UNSPECIFIED. ) ;
#60645 = CARTESIAN_POINT ( 'NONE',  ( 195.6903230345702411, 265.3535381266730155, 4.357112901190284049 ) ) ;
#60646 = CARTESIAN_POINT ( 'NONE',  ( 178.7412395063929011, 273.4583285910464951, -17.81739543535002568 ) ) ;
#60647 = CARTESIAN_POINT ( 'NONE',  ( 82.65084931856372918, 45.44814966469950690, 10.48390544538666802 ) ) ;
#60649 = DIRECTION ( 'NONE',  ( 1.000000000000000000, 0.000000000000000000, 0.000000000000000000 ) ) ;
#60648 = CARTESIAN_POINT ( 'NONE',  ( -34.42581292930597670, 25.91608375674935871, -10.00000000000000000 ) ) ;
#60650 = CARTESIAN_POINT ( 'NONE',  ( 201.4214977800931763, 281.7747274386935601, -17.04225209925078133 ) ) ;
#60651 = ORIENTED_EDGE ( 'NONE', *, *, #2847, .F. ) ;
#60652 = CARTESIAN_POINT ( 'NONE',  ( 204.6163864379986705, 276.2410179586759682, 14.66911174422491726 ) ) ;
#60653 = CARTESIAN_POINT ( 'NONE',  ( 71.49811913338204761, 62.77384012672010272, 13.87084472012334047 ) ) ;
#60654 = CARTESIAN_POINT ( 'NONE',  ( 190.4989056847608424, 264.3463537290907084, -9.383834525416400396 ) ) ;
#60655 = CARTESIAN_POINT ( 'NONE',  ( 173.1859566361134739, 251.6088681268793152, -0.2708286262129965816 ) ) ;
#60656 = CARTESIAN_POINT ( 'NONE',  ( 189.2760668188215902, 269.4823757547970899, -13.97719911248058366 ) ) ;
#60657 = DIRECTION ( 'NONE',  ( -0.000000000000000000, 0.000000000000000000, -1.000000000000000000 ) ) ;
#60658 = VECTOR ( 'NONE', #85648, 1000.000000000000000 ) ;
#60659 = CARTESIAN_POINT ( 'NONE',  ( 84.63953139824421612, 45.77662167243946101, 9.618633832723032739 ) ) ;
#60660 = CARTESIAN_POINT ( 'NONE',  ( 168.0462690533684338, 251.4142709888886884, 10.74789308012043954 ) ) ;
#60661 = CARTESIAN_POINT ( 'NONE',  ( 189.0446170559639256, 298.4692272884965973, 7.774481545468416854 ) ) ;
#60662 = CARTESIAN_POINT ( 'NONE',  ( 82.69964235597838353, 53.57960405717556540, -15.73923566368025817 ) ) ;
#60663 = CARTESIAN_POINT ( 'NONE',  ( 78.11742282250361313, 228.1589784336661353, -6.496448406907675876E-16 ) ) ;
#60664 = CARTESIAN_POINT ( 'NONE',  ( 206.1405152101578437, 273.6011494880188479, -9.618815605734603480 ) ) ;
#60665 = PLANE ( 'NONE',  #45064 ) ;
#60666 = CARTESIAN_POINT ( 'NONE',  ( 5.404797899793122973, 27.42564005363386315, -10.00000000000000000 ) ) ;
#60667 = CIRCLE ( 'NONE', #94720, 70.00000000000001421 ) ;
#60668 = DIRECTION ( 'NONE',  ( 0.5000000000000001110, -0.8660254037844384856, -0.000000000000000000 ) ) ;
#60669 = CARTESIAN_POINT ( 'NONE',  ( 207.8844858873204657, 270.5805036682629066, -6.251308616122969397 ) ) ;
#60670 = CARTESIAN_POINT ( 'NONE',  ( 67.61660396824018449, 69.64692688607806303, -0.1948645553118400486 ) ) ;
#60672 = DIRECTION ( 'NONE',  ( -0.8660254037844379305, -0.5000000000000014433, -0.000000000000000000 ) ) ;
#60671 = CARTESIAN_POINT ( 'NONE',  ( 73.47631802762754205, 69.90797475050369769, -9.735925655486411756 ) ) ;
#60673 = PRESENTATION_STYLE_ASSIGNMENT (( #83042 ) ) ;
#60674 = DIRECTION ( 'NONE',  ( -0.8660254037844378194, -0.5000000000000014433, -0.000000000000000000 ) ) ;
#60675 = CARTESIAN_POINT ( 'NONE',  ( 80.07812099633126479, 57.44764983040322193, -16.59488970948941500 ) ) ;
#60676 = CARTESIAN_POINT ( 'NONE',  ( 82.41572850117692894, 54.24742443672926839, 15.60867231807350386 ) ) ;
#60677 = B_SPLINE_CURVE_WITH_KNOTS ( 'NONE', 3,
 ( #65039, #73641, #19945, #56429 ),
 .UNSPECIFIED., .F., .F.,
 ( 4, 4 ),
 ( 0.000000000000000000, 0.003851982118655459045 ),
 .UNSPECIFIED. ) ;
#60678 = CARTESIAN_POINT ( 'NONE',  ( 72.19644594898640833, 72.08809165107794570, 3.016574430004901775 ) ) ;
#60679 = CARTESIAN_POINT ( 'NONE',  ( 29.05227845693028854, 178.3923013555409796, 4.594050593750050204 ) ) ;
#60680 = EDGE_CURVE ( 'NONE', #33648, #45420, #53333, .T. ) ;
#60681 = CARTESIAN_POINT ( 'NONE',  ( 59.71473008784930414, 205.2833772461660828, -9.188101187500095079 ) ) ;
#60682 = CARTESIAN_POINT ( 'NONE',  ( 196.1241105319816143, 290.9500712997905794, 15.97146679939154268 ) ) ;
#60683 = CARTESIAN_POINT ( 'NONE',  ( 199.9978482223838512, 277.8398790452972662, 15.22479436670069930 ) ) ;
#60684 = B_SPLINE_CURVE_WITH_KNOTS ( 'NONE', 3,
 ( #19453, #12839, #20428, #11835, #43699, #97925, #50309, #81262, #28500, #35107, #42694, #44190, #21413, #75129, #5704, #90861, #36595, #67499, #83236, #44683, #73625, #4210, #75615, #6204, #91840, #7191, #53296, #61878, #68495, #84249, #76605 ),
 .UNSPECIFIED., .F., .F.,
 ( 4, 3, 3, 3, 3, 3, 3, 3, 3, 3, 4 ),
 ( 0.000000000000000000, 0.1333490885032384554, 0.3007194338854541904, 0.4699862290245523377, 0.5844252810809684728, 0.6686540514502963273, 0.7354980260655706870, 0.8028463152565942229, 0.8633854507757449115, 0.9437142632667596676, 1.000000000000000000 ),
 .UNSPECIFIED. ) ;
#60685 = CARTESIAN_POINT ( 'NONE',  ( -19.65312891409030271, 93.06504152958497400, -59.99999999999999289 ) ) ;
#60686 = CARTESIAN_POINT ( 'NONE',  ( -17.65922707974272399, 170.6115022471903160, -5.000000000000047962 ) ) ;
#60687 = CARTESIAN_POINT ( 'NONE',  ( 48.99766571601688270, 199.0958772461660544, -9.188101187500095079 ) ) ;
#60688 = CIRCLE ( 'NONE', #67229, 0.1418229129681591871 ) ;
#60689 = CARTESIAN_POINT ( 'NONE',  ( 20.11807774711229868, 23.56628583063840665, 9.188101187500006262 ) ) ;
#60690 = CARTESIAN_POINT ( 'NONE',  ( 151.2964716097791325, 268.5938194963972592, -15.66250187539618111 ) ) ;
#60691 = CARTESIAN_POINT ( 'NONE',  ( 149.4456112649506281, 271.7996036513546869, -12.95648166494593667 ) ) ;
#60692 = CARTESIAN_POINT ( 'NONE',  ( 35.61831302110521591, 44.65659080271453263, -1.878358725466461243E-16 ) ) ;
#60693 = CARTESIAN_POINT ( 'NONE',  ( 157.0887340267001946, 258.5613266995183039, -17.61824281915036394 ) ) ;
#60694 = CARTESIAN_POINT ( 'NONE',  ( 158.6775083298138043, 256.2244800708343746, -16.16179708298373896 ) ) ;
#60695 = CARTESIAN_POINT ( 'NONE',  ( 75.45705218706063988, 56.32278965122512204, 16.59324974296169941 ) ) ;
#60696 = CARTESIAN_POINT ( 'NONE',  ( 179.9209375999747351, 276.5811748711908535, 17.74520275588677265 ) ) ;
#60697 = CARTESIAN_POINT ( 'NONE',  ( 82.51842583923367158, 41.01935388997881660, -1.203081695168224607 ) ) ;
#60698 = CARTESIAN_POINT ( 'NONE',  ( 149.2163037105164278, 275.3995219928863207, 7.552778309360953735 ) ) ;
#60699 = CARTESIAN_POINT ( 'NONE',  ( 168.8244094625508751, 257.0541383169796745, -14.93690306707719628 ) ) ;
#60700 = CARTESIAN_POINT ( 'NONE',  ( 93.55286852290896604, 231.4865022471903160, 10.00000000000009237 ) ) ;
#60701 = CARTESIAN_POINT ( 'NONE',  ( 41.47569090598247499, 209.1868197944957899, 17.47570218321535407 ) ) ;
#60702 = CARTESIAN_POINT ( 'NONE',  ( 194.5231616572618520, 285.4348527426450914, -17.22218120948694775 ) ) ;
#60703 = ORIENTED_EDGE ( 'NONE', *, *, #13366, .T. ) ;
#60704 = CARTESIAN_POINT ( 'NONE',  ( 58.84905177982988533, 192.5327760586659451, 1.948934522072303157E-15 ) ) ;
#60705 = VERTEX_POINT ( 'NONE', #73863 ) ;
#60706 = CARTESIAN_POINT ( 'NONE',  ( 166.5905980234743140, 264.6682795497030725, 17.25980299922107264 ) ) ;
#60707 = CARTESIAN_POINT ( 'NONE',  ( 146.8195026170398023, 276.3481572557323034, 4.765869558735466249 ) ) ;
#60708 = DIRECTION ( 'NONE',  ( -0.8660254037844387076, -0.4999999999999998890, -0.000000000000000000 ) ) ;
#60709 = ORIENTED_EDGE ( 'NONE', *, *, #33178, .F. ) ;
#60710 = CARTESIAN_POINT ( 'NONE',  ( -16.25778278694858514, 23.14743555886465032, 10.00000000000000000 ) ) ;
#60711 = CARTESIAN_POINT ( 'NONE',  ( 79.26634259771995517, 46.14609980727534122, -13.24417246943884585 ) ) ;
#60712 = CARTESIAN_POINT ( 'NONE',  ( 147.6512387128590262, 274.9075480792844246, -8.209968531507987777 ) ) ;
#60713 = CARTESIAN_POINT ( 'NONE',  ( 73.05865758147265865, 70.45434667956401142, -8.047668221016442303 ) ) ;
#60714 = CARTESIAN_POINT ( 'NONE',  ( 204.8109598484962532, 275.9040069258922472, 13.12942483889034762 ) ) ;
#60715 = ORIENTED_EDGE ( 'NONE', *, *, #34281, .T. ) ;
#60716 = CARTESIAN_POINT ( 'NONE',  ( 26.03951966209473312, 17.96004757982090538, -5.678558825948275768 ) ) ;
#60717 = CARTESIAN_POINT ( 'NONE',  ( 75.46625377326144246, 57.04332640536068055, 16.11435909797048538 ) ) ;
#60718 = CARTESIAN_POINT ( 'NONE',  ( 175.5341286262602978, 254.1345785787596583, 8.090077792417549318 ) ) ;
#60719 = DIRECTION ( 'NONE',  ( 0.4999999999999992784, -0.8660254037844390407, 0.000000000000000000 ) ) ;
#60720 = ORIENTED_EDGE ( 'NONE', *, *, #76516, .T. ) ;
#60721 = CARTESIAN_POINT ( 'NONE',  ( 189.5534384022301424, 269.0062095459838929, -14.92796778812864922 ) ) ;
#60722 = CARTESIAN_POINT ( 'NONE',  ( 160.0081047537594543, 253.5048282741223602, -16.11956848123596941 ) ) ;
#60723 = AXIS2_PLACEMENT_3D ( 'NONE', #74864, #97184, #74376 ) ;
#60724 = ORIENTED_EDGE ( 'NONE', *, *, #79915, .T. ) ;
#60725 = ORIENTED_EDGE ( 'NONE', *, *, #62312, .T. ) ;
#60726 = CARTESIAN_POINT ( 'NONE',  ( 80.68086640182862368, 49.71203738446756404, -14.26703970971597357 ) ) ;
#60728 = CARTESIAN_POINT ( 'NONE',  ( -69.42519150082246426, 45.64199051378594874, 10.00000000000000000 ) ) ;
#60727 = DIRECTION ( 'NONE',  ( 0.000000000000000000, 0.000000000000000000, 1.000000000000000000 ) ) ;
#60729 = CARTESIAN_POINT ( 'NONE',  ( 163.3723087697842971, 247.6778559913402091, -10.08585062664141319 ) ) ;
#60730 = CARTESIAN_POINT ( 'NONE',  ( 204.2133777088835700, 276.9390495533970693, 13.75768580338462144 ) ) ;
#60731 = CARTESIAN_POINT ( 'NONE',  ( 198.5612432604688991, 286.7288335892616260, 18.30793681285053509 ) ) ;
#60732 = DIRECTION ( 'NONE',  ( -0.8660254037844387076, -0.4999999999999998890, -0.000000000000000000 ) ) ;
#60734 = CARTESIAN_POINT ( 'NONE',  ( 139.7141738582018604, 239.2202760586659736, -5.415160957724236172E-17 ) ) ;
#60733 = PRODUCT_DEFINITION_FORMATION_WITH_SPECIFIED_SOURCE ( 'ANY', '', #74307, .NOT_KNOWN. ) ;
#60735 = CARTESIAN_POINT ( 'NONE',  ( 159.7100847800667509, 255.0739582339791696, -15.92588830848799475 ) ) ;
#60736 = CARTESIAN_POINT ( 'NONE',  ( 180.3268137483904354, 258.1330830615356149, 10.30874540274224849 ) ) ;
#60737 = CARTESIAN_POINT ( 'NONE',  ( 70.32319418844367931, 223.6589784336661921, -6.496448406907675876E-16 ) ) ;
#60738 = ORIENTED_EDGE ( 'NONE', *, *, #65631, .F. ) ;
#60739 = CARTESIAN_POINT ( 'NONE',  ( 173.7695364597527430, 265.5330474293953671, 16.17611066364563044 ) ) ;
#60740 = LINE ( 'NONE', #46044, #10838 ) ;
#60741 = EDGE_CURVE ( 'NONE', #79661, #76651, #63033, .T. ) ;
#60742 = ORIENTED_EDGE ( 'NONE', *, *, #82016, .T. ) ;
#60743 = CARTESIAN_POINT ( 'NONE',  ( 169.8069776206597226, 261.6727971985682757, -16.70353856883196286 ) ) ;
#60744 = ORIENTED_EDGE ( 'NONE', *, *, #410, .T. ) ;
#60745 = ORIENTED_EDGE ( 'NONE', *, *, #80304, .T. ) ;
#60746 = CARTESIAN_POINT ( 'NONE',  ( 90.45192255479418009, 211.4824982072973683, 3.021315404115420679E-15 ) ) ;
#60747 = CARTESIAN_POINT ( 'NONE',  ( 66.94215247483215592, 67.56144765985021650, 6.663993637373098800 ) ) ;
#60748 = CARTESIAN_POINT ( 'NONE',  ( 1.663964738649737374, 161.7677522451418213, -5.000000000000041744 ) ) ;
#60749 = CARTESIAN_POINT ( 'NONE',  ( 146.6138605399200117, 276.7043397814778132, -0.5394499176159462950 ) ) ;
#60750 = CARTESIAN_POINT ( 'NONE',  ( 110.0795199784619882, 244.3615022471903160, 5.000000000000046185 ) ) ;
#60751 = CARTESIAN_POINT ( 'NONE',  ( 154.9910882912764123, 262.1945556895526579, 18.38052604520346023 ) ) ;
#60752 = CARTESIAN_POINT ( 'NONE',  ( 37.48526053816526371, 54.83666944042810343, 10.00000000000000000 ) ) ;
#60753 = CARTESIAN_POINT ( 'NONE',  ( 87.49951909536234496, 45.04593868083598807, 6.937257679092508234 ) ) ;
#60754 = ORIENTED_EDGE ( 'NONE', *, *, #97908, .T. ) ;
#60755 = EDGE_CURVE ( 'NONE', #85997, #95115, #89608, .T. ) ;
#60756 = DIRECTION ( 'NONE',  ( 4.546899780356472071E-16, -9.093799560712944142E-16, 1.000000000000000000 ) ) ;
#60757 = CARTESIAN_POINT ( 'NONE',  ( 161.8319415995885038, 250.3458501924305608, -12.75194401834632529 ) ) ;
#60758 = ORIENTED_EDGE ( 'NONE', *, *, #25612, .T. ) ;
#60759 = EDGE_CURVE ( 'NONE', #10175, #46284, #73370, .T. ) ;
#60760 = CARTESIAN_POINT ( 'NONE',  ( 76.10854616902780378, 51.47353040525071322, -15.66966529414775344 ) ) ;
#60761 = CARTESIAN_POINT ( 'NONE',  ( 76.01570425163725986, 65.59347775405139203, -14.29814048726880316 ) ) ;
#60762 = AXIS2_PLACEMENT_3D ( 'NONE', #40362, #33280, #56056 ) ;
#60763 = CARTESIAN_POINT ( 'NONE',  ( -73.81593683174931186, 48.72104262922892559, 10.00000000000000000 ) ) ;
#60764 = DIRECTION ( 'NONE',  ( -1.000000000000000000, 0.000000000000000000, 0.000000000000000000 ) ) ;
#60765 = CARTESIAN_POINT ( 'NONE',  ( 142.3122500695552048, 240.7202760586659736, -5.415160957724236172E-17 ) ) ;
#60766 = VERTEX_POINT ( 'NONE', #89128 ) ;
#60767 = FACE_OUTER_BOUND ( 'NONE', #13164, .T. ) ;
#60768 = CARTESIAN_POINT ( 'NONE',  ( 182.3318571492640956, 257.5104630292192383, 6.722139348466238395 ) ) ;
#60769 = CARTESIAN_POINT ( 'NONE',  ( -31.49356256989596758, 94.88921800892812541, 36.50000000000000000 ) ) ;
#60770 = CARTESIAN_POINT ( 'NONE',  ( 152.7295469705997277, 266.1116601603806657, -17.40211458100010589 ) ) ;
#60771 = AXIS2_PLACEMENT_3D ( 'NONE', #10992, #97115, #64680 ) ;
#60772 = CARTESIAN_POINT ( 'NONE',  ( 72.96752522106987726, 70.88037482455226268, 8.005050465142900862 ) ) ;
#60773 = CARTESIAN_POINT ( 'NONE',  ( -34.42581292930597670, 25.91608375674935161, 10.00000000000000000 ) ) ;
#60774 = ORIENTED_EDGE ( 'NONE', *, *, #77078, .T. ) ;
#60775 = CARTESIAN_POINT ( 'NONE',  ( 198.3172001563159768, 266.5884540843370587, 4.492955043302433893 ) ) ;
#60776 = CARTESIAN_POINT ( 'NONE',  ( 181.7549530557583921, 291.6705231334538553, 10.34832551352762309 ) ) ;
#60777 = DIRECTION ( 'NONE',  ( -0.5295078238379101743, -0.5024823063052971106, 0.6834712842135728383 ) ) ;
#60778 = CARTESIAN_POINT ( 'NONE',  ( 79.78458617808020392, 47.16083178010686794, 13.11770283550262128 ) ) ;
#60779 = CARTESIAN_POINT ( 'NONE',  ( 202.5909524705457727, 267.2871136637904215, 0.8794807786250381509 ) ) ;
#60780 = ORIENTED_EDGE ( 'NONE', *, *, #5945, .T. ) ;
#60781 = CARTESIAN_POINT ( 'NONE',  ( 147.5177358149801421, 275.1387818813681179, 4.867883209065928085 ) ) ;
#60782 = CARTESIAN_POINT ( 'NONE',  ( 183.5730992744960020, 281.1681395334279046, 17.34192960090523883 ) ) ;
#60783 = AXIS2_PLACEMENT_3D ( 'NONE', #87683, #24796, #9630 ) ;
#60784 = CARTESIAN_POINT ( 'NONE',  ( 164.9779129355220562, 244.8968679994381148, -1.771286574179712803 ) ) ;
#60786 = CARTESIAN_POINT ( 'NONE',  ( 193.5571956648599325, 268.3914742393835695, 12.81656483086835330 ) ) ;
#60785 = CARTESIAN_POINT ( 'NONE',  ( 177.2821372360434395, 264.4767462412605141, -15.52096391193404834 ) ) ;
#60787 = EDGE_CURVE ( 'NONE', #53616, #66781, #89643, .T. ) ;
#60788 = EDGE_CURVE ( 'NONE', #39182, #39202, #56924, .T. ) ;
#60789 = CARTESIAN_POINT ( 'NONE',  ( 26.22111236500157361, 16.10801979619929369, 3.090169943749476733 ) ) ;
#60790 = CARTESIAN_POINT ( 'NONE',  ( 50.26447705663006360, 96.46038765672592774, -10.00000000000000000 ) ) ;
#60791 = LINE ( 'NONE', #68413, #75814 ) ;
#60792 = CARTESIAN_POINT ( 'NONE',  ( 49.80235952159635815, 85.00000000000000000, -10.00000000000000000 ) ) ;
#60793 = AXIS2_PLACEMENT_3D ( 'NONE', #5746, #99961, #29549 ) ;
#60794 = CARTESIAN_POINT ( 'NONE',  ( 159.7897726928491409, 253.8829904965402875, 16.83923858130328810 ) ) ;
#60795 =( BOUNDED_CURVE ( )  B_SPLINE_CURVE ( 2, ( #27691, #89532, #73290, #3884, #50963, #81916, #60046, #45352, #84893 ),
 .UNSPECIFIED., .F., .T. ) 
 B_SPLINE_CURVE_WITH_KNOTS ( ( 3, 2, 2, 2, 3 ),
 ( 0.8427419354838709964, 0.8440860215053763715, 0.8467741935483871218, 0.8494623655913978721, 0.8508064516129032473 ),
 .UNSPECIFIED. ) 
 CURVE ( )  GEOMETRIC_REPRESENTATION_ITEM ( )  RATIONAL_B_SPLINE_CURVE ( ( 0.9330127018922194093, 0.9330127018922194093, 1.000000000000000000, 0.8660254037844387076, 1.000000000000000000, 0.8660254037844387076, 1.000000000000000000, 0.9330127018922194093, 0.9330127018922194093 ) ) 
 REPRESENTATION_ITEM ( '' )  );
#60796 = CARTESIAN_POINT ( 'NONE',  ( -16.14394294671762253, 170.6744531367911293, 4.594050593750047540 ) ) ;
#60797 = DIRECTION ( 'NONE',  ( 0.4999999999999992784, -0.8660254037844390407, 0.000000000000000000 ) ) ;
#60798 = ORIENTED_EDGE ( 'NONE', *, *, #94019, .F. ) ;
#60799 = PRODUCT_DEFINITION_FORMATION_WITH_SPECIFIED_SOURCE ( 'ANY', '', #43521, .NOT_KNOWN. ) ;
#60800 = EDGE_CURVE ( 'NONE', #92056, #81006, #9359, .T. ) ;
#60801 = CARTESIAN_POINT ( 'NONE',  ( 66.67858973989486060, 68.09147666472189542, -6.506024203352879454 ) ) ;
#60802 = CARTESIAN_POINT ( 'NONE',  ( 72.81549581358450496, 70.27905260404436660, -8.103349982428230902 ) ) ;
#60803 = CARTESIAN_POINT ( 'NONE',  ( 151.3124059063077311, 268.5662204852269497, -14.45542936000225609 ) ) ;
#60804 = CARTESIAN_POINT ( 'NONE',  ( 10.02652254571713719, 176.5958772461660544, -9.188101187500095079 ) ) ;
#60805 = CARTESIAN_POINT ( 'NONE',  ( 172.2317120015379430, 290.4289517053596228, 2.752192634013410633 ) ) ;
#60806 = CARTESIAN_POINT ( 'NONE',  ( 179.1290479419255064, 274.0445995950666997, -16.71137309026022422 ) ) ;
#60807 = CARTESIAN_POINT ( 'NONE',  ( 20.61848683307935914, 34.83705186507754803, 3.090169943749475401 ) ) ;
#60808 = CARTESIAN_POINT ( 'NONE',  ( 85.63218110832043806, 48.66108713908771932, 12.42024371201311972 ) ) ;
#60809 = CARTESIAN_POINT ( 'NONE',  ( 171.1784325634547201, 271.3965276148621228, -17.73125513023947875 ) ) ;
#60810 = CARTESIAN_POINT ( 'NONE',  ( 72.08668889666979851, 71.79979336344656815, -3.927014794161233890 ) ) ;
#60811 = CYLINDRICAL_SURFACE ( 'NONE', #99254, 10.00000000000010658 ) ;
#60812 = EDGE_CURVE ( 'NONE', #54901, #14998, #80000, .T. ) ;
#60813 = CARTESIAN_POINT ( 'NONE',  ( 175.7745498293659807, 253.0239432584050974, -3.279651895664616124 ) ) ;
#60814 = CARTESIAN_POINT ( 'NONE',  ( 198.7606870255174272, 286.3833868549447743, 17.68329551240030284 ) ) ;
#60815 = CARTESIAN_POINT ( 'NONE',  ( 44.69460199273685674, 206.6115022471903160, -5.000000000000047962 ) ) ;
#60816 = DIRECTION ( 'NONE',  ( -0.8660254037844387076, -0.4999999999999998890, -0.000000000000000000 ) ) ;
#60817 = CARTESIAN_POINT ( 'NONE',  ( 189.8763472015711216, 301.7715148217271803, -0.1184663095182975079 ) ) ;
#60818 = CARTESIAN_POINT ( 'NONE',  ( 15.22267496842377099, 179.5958772461660544, -9.188101187500095079 ) ) ;
#60819 = CARTESIAN_POINT ( 'NONE',  ( 72.67106054446416863, 70.72958228892086652, -7.972900045040105077 ) ) ;
#60820 = CARTESIAN_POINT ( 'NONE',  ( 130.4311169673963775, 246.1115022471902591, 10.00000000000009592 ) ) ;
#60821 = CARTESIAN_POINT ( 'NONE',  ( 77.36600796148924530, 49.13692148722834929, -14.77749963168140113 ) ) ;
#60822 = CARTESIAN_POINT ( 'NONE',  ( 134.5988642195610225, 258.5177522451419350, 5.000000000000046185 ) ) ;
#60823 = B_SPLINE_CURVE_WITH_KNOTS ( 'NONE', 3,
 ( #35013, #18843, #18344, #49722 ),
 .UNSPECIFIED., .F., .F.,
 ( 4, 4 ),
 ( 1.520235486122029408E-16, 0.001720210420923555137 ),
 .UNSPECIFIED. ) ;
#60824 = CARTESIAN_POINT ( 'NONE',  ( 207.6900289502458179, 270.9173129631602706, 7.178327969100043227 ) ) ;
#60825 = CARTESIAN_POINT ( 'NONE',  ( -58.62427208439001447, 70.56504152958493137, 45.00000000000000711 ) ) ;
#60826 = CARTESIAN_POINT ( 'NONE',  ( 49.80235952159635104, 79.38263285747564169, 10.00000000000000000 ) ) ;
#60827 = B_SPLINE_CURVE_WITH_KNOTS ( 'NONE', 3,
 ( #26111, #49401, #87484, #25089 ),
 .UNSPECIFIED., .F., .F.,
 ( 4, 4 ),
 ( 0.008475005499723171562, 0.01486344536556217372 ),
 .UNSPECIFIED. ) ;
#60828 = CARTESIAN_POINT ( 'NONE',  ( 164.1327037607566410, 281.5579544899051712, 8.906674246401461659 ) ) ;
#60829 = PRODUCT_CONTEXT ( 'NONE', #18827, 'mechanical' ) ;
#60830 = CARTESIAN_POINT ( 'NONE',  ( 16.40018271037384068, 27.65586893147755987, -7.433330006724137462 ) ) ;
#60831 = CARTESIAN_POINT ( 'NONE',  ( 15.40662013169548672, 9.864269794150882120, -3.090169943749474069 ) ) ;
#60832 = CARTESIAN_POINT ( 'NONE',  ( 71.41401697283629346, 59.26550905095592725, 15.24935196003983329 ) ) ;
#60833 = AXIS2_PLACEMENT_3D ( 'NONE', #72928, #64806, #62785 ) ;
#60834 = CARTESIAN_POINT ( 'NONE',  ( 155.5770330754656072, 261.1796695529068302, 18.26969263326161297 ) ) ;
#60835 = VERTEX_POINT ( 'NONE', #50058 ) ;
#60836 = CARTESIAN_POINT ( 'NONE',  ( 185.4724630939025758, 290.9233636149379549, 12.26262842363110117 ) ) ;
#60837 = VECTOR ( 'NONE', #23531, 1000.000000000000000 ) ;
#60838 = CARTESIAN_POINT ( 'NONE',  ( 164.6655030961912871, 284.0863298189144643, -8.309311456134647500 ) ) ;
#60839 = CARTESIAN_POINT ( 'NONE',  ( -3.985554314188680003, 180.0530062829863311, 2.649461200531984646E-14 ) ) ;
#60840 = FACE_OUTER_BOUND ( 'NONE', #46896, .T. ) ;
#60841 = ORIENTED_EDGE ( 'NONE', *, *, #44688, .F. ) ;
#60842 = PLANE ( 'NONE',  #52207 ) ;
#60843 = CARTESIAN_POINT ( 'NONE',  ( 71.99578165902696014, 71.45753870159522592, -4.731601630015590310 ) ) ;
#60844 = CARTESIAN_POINT ( 'NONE',  ( 77.23262995875991521, 63.36386537804837360, 15.13973818951359007 ) ) ;
#60845 = CARTESIAN_POINT ( 'NONE',  ( 155.5066938333533528, 261.3015006940112244, -18.40036130547566273 ) ) ;
#60846 = ORIENTED_EDGE ( 'NONE', *, *, #34279, .F. ) ;
#60847 = ORIENTED_EDGE ( 'NONE', *, *, #63540, .F. ) ;
#60849 = CARTESIAN_POINT ( 'NONE',  ( 164.4294002498235159, 245.8469198396639399, 6.098783631055905374 ) ) ;
#60848 = CARTESIAN_POINT ( 'NONE',  ( 187.4676533354318906, 272.4601757945604845, -16.88503403312462936 ) ) ;
#60850 = ORIENTED_EDGE ( 'NONE', *, *, #40469, .F. ) ;
#60851 = CARTESIAN_POINT ( 'NONE',  ( 153.2283961777204695, 265.2476279883323400, -17.66880461074566000 ) ) ;
#60852 = DIRECTION ( 'NONE',  ( -1.000000000000000000, 0.000000000000000000, 0.000000000000000000 ) ) ;
#60853 = DIRECTION ( 'NONE',  ( -0.8660254037844387076, -0.4999999999999998890, -0.000000000000000000 ) ) ;
#60854 = LINE ( 'NONE', #21391, #19329 ) ;
#60855 = ORIENTED_EDGE ( 'NONE', *, *, #53722, .T. ) ;
#60856 = CARTESIAN_POINT ( 'NONE',  ( 147.8503508990560533, 274.5626756563852950, 7.845851077393495743 ) ) ;
#60857 = CARTESIAN_POINT ( 'NONE',  ( 149.5390997184345281, 271.6376768999995761, -11.52989534384373016 ) ) ;
#60858 = CARTESIAN_POINT ( 'NONE',  ( 178.9737876148604130, 272.7588148741942291, 17.78336666879676642 ) ) ;
#60859 = EDGE_CURVE ( 'NONE', #18980, #100037, #6073, .T. ) ;
#60860 = ORIENTED_EDGE ( 'NONE', *, *, #58748, .T. ) ;
#60861 = CARTESIAN_POINT ( 'NONE',  ( 205.8918578537579833, 274.0318366629789466, 11.52627491423194250 ) ) ;
#60862 = VECTOR ( 'NONE', #36767, 1000.000000000000000 ) ;
#60863 = CARTESIAN_POINT ( 'NONE',  ( 75.25170673533752108, 66.73598490943447814, 12.94887977284632896 ) ) ;
#60864 = ORIENTED_EDGE ( 'NONE', *, *, #13996, .T. ) ;
#60865 = CARTESIAN_POINT ( 'NONE',  ( 149.6036070299368532, 271.5259469590175740, 11.63513718912356865 ) ) ;
#60866 = CARTESIAN_POINT ( 'NONE',  ( 156.2224770818481545, 267.4677849582849376, -16.91854127892884208 ) ) ;
#60867 = ADVANCED_FACE ( 'NONE', ( #28245 ), #41444, .F. ) ;
#60868 = ORIENTED_EDGE ( 'NONE', *, *, #16976, .T. ) ;
#60869 = CARTESIAN_POINT ( 'NONE',  ( 2.945768331249355665, 38.91607694435867160, 59.99999999999999289 ) ) ;
#60870 = CARTESIAN_POINT ( 'NONE',  ( 88.86189758574327868, 222.1115022471902591, 10.00000000000009592 ) ) ;
#60871 = CARTESIAN_POINT ( 'NONE',  ( 78.22627483185729602, 47.75561434913958436, -14.49489253473961092 ) ) ;
#60873 = AXIS2_PLACEMENT_3D ( 'NONE', #49290, #23975, #54874 ) ;
#60872 = CARTESIAN_POINT ( 'NONE',  ( 83.83559978620640152, 51.92718615610179711, 14.52128790932804137 ) ) ;
#60874 = ORIENTED_EDGE ( 'NONE', *, *, #41095, .T. ) ;
#60875 = ORIENTED_EDGE ( 'NONE', *, *, #49202, .F. ) ;
#60876 = CARTESIAN_POINT ( 'NONE',  ( 80.86872469022158327, 51.16822586326628652, -15.30852264838738108 ) ) ;
#60877 = CARTESIAN_POINT ( 'NONE',  ( 146.8729474948188454, 276.2555880120147549, 3.934020695290606273 ) ) ;
#60878 = CARTESIAN_POINT ( 'NONE',  ( 147.7978300115112233, 274.6536445020713018, 7.902890709649431855 ) ) ;
#60879 = CARTESIAN_POINT ( 'NONE',  ( 149.0761751337341821, 272.4394858007734683, 11.56094486755886130 ) ) ;
#60880 = CARTESIAN_POINT ( 'NONE',  ( 153.4289928607825573, 264.9001843414388873, 17.27358709529985958 ) ) ;
#60881 = EDGE_CURVE ( 'NONE', #53329, #86782, #78577, .T. ) ;
#60882 = CARTESIAN_POINT ( 'NONE',  ( 147.1288613282876554, 275.8123322500870245, 0.6663123207720744734 ) ) ;
#60883 = CARTESIAN_POINT ( 'NONE',  ( 147.2592533090473239, 275.5864867145116932, -0.3770461397900867762 ) ) ;
#60885 = FACE_OUTER_BOUND ( 'NONE', #95075, .T. ) ;
#60884 = B_SPLINE_CURVE_WITH_KNOTS ( 'NONE', 3,
 ( #95624, #50455, #97584, #35758, #89997, #20573, #51451, #82420, #26173, #10985, #41857, #72802, #38218, #84880, #30651, #91996, #75271, #53918, #99069, #61535, #68637, #74784, #21559, #51959, #5364, #90997, #92478, #52441, #22547, #14929, #5856, #45337, #75769, #36741, #36245, #13955, #43845, #76269, #68141, #82899, #6357, #6842, #67647, #29162, #37243, #90510 ),
 .UNSPECIFIED., .F., .F.,
 ( 4, 1, 2, 2, 1, 2, 2, 1, 1, 2, 2, 1, 1, 2, 2, 1, 1, 2, 2, 1, 1, 1, 2, 2, 1, 1, 1, 2, 2, 4 ),
 ( 0.000000000000000000, 0.06249999999998620548, 0.09374999999997919720, 0.1249999999999721889, 0.1874999999999613365, 0.2187499999999554523, 0.2499999999999495959, 0.3124999999999385492, 0.3437499999999330536, 0.3593749999999300004, 0.3749999999999269473, 0.4374999999999178990, 0.4687499999999141798, 0.4843749999999123479, 0.4999999999999105160, 0.5624999999999169553, 0.5937499999999182876, 0.6093749999999193978, 0.6249999999999203970, 0.6874999999999228395, 0.7187499999999235056, 0.7343749999999257261, 0.7421874999999290567, 0.7499999999999322764, 0.8124999999999713562, 0.8437499999999910072, 0.8593750000000005551, 0.8671875000000035527, 0.8750000000000065503, 1.000000000000000000 ),
 .UNSPECIFIED. ) ;
#60886 = B_SPLINE_CURVE_WITH_KNOTS ( 'NONE', 3,
 ( #6615, #16, #84641, #45589 ),
 .UNSPECIFIED., .F., .F.,
 ( 4, 4 ),
 ( 5.779565477066665081E-15, 0.005039604220546898931 ),
 .UNSPECIFIED. ) ;
#60887 = CARTESIAN_POINT ( 'NONE',  ( 70.25033766539972646, 68.19075070162745078, 8.808644737539518488 ) ) ;
#60888 = LINE ( 'NONE', #91851, #40145 ) ;
#60889 = CARTESIAN_POINT ( 'NONE',  ( 67.12762392158883529, 66.70947246983655532, 8.261873050784338091 ) ) ;
#60890 = CARTESIAN_POINT ( 'NONE',  ( 171.5146568604302502, 288.8597905981943654, 4.230659075081162790 ) ) ;
#60891 = CARTESIAN_POINT ( 'NONE',  ( 78.37377739669621235, 47.42489695864805554, 14.28740524439509230 ) ) ;
#60892 = CARTESIAN_POINT ( 'NONE',  ( 104.3964885861764600, 221.8923013555410080, 4.594050593750050204 ) ) ;
#60893 = ORIENTED_EDGE ( 'NONE', *, *, #78407, .F. ) ;
#60894 = DIRECTION ( 'NONE',  ( -0.8660254037844387076, -0.4999999999999998890, -0.000000000000000000 ) ) ;
#60895 = CARTESIAN_POINT ( 'NONE',  ( 80.28604642359979948, 52.75975974871795415, -15.47868605385456497 ) ) ;
#60896 = CARTESIAN_POINT ( 'NONE',  ( 200.3293654959697392, 273.7156512906800572, 13.98704503334941229 ) ) ;
#60897 = EDGE_CURVE ( 'NONE', #49659, #66923, #7327, .T. ) ;
#60898 = CARTESIAN_POINT ( 'NONE',  ( 79.11953551025055731, 46.13320601581522595, 12.69056890641700086 ) ) ;
#60899 = EDGE_CURVE ( 'NONE', #34934, #44815, #33884, .T. ) ;
#60900 = CARTESIAN_POINT ( 'NONE',  ( -17.42236680055705023, 149.2012482093457777, 0.000000000000000000 ) ) ;
#60901 = CARTESIAN_POINT ( 'NONE',  ( 189.8305642146623029, 301.8508132811754763, -0.4120780911254784407 ) ) ;
#60902 = CARTESIAN_POINT ( 'NONE',  ( 69.26382730489497419, 65.05794468884164417, -11.47466192821767805 ) ) ;
#60903 = ORIENTED_EDGE ( 'NONE', *, *, #8863, .F. ) ;
#60904 = CARTESIAN_POINT ( 'NONE',  ( 208.2124092825819162, 270.0125236866795149, -2.339659020816897694 ) ) ;
#60905 = FACE_OUTER_BOUND ( 'NONE', #57784, .T. ) ;
#60906 = CARTESIAN_POINT ( 'NONE',  ( 72.16868224958085420, 71.71251872039211150, 5.498261171115592205 ) ) ;
#60907 = CARTESIAN_POINT ( 'NONE',  ( 37.53185021205516847, 199.1427522451419065, 10.00000000000009237 ) ) ;
#60908 = CARTESIAN_POINT ( 'NONE',  ( 118.1174918034448922, 232.8768266524160140, 9.188101187500096856 ) ) ;
#60909 = CARTESIAN_POINT ( 'NONE',  ( 198.9369963555428740, 286.0780101374919013, -18.58432392708837710 ) ) ;
#60910 = DIRECTION ( 'NONE',  ( -0.8660254037844377084, -0.5000000000000014433, -0.000000000000000000 ) ) ;
#60911 = CARTESIAN_POINT ( 'NONE',  ( 157.8849654228661166, 257.1822134667773980, 17.43614750057631468 ) ) ;
#60912 = CARTESIAN_POINT ( 'NONE',  ( 41.97569090598254604, 208.3207943907112849, 18.47570218321542868 ) ) ;
#60913 = CARTESIAN_POINT ( 'NONE',  ( 37.57712925149210292, 186.3768266524160140, 9.188101187500098632 ) ) ;
#60914 = VECTOR ( 'NONE', #66392, 1000.000000000000000 ) ;
#60915 = DIRECTION ( 'NONE',  ( -0.8435938723211520163, -0.5369817302126803638, 0.000000000000000000 ) ) ;
#60916 = CIRCLE ( 'NONE', #9235, 3.300000000000010925 ) ;
#60917 = VERTEX_POINT ( 'NONE', #60125 ) ;
#60918 = CARTESIAN_POINT ( 'NONE',  ( 178.9948746410809690, 264.1102681154287097, -15.56640332105143720 ) ) ;
#60919 = CARTESIAN_POINT ( 'NONE',  ( 178.1274316576357819, 265.4983894697847404, 15.93396044624996399 ) ) ;
#60920 = EDGE_CURVE ( 'NONE', #16011, #36668, #74993, .T. ) ;
#60921 = B_SPLINE_SURFACE_WITH_KNOTS ( 'NONE', 3, 1, ( 
 ( #53073, #83521 ),
 ( #14084, #89638 ),
 ( #90122, #43472 ),
 ( #44466, #84028 ),
 ( #90637, #6974 ),
 ( #20200, #76399 ),
 ( #82541, #37858 ),
 ( #52078, #75398 ),
 ( #75908, #5001 ),
 ( #74416, #5982 ),
 ( #35878, #36877 ),
 ( #97707, #13105 ),
 ( #7467, #99691 ),
 ( #69269, #84518 ),
 ( #54051, #30275 ),
 ( #77385, #38360 ),
 ( #46455, #94116 ),
 ( #78392, #70775 ),
 ( #70264, #377 ),
 ( #92133, #7987 ),
 ( #31751, #23655 ),
 ( #24177, #61164 ),
 ( #85009, #38863 ),
 ( #77893, #47958 ),
 ( #31265, #32269 ),
 ( #15061, #69769 ),
 ( #55060, #62657 ),
 ( #1389, #93608 ),
 ( #8973, #86043 ),
 ( #15553, #23160 ),
 ( #39843, #100198 ),
 ( #40356, #63172 ),
 ( #76869, #62152 ),
 ( #85529, #16571 ) ),
 .UNSPECIFIED., .T., .F., .F.,
 ( 4, 2, 2, 2, 2, 2, 2, 2, 2, 2, 2, 2, 2, 2, 2, 2, 4 ),
 ( 2, 2 ),
 ( 0.000000000000000000, 0.06250000000000000000, 0.1250000000000000000, 0.1875000000000000000, 0.2500000000000000000, 0.3125000000000000000, 0.3750000000000000000, 0.4375000000000000000, 0.5000000000000000000, 0.5625000000000000000, 0.6250000000000000000, 0.6875000000000000000, 0.7500000000000000000, 0.8125000000000000000, 0.8750000000000000000, 0.9375000000000000000, 1.000000000000000000 ),
 ( 0.000000000000000000, 1.000000000000000000 ),
 .UNSPECIFIED. ) ;
#60922 = CARTESIAN_POINT ( 'NONE',  ( 49.66226845319755512, 83.29899382260626339, 10.00000000000000000 ) ) ;
#60923 = VECTOR ( 'NONE', #56419, 1000.000000000000114 ) ;
#60924 = DIRECTION ( 'NONE',  ( 0.000000000000000000, -0.000000000000000000, 1.000000000000000000 ) ) ;
#60925 = CARTESIAN_POINT ( 'NONE',  ( 81.93485011922251715, 41.32099105351304758, -5.877334436009162388 ) ) ;
#60926 = CARTESIAN_POINT ( 'NONE',  ( 76.45572749640669485, 51.64231386250387601, -16.15369532800221108 ) ) ;
#60927 = CARTESIAN_POINT ( 'NONE',  ( 68.68909986782581711, 64.16576715805911135, -12.55144644517788421 ) ) ;
#60928 = EDGE_CURVE ( 'NONE', #35860, #80312, #97960, .T. ) ;
#60929 = CARTESIAN_POINT ( 'NONE',  ( 106.0921946783233096, 225.3927522451418213, 10.00000000000009592 ) ) ;
#60930 = DIRECTION ( 'NONE',  ( 0.7691052716734813055, 0.08748735329024863450, 0.6331058711608413825 ) ) ;
#60931 = ORIENTED_EDGE ( 'NONE', *, *, #10382, .T. ) ;
#60932 = CARTESIAN_POINT ( 'NONE',  ( 161.2977680094314223, 251.2710659906439616, -13.03191437619249982 ) ) ;
#60933 = EDGE_CURVE ( 'NONE', #24489, #69981, #65289, .T. ) ;
#60934 = CARTESIAN_POINT ( 'NONE',  ( 155.4040338355446522, 279.7651995206167612, -2.031698524654040661 ) ) ;
#60935 = CARTESIAN_POINT ( 'NONE',  ( 154.2086446512540761, 265.3719949574480665, 17.07260120196946573 ) ) ;
#60936 = ADVANCED_FACE ( 'NONE', ( #85488 ), #77343, .T. ) ;
#60937 = VECTOR ( 'NONE', #8483, 1000.000000000000000 ) ;
#60938 = CARTESIAN_POINT ( 'NONE',  ( 21.69106252476256458, 174.1423013555409796, -4.594050593750043987 ) ) ;
#60939 = CARTESIAN_POINT ( 'NONE',  ( 7.004301291108590455, 25.81751292744054282, -6.180339887498951690 ) ) ;
#60940 = AXIS2_PLACEMENT_3D ( 'NONE', #79157, #48211, #9738 ) ;
#60941 = CARTESIAN_POINT ( 'NONE',  ( -14.47810378888552130, 105.4554537110193024, 43.92042717844079647 ) ) ;
#60942 = LINE ( 'NONE', #6761, #41651 ) ;
#60943 = CARTESIAN_POINT ( 'NONE',  ( 73.13555747811004437, 69.81939941050913490, 9.605153593488003239 ) ) ;
#60944 = EDGE_CURVE ( 'NONE', #81025, #14044, #40318, .T. ) ;
#60946 = CARTESIAN_POINT ( 'NONE',  ( 71.67687952550437558, 206.0643266524160140, 9.188101187500095079 ) ) ;
#60945 = CARTESIAN_POINT ( 'NONE',  ( 195.5687578856996822, 275.7294477338082288, -15.46242989827094227 ) ) ;
#60947 = CARTESIAN_POINT ( 'NONE',  ( 208.3135187673106543, 269.8373969220020285, 2.829653198597726682 ) ) ;
#60948 = CARTESIAN_POINT ( 'NONE',  ( 72.58511477355777686, 57.25044146139839540, 15.86244954290823017 ) ) ;
#60949 = CARTESIAN_POINT ( 'NONE',  ( -30.57234814819119606, 96.78886779632826176, 44.55697900252199162 ) ) ;
#60950 = CARTESIAN_POINT ( 'NONE',  ( 164.9836323268835940, 244.8869617230113249, -2.696511969808454534 ) ) ;
#60951 = ORIENTED_EDGE ( 'NONE', *, *, #48102, .F. ) ;
#60952 = CARTESIAN_POINT ( 'NONE',  ( 163.0340262847632289, 267.8216940496866982, 16.48747052884350950 ) ) ;
#60953 = CARTESIAN_POINT ( 'NONE',  ( 17.48697055717582316, 174.2365022471902023, -10.00000000000009059 ) ) ;
#60954 = CARTESIAN_POINT ( 'NONE',  ( 163.9910908123517288, 246.6060940548019289, -7.333295033952830444 ) ) ;
#60955 = CARTESIAN_POINT ( 'NONE',  ( 137.6570164284488271, 250.2833772461660544, -9.188101187500095079 ) ) ;
#60956 = CARTESIAN_POINT ( 'NONE',  ( 35.39919958817179690, 22.29860640527294535, -2.839279412974138328 ) ) ;
#60957 = CARTESIAN_POINT ( 'NONE',  ( 167.6212268600468462, 262.3307149636390818, -17.03867496724294028 ) ) ;
#60958 = LINE ( 'NONE', #5288, #85672 ) ;
#60959 = CARTESIAN_POINT ( 'NONE',  ( 75.12085108667970701, 52.90659536716842126, -15.99877795348665011 ) ) ;
#60961 = CARTESIAN_POINT ( 'NONE',  ( 170.4623819437503016, 288.8056674672355939, -5.476885062779371260 ) ) ;
#60960 = CARTESIAN_POINT ( 'NONE',  ( 203.9914640947099826, 268.0458192746789337, 1.179109546621946114 ) ) ;
#60962 = PLANE ( 'NONE',  #78858 ) ;
#60963 = EDGE_LOOP ( 'NONE', ( #90984, #37325, #14469, #7326 ) ) ;
#60964 = CARTESIAN_POINT ( 'NONE',  ( 64.58718584504546811, 196.5494855054052152, -2.679491924311248496 ) ) ;
#60965 =( LENGTH_UNIT ( ) NAMED_UNIT ( * ) SI_UNIT ( .MILLI., .METRE. ) );
#60966 = CARTESIAN_POINT ( 'NONE',  ( 170.8843335314017509, 274.4719442773359219, 17.28596511953734449 ) ) ;
#60967 = LINE ( 'NONE', #62452, #79058 ) ;
#60968 = CARTESIAN_POINT ( 'NONE',  ( 12.16146256644911716, 9.947547579820875896, 5.678558825948272215 ) ) ;
#60969 = ORIENTED_EDGE ( 'NONE', *, *, #72032, .T. ) ;
#60970 = CARTESIAN_POINT ( 'NONE',  ( 206.7474059308681262, 272.5499839251064031, 9.504501883383504435 ) ) ;
#60971 = CARTESIAN_POINT ( 'NONE',  ( -14.42967401501114999, 169.1427522451419065, 10.00000000000009415 ) ) ;
#60972 = LINE ( 'NONE', #187, #61898 ) ;
#60973 = CARTESIAN_POINT ( 'NONE',  ( 31.27120823407814854, 178.8615022471902023, 5.000000000000051514 ) ) ;
#60974 = CARTESIAN_POINT ( 'NONE',  ( 175.8759543544349810, 265.7665519414402979, 16.89567470503287794 ) ) ;
#60975 = CARTESIAN_POINT ( 'NONE',  ( 208.0006710756887287, 270.3792650189220126, -0.8737665032493013850 ) ) ;
#60976 = CARTESIAN_POINT ( 'NONE',  ( -51.76626358812258388, 84.50539129967802410, -10.00000000000000000 ) ) ;
#60977 = VERTEX_POINT ( 'NONE', #39312 ) ;
#60978 = CYLINDRICAL_SURFACE ( 'NONE', #4988, 70.00000000000002842 ) ;
#60979 = CARTESIAN_POINT ( 'NONE',  ( 10.55946980724658069, 24.83478043621386888, -8.090169943749479842 ) ) ;
#60980 = CARTESIAN_POINT ( 'NONE',  ( 86.70911053808110580, 46.89117940024963360, 10.21290512048939014 ) ) ;
#60981 = VERTEX_POINT ( 'NONE', #1348 ) ;
#60982 = CARTESIAN_POINT ( 'NONE',  ( 149.6700657135140489, 271.4108371424580355, 12.58635654151485284 ) ) ;
#60983 = CARTESIAN_POINT ( 'NONE',  ( 86.54659259230355417, 47.35344409918261732, -10.80230753912617914 ) ) ;
#60984 = CARTESIAN_POINT ( 'NONE',  ( 189.1253271041844073, 297.0913391992372112, 8.133032840077193626 ) ) ;
#60985 = EDGE_LOOP ( 'NONE', ( #67582, #27977, #9602, #49299 ) ) ;
#60986 = CARTESIAN_POINT ( 'NONE',  ( 191.8210230231139803, 298.4032374945642232, -8.800268167321144475 ) ) ;
#60987 = CARTESIAN_POINT ( 'NONE',  ( 162.9254136962317148, 277.9293967287522946, 13.77390558128574760 ) ) ;
#60988 = CARTESIAN_POINT ( 'NONE',  ( 163.8670932201372352, 246.8208641845333773, 5.912697114930636211 ) ) ;
#60989 = AXIS2_PLACEMENT_3D ( 'NONE', #14496, #45859, #68675 ) ;
#60990 = CARTESIAN_POINT ( 'NONE',  ( 69.94772996192264713, 62.88149894362739190, 13.87021638775245336 ) ) ;
#60991 = ORIENTED_EDGE ( 'NONE', *, *, #65121, .F. ) ;
#60992 = CARTESIAN_POINT ( 'NONE',  ( 101.1217432541752856, 223.0643266524159571, -9.188101187500093303 ) ) ;
#60993 = CARTESIAN_POINT ( 'NONE',  ( 200.1102648775588193, 284.0458494464393198, 17.54251420653697835 ) ) ;
#60994 = CARTESIAN_POINT ( 'NONE',  ( 81.22534965261213813, 42.38499988906294647, -7.548277495761163358 ) ) ;
#60995 = ORIENTED_EDGE ( 'NONE', *, *, #75477, .T. ) ;
#60996 = ORIENTED_EDGE ( 'NONE', *, *, #21395, .F. ) ;
#60997 = ORIENTED_EDGE ( 'NONE', *, *, #45322, .F. ) ;
#60998 = CARTESIAN_POINT ( 'NONE',  ( 81.90811180363191113, 52.66149361526625938, 15.20919891352879993 ) ) ;
#60999 = ORIENTED_EDGE ( 'NONE', *, *, #47220, .F. ) ;
#61000 = CARTESIAN_POINT ( 'NONE',  ( 68.31157111924099468, 68.55647029866582898, 6.335902121074872717 ) ) ;
#61001 = ORIENTED_EDGE ( 'NONE', *, *, #41483, .T. ) ;
#61002 = CARTESIAN_POINT ( 'NONE',  ( 163.7323023463233937, 247.0543288263758086, -6.244751637846886361 ) ) ;
#61003 = CIRCLE ( 'NONE', #82114, 0.1418229129680828593 ) ;
#61004 = CARTESIAN_POINT ( 'NONE',  ( 169.2996641469526367, 281.9763651243665095, 11.69048842974035018 ) ) ;
#61005 = CARTESIAN_POINT ( 'NONE',  ( -23.56280764616852963, 99.74919597147199113, 45.19946569820528737 ) ) ;
#61006 = EDGE_CURVE ( 'NONE', #91430, #79527, #46420, .T. ) ;
#61007 = CARTESIAN_POINT ( 'NONE',  ( 82.86418038935372010, 53.70170152444392642, -15.38246542855200261 ) ) ;
#61008 = CARTESIAN_POINT ( 'NONE',  ( 75.28641870618297105, 56.93067274799551569, -16.55615621114917957 ) ) ;
#61009 = CARTESIAN_POINT ( 'NONE',  ( 16.25825050073692069, 15.10170272979925876, -7.433330006724141015 ) ) ;
#61010 = CARTESIAN_POINT ( 'NONE',  ( 201.6553334440559695, 279.0490965050211116, -15.83750187978207435 ) ) ;
#61011 = LINE ( 'NONE', #22533, #40220 ) ;
#61013 = ORIENTED_EDGE ( 'NONE', *, *, #49498, .F. ) ;
#61012 = CARTESIAN_POINT ( 'NONE',  ( 123.7735466722555771, 232.2677522451417929, -5.000000000000041744 ) ) ;
#61014 = CIRCLE ( 'NONE', #41637, 17.82106496071138935 ) ;
#61015 = CARTESIAN_POINT ( 'NONE',  ( 203.0507839702407580, 278.9527209772879814, 16.21318481136342626 ) ) ;
#61016 = CARTESIAN_POINT ( 'NONE',  ( 188.7366574086433388, 259.9223475325732124, 2.251677873538305175 ) ) ;
#61017 = EDGE_CURVE ( 'NONE', #97001, #29279, #16533, .T. ) ;
#61018 = CARTESIAN_POINT ( 'NONE',  ( 80.00173192732594885, 44.68233805328101482, 11.15140268308046601 ) ) ;
#61019 = CARTESIAN_POINT ( 'NONE',  ( 182.0925017600785054, 256.7772607896355339, 6.510642260905229683 ) ) ;
#61020 = EDGE_CURVE ( 'NONE', #97169, #59501, #59151, .T. ) ;
#61021 = CARTESIAN_POINT ( 'NONE',  ( 171.5232944563295234, 255.4040756630877524, 11.03579953863793328 ) ) ;
#61022 = CARTESIAN_POINT ( 'NONE',  ( 192.2546761845801200, 262.7471528669759664, -0.7532661484371161453 ) ) ;
#61023 = EDGE_LOOP ( 'NONE', ( #82862, #63125, #98040, #15112 ) ) ;
#61024 = CARTESIAN_POINT ( 'NONE',  ( 181.8631805538818469, 270.4478486503479076, -17.10574755700200456 ) ) ;
#61025 = AXIS2_PLACEMENT_3D ( 'NONE', #85299, #62948, #157 ) ;
#61026 = CARTESIAN_POINT ( 'NONE',  ( 75.03771487841180488, 67.29470115673238695, -12.93936238812017336 ) ) ;
#61027 = PLANE ( 'NONE',  #64549 ) ;
#61028 = CARTESIAN_POINT ( 'NONE',  ( 3.035171627975086217, 165.8927522451417929, -10.00000000000009059 ) ) ;
#61029 = B_SPLINE_CURVE_WITH_KNOTS ( 'NONE', 3,
 ( #47691, #17305, #70501, #31993, #94843, #41088, #62903, #16804, #48209, #40086, #25404, #56295, #92841, #77629, #1632, #17823, #10220, #31001, #61890, #56800, #26913, #95861, #88269, #87785 ),
 .UNSPECIFIED., .F., .F.,
 ( 4, 2, 2, 2, 2, 2, 2, 2, 2, 2, 2, 4 ),
 ( 0.000000000000000000, 0.1250000000000054123, 0.2500000000000108247, 0.3750000000000162093, 0.4375000000000207057, 0.5000000000000252021, 0.5625000000000296430, 0.6250000000000341949, 0.6875000000000386358, 0.7500000000000431877, 0.8750000000000215383, 1.000000000000000000 ),
 .UNSPECIFIED. ) ;
#61030 = CARTESIAN_POINT ( 'NONE',  ( 193.9656327198519250, 268.1476455479440801, -10.86522118760852251 ) ) ;
#61031 = CARTESIAN_POINT ( 'NONE',  ( 172.3697519336014921, 280.6551101671673223, -15.35839400997692650 ) ) ;
#61032 = CARTESIAN_POINT ( 'NONE',  ( 163.4595051773099215, 247.5268273832681132, -8.749824153777744584 ) ) ;
#61033 = CARTESIAN_POINT ( 'NONE',  ( 86.19940314562042261, 44.63913117227356508, -6.631687147223989776 ) ) ;
#61034 = CARTESIAN_POINT ( 'NONE',  ( 162.5256129416874558, 250.7632698397880233, -12.89907038147651619 ) ) ;
#61036 = CARTESIAN_POINT ( 'NONE',  ( 24.34666095796415419, 37.55466486950700755, 7.012934429366973338E-14 ) ) ;
#61035 = CARTESIAN_POINT ( 'NONE',  ( -4.262896616726100874, 168.3458772461660544, 9.188101187500095079 ) ) ;
#61037 = CARTESIAN_POINT ( 'NONE',  ( 58.36827475829091583, 216.0530062829863311, -4.648177544792955347E-16 ) ) ;
#61038 = VERTEX_POINT ( 'NONE', #54016 ) ;
#61039 = VERTEX_POINT ( 'NONE', #9443 ) ;
#61040 = DIRECTION ( 'NONE',  ( 0.000000000000000000, 0.000000000000000000, 1.000000000000000000 ) ) ;
#61041 = CYLINDRICAL_SURFACE ( 'NONE', #77146, 14.99999999999968381 ) ;
#61042 = CARTESIAN_POINT ( 'NONE',  ( 84.15081258030213007, 46.26608709097053662, -10.48838324873663019 ) ) ;
#61043 = CARTESIAN_POINT ( 'NONE',  ( 193.5005633302724277, 262.8551920378705518, -5.236817587991198231 ) ) ;
#61044 = CARTESIAN_POINT ( 'NONE',  ( 202.2805801041352254, 280.2867532055686297, -17.40773220476747696 ) ) ;
#61045 = CARTESIAN_POINT ( 'NONE',  ( 198.8683739244561082, 276.4215138120039796, -15.93986209720707414 ) ) ;
#61046 = CARTESIAN_POINT ( 'NONE',  ( 150.0128543151502072, 276.7587017117480173, 3.258831262238442772 ) ) ;
#61047 = EDGE_CURVE ( 'NONE', #97906, #40669, #4315, .T. ) ;
#61048 = B_SPLINE_CURVE_WITH_KNOTS ( 'NONE', 3,
 ( #25952, #2651, #4122, #88294 ),
 .UNSPECIFIED., .F., .F.,
 ( 4, 4 ),
 ( 0.01040196219446366636, 0.01876899884930364679 ),
 .UNSPECIFIED. ) ;
#61049 = CARTESIAN_POINT ( 'NONE',  ( 19.09298631340924501, 172.6423013555409796, -4.594050593750043987 ) ) ;
#61050 = CARTESIAN_POINT ( 'NONE',  ( 112.3797264076079756, 241.8149278399160949, 9.188101187500093303 ) ) ;
#61051 = CARTESIAN_POINT ( 'NONE',  ( 181.3848234261387802, 294.5949326645637711, -6.610599456467063817 ) ) ;
#61052 = CARTESIAN_POINT ( 'NONE',  ( 183.4174296676025904, 257.2981747246719806, -3.184370871148272109 ) ) ;
#61053 = CARTESIAN_POINT ( 'NONE',  ( 149.9951969083232370, 271.6664457055391040, -11.69466652306437560 ) ) ;
#61054 = EDGE_CURVE ( 'NONE', #78693, #8334, #8443, .T. ) ;
#61055 = CARTESIAN_POINT ( 'NONE',  ( -56.12829894168721978, 48.04152121768972705, 59.99999999999999289 ) ) ;
#61056 = VECTOR ( 'NONE', #36507, 1000.000000000000000 ) ;
#61057 = CARTESIAN_POINT ( 'NONE',  ( 77.86314341856081001, 54.34344560458549012, -16.01061743008826355 ) ) ;
#61058 = CARTESIAN_POINT ( 'NONE',  ( 195.8449251089225811, 291.4336346372613775, 16.14492769602857081 ) ) ;
#61059 = VECTOR ( 'NONE', #48275, 1000.000000000000000 ) ;
#61060 = DIRECTION ( 'NONE',  ( 0.000000000000000000, 0.000000000000000000, 1.000000000000000000 ) ) ;
#61061 = CARTESIAN_POINT ( 'NONE',  ( 207.5462191418491500, 271.1663988579299485, -5.239401497773396699 ) ) ;
#61062 = CARTESIAN_POINT ( 'NONE',  ( 189.2296340506370029, 284.2231390282569237, 16.49936049877286592 ) ) ;
#61063 = EDGE_CURVE ( 'NONE', #24620, #62277, #31714, .T. ) ;
#61064 = CARTESIAN_POINT ( 'NONE',  ( 168.0319076612829861, 278.6233240676867240, 14.86836655933751317 ) ) ;
#61065 = CARTESIAN_POINT ( 'NONE',  ( 189.2051289032725947, 299.6734310816647167, -0.5827320972813355704 ) ) ;
#61066 = CARTESIAN_POINT ( 'NONE',  ( 68.71908087017774847, 68.45513031344326293, 6.959568858202175967 ) ) ;
#61067 = CARTESIAN_POINT ( 'NONE',  ( -19.51556777096616457, 93.03053543526598901, 59.99999999999999289 ) ) ;
#61068 = CARTESIAN_POINT ( 'NONE',  ( 184.3466702497243830, 268.6818309632849946, -15.29285969151670521 ) ) ;
#61069 = VERTEX_POINT ( 'NONE', #47922 ) ;
#61070 = CARTESIAN_POINT ( 'NONE',  ( 166.5497620933320775, 284.9599651698292178, -8.643830016708903941 ) ) ;
#61071 = CARTESIAN_POINT ( 'NONE',  ( 181.4153963986084079, 267.9065476240749604, 15.01311212035915332 ) ) ;
#61072 = CARTESIAN_POINT ( 'NONE',  ( 99.71410487726056715, 234.5024278399160949, 9.188101187500095079 ) ) ;
#61073 = CARTESIAN_POINT ( 'NONE',  ( 207.8431546909062320, 270.6520914003897360, -6.441273666418043220 ) ) ;
#61074 = CARTESIAN_POINT ( 'NONE',  ( 151.3589047706063582, 268.4856820897672378, 14.56544807350869419 ) ) ;
#61075 = DIRECTION ( 'NONE',  ( -0.2702110370271911810, -0.9515975153008192633, -0.1464519181915933110 ) ) ;
#61076 = AXIS2_PLACEMENT_3D ( 'NONE', #1586, #32956, #65360 ) ;
#61078 = CARTESIAN_POINT ( 'NONE',  ( 191.6900977084123951, 277.0292895703833551, 16.71431191694982843 ) ) ;
#61077 = DIRECTION ( 'NONE',  ( -0.5000000000000016653, 0.8660254037844377084, 0.000000000000000000 ) ) ;
#61079 = CARTESIAN_POINT ( 'NONE',  ( 201.9158970844873977, 271.2653056115948402, -9.820632838803758702 ) ) ;
#61080 = CARTESIAN_POINT ( 'NONE',  ( 198.4427928769277969, 286.9339956717308837, -17.97122743692687763 ) ) ;
#61081 = DIRECTION ( 'NONE',  ( 0.000000000000000000, -0.000000000000000000, 1.000000000000000000 ) ) ;
#61082 = CARTESIAN_POINT ( 'NONE',  ( 41.95273645663377948, 27.14754757982093381, -5.678558825948275768 ) ) ;
#61083 = CARTESIAN_POINT ( 'NONE',  ( -19.65312891409030271, 93.06504152958497400, 177.5919119679930134 ) ) ;
#61084 = CARTESIAN_POINT ( 'NONE',  ( 174.4279836968870541, 287.7471250269960592, -10.96444086789414030 ) ) ;
#61085 = VERTEX_POINT ( 'NONE', #87008 ) ;
#61086 = CARTESIAN_POINT ( 'NONE',  ( 28.77833178495667710, 28.56628583063842441, 9.188101187500006262 ) ) ;
#61087 = VECTOR ( 'NONE', #77611, 1000.000000000000000 ) ;
#61088 = CARTESIAN_POINT ( 'NONE',  ( 70.81027263193901433, 64.39395113940368276, -13.25098958810220395 ) ) ;
#61089 = CARTESIAN_POINT ( 'NONE',  ( 192.8607783413999073, 296.6023284558532396, -11.80574095728561446 ) ) ;
#61090 = CARTESIAN_POINT ( 'NONE',  ( 196.4783028304046013, 290.3365922432724346, -16.37291435488387492 ) ) ;
#61091 = CARTESIAN_POINT ( 'NONE',  ( 84.81216594078708226, 50.08139507223255293, -13.70157583983569971 ) ) ;
#61092 = CARTESIAN_POINT ( 'NONE',  ( 76.01947567912945658, 65.31078134063972129, -14.44091581795174051 ) ) ;
#61093 = CARTESIAN_POINT ( 'NONE',  ( 183.4250023545107524, 264.1063932265387280, -13.71376836473408645 ) ) ;
#61094 = CARTESIAN_POINT ( 'NONE',  ( 169.3341204084158846, 252.1170729295009778, -8.741246645408743632 ) ) ;
#61095 = DIRECTION ( 'NONE',  ( 0.000000000000000000, 0.000000000000000000, 1.000000000000000000 ) ) ;
#61096 = AXIS2_PLACEMENT_3D ( 'NONE', #67168, #37262, #14948 ) ;
#61097 = ORIENTED_EDGE ( 'NONE', *, *, #85127, .T. ) ;
#61098 = CARTESIAN_POINT ( 'NONE',  ( 187.2681015796103736, 278.8103706783136317, 17.45891525344013218 ) ) ;
#61099 = CARTESIAN_POINT ( 'NONE',  ( 28.93411276635479368, 38.74646525600392266, 2.839279412974139660 ) ) ;
#61100 = ORIENTED_EDGE ( 'NONE', *, *, #54772, .F. ) ;
#61101 = CARTESIAN_POINT ( 'NONE',  ( 168.2356071464602962, 248.8554872198452301, 6.669745218284529820 ) ) ;
#61102 = EDGE_CURVE ( 'NONE', #75897, #91070, #33235, .T. ) ;
#61103 = FACE_OUTER_BOUND ( 'NONE', #100185, .T. ) ;
#61104 = EDGE_LOOP ( 'NONE', ( #97651, #32978, #79110, #60280 ) ) ;
#61105 = CARTESIAN_POINT ( 'NONE',  ( 86.52685127962818967, 47.39493317473652212, -10.85533565734824890 ) ) ;
#61106 = DIRECTION ( 'NONE',  ( 0.9403255362191060840, -0.3402761906661271873, 0.000000000000000000 ) ) ;
#61107 = CARTESIAN_POINT ( 'NONE',  ( 190.5068628727836710, 278.6829438244865855, -16.50779966355658601 ) ) ;
#61108 = CARTESIAN_POINT ( 'NONE',  ( 153.5862473704880244, 264.6278115409098746, -16.56056475222486668 ) ) ;
#61109 = CARTESIAN_POINT ( 'NONE',  ( 200.8665851640556070, 282.7358642834317948, -16.69422397739980823 ) ) ;
#61110 = CARTESIAN_POINT ( 'NONE',  ( 35.97235683590213284, 38.95586893147758190, 7.433330006724141015 ) ) ;
#61111 = FACE_OUTER_BOUND ( 'NONE', #90220, .T. ) ;
#61112 = DIRECTION ( 'NONE',  ( -0.8660254037844380415, -0.5000000000000011102, 0.000000000000000000 ) ) ;
#61114 = ORIENTED_EDGE ( 'NONE', *, *, #9599, .F. ) ;
#61113 =( BOUNDED_CURVE ( )  B_SPLINE_CURVE ( 2, ( #91434, #97532, #5802, #73718, #35205, #35707, #66605, #28101, #58974 ),
 .UNSPECIFIED., .F., .T. ) 
 B_SPLINE_CURVE_WITH_KNOTS ( ( 3, 2, 2, 2, 3 ),
 ( 0.6330645161290322509, 0.6344086021505376261, 0.6370967741935483764, 0.6397849462365591267, 0.6411290322580645018 ),
 .UNSPECIFIED. ) 
 CURVE ( )  GEOMETRIC_REPRESENTATION_ITEM ( )  RATIONAL_B_SPLINE_CURVE ( ( 0.9330127018922194093, 0.9330127018922194093, 1.000000000000000000, 0.8660254037844387076, 1.000000000000000000, 0.8660254037844387076, 1.000000000000000000, 0.9330127018922194093, 0.9330127018922194093 ) ) 
 REPRESENTATION_ITEM ( '' )  );
#61115 = CARTESIAN_POINT ( 'NONE',  ( 196.1831030080164169, 290.3823853032309898, 16.15582348271726332 ) ) ;
#61116 = ORIENTED_EDGE ( 'NONE', *, *, #7740, .T. ) ;
#61117 = VERTEX_POINT ( 'NONE', #23617 ) ;
#61118 = CARTESIAN_POINT ( 'NONE',  ( 198.2391837281077756, 286.3575794386269422, 17.25947343406376078 ) ) ;
#61119 = CARTESIAN_POINT ( 'NONE',  ( 86.86990765421666083, 45.77415147683691288, -8.704208088459520098 ) ) ;
#61120 = CARTESIAN_POINT ( 'NONE',  ( 79.74434664762874547, 56.88260642345687756, 16.21928422613826370 ) ) ;
#61122 = CARTESIAN_POINT ( 'NONE',  ( 164.4811395904728784, 246.2125872648383620, 1.945510398998699042 ) ) ;
#61121 = PLANE ( 'NONE',  #56812 ) ;
#61123 = DIRECTION ( 'NONE',  ( 0.000000000000000000, 0.000000000000000000, 1.000000000000000000 ) ) ;
#61124 = CARTESIAN_POINT ( 'NONE',  ( 197.6875078399188794, 272.6683531706096915, -13.23822772498251155 ) ) ;
#61125 = CARTESIAN_POINT ( 'NONE',  ( 74.80133982707299367, 60.85566197117798026, -15.41540466998751846 ) ) ;
#61126 = CARTESIAN_POINT ( 'NONE',  ( 189.8171280724701546, 301.8740853621098950, -0.4360232994423257624 ) ) ;
#61127 = VECTOR ( 'NONE', #50376, 1000.000000000000114 ) ;
#61128 = CARTESIAN_POINT ( 'NONE',  ( 171.6228816214248809, 250.6675204659138956, -5.726922243694214210 ) ) ;
#61129 = CARTESIAN_POINT ( 'NONE',  ( 76.82578666445662918, 64.07401149769333415, -15.18382690731647600 ) ) ;
#61130 = ADVANCED_FACE ( 'NONE', ( #62619 ), #90274, .F. ) ;
#61131 = CARTESIAN_POINT ( 'NONE',  ( 183.4234925895679567, 284.6666860932168674, -15.01880897167392703 ) ) ;
#61132 = CARTESIAN_POINT ( 'NONE',  ( 110.0524566828198232, 234.3458772461660544, 9.188101187500095079 ) ) ;
#61133 = ORIENTED_EDGE ( 'NONE', *, *, #84637, .T. ) ;
#61134 = CARTESIAN_POINT ( 'NONE',  ( 44.35815684012577265, 67.96982248125696913, -10.00000000000000000 ) ) ;
#61135 = CARTESIAN_POINT ( 'NONE',  ( 38.30580752471379213, 37.51421378149922958, -9.188101187500004485 ) ) ;
#61136 = DIRECTION ( 'NONE',  ( -1.000000000000000000, 0.000000000000000000, 0.000000000000000000 ) ) ;
#61137 = VECTOR ( 'NONE', #11498, 1000.000000000000000 ) ;
#61138 = VERTEX_POINT ( 'NONE', #6801 ) ;
#61139 = VECTOR ( 'NONE', #33582, 1000.000000000000227 ) ;
#61140 = CARTESIAN_POINT ( 'NONE',  ( 73.97927654802940367, 68.30869415006648637, -11.66811813765111516 ) ) ;
#61141 = CARTESIAN_POINT ( 'NONE',  ( 180.2423226582527604, 295.0003840256651415, -2.029293836717157351 ) ) ;
#61142 = CARTESIAN_POINT ( 'NONE',  ( 204.9090237380674182, 269.5176180222230755, 5.449509932175979010 ) ) ;
#61143 = CARTESIAN_POINT ( 'NONE',  ( 190.4356836585210431, 300.3996184492839916, -0.5836641476860114919 ) ) ;
#61144 = ADVANCED_FACE ( 'NONE', ( #86726 ), #37681, .T. ) ;
#61145 = CARTESIAN_POINT ( 'NONE',  ( 47.32807415326522715, 108.5480133836684900, -10.00000000000000000 ) ) ;
#61146 = EDGE_LOOP ( 'NONE', ( #92489, #53049, #45241, #73246 ) ) ;
#61147 = CARTESIAN_POINT ( 'NONE',  ( 148.5647453719543591, 273.3253081326787992, 9.005903527242661966 ) ) ;
#61148 = EDGE_CURVE ( 'NONE', #68725, #63243, #60415, .T. ) ;
#61149 = VECTOR ( 'NONE', #10266, 1000.000000000000000 ) ;
#61150 = ORIENTED_EDGE ( 'NONE', *, *, #79651, .T. ) ;
#61151 = CARTESIAN_POINT ( 'NONE',  ( -19.65312891409030271, 93.06504152958497400, 59.99999999999999289 ) ) ;
#61152 = FACE_OUTER_BOUND ( 'NONE', #49059, .T. ) ;
#61153 = ORIENTED_EDGE ( 'NONE', *, *, #97284, .T. ) ;
#61154 = CARTESIAN_POINT ( 'NONE',  ( 188.3408396332539212, 265.5067415902187804, -11.62187238349581975 ) ) ;
#61155 = AXIS2_PLACEMENT_3D ( 'NONE', #61863, #61373, #31468 ) ;
#61156 = B_SPLINE_CURVE_WITH_KNOTS ( 'NONE', 3,
 ( #68935, #9671, #86205, #61830 ),
 .UNSPECIFIED., .F., .F.,
 ( 4, 4 ),
 ( 0.04659044411497612059, 0.04887120950165271815 ),
 .UNSPECIFIED. ) ;
#61157 = CARTESIAN_POINT ( 'NONE',  ( 195.2523433541918791, 265.1293616091613217, 4.413780863583922631 ) ) ;
#61158 = CARTESIAN_POINT ( 'NONE',  ( 187.9334280069057570, 258.7324837002516347, 0.4517059538649245143 ) ) ;
#61159 = CARTESIAN_POINT ( 'NONE',  ( 202.7865629936218284, 279.4103651332174536, 17.10878160033216133 ) ) ;
#61161 = CARTESIAN_POINT ( 'NONE',  ( 160.7349768583320042, 281.5384896374872596, 5.620271226638340778 ) ) ;
#61160 = CARTESIAN_POINT ( 'NONE',  ( 187.1742838492968986, 290.8334520998986363, -13.54031411274703522 ) ) ;
#61162 = FACE_OUTER_BOUND ( 'NONE', #47653, .T. ) ;
#61163 = ORIENTED_EDGE ( 'NONE', *, *, #74763, .F. ) ;
#61164 = CARTESIAN_POINT ( 'NONE',  ( 147.3023124603499809, 275.5119060767245287, 5.196938859334171212 ) ) ;
#61166 = CARTESIAN_POINT ( 'NONE',  ( 72.77247963031311428, 66.86076665135031760, 11.73453098109765058 ) ) ;
#61165 = B_SPLINE_SURFACE_WITH_KNOTS ( 'NONE', 3, 1, ( 
 ( #62147, #76393 ),
 ( #30269, #15548 ),
 ( #61159, #57558 ),
 ( #64681, #88039 ),
 ( #48979, #47952 ),
 ( #72297, #33797 ),
 ( #72808, #80421 ),
 ( #18588, #79419 ),
 ( #26179, #64172 ),
 ( #94607, #65166 ),
 ( #95631, #49466 ),
 ( #41866, #17570 ),
 ( #19096, #3397 ),
 ( #34272, #71288 ),
 ( #48477, #1881 ),
 ( #40845, #33269 ),
 ( #25162, #95120 ),
 ( #96618, #11500 ),
 ( #3876, #9480 ),
 ( #63668, #41355 ),
 ( #57057, #56565 ),
 ( #78895, #40351 ),
 ( #79916, #2904 ),
 ( #17061, #56045 ),
 ( #10994, #26672 ),
 ( #32762, #87037 ),
 ( #88534, #96118 ),
 ( #49974, #80931 ),
 ( #42352, #9985 ),
 ( #71791, #2389 ),
 ( #73283, #10478 ),
 ( #25685, #87551 ),
 ( #18084, #55547 ),
 ( #65659, #34759 ) ),
 .UNSPECIFIED., .T., .F., .F.,
 ( 4, 2, 2, 2, 2, 2, 2, 2, 2, 2, 2, 2, 2, 2, 2, 2, 4 ),
 ( 2, 2 ),
 ( 0.000000000000000000, 0.06250000000000000000, 0.1250000000000000000, 0.1875000000000000000, 0.2500000000000000000, 0.3125000000000000000, 0.3750000000000000000, 0.4375000000000000000, 0.5000000000000000000, 0.5625000000000000000, 0.6250000000000000000, 0.6875000000000000000, 0.7500000000000000000, 0.8125000000000000000, 0.8750000000000000000, 0.9375000000000000000, 1.000000000000000000 ),
 ( 0.000000000000000000, 1.000000000000000000 ),
 .UNSPECIFIED. ) ;
#61167 = CARTESIAN_POINT ( 'NONE',  ( 82.31724296769202454, 41.27996126847105529, -3.439593570527449629 ) ) ;
#61168 = LINE ( 'NONE', #84520, #51320 ) ;
#61169 = CARTESIAN_POINT ( 'NONE',  ( 192.3395334592007941, 271.2003706416659838, -15.16840763204049658 ) ) ;
#61170 = CARTESIAN_POINT ( 'NONE',  ( 172.2467550100553808, 258.4300157609564508, -14.58559033337875377 ) ) ;
#61171 = CARTESIAN_POINT ( 'NONE',  ( -19.65312891409030271, 93.06504152958497400, 177.5919119679930134 ) ) ;
#61172 = DIRECTION ( 'NONE',  ( 0.9263643838751153270, 0.3766285016932175433, 0.000000000000000000 ) ) ;
#61173 = CARTESIAN_POINT ( 'NONE',  ( 194.4904290197884507, 293.7796906822950973, 14.50206953321744940 ) ) ;
#61174 = CARTESIAN_POINT ( 'NONE',  ( 33.86928444543146810, 180.3615022471902023, 5.000000000000051514 ) ) ;
#61175 = VECTOR ( 'NONE', #48238, 1000.000000000000114 ) ;
#61176 = EDGE_CURVE ( 'NONE', #70394, #17777, #26872, .T. ) ;
#61177 = CARTESIAN_POINT ( 'NONE',  ( 82.54140815357128247, 53.47864718817667296, -15.73643156343348259 ) ) ;
#61178 = CARTESIAN_POINT ( 'NONE',  ( 74.03095222233704931, 222.7369531367911293, -4.594050593750048428 ) ) ;
#61179 = CARTESIAN_POINT ( 'NONE',  ( 206.3423291502491566, 273.2515974901050413, -10.76717883871977577 ) ) ;
#61180 = CARTESIAN_POINT ( 'NONE',  ( 192.6247335881259630, 297.0111699613833594, -13.30158778996737290 ) ) ;
#61181 = CARTESIAN_POINT ( 'NONE',  ( 163.4222916751007801, 247.5912830598222172, -10.52132777929285012 ) ) ;
#61182 = CARTESIAN_POINT ( 'NONE',  ( 66.45995819386082815, 67.97305414892089459, 6.490190279896535408 ) ) ;
#61183 = CARTESIAN_POINT ( 'NONE',  ( 207.8570869662935365, 270.6279599915536664, -5.669188455878507504 ) ) ;
#61184 = DIRECTION ( 'NONE',  ( -0.000000000000000000, -0.000000000000000000, -1.000000000000000000 ) ) ;
#61186 = CARTESIAN_POINT ( 'NONE',  ( 76.41050813019120369, 51.44656437704933438, 15.62581973270596514 ) ) ;
#61185 = CARTESIAN_POINT ( 'NONE',  ( 73.42123007364070020, 69.75766128465485849, -9.876216450746401421 ) ) ;
#61187 = CARTESIAN_POINT ( 'NONE',  ( 191.4155626767636704, 260.8708449615334075, 2.063941295486333427 ) ) ;
#61188 = CARTESIAN_POINT ( 'NONE',  ( 45.27367124825920541, 27.10801979619933277, 3.090169943749476733 ) ) ;
#61189 = CARTESIAN_POINT ( 'NONE',  ( 205.3054132066514796, 275.0475885875939639, -12.25171873544422141 ) ) ;
#61190 = CARTESIAN_POINT ( 'NONE',  ( 157.8740713127050981, 257.2010826190796706, 17.31862062017425075 ) ) ;
#61191 = CARTESIAN_POINT ( 'NONE',  ( 72.14978007694548978, 72.25075206688683238, 3.885827817524740713 ) ) ;
#61192 = CARTESIAN_POINT ( 'NONE',  ( 33.19304919271588972, 177.7202760586659736, -5.415160957724236172E-17 ) ) ;
#61193 = VECTOR ( 'NONE', #77102, 1000.000000000000114 ) ;
#61194 = CARTESIAN_POINT ( 'NONE',  ( 44.66719160132967659, 208.8464784336661353, 1.353441290958777327E-15 ) ) ;
#61195 = CARTESIAN_POINT ( 'NONE',  ( 157.8562613713738472, 257.2319303423452652, 17.81420683562559404 ) ) ;
#61196 = CARTESIAN_POINT ( 'NONE',  ( 81.64670023727850889, 42.65128533460878657, -7.584980231169042852 ) ) ;
#61197 = VECTOR ( 'NONE', #8153, 1000.000000000000000 ) ;
#61198 = CARTESIAN_POINT ( 'NONE',  ( 80.02673061647857367, 50.59600265380255024, -14.77882822326097845 ) ) ;
#61199 = CARTESIAN_POINT ( 'NONE',  ( 142.5284093247362591, 253.0958772461660544, -9.188101187500095079 ) ) ;
#61200 = CARTESIAN_POINT ( 'NONE',  ( 52.62397354648171444, 207.3149278399161233, 9.188101187500093303 ) ) ;
#61202 = EDGE_CURVE ( 'NONE', #41077, #34164, #24196, .T. ) ;
#61201 = AXIS2_PLACEMENT_3D ( 'NONE', #93876, #62408, #54819 ) ;
#61203 = CARTESIAN_POINT ( 'NONE',  ( 23.51121325743158508, 19.28920272979927120, -7.433330006724141015 ) ) ;
#61204 = CARTESIAN_POINT ( 'NONE',  ( -12.96825614257699399, 169.9865022471903160, 10.00000000000009415 ) ) ;
#61205 = CARTESIAN_POINT ( 'NONE',  ( 149.7072529793668707, 271.3464269086063041, -11.98883662638834657 ) ) ;
#61206 = CARTESIAN_POINT ( 'NONE',  ( 14.61458989734527947, 10.29860640527290805, -2.839279412974138328 ) ) ;
#61207 = CARTESIAN_POINT ( 'NONE',  ( 205.0520875136525376, 275.4863615587311756, -14.16385635411862509 ) ) ;
#61208 = CARTESIAN_POINT ( 'NONE',  ( 77.27782791576461818, 63.42193016440150899, 15.51014190020122641 ) ) ;
#61209 = CARTESIAN_POINT ( 'NONE',  ( 76.57849375015202043, 63.06061772104433771, 15.49930747022867195 ) ) ;
#61210 = AXIS2_PLACEMENT_3D ( 'NONE', #37842, #851, #39330 ) ;
#61211 = CARTESIAN_POINT ( 'NONE',  ( 198.1300353965528984, 287.4757075181870505, 18.48278456664528946 ) ) ;
#61212 = CARTESIAN_POINT ( 'NONE',  ( 72.67360971685785387, 61.67685437178258212, 14.68373298776349856 ) ) ;
#61213 = CARTESIAN_POINT ( 'NONE',  ( 153.3133634134964609, 265.1004604189892575, 17.35325068284992867 ) ) ;
#61214 = CARTESIAN_POINT ( 'NONE',  ( 77.35066759761136268, 56.08440499094516696, -16.16557419915228166 ) ) ;
#61216 = CARTESIAN_POINT ( 'NONE',  ( 87.77948443791279942, 45.22530890134208903, -6.970560438077714416 ) ) ;
#61215 = VECTOR ( 'NONE', #86502, 1000.000000000000000 ) ;
#61217 = CARTESIAN_POINT ( 'NONE',  ( 104.4503548538631463, 241.1115022471902876, -5.000000000000047962 ) ) ;
#61218 = CYLINDRICAL_SURFACE ( 'NONE', #39327, 10.00000000000010658 ) ;
#61219 = CARTESIAN_POINT ( 'NONE',  ( 193.3529349556220325, 284.7064891731757825, -16.83000617485832962 ) ) ;
#61220 = ORIENTED_EDGE ( 'NONE', *, *, #77788, .F. ) ;
#61221 = CARTESIAN_POINT ( 'NONE',  ( 76.92172728274191229, 49.74558783373824156, 15.08244268300244784 ) ) ;
#61222 = VERTEX_POINT ( 'NONE', #58253 ) ;
#61223 = CARTESIAN_POINT ( 'NONE',  ( 206.0870578475358172, 273.6937403561189512, -10.07771901274806581 ) ) ;
#61224 = CARTESIAN_POINT ( 'NONE',  ( 190.1526130375667094, 278.5908336017399165, -16.50440980714951777 ) ) ;
#61225 = CARTESIAN_POINT ( 'NONE',  ( 192.3713340522295709, 271.8780416168410170, 15.57788208939756380 ) ) ;
#61226 = ORIENTED_EDGE ( 'NONE', *, *, #86339, .T. ) ;
#61227 = CARTESIAN_POINT ( 'NONE',  ( 79.09449567167088446, 45.94901772720934474, -12.57695653887258480 ) ) ;
#61228 = CARTESIAN_POINT ( 'NONE',  ( 194.8708600166808651, 293.1207648669033006, -14.79199694356877970 ) ) ;
#61229 = CARTESIAN_POINT ( 'NONE',  ( 175.7622132985686392, 274.0430017844784629, -17.75579533532145504 ) ) ;
#61230 = DIRECTION ( 'NONE',  ( 1.000000000000000000, 0.000000000000000000, 0.000000000000000000 ) ) ;
#61231 = VERTEX_POINT ( 'NONE', #81603 ) ;
#61232 = CARTESIAN_POINT ( 'NONE',  ( 15.27916758686040311, 29.79752408145592568, -5.678558825948271327 ) ) ;
#61233 = CARTESIAN_POINT ( 'NONE',  ( 75.19925724589786853, 55.75564056399659307, 16.15125504434804782 ) ) ;
#61234 = CARTESIAN_POINT ( 'NONE',  ( 172.4831635826484444, 290.8796410925290843, -1.652085212636280609 ) ) ;
#61235 = DIRECTION ( 'NONE',  ( -0.8660254037844387076, -0.4999999999999998890, -0.000000000000000000 ) ) ;
#61236 = ORIENTED_EDGE ( 'NONE', *, *, #50440, .T. ) ;
#61237 = CARTESIAN_POINT ( 'NONE',  ( 198.4160757083882345, 267.1808215963346242, -8.346050686629251203 ) ) ;
#61238 = LINE ( 'NONE', #55626, #62656 ) ;
#61239 = VERTEX_POINT ( 'NONE', #48682 ) ;
#61240 = CARTESIAN_POINT ( 'NONE',  ( 174.7533417775181306, 286.2318505546784877, 11.43544241327690258 ) ) ;
#61242 = CARTESIAN_POINT ( 'NONE',  ( 68.13485488127290068, 65.64062842649776996, -10.28058960440808534 ) ) ;
#61241 = CARTESIAN_POINT ( 'NONE',  ( 159.9924463476198753, 283.3850188831759169, -3.371971149216307140 ) ) ;
#61243 = CARTESIAN_POINT ( 'NONE',  ( 162.6541320028305506, 248.9217746405196294, -10.16950121496441817 ) ) ;
#61244 = CARTESIAN_POINT ( 'NONE',  ( 204.5831314780710954, 276.2986172388744421, 13.28075685133257089 ) ) ;
#61245 = CARTESIAN_POINT ( 'NONE',  ( 188.6535065314160704, 295.1378203055187441, -11.17103305312315520 ) ) ;
#61246 = CARTESIAN_POINT ( 'NONE',  ( 161.0164413264604661, 262.9588007402923040, -17.56398238099813014 ) ) ;
#61247 = CARTESIAN_POINT ( 'NONE',  ( 129.8627877943888791, 245.7833772461660544, -9.188101187500095079 ) ) ;
#61248 = CARTESIAN_POINT ( 'NONE',  ( 202.9785155578410354, 267.9986174989653591, 2.523388936575725161 ) ) ;
#61249 = CARTESIAN_POINT ( 'NONE',  ( 195.6979370051232934, 290.6267181618097766, -16.31163916660881341 ) ) ;
#61250 = CARTESIAN_POINT ( 'NONE',  ( 67.72511797709034909, 222.1589784336661637, -6.496448406907675876E-16 ) ) ;
#61251 = ORIENTED_EDGE ( 'NONE', *, *, #26198, .T. ) ;
#61252 = PLANE ( 'NONE',  #47828 ) ;
#61253 = DIRECTION ( 'NONE',  ( -0.000000000000000000, -0.000000000000000000, -1.000000000000000000 ) ) ;
#61254 = VECTOR ( 'NONE', #48755, 1000.000000000000000 ) ;
#61255 = ORIENTED_EDGE ( 'NONE', *, *, #9088, .T. ) ;
#61256 = DIRECTION ( 'NONE',  ( 0.5280678506503729830, 0.8492021815265757834, 0.000000000000000000 ) ) ;
#61257 = ORIENTED_EDGE ( 'NONE', *, *, #86975, .T. ) ;
#61258 = FACE_BOUND ( 'NONE', #34579, .T. ) ;
#61259 = CARTESIAN_POINT ( 'NONE',  ( 67.08790609839790875, 67.65794649167050068, 6.640929181028614181 ) ) ;
#61260 = CARTESIAN_POINT ( 'NONE',  ( 194.2695434292520247, 284.8040030035346604, 17.71845281746924883 ) ) ;
#61261 = CARTESIAN_POINT ( 'NONE',  ( -32.46101061832366952, 95.98221459296189551, 11.49967512814420445 ) ) ;
#61262 = CARTESIAN_POINT ( 'NONE',  ( 81.18434463996317163, 55.62183548715842107, 16.37412944077603782 ) ) ;
#61263 = CARTESIAN_POINT ( 'NONE',  ( 155.6559071247401960, 261.0430556921643870, 17.79853447468815375 ) ) ;
#61264 = ADVANCED_FACE ( 'NONE', ( #73976 ), #50164, .T. ) ;
#61265 = CARTESIAN_POINT ( 'NONE',  ( 70.57311072637669724, 64.37600167932460238, 12.58562827297202347 ) ) ;
#61266 = CARTESIAN_POINT ( 'NONE',  ( 76.60222546164588664, 215.0333772461660544, 9.188101187500095079 ) ) ;
#61267 = EDGE_LOOP ( 'NONE', ( #28985, #4443, #30115, #77751 ) ) ;
#61268 = EDGE_CURVE ( 'NONE', #32407, #38046, #2587, .T. ) ;
#61270 = ADVANCED_FACE ( 'NONE', ( #64877 ), #97294, .T. ) ;
#61269 = CARTESIAN_POINT ( 'NONE',  ( 161.6539040693529046, 250.6542202404525312, -12.66790845110597807 ) ) ;
#61271 = EDGE_LOOP ( 'NONE', ( #46331, #29152, #83387, #43815 ) ) ;
#61272 = CARTESIAN_POINT ( 'NONE',  ( 76.09263634981390112, 51.44000213080718709, -15.66469206649365198 ) ) ;
#61273 = EDGE_CURVE ( 'NONE', #94177, #52768, #4839, .T. ) ;
#61274 = VECTOR ( 'NONE', #38165, 1000.000000000000000 ) ;
#61275 = B_SPLINE_CURVE_WITH_KNOTS ( 'NONE', 3,
 ( #3794, #11413, #65082, #89437, #43262, #74707, #58465, #57468, #13392, #19992, #80843, #19010, #81821, #4797, #12396, #88451 ),
 .UNSPECIFIED., .F., .F.,
 ( 4, 1, 2, 2, 2, 1, 2, 2, 4 ),
 ( 0.000000000000000000, 0.1250000000000012768, 0.1875000000000005829, 0.2499999999999998890, 0.4999999999999976685, 0.6249999999999978906, 0.6874999999999987788, 0.7499999999999996669, 1.000000000000000000 ),
 .UNSPECIFIED. ) ;
#61276 = B_SPLINE_CURVE_WITH_KNOTS ( 'NONE', 3,
 ( #40538, #55721, #92783, #23337 ),
 .UNSPECIFIED., .F., .F.,
 ( 4, 4 ),
 ( 0.04233433915237033024, 0.04887066958154941132 ),
 .UNSPECIFIED. ) ;
#61277 = CARTESIAN_POINT ( 'NONE',  ( 75.80192922086310148, 65.84738460970490337, -14.09986028324621898 ) ) ;
#61278 = VECTOR ( 'NONE', #38472, 1000.000000000000000 ) ;
#61279 = CARTESIAN_POINT ( 'NONE',  ( 164.3493441216711517, 245.9855811210807417, 1.722120810491653664 ) ) ;
#61280 = CARTESIAN_POINT ( 'NONE',  ( 161.5504232052330167, 284.0438539892405743, 0.5273125768649428169 ) ) ;
#61281 = CARTESIAN_POINT ( 'NONE',  ( 198.1297952544482541, 280.7479725296748825, 16.71566180775300481 ) ) ;
#61282 = CARTESIAN_POINT ( 'NONE',  ( 147.4771028564622100, 275.6046161191591182, 9.141179566768406735E-14 ) ) ;
#61283 = VECTOR ( 'NONE', #21759, 1000.000000000000114 ) ;
#61284 = VERTEX_POINT ( 'NONE', #41554 ) ;
#61285 = CARTESIAN_POINT ( 'NONE',  ( 87.73298548431468191, 44.18903561216112763, 4.633618514853090176 ) ) ;
#61286 = CARTESIAN_POINT ( 'NONE',  ( 185.3162954522941561, 260.2450069084709412, 6.201801027297742408 ) ) ;
#61287 = CARTESIAN_POINT ( 'NONE',  ( 88.07576543976308869, 43.78748546321877910, -2.154750241475199335 ) ) ;
#61288 = CARTESIAN_POINT ( 'NONE',  ( 201.4066285247549786, 281.8004817444100354, -17.79749223817309201 ) ) ;
#61289 = CARTESIAN_POINT ( 'NONE',  ( 79.51501685758188387, 59.30344737611886075, -16.21767406144808987 ) ) ;
#61290 = CARTESIAN_POINT ( 'NONE',  ( 72.78409883976615902, 66.98531790838794109, -11.66862470457359002 ) ) ;
#61291 = ORIENTED_EDGE ( 'NONE', *, *, #78890, .T. ) ;
#61292 = CARTESIAN_POINT ( 'NONE',  ( 195.7397332151493003, 265.3334278097593710, 5.020291378112107239 ) ) ;
#61293 = AXIS2_PLACEMENT_3D ( 'NONE', #78210, #33607, #26014 ) ;
#61294 = CARTESIAN_POINT ( 'NONE',  ( 87.73782093965644435, 209.9155109091896065, 2.679491924311254714 ) ) ;
#61295 = CARTESIAN_POINT ( 'NONE',  ( 82.11473172643496810, 40.78303678057567083, 1.182234453112787298 ) ) ;
#61296 = CARTESIAN_POINT ( 'NONE',  ( 79.56975053609437509, 46.55862065107593395, 12.80488734779169846 ) ) ;
#61297 = CARTESIAN_POINT ( 'NONE',  ( 83.29275869314055569, 52.39031112279613467, 14.85814565312617397 ) ) ;
#61298 = CARTESIAN_POINT ( 'NONE',  ( 198.5033866919546881, 266.2084897167371196, 0.6426914612636319690 ) ) ;
#61299 = ORIENTED_EDGE ( 'NONE', *, *, #14221, .F. ) ;
#61300 = CARTESIAN_POINT ( 'NONE',  ( 147.4368675721658519, 275.2788497866417288, 5.050119523016719292 ) ) ;
#61301 = CARTESIAN_POINT ( 'NONE',  ( 183.7271510445999070, 281.0151571664360404, 16.38277545986319694 ) ) ;
#61302 = AXIS2_PLACEMENT_3D ( 'NONE', #16228, #39497, #69913 ) ;
#61303 = CARTESIAN_POINT ( 'NONE',  ( 206.9377610035629118, 272.2202792677204002, 7.440532334334675646 ) ) ;
#61305 = CARTESIAN_POINT ( 'NONE',  ( 81.74119788692269140, 59.14441083166271795, 0.000000000000000000 ) ) ;
#61304 = CARTESIAN_POINT ( 'NONE',  ( 155.2419697281468416, 261.7600162942170527, 18.58580762350309357 ) ) ;
#61306 = CARTESIAN_POINT ( 'NONE',  ( 26.39431744575845684, 16.20801979619929156, -3.090169943749474069 ) ) ;
#61307 = CARTESIAN_POINT ( 'NONE',  ( 19.85049821812286908, 192.2677522451419350, -5.000000000000047962 ) ) ;
#61308 = CARTESIAN_POINT ( 'NONE',  ( 163.6469966371277849, 283.9424131525427697, -3.116750258215220448 ) ) ;
#61309 = CARTESIAN_POINT ( 'NONE',  ( 48.77433535142598231, 99.76555324011610537, -10.00000000000000000 ) ) ;
#61310 = CARTESIAN_POINT ( 'NONE',  ( 198.2414483977475754, 287.2827345394944700, 16.94931984969033678 ) ) ;
#61311 = CARTESIAN_POINT ( 'NONE',  ( 141.9600801517287323, 262.7677522451419350, -5.000000000000047962 ) ) ;
#61312 = CARTESIAN_POINT ( 'NONE',  ( -57.77801984846012573, 31.16909059156539996, 59.99999999999999289 ) ) ;
#61313 = ORIENTED_EDGE ( 'NONE', *, *, #53586, .F. ) ;
#61314 = DIRECTION ( 'NONE',  ( 0.8660254037844379305, 0.5000000000000014433, 0.000000000000000000 ) ) ;
#61315 = CARTESIAN_POINT ( 'NONE',  ( 72.62340041749850172, 70.70648146094342223, -7.965908336710425530 ) ) ;
#61316 = CARTESIAN_POINT ( 'NONE',  ( 81.85549098805211088, 41.30720913978863962, 5.950207739220628511 ) ) ;
#61317 = CARTESIAN_POINT ( 'NONE',  ( 17.27983239817682559, 168.5327760586659451, 1.948934522072302763E-15 ) ) ;
#61318 = EDGE_CURVE ( 'NONE', #31684, #71618, #35458, .T. ) ;
#61319 = CARTESIAN_POINT ( 'NONE',  ( 178.5822171558442619, 273.7261340967344836, -16.93785058890262007 ) ) ;
#61320 = CARTESIAN_POINT ( 'NONE',  ( 33.69734285410222441, 21.58380873178789017, 6.180339887498953466 ) ) ;
#61321 = CARTESIAN_POINT ( 'NONE',  ( 130.8844835975280887, 234.8262482093457493, 3.021315404115420679E-15 ) ) ;
#61322 = CARTESIAN_POINT ( 'NONE',  ( 182.1439385020048860, 290.0253507885926183, 13.01467259685074573 ) ) ;
#61323 = DIRECTION ( 'NONE',  ( 0.5000000000000048850, -0.8660254037844358210, 0.000000000000000000 ) ) ;
#61324 = CARTESIAN_POINT ( 'NONE',  ( 187.4995632756286739, 259.3762926903145285, -0.7801709818681489272 ) ) ;
#61325 = CARTESIAN_POINT ( 'NONE',  ( 183.1000404951680878, 295.7276604254721519, 1.087596103637166189 ) ) ;
#61326 = CARTESIAN_POINT ( 'NONE',  ( 65.91222438545561602, 218.8615022471903160, 5.000000000000046185 ) ) ;
#61327 = CARTESIAN_POINT ( 'NONE',  ( 82.31762945370437023, 41.36718402847516529, 5.460911063167284141 ) ) ;
#61328 = CARTESIAN_POINT ( 'NONE',  ( 148.2267527339363369, 273.9107285543102535, 7.913369084260907016 ) ) ;
#61329 = VECTOR ( 'NONE', #16369, 1000.000000000000000 ) ;
#61330 = CARTESIAN_POINT ( 'NONE',  ( 32.89474554257621719, 198.9869531367911293, 4.594050593750046652 ) ) ;
#61331 = CARTESIAN_POINT ( 'NONE',  ( 72.49337063691619676, 70.67504402769608873, -7.896386945446496775 ) ) ;
#61332 = ADVANCED_FACE ( 'NONE', ( #66361 ), #27370, .F. ) ;
#61333 = SURFACE_STYLE_FILL_AREA ( #93789 ) ;
#61334 = CARTESIAN_POINT ( 'NONE',  ( 42.70206918026080700, 25.44966523072497822, -2.296566073217252530E-15 ) ) ;
#61335 = CARTESIAN_POINT ( 'NONE',  ( 89.18655626861060171, 155.9036630683315821, 0.000000000000000000 ) ) ;
#61337 = CARTESIAN_POINT ( 'NONE',  ( 164.4440639631384045, 245.8215215431751233, -2.910115319305802029 ) ) ;
#61336 = AXIS2_PLACEMENT_3D ( 'NONE', #6575, #83605, #58870 ) ;
#61338 = CARTESIAN_POINT ( 'NONE',  ( 188.8123461939931076, 268.1836859051376223, 13.59473602984847140 ) ) ;
#61339 = CARTESIAN_POINT ( 'NONE',  ( 202.8965239598698247, 278.6747210883311823, -15.08919433053647374 ) ) ;
#61340 = CARTESIAN_POINT ( 'NONE',  ( 161.2976129585435956, 280.2619845096857034, 9.013726905557600588 ) ) ;
#61341 = APPLICATION_PROTOCOL_DEFINITION ( 'draft international standard', 'automotive_design', 1998, #33745 ) ;
#61342 = CARTESIAN_POINT ( 'NONE',  ( 14.90450122504689823, 30.64646525600389637, -2.839279412974133887 ) ) ;
#61343 = CARTESIAN_POINT ( 'NONE',  ( 148.3707431749605234, 273.6613297946520902, 8.912574527564540716 ) ) ;
#61344 = CARTESIAN_POINT ( 'NONE',  ( 72.03620616349491002, 59.26415205210582826, 15.35034427320005079 ) ) ;
#61345 = CARTESIAN_POINT ( 'NONE',  ( 155.2098048002210930, 261.8157275836062468, 16.98811268941991059 ) ) ;
#61346 = ORIENTED_EDGE ( 'NONE', *, *, #45048, .F. ) ;
#61347 = AXIS2_PLACEMENT_3D ( 'NONE', #50956, #35265, #27684 ) ;
#61348 = CARTESIAN_POINT ( 'NONE',  ( 43.71482552144721723, 26.20801979619932354, -3.090169943749474069 ) ) ;
#61349 = FACE_OUTER_BOUND ( 'NONE', #13472, .T. ) ;
#61350 = B_SPLINE_CURVE_WITH_KNOTS ( 'NONE', 3,
 ( #41203, #56909, #72143, #64023, #1743, #26039, #63520, #64529, #2243, #79772, #94459, #33122, #15915, #9849, #95487, #46821, #77744, #70107, #716, #24016, #80780, #57409, #80269, #34616, #5221, #19934, #11838, #26536, #20431, #89380, #66515, #74645, #42697, #67002, #27537, #97440, #88390, #18944, #49822, #19457, #88895, #28010, #12331, #58406 ),
 .UNSPECIFIED., .F., .F.,
 ( 4, 2, 2, 2, 2, 2, 2, 2, 2, 2, 2, 2, 2, 2, 2, 2, 2, 2, 2, 2, 2, 4 ),
 ( 0.001113145019558975379, 0.001593043127414757280, 0.002072941235270539181, 0.002312890289198457454, 0.002552839343126374859, 0.002672813870090334429, 0.002792788397054293131, 0.002912762924018251834, 0.003032737450982210536, 0.003512635558838129047, 0.003992533666694047557, 0.004952329882406020754, 0.005912126098117993951, 0.006392024205973977947, 0.006871922313829961944, 0.006991896840793983096, 0.007051884104275961580, 0.007111871367757939197, 0.007351820421685926858, 0.007831718529541909987, 0.008311616637397895718, 0.008791514745253877980 ),
 .UNSPECIFIED. ) ;
#61351 = CARTESIAN_POINT ( 'NONE',  ( 75.34249057394406179, 53.53749946893489664, -16.04535326226222480 ) ) ;
#61352 = CARTESIAN_POINT ( 'NONE',  ( 148.6890168490380688, 273.7113373112761678, -8.655580785000621447 ) ) ;
#61353 = CARTESIAN_POINT ( 'NONE',  ( 81.52647152047666168, 42.51558550804076475, 7.474308617801350252 ) ) ;
#61354 = ORIENTED_EDGE ( 'NONE', *, *, #80820, .F. ) ;
#61355 = CARTESIAN_POINT ( 'NONE',  ( -10.80656490723494123, 24.88181024604954672, -10.00000000000000000 ) ) ;
#61356 = CARTESIAN_POINT ( 'NONE',  ( 72.63327417104410699, 71.45201850668806287, -5.742053798226967487 ) ) ;
#61357 = FACE_OUTER_BOUND ( 'NONE', #100269, .T. ) ;
#61358 = CARTESIAN_POINT ( 'NONE',  ( 181.2250113611592042, 257.6047676075520485, -7.592445647342843884 ) ) ;
#61359 = ORIENTED_EDGE ( 'NONE', *, *, #74536, .F. ) ;
#61360 = AXIS2_PLACEMENT_3D ( 'NONE', #7055, #28361, #29862 ) ;
#61361 = ORIENTED_EDGE ( 'NONE', *, *, #17958, .T. ) ;
#61363 = SURFACE_SIDE_STYLE ('',( #86731 ) ) ;
#61362 = CARTESIAN_POINT ( 'NONE',  ( 202.4568751826897426, 279.4272769738290094, 15.52666735877811455 ) ) ;
#61364 = ORIENTED_EDGE ( 'NONE', *, *, #40977, .T. ) ;
#61365 = CARTESIAN_POINT ( 'NONE',  ( 151.4361976351029000, 268.3518069213970421, 15.15218985681980612 ) ) ;
#61366 = DIRECTION ( 'NONE',  ( 0.4999999999999998890, -0.8660254037844385966, 0.000000000000000000 ) ) ;
#61367 = CARTESIAN_POINT ( 'NONE',  ( -30.18034446749236821, 25.12100238203590763, -10.00000000000000000 ) ) ;
#61368 = ORIENTED_EDGE ( 'NONE', *, *, #47988, .T. ) ;
#61369 = CARTESIAN_POINT ( 'NONE',  ( 148.3707431749605234, 273.6613297946520902, 8.912574527564540716 ) ) ;
#61370 = VECTOR ( 'NONE', #93276, 1000.000000000000000 ) ;
#61371 = CARTESIAN_POINT ( 'NONE',  ( 176.0994133278866229, 271.7662213919938381, 17.81274505597714253 ) ) ;
#61372 = VERTEX_POINT ( 'NONE', #26376 ) ;
#61373 = DIRECTION ( 'NONE',  ( -0.8660254037844379305, -0.5000000000000014433, -0.000000000000000000 ) ) ;
#61374 = DIRECTION ( 'NONE',  ( -0.000000000000000000, -0.000000000000000000, -1.000000000000000000 ) ) ;
#61375 = ORIENTED_EDGE ( 'NONE', *, *, #5206, .T. ) ;
#61376 = ADVANCED_FACE ( 'NONE', ( #27861 ), #11683, .F. ) ;
#61377 = CARTESIAN_POINT ( 'NONE',  ( 166.7959447105422157, 276.3626885415273478, 15.91653206054683523 ) ) ;
#61378 = CARTESIAN_POINT ( 'NONE',  ( 78.13699514187493378, 47.68854696100831347, -13.93943695986319931 ) ) ;
#61379 = ORIENTED_EDGE ( 'NONE', *, *, #46720, .T. ) ;
#61380 = CARTESIAN_POINT ( 'NONE',  ( 172.4419760422836134, 290.9306500000749907, -0.6531725299933459628 ) ) ;
#61381 = CARTESIAN_POINT ( 'NONE',  ( 150.6453220160077251, 269.7216436761371483, 14.94145576020818034 ) ) ;
#61382 = CARTESIAN_POINT ( 'NONE',  ( 29.30989995549245464, 44.80713248141895377, 10.00000000000000000 ) ) ;
#61383 = CARTESIAN_POINT ( 'NONE',  ( 83.21184101803882527, 52.33542056097268613, 14.85481608591265967 ) ) ;
#61384 = VERTEX_POINT ( 'NONE', #73477 ) ;
#61385 = ORIENTED_EDGE ( 'NONE', *, *, #87882, .F. ) ;
#61386 = CARTESIAN_POINT ( 'NONE',  ( 190.5586441464129450, 299.4817191808413668, 6.393230458720348786 ) ) ;
#61387 = LINE ( 'NONE', #38075, #42816 ) ;
#61388 = CARTESIAN_POINT ( 'NONE',  ( 148.3930300673291640, 273.6227277647267897, 8.375036249079425232 ) ) ;
#61389 = CARTESIAN_POINT ( 'NONE',  ( 190.2318383114841254, 301.1557861577188078, 3.177919994438449525 ) ) ;
#61390 = CARTESIAN_POINT ( 'NONE',  ( 141.3928138467258009, 240.8932355074535678, -2.679491924311248496 ) ) ;
#61391 = EDGE_CURVE ( 'NONE', #18565, #21768, #4060, .T. ) ;
#61392 = CARTESIAN_POINT ( 'NONE',  ( 191.6444038793167977, 298.7091508252102017, 8.370770059625519011 ) ) ;
#61393 = EDGE_CURVE ( 'NONE', #52271, #46169, #51667, .T. ) ;
#61394 = CARTESIAN_POINT ( 'NONE',  ( 191.2211340522693774, 299.4422756709672626, -8.405362570633277741 ) ) ;
#61396 = CARTESIAN_POINT ( 'NONE',  ( 162.3596268837808907, 257.1951048930611705, 15.63890487423926601 ) ) ;
#61395 = B_SPLINE_CURVE_WITH_KNOTS ( 'NONE', 3,
 ( #30561, #36650, #37640, #99476 ),
 .UNSPECIFIED., .F., .F.,
 ( 4, 4 ),
 ( 0.01120786676255014318, 0.01708091092720957077 ),
 .UNSPECIFIED. ) ;
#61397 = CARTESIAN_POINT ( 'NONE',  ( 71.77039740172594406, 70.92856646297812517, 5.774134966689192794 ) ) ;
#61398 = CARTESIAN_POINT ( 'NONE',  ( 67.09442320589272413, 69.80147035112786114, 1.451480095758326039 ) ) ;
#61399 = CARTESIAN_POINT ( 'NONE',  ( 67.15803325889245912, 66.63036032015114074, 8.397731182079862577 ) ) ;
#61400 = CARTESIAN_POINT ( 'NONE',  ( 169.8554095453154105, 287.3059200333181025, 4.097349522332975447 ) ) ;
#61401 = CARTESIAN_POINT ( 'NONE',  ( 78.64589612872744340, 47.50488844158302015, 14.24760414073640646 ) ) ;
#61402 = ORIENTED_EDGE ( 'NONE', *, *, #98372, .F. ) ;
#61403 = CARTESIAN_POINT ( 'NONE',  ( 149.6625482771057420, 271.4238577242598467, -11.76596961571646460 ) ) ;
#61404 = CARTESIAN_POINT ( 'NONE',  ( 81.75096066047075283, 229.5530062829863027, -4.648177544792955347E-16 ) ) ;
#61405 = CARTESIAN_POINT ( 'NONE',  ( -27.42236680055714260, 166.5217562850347406, 1.224646799147364892E-15 ) ) ;
#61406 = CARTESIAN_POINT ( 'NONE',  ( 79.41534452234611763, 46.24203507740502772, 12.64746779647137487 ) ) ;
#61407 = CARTESIAN_POINT ( 'NONE',  ( 81.84288204769163144, 58.96828869888589253, -0.4567727288213002668 ) ) ;
#61408 = CARTESIAN_POINT ( 'NONE',  ( 72.84093999290328725, 56.97456911652175648, -16.40692799624908815 ) ) ;
#61409 = CARTESIAN_POINT ( 'NONE',  ( 68.10039974585599509, 65.18542567973287305, -10.72853162865224519 ) ) ;
#61410 = VERTEX_POINT ( 'NONE', #13180 ) ;
#61411 = CARTESIAN_POINT ( 'NONE',  ( 208.3194307158603067, 269.8271571267425770, -2.120200867047394855 ) ) ;
#61412 =( BOUNDED_CURVE ( )  B_SPLINE_CURVE ( 2, ( #8368, #262, #755, #32658, #46859, #31143, #71183, #31639, #85931 ),
 .UNSPECIFIED., .F., .T. ) 
 B_SPLINE_CURVE_WITH_KNOTS ( ( 3, 2, 2, 2, 3 ),
 ( 0.7540322580645161255, 0.7553763440860215006, 0.7580645161290322509, 0.7607526881720430012, 0.7620967741935483764 ),
 .UNSPECIFIED. ) 
 CURVE ( )  GEOMETRIC_REPRESENTATION_ITEM ( )  RATIONAL_B_SPLINE_CURVE ( ( 0.9330127018922194093, 0.9330127018922194093, 1.000000000000000000, 0.8660254037844387076, 1.000000000000000000, 0.8660254037844387076, 1.000000000000000000, 0.9330127018922194093, 0.9330127018922194093 ) ) 
 REPRESENTATION_ITEM ( '' )  );
#61413 = CARTESIAN_POINT ( 'NONE',  ( 72.49520321802694411, 71.62171839754151392, 6.144630347475415810 ) ) ;
#61414 = CARTESIAN_POINT ( 'NONE',  ( 45.32607884611513072, 203.6427522451419065, 10.00000000000009237 ) ) ;
#61415 = CARTESIAN_POINT ( 'NONE',  ( 125.3701074643745699, 249.3149278399160949, 9.188101187500093303 ) ) ;
#61416 = CARTESIAN_POINT ( 'NONE',  ( 180.6483990817532685, 294.3080752668889772, -3.362655399551144786 ) ) ;
#61417 = CIRCLE ( 'NONE', #17761, 1.449999999999993072 ) ;
#61418 = CARTESIAN_POINT ( 'NONE',  ( 66.85822330536446145, 67.61959507708256467, -6.456617525293864013 ) ) ;
#61419 = CARTESIAN_POINT ( 'NONE',  ( 196.0034224882197975, 291.1591091234520263, 17.53794140922627776 ) ) ;
#61420 = CARTESIAN_POINT ( 'NONE',  ( 175.4077757953151604, 253.5139745403514553, -3.897595921025101884 ) ) ;
#61421 = CARTESIAN_POINT ( 'NONE',  ( 45.45211389745056607, 206.2369531367911293, -4.594050593750048428 ) ) ;
#61422 = CARTESIAN_POINT ( 'NONE',  ( -19.65312891409030271, 93.06504152958497400, -10.00000000000000888 ) ) ;
#61423 = CARTESIAN_POINT ( 'NONE',  ( 85.68664465223866955, 48.45350732935998650, -12.23334744974732402 ) ) ;
#61424 = VERTEX_POINT ( 'NONE', #75469 ) ;
#61425 = LINE ( 'NONE', #47228, #42974 ) ;
#61426 = CARTESIAN_POINT ( 'NONE',  ( 180.9399124977257145, 267.5927373598447048, 15.00208439449252751 ) ) ;
#61427 = CARTESIAN_POINT ( 'NONE',  ( -105.0000000000000000, 10.00000000000000000, -14.21260523776212281 ) ) ;
#61428 = CARTESIAN_POINT ( 'NONE',  ( 162.8384627734353387, 250.8402808221231624, -13.07578932517241732 ) ) ;
#61429 = DIRECTION ( 'NONE',  ( 0.000000000000000000, 0.000000000000000000, 1.000000000000000000 ) ) ;
#61430 = CARTESIAN_POINT ( 'NONE',  ( -6.281727404287059890, 25.63055774385195207, -10.00000000000000000 ) ) ;
#61431 = AXIS2_PLACEMENT_3D ( 'NONE', #99843, #32430, #63325 ) ;
#61432 = CARTESIAN_POINT ( 'NONE',  ( 182.2055061536417497, 262.5723910214719581, 12.91931843363846966 ) ) ;
#61433 = CARTESIAN_POINT ( 'NONE',  ( 101.6177300921036419, 236.1427522451419065, -10.00000000000009415 ) ) ;
#61434 = B_SPLINE_SURFACE_WITH_KNOTS ( 'NONE', 3, 1, ( 
 ( #56630, #80987 ),
 ( #88597, #11052 ),
 ( #58125, #10044 ),
 ( #25227, #19160 ),
 ( #2968, #1941 ),
 ( #26242, #40907 ),
 ( #12044, #42897 ),
 ( #3455, #79975 ),
 ( #95695, #50034 ),
 ( #11553, #80481 ),
 ( #10544, #81470 ),
 ( #32827, #89106 ),
 ( #63735, #41418 ),
 ( #64745, #72865 ),
 ( #17643, #96173 ),
 ( #33861, #41929 ),
 ( #87613, #34334 ),
 ( #94670, #26734 ),
 ( #42412, #57116 ),
 ( #88099, #18141 ),
 ( #56114, #3933 ),
 ( #18648, #65230 ),
 ( #34816, #49528 ),
 ( #2452, #73346 ),
 ( #79480, #65717 ),
 ( #87105, #48541 ),
 ( #71855, #33334 ),
 ( #96673, #27241 ),
 ( #19656, #50518 ),
 ( #64231, #95181 ),
 ( #49041, #51017 ),
 ( #75847, #83459 ),
 ( #28222, #52511 ),
 ( #44412, #98650 ) ),
 .UNSPECIFIED., .T., .F., .F.,
 ( 4, 2, 2, 2, 2, 2, 2, 2, 2, 2, 2, 2, 2, 2, 2, 2, 4 ),
 ( 2, 2 ),
 ( 0.000000000000000000, 0.06250000000000000000, 0.1250000000000000000, 0.1875000000000000000, 0.2500000000000000000, 0.3125000000000000000, 0.3750000000000000000, 0.4375000000000000000, 0.5000000000000000000, 0.5625000000000000000, 0.6250000000000000000, 0.6875000000000000000, 0.7500000000000000000, 0.8125000000000000000, 0.8750000000000000000, 0.9375000000000000000, 1.000000000000000000 ),
 ( 0.000000000000000000, 1.000000000000000000 ),
 .UNSPECIFIED. ) ;
#61435 = CARTESIAN_POINT ( 'NONE',  ( 198.2505066714982149, 285.2670451491296149, 0.000000000000000000 ) ) ;
#61436 = VERTEX_POINT ( 'NONE', #89713 ) ;
#61437 = CARTESIAN_POINT ( 'NONE',  ( 202.7599932440484451, 279.4563852894229967, 15.58249343055423353 ) ) ;
#61438 = CARTESIAN_POINT ( 'NONE',  ( 208.3586375946586315, 269.7592488206576604, -1.970210487958146128 ) ) ;
#61439 = AXIS2_PLACEMENT_3D ( 'NONE', #63102, #31196, #24102 ) ;
#61440 = ADVANCED_FACE ( 'NONE', ( #44536 ), #67860, .F. ) ;
#61441 = CARTESIAN_POINT ( 'NONE',  ( 28.02335264628875677, 196.1744531367911293, 4.594050593750047540 ) ) ;
#61442 = CARTESIAN_POINT ( 'NONE',  ( 13.25914332478948410, 9.783808731787853930, -6.180339887498949025 ) ) ;
#61443 = CARTESIAN_POINT ( 'NONE',  ( 192.4771936439569515, 272.0680645981377666, 14.18742438910983594 ) ) ;
#61444 = CARTESIAN_POINT ( 'NONE',  ( 40.06784160394645511, 182.3932355074535394, -2.679491924311248496 ) ) ;
#61445 = CARTESIAN_POINT ( 'NONE',  ( 73.03785937943386841, 69.69865149502336976, 9.683281169778272357 ) ) ;
#61447 = CARTESIAN_POINT ( 'NONE',  ( 66.99449581658849695, 218.6744531367911293, 4.594050593750047540 ) ) ;
#61446 = CARTESIAN_POINT ( 'NONE',  ( 198.1897299879200602, 277.3109323272205415, -15.34172296478933717 ) ) ;
#61448 = ADVANCED_FACE ( 'NONE', ( #68840 ), #44949, .F. ) ;
#61449 = CARTESIAN_POINT ( 'NONE',  ( 200.2316334480823912, 283.8356329158505105, 17.02791935830326508 ) ) ;
#61450 = CARTESIAN_POINT ( 'NONE',  ( 72.53392300481422694, 57.31226291295279651, 15.84842549994240990 ) ) ;
#61451 = CARTESIAN_POINT ( 'NONE',  ( -29.35832683651975472, 95.01536403814361620, 44.58472265727041872 ) ) ;
#61452 = CARTESIAN_POINT ( 'NONE',  ( 8.758203689844268780, 28.55466486950697913, -1.111400068045478839E-16 ) ) ;
#61453 = ORIENTED_EDGE ( 'NONE', *, *, #81668, .T. ) ;
#61454 = CARTESIAN_POINT ( 'NONE',  ( 164.7681158011125717, 268.8552380765891030, 16.67724236807602267 ) ) ;
#61455 = CARTESIAN_POINT ( 'NONE',  ( 14.81672556217377235, 179.3615022471902591, -10.00000000000009592 ) ) ;
#61456 = CARTESIAN_POINT ( 'NONE',  ( 164.1821508476733698, 246.2751683663292397, -7.347745041495428175 ) ) ;
#61457 = CARTESIAN_POINT ( 'NONE',  ( 144.4230134433972239, 248.0643266524160140, 9.188101187500095079 ) ) ;
#61458 = CARTESIAN_POINT ( 'NONE',  ( 34.51455378690028652, 28.43085787977765477, -9.188101187500008038 ) ) ;
#61460 = EDGE_CURVE ( 'NONE', #86782, #74702, #93123, .T. ) ;
#61459 = CARTESIAN_POINT ( 'NONE',  ( 167.6696528517744014, 262.3690162733964826, -17.00514220863813364 ) ) ;
#61461 = CARTESIAN_POINT ( 'NONE',  ( 185.2747196154622316, 260.3698368134728867, 6.698900342170079902 ) ) ;
#61462 = CARTESIAN_POINT ( 'NONE',  ( 74.94213196210210981, 53.20634399479197896, -16.03712342241558275 ) ) ;
#61464 = CARTESIAN_POINT ( 'NONE',  ( 185.1984267626157248, 277.5364252950313357, -17.64468014200656398 ) ) ;
#61463 = CARTESIAN_POINT ( 'NONE',  ( 70.32223144932660830, 70.48993496229302025, 5.907123158273768659 ) ) ;
#61465 = CARTESIAN_POINT ( 'NONE',  ( 68.55596672819507376, 64.28337496226291137, 12.40357123185196819 ) ) ;
#61466 = ORIENTED_EDGE ( 'NONE', *, *, #989, .T. ) ;
#61467 = CARTESIAN_POINT ( 'NONE',  ( 150.6790040019602088, 269.6633047651677089, 15.38315204620803378 ) ) ;
#61468 =( NAMED_UNIT ( * ) SI_UNIT ( $, .STERADIAN. ) SOLID_ANGLE_UNIT ( ) );
#61469 = CARTESIAN_POINT ( 'NONE',  ( 6.802937163926562114, 15.87878583063839066, -9.188101187500006262 ) ) ;
#61470 = LINE ( 'NONE', #76209, #85583 ) ;
#61471 = CARTESIAN_POINT ( 'NONE',  ( 7.290083236948965428, 25.18502408145589655, 5.678558825948276656 ) ) ;
#61472 = ORIENTED_EDGE ( 'NONE', *, *, #3104, .F. ) ;
#61473 = CARTESIAN_POINT ( 'NONE',  ( 206.7778081894269064, 272.4973256686178615, 7.979133442510888408 ) ) ;
#61474 = CARTESIAN_POINT ( 'NONE',  ( -59.75159773472199021, 60.38055040163846598, 59.99999999999999289 ) ) ;
#61475 = CARTESIAN_POINT ( 'NONE',  ( 69.53667171941721392, 62.56887577352630814, 13.34165820888200216 ) ) ;
#61476 = ADVANCED_FACE ( 'NONE', ( #17143 ), #86117, .T. ) ;
#61477 = CARTESIAN_POINT ( 'NONE',  ( 148.8985332352210946, 273.2084804242117571, -9.391003212318970839 ) ) ;
#61478 = CARTESIAN_POINT ( 'NONE',  ( -48.47243291925848752, 30.64988553008148031, -10.00000000000000000 ) ) ;
#61479 = CARTESIAN_POINT ( 'NONE',  ( 149.6987302396718178, 272.4200664568434718, 11.31912059095424183 ) ) ;
#61480 = CARTESIAN_POINT ( 'NONE',  ( 208.0421103033489771, 270.3074901711881353, -2.473242163239977476 ) ) ;
#61481 = CARTESIAN_POINT ( 'NONE',  ( 153.0927037754837556, 265.4826541232073964, -16.15085267704102634 ) ) ;
#61482 = ORIENTED_EDGE ( 'NONE', *, *, #79693, .T. ) ;
#61483 = CARTESIAN_POINT ( 'NONE',  ( 191.4544176431711264, 281.2354317515596449, 16.67543541242699945 ) ) ;
#61484 = CARTESIAN_POINT ( 'NONE',  ( 72.48280754011685190, 70.60311863597817705, 7.264376673680498442 ) ) ;
#61485 = VERTEX_POINT ( 'NONE', #23237 ) ;
#61486 = CARTESIAN_POINT ( 'NONE',  ( 149.5593209768671841, 271.6026526530012575, 11.55487339793564949 ) ) ;
#61487 = CARTESIAN_POINT ( 'NONE',  ( 15.15952728095722613, 172.8927522451418213, 10.00000000000009948 ) ) ;
#61488 = CARTESIAN_POINT ( 'NONE',  ( 81.59902824993105241, 45.46755018456938302, -11.06827361697009060 ) ) ;
#61489 = ORIENTED_EDGE ( 'NONE', *, *, #34851, .T. ) ;
#61490 = VECTOR ( 'NONE', #46856, 1000.000000000000114 ) ;
#61491 = DIRECTION ( 'NONE',  ( 0.09274582908232943679, 0.9956898167541091693, 0.000000000000000000 ) ) ;
#61492 = LINE ( 'NONE', #69094, #39479 ) ;
#61493 = CARTESIAN_POINT ( 'NONE',  ( 149.5796913320911870, 271.5673701627850960, -12.80793412251569841 ) ) ;
#61494 = CARTESIAN_POINT ( 'NONE',  ( 69.33571648121584019, 62.94790354691227918, 13.62394890031374572 ) ) ;
#61495 = VERTEX_POINT ( 'NONE', #46530 ) ;
#61496 = CARTESIAN_POINT ( 'NONE',  ( 101.2839494695023603, 229.2833772461660544, -9.188101187500095079 ) ) ;
#61497 = CARTESIAN_POINT ( 'NONE',  ( 155.6860346224306682, 260.9908733354596961, 18.34621944435518870 ) ) ;
#61498 = B_SPLINE_CURVE_WITH_KNOTS ( 'NONE', 3,
 ( #6927, #47419, #85479, #46411 ),
 .UNSPECIFIED., .F., .F.,
 ( 4, 4 ),
 ( 0.003806595552051763101, 0.007765155676520470000 ),
 .UNSPECIFIED. ) ;
#61499 = CARTESIAN_POINT ( 'NONE',  ( 151.0099717111976076, 269.0900518771037468, 15.84752309685681659 ) ) ;
#61500 = CARTESIAN_POINT ( 'NONE',  ( 139.8671854259164320, 244.8927522451418497, 10.00000000000009948 ) ) ;
#61501 = ORIENTED_EDGE ( 'NONE', *, *, #82054, .F. ) ;
#61502 = EDGE_CURVE ( 'NONE', #41184, #61039, #87062, .T. ) ;
#61503 = ORIENTED_EDGE ( 'NONE', *, *, #27895, .T. ) ;
#61504 = ORIENTED_EDGE ( 'NONE', *, *, #86975, .F. ) ;
#61505 = CARTESIAN_POINT ( 'NONE',  ( 73.99038332904399340, 64.06192407381385578, 14.02288482052439456 ) ) ;
#61506 = ORIENTED_EDGE ( 'NONE', *, *, #43172, .F. ) ;
#61507 = CARTESIAN_POINT ( 'NONE',  ( 192.5672132233574700, 296.7161803602032819, 11.26440590052197521 ) ) ;
#61508 = CIRCLE ( 'NONE', #17855, 17.82106496071138935 ) ;
#61509 = ORIENTED_EDGE ( 'NONE', *, *, #56009, .T. ) ;
#61510 = EDGE_CURVE ( 'NONE', #15709, #24115, #26231, .T. ) ;
#61511 = CARTESIAN_POINT ( 'NONE',  ( 163.7038023771459052, 247.1036922210055025, -6.448491958542482472 ) ) ;
#61512 = FACE_OUTER_BOUND ( 'NONE', #26495, .T. ) ;
#61513 = CARTESIAN_POINT ( 'NONE',  ( 171.0838469510729283, 283.5197208256832937, 12.13844873189909457 ) ) ;
#61514 = CARTESIAN_POINT ( 'NONE',  ( 148.3625667886952044, 273.6754917110858401, -8.960758510948144462 ) ) ;
#61515 = EDGE_CURVE ( 'NONE', #47543, #77760, #30299, .T. ) ;
#61516 = CARTESIAN_POINT ( 'NONE',  ( 82.56047309644807797, 54.07683023134061528, -15.52634518316282097 ) ) ;
#61517 = ADVANCED_FACE ( 'NONE', ( #77963 ), #38936, .F. ) ;
#61518 = CARTESIAN_POINT ( 'NONE',  ( 74.04864439501488960, 57.31504094317030251, -16.45781754585126677 ) ) ;
#61519 = CARTESIAN_POINT ( 'NONE',  ( 10.08301516415377641, 26.79752408145591147, -5.678558825948271327 ) ) ;
#61520 = CARTESIAN_POINT ( 'NONE',  ( 199.3479728691114587, 277.9353724323879078, -15.41277036647585597 ) ) ;
#61521 = CARTESIAN_POINT ( 'NONE',  ( 80.12283971196008281, 57.76720862780120314, 16.60271659255639065 ) ) ;
#61523 = ORIENTED_EDGE ( 'NONE', *, *, #37929, .T. ) ;
#61522 = FACE_OUTER_BOUND ( 'NONE', #62971, .T. ) ;
#61524 = EDGE_CURVE ( 'NONE', #68209, #74106, #61238, .T. ) ;
#61525 = APPLICATION_CONTEXT ( 'automotive_design' ) ;
#61526 = CARTESIAN_POINT ( 'NONE',  ( 202.4017613376760494, 280.0768611521521620, 15.73960524502980540 ) ) ;
#61527 = EDGE_CURVE ( 'NONE', #61138, #43154, #39923, .T. ) ;
#61528 = CARTESIAN_POINT ( 'NONE',  ( 188.1240574672448247, 260.7517132086819629, 2.838756651779489104 ) ) ;
#61529 = CARTESIAN_POINT ( 'NONE',  ( 15.94180138266918689, 46.41934012499306306, 59.99999999999999289 ) ) ;
#61530 = CARTESIAN_POINT ( 'NONE',  ( 67.95331009947700807, 66.07265274243333408, -10.46626145091951621 ) ) ;
#61531 = CARTESIAN_POINT ( 'NONE',  ( 200.5438717407500917, 283.2948203288816558, 18.39667691545567152 ) ) ;
#61532 = CARTESIAN_POINT ( 'NONE',  ( 157.9492502841812893, 281.0771850073649034, 1.816109525321617291 ) ) ;
#61533 = ORIENTED_EDGE ( 'NONE', *, *, #4114, .F. ) ;
#61534 = CARTESIAN_POINT ( 'NONE',  ( 155.4220579613188704, 261.4480943245178537, -17.00714975260428474 ) ) ;
#61535 = CARTESIAN_POINT ( 'NONE',  ( 73.89769204157855143, 62.62724885997820934, -14.63212924024895933 ) ) ;
#61536 = FACE_OUTER_BOUND ( 'NONE', #89121, .T. ) ;
#61537 = CARTESIAN_POINT ( 'NONE',  ( 8.086986483384336566, 162.1427522451417644, 1.119607411625061291E-15 ) ) ;
#61538 = CARTESIAN_POINT ( 'NONE',  ( 193.2604171883379536, 267.6068621284443907, -10.96396649826040282 ) ) ;
#61539 = DIRECTION ( 'NONE',  ( -1.000000000000000000, 0.000000000000000000, -0.000000000000000000 ) ) ;
#61540 = CARTESIAN_POINT ( 'NONE',  ( 204.2359371119229650, 276.8999755211443130, -15.33127121419060401 ) ) ;
#61541 = CARTESIAN_POINT ( 'NONE',  ( 161.5226180746127227, 251.2552919257010728, -12.89472374756154949 ) ) ;
#61543 = CARTESIAN_POINT ( 'NONE',  ( 87.79103858326931231, 44.11529954957103428, 2.696194862051933150 ) ) ;
#61542 = CARTESIAN_POINT ( 'NONE',  ( -6.860972828079417773, 166.8458772461660544, 9.188101187500095079 ) ) ;
#61544 = CARTESIAN_POINT ( 'NONE',  ( 58.25224935450648189, 215.9860189848785694, -2.679491924311252493 ) ) ;
#61545 = ORIENTED_EDGE ( 'NONE', *, *, #25834, .F. ) ;
#61546 = EDGE_LOOP ( 'NONE', ( #60864, #50809, #67728, #9747 ) ) ;
#61547 = DIRECTION ( 'NONE',  ( 0.000000000000000000, 0.000000000000000000, 1.000000000000000000 ) ) ;
#61548 = CARTESIAN_POINT ( 'NONE',  ( 26.18314342202568668, 41.82794442100486521, 10.00000000000000000 ) ) ;
#61549 = CARTESIAN_POINT ( 'NONE',  ( 84.68093819348166562, 42.16537887657799644, 0.2499978311480390847 ) ) ;
#61550 = PLANE ( 'NONE',  #47861 ) ;
#61551 = CARTESIAN_POINT ( 'NONE',  ( 82.68581151109542304, 43.22490338220254102, 7.598561826035989064 ) ) ;
#61552 = CARTESIAN_POINT ( 'NONE',  ( 149.9586195398654525, 276.8495302347727147, 3.185754299552747248 ) ) ;
#61553 = CARTESIAN_POINT ( 'NONE',  ( 29.48529115882250551, 178.6423013555409796, -4.594050593750043987 ) ) ;
#61554 = CARTESIAN_POINT ( 'NONE',  ( 124.8563387505838165, 233.7048013555409796, 4.594050593750051981 ) ) ;
#61555 = DIRECTION ( 'NONE',  ( -1.000000000000000000, 0.000000000000000000, 0.000000000000000000 ) ) ;
#61556 = CARTESIAN_POINT ( 'NONE',  ( -17.42236680055705023, 149.2012482093457777, 0.000000000000000000 ) ) ;
#61557 = CARTESIAN_POINT ( 'NONE',  ( 33.07542782529571923, 183.2365022471901739, -10.00000000000009237 ) ) ;
#61558 = CARTESIAN_POINT ( 'NONE',  ( 178.4974649003195850, 283.7799215797293755, -14.74701626068640259 ) ) ;
#61559 = CARTESIAN_POINT ( 'NONE',  ( 76.38284716662768403, 54.82274627456094152, -16.11362980023774227 ) ) ;
#61560 = CARTESIAN_POINT ( 'NONE',  ( 80.57046890446221710, 57.17601910317578984, -16.22952344167990901 ) ) ;
#61561 = CARTESIAN_POINT ( 'NONE',  ( 155.6276701977099890, 261.0919634844306643, 17.49722577287685255 ) ) ;
#61562 = CARTESIAN_POINT ( 'NONE',  ( 161.1150691641480535, 251.5875096731584506, -13.48836942566120101 ) ) ;
#61563 = CARTESIAN_POINT ( 'NONE',  ( -19.65312891409030271, 93.06504152958497400, -10.00000000000000888 ) ) ;
#61564 = CARTESIAN_POINT ( 'NONE',  ( 193.1995342044276640, 264.0813980297376133, 7.606167026564889966 ) ) ;
#61565 = CARTESIAN_POINT ( 'NONE',  ( 171.5385771854158179, 279.8808931372358302, 13.92051632058779198 ) ) ;
#61566 = CARTESIAN_POINT ( 'NONE',  ( 204.0884846259506276, 275.1553707185394728, 13.46337290381501717 ) ) ;
#61567 = CARTESIAN_POINT ( 'NONE',  ( 68.74125309881081591, 68.48789582852654689, 6.924389039908457555 ) ) ;
#61568 = CARTESIAN_POINT ( 'NONE',  ( 147.7870527676176948, 274.6723112360602386, 9.257357958194809555 ) ) ;
#61569 = CARTESIAN_POINT ( 'NONE',  ( 180.9828039363494554, 267.0267840551962877, -14.76148221183092524 ) ) ;
#61570 = ORIENTED_EDGE ( 'NONE', *, *, #61826, .T. ) ;
#61571 = CARTESIAN_POINT ( 'NONE',  ( 152.5396176296194710, 266.8690347833386909, -15.56576981617802424 ) ) ;
#61572 = CARTESIAN_POINT ( 'NONE',  ( 184.6479839499307332, 269.5423948272451753, 15.39131224564481037 ) ) ;
#61573 = CARTESIAN_POINT ( 'NONE',  ( 90.37718171876834106, 232.1744531367911293, 4.594050593750047540 ) ) ;
#61574 = CARTESIAN_POINT ( 'NONE',  ( 13.03712377304622194, 16.03085787977761356, 9.188101187500006262 ) ) ;
#61576 = EDGE_CURVE ( 'NONE', #10473, #10907, #1468, .T. ) ;
#61575 = CARTESIAN_POINT ( 'NONE',  ( 74.83655476910676896, 53.51806293180212037, 16.54630480343736920 ) ) ;
#61577 = FACE_OUTER_BOUND ( 'NONE', #51842, .T. ) ;
#61579 = CARTESIAN_POINT ( 'NONE',  ( 191.6023198849542837, 276.9562025558888081, 16.79891912045939151 ) ) ;
#61578 = DIRECTION ( 'NONE',  ( -0.8660254037844387076, -0.4999999999999998890, -0.000000000000000000 ) ) ;
#61580 = CARTESIAN_POINT ( 'NONE',  ( 149.5130609720542623, 271.6827773316956609, 13.04552708959771934 ) ) ;
#61581 = DIRECTION ( 'NONE',  ( -0.8660254037844387076, -0.4999999999999998890, -0.000000000000000000 ) ) ;
#61582 = CARTESIAN_POINT ( 'NONE',  ( -69.61464189717713680, 45.83092310410447112, 10.00000000000000000 ) ) ;
#61583 = CARTESIAN_POINT ( 'NONE',  ( 55.59208832369112230, 196.2365022471902307, 10.00000000000009948 ) ) ;
#61584 = DIRECTION ( 'NONE',  ( 0.9532659690011938691, -0.2314883312386622760, 0.1941575258509293800 ) ) ;
#61585 = CARTESIAN_POINT ( 'NONE',  ( 86.33473264480980447, 47.64805230391016977, 10.69327747295855247 ) ) ;
#61586 = ORIENTED_EDGE ( 'NONE', *, *, #92315, .F. ) ;
#61587 = CARTESIAN_POINT ( 'NONE',  ( 33.49394369984602804, 21.19860640527294038, 2.839279412974134775 ) ) ;
#61588 = CARTESIAN_POINT ( 'NONE',  ( 177.9874092160698069, 279.9792724555832706, 15.65335057370039884 ) ) ;
#61589 = CARTESIAN_POINT ( 'NONE',  ( 199.9859019575963259, 270.1052791603114542, 9.171208846631140332 ) ) ;
#61590 = CARTESIAN_POINT ( 'NONE',  ( 149.3629284598386278, 271.9428144707212027, -12.99253781774931049 ) ) ;
#61592 = ORIENTED_EDGE ( 'NONE', *, *, #41565, .T. ) ;
#61591 = ADVANCED_FACE ( 'NONE', ( #15129 ), #54628, .F. ) ;
#61593 = EDGE_CURVE ( 'NONE', #87380, #45306, #79870, .T. ) ;
#61594 = CARTESIAN_POINT ( 'NONE',  ( 84.48836950856804151, 49.89909654526366722, -13.70430404532020319 ) ) ;
#61595 = CARTESIAN_POINT ( 'NONE',  ( 78.72343666810984075, 48.48097556600880864, 14.16619407085236837 ) ) ;
#61596 = CARTESIAN_POINT ( 'NONE',  ( 180.4572463832561482, 261.7460625851787199, -13.63662180976220384 ) ) ;
#61597 = CARTESIAN_POINT ( 'NONE',  ( 169.7161983584676932, 251.3797710867630713, -8.400916520806605448 ) ) ;
#61598 = CARTESIAN_POINT ( 'NONE',  ( 152.6656396574222754, 266.2223508737794759, 17.04346597795114349 ) ) ;
#61599 = ORIENTED_EDGE ( 'NONE', *, *, #80736, .F. ) ;
#61600 = CARTESIAN_POINT ( 'NONE',  ( 73.64088816139484095, 69.63733386616164012, 10.15931356738738423 ) ) ;
#61601 = CARTESIAN_POINT ( 'NONE',  ( 27.02885687802902837, 37.64646525600391413, -2.839279412974133887 ) ) ;
#61602 = ORIENTED_EDGE ( 'NONE', *, *, #45891, .F. ) ;
#61603 = CARTESIAN_POINT ( 'NONE',  ( 84.37825102736907468, 49.99960613749294680, 13.80049582259581520 ) ) ;
#61604 = CARTESIAN_POINT ( 'NONE',  ( 169.0079941869541074, 269.5332732215450733, -17.80121103236473346 ) ) ;
#61605 = ORIENTED_EDGE ( 'NONE', *, *, #72309, .T. ) ;
#61606 = CARTESIAN_POINT ( 'NONE',  ( 86.53913842531343903, 47.33648749047813453, -10.24973804167819935 ) ) ;
#61607 = CARTESIAN_POINT ( 'NONE',  ( 158.8194364388402562, 255.9479314064563766, 16.03906445419635673 ) ) ;
#61608 = CARTESIAN_POINT ( 'NONE',  ( 84.56695678370634539, 50.23807730109928826, 13.87492620287773804 ) ) ;
#61609 = CARTESIAN_POINT ( 'NONE',  ( 192.8739241956344017, 296.5795591684099577, -13.56467825654580928 ) ) ;
#61610 = CARTESIAN_POINT ( 'NONE',  ( 201.2139346379346705, 282.1342373466909521, -16.65315141107179286 ) ) ;
#61611 = CARTESIAN_POINT ( 'NONE',  ( 86.26411663623493098, 44.87056880271241255, -7.873569013553530560 ) ) ;
#61612 = CARTESIAN_POINT ( 'NONE',  ( 80.24827019267925721, 44.30331806697298447, 11.36816880119114437 ) ) ;
#61613 = CARTESIAN_POINT ( 'NONE',  ( 79.14312167556931854, 57.64441083166269664, 0.000000000000000000 ) ) ;
#61614 = CARTESIAN_POINT ( 'NONE',  ( 148.6023484834014425, 275.2601776331305814, 7.517535991345212665 ) ) ;
#61615 = ORIENTED_EDGE ( 'NONE', *, *, #44813, .F. ) ;
#61616 = CARTESIAN_POINT ( 'NONE',  ( 176.3865323452404823, 258.8737835494043225, 13.24306684835586623 ) ) ;
#61617 = EDGE_LOOP ( 'NONE', ( #96926, #44415, #21410, #3627 ) ) ;
#61618 = VERTEX_POINT ( 'NONE', #58140 ) ;
#61619 = CARTESIAN_POINT ( 'NONE',  ( 172.8702133838303041, 271.0664845223420230, 16.42754727834196160 ) ) ;
#61620 = VERTEX_POINT ( 'NONE', #42913 ) ;
#61621 = EDGE_CURVE ( 'NONE', #87203, #3988, #49058, .T. ) ;
#61623 = CARTESIAN_POINT ( 'NONE',  ( 45.80758703142363686, 72.03864405183792030, -10.00000000000000000 ) ) ;
#61622 = CARTESIAN_POINT ( 'NONE',  ( 172.6025460550783919, 256.6729997644848140, -11.64617786982520897 ) ) ;
#61624 = CARTESIAN_POINT ( 'NONE',  ( 175.3932935011599170, 269.2958584618301643, -17.65833184418574930 ) ) ;
#61625 = CARTESIAN_POINT ( 'NONE',  ( 201.2723982155681028, 274.9066758845833647, -14.03142259981584772 ) ) ;
#61626 = CARTESIAN_POINT ( 'NONE',  ( 160.1795347027651815, 282.8633239002924711, 5.491715875156680582 ) ) ;
#61627 = CARTESIAN_POINT ( 'NONE',  ( 78.90549422596571105, 46.47045305960070039, 12.99985401326298984 ) ) ;
#61628 = CARTESIAN_POINT ( 'NONE',  ( 184.5123196318015459, 277.1383014161853566, -17.82024832176989904 ) ) ;
#61629 = CARTESIAN_POINT ( 'NONE',  ( 76.69634485559663517, 63.33187278031594758, -15.42689205524521157 ) ) ;
#61630 = ADVANCED_FACE ( 'NONE', ( #17659 ), #10560, .T. ) ;
#61631 = CARTESIAN_POINT ( 'NONE',  ( 178.0470025766832123, 255.4632854186900772, 5.005086694065276731 ) ) ;
#61632 = ADVANCED_FACE ( 'NONE', ( #65733 ), #2469, .F. ) ;
#61633 = CARTESIAN_POINT ( 'NONE',  ( 114.9778026189612632, 243.3149278399160664, 9.188101187500093303 ) ) ;
#61634 = CARTESIAN_POINT ( 'NONE',  ( 70.73253466316766946, 60.52854348683570151, -14.67665510802405748 ) ) ;
#61635 = CARTESIAN_POINT ( 'NONE',  ( 161.3088938790619409, 283.6794878094777914, 2.159307202287777727 ) ) ;
#61636 = CARTESIAN_POINT ( 'NONE',  ( 188.0760642469317645, 273.6708693882125090, 17.00871842608619033 ) ) ;
#61637 = ORIENTED_EDGE ( 'NONE', *, *, #99957, .F. ) ;
#61638 = EDGE_CURVE ( 'NONE', #64789, #82018, #48111, .T. ) ;
#61639 = CARTESIAN_POINT ( 'NONE',  ( 164.1654149204426858, 248.3041558426086226, -9.671695341034215687 ) ) ;
#61640 = ADVANCED_FACE ( 'NONE', ( #89120 ), #95709, .T. ) ;
#61641 = CARTESIAN_POINT ( 'NONE',  ( 73.88216889899386786, 63.33152347620602285, -14.31039344191799323 ) ) ;
#61642 = EDGE_CURVE ( 'NONE', #7878, #74497, #15851, .T. ) ;
#61643 = PLANE ( 'NONE',  #81952 ) ;
#61644 = CARTESIAN_POINT ( 'NONE',  ( 157.3363371328520088, 258.1324655395517311, 18.24585617226787093 ) ) ;
#61645 = CARTESIAN_POINT ( 'NONE',  ( 73.60132943463672461, 67.75729915613128185, 11.45358097554368904 ) ) ;
#61646 = LINE ( 'NONE', #30765, #23825 ) ;
#61647 = CARTESIAN_POINT ( 'NONE',  ( 73.92365886092795790, 54.91122253338699011, -16.13237890612813885 ) ) ;
#61648 = ORIENTED_EDGE ( 'NONE', *, *, #99241, .F. ) ;
#61649 = CARTESIAN_POINT ( 'NONE',  ( 147.9745743502305118, 274.3475143274592938, 10.02752110366533778 ) ) ;
#61650 = CIRCLE ( 'NONE', #81167, 0.1418229129680828593 ) ;
#61651 = ORIENTED_EDGE ( 'NONE', *, *, #48180, .T. ) ;
#61652 = CARTESIAN_POINT ( 'NONE',  ( 148.1974503712686158, 273.9614817352322120, -7.884397846570731616 ) ) ;
#61653 = CARTESIAN_POINT ( 'NONE',  ( 39.26390101962405055, 200.1427522451419350, -10.00000000000009592 ) ) ;
#61654 = EDGE_LOOP ( 'NONE', ( #91445, #60495, #25844, #12302 ) ) ;
#61655 = CARTESIAN_POINT ( 'NONE',  ( 188.0293636999220723, 266.1540144583576648, -11.80271381409143672 ) ) ;
#61656 = CARTESIAN_POINT ( 'NONE',  ( 159.9714013527444649, 278.6080261497965580, 10.43375755400861848 ) ) ;
#61657 = CARTESIAN_POINT ( 'NONE',  ( 176.0575385324409865, 258.1988160713917182, -12.86591411535773233 ) ) ;
#61658 = CARTESIAN_POINT ( 'NONE',  ( 157.7045215221510830, 262.9535044009366516, 17.16314129935500077 ) ) ;
#61659 = CARTESIAN_POINT ( 'NONE',  ( 81.50391902668040700, 43.19956922895749329, 8.559400874430535211 ) ) ;
#61661 = CARTESIAN_POINT ( 'NONE',  ( 69.81582973446273854, 63.14295414325376044, -13.67321376832284230 ) ) ;
#61660 = CARTESIAN_POINT ( 'NONE',  ( 184.7099738404339178, 289.1045521149691808, -13.19732552672321368 ) ) ;
#61662 = CARTESIAN_POINT ( 'NONE',  ( 158.1690553627090310, 281.8858333404083965, -5.006681078564091614 ) ) ;
#61663 = ORIENTED_EDGE ( 'NONE', *, *, #69840, .F. ) ;
#61664 = CARTESIAN_POINT ( 'NONE',  ( 205.2564848266901834, 271.9733254596621350, -9.597888780111448526 ) ) ;
#61665 = CARTESIAN_POINT ( 'NONE',  ( -29.63305522156611005, 61.36453520006032392, -10.00000000000000000 ) ) ;
#61666 = CARTESIAN_POINT ( 'NONE',  ( 163.6101490995871472, 247.6943118105651536, -7.655108696039592431 ) ) ;
#61667 = LINE ( 'NONE', #7991, #17337 ) ;
#61668 = CARTESIAN_POINT ( 'NONE',  ( 192.5677150043008794, 271.3893586466145962, -15.08671890483280009 ) ) ;
#61669 = CARTESIAN_POINT ( 'NONE',  ( 188.3311882918543745, 299.0666206182007159, -3.691789600375173563 ) ) ;
#61670 = CARTESIAN_POINT ( 'NONE',  ( 83.20126876621219481, 43.26424907438605771, 7.146979139294720618 ) ) ;
#61671 = DIRECTION ( 'NONE',  ( -0.000000000000000000, -0.000000000000000000, -1.000000000000000000 ) ) ;
#61672 = CARTESIAN_POINT ( 'NONE',  ( 11.39698775767666916, 6.984156793818252495, 0.000000000000000000 ) ) ;
#61673 = CARTESIAN_POINT ( 'NONE',  ( 72.88043634756726874, 66.05899410211006284, -12.94925710025703758 ) ) ;
#61674 = CARTESIAN_POINT ( 'NONE',  ( 66.66973629016931113, 218.4869531367911293, 4.594050593750046652 ) ) ;
#61675 = CARTESIAN_POINT ( 'NONE',  ( 44.35815684012577265, 67.96982248125696913, 10.00000000000000000 ) ) ;
#61676 = CARTESIAN_POINT ( 'NONE',  ( 147.3715240516018810, 275.3920280842035595, -3.728968767617475866 ) ) ;
#61677 = CARTESIAN_POINT ( 'NONE',  ( 208.2912792141756029, 269.8759169579697641, -2.198672330625011995 ) ) ;
#61678 = ADVANCED_FACE ( 'NONE', ( #87126 ), #79497, .T. ) ;
#61679 = CARTESIAN_POINT ( 'NONE',  ( 154.8833801513861772, 262.3811116602312268, -17.49275566389638215 ) ) ;
#61680 = CARTESIAN_POINT ( 'NONE',  ( 161.8839333999304415, 250.2557977526613229, -13.90128376743482441 ) ) ;
#61681 = FACE_OUTER_BOUND ( 'NONE', #91803, .T. ) ;
#61682 = DIRECTION ( 'NONE',  ( -0.8660254037844377084, -0.5000000000000015543, -0.000000000000000000 ) ) ;
#61684 = CARTESIAN_POINT ( 'NONE',  ( 76.51704343084249160, 51.19216947614988555, 16.04754391915694001 ) ) ;
#61683 = CARTESIAN_POINT ( 'NONE',  ( 73.47333430897622009, 69.87645613598228067, -9.771583980831868743 ) ) ;
#61685 = CARTESIAN_POINT ( 'NONE',  ( 169.1862348568044752, 252.0532904165472701, -8.781961744297172245 ) ) ;
#61686 = CARTESIAN_POINT ( 'NONE',  ( 205.4186965677407954, 274.8513760505354639, -12.35476167499131783 ) ) ;
#61687 = CARTESIAN_POINT ( 'NONE',  ( 195.7617614321055157, 291.5776783508526364, 16.33009124109666033 ) ) ;
#61688 =( BOUNDED_CURVE ( )  B_SPLINE_CURVE ( 2, ( #49539, #11065, #72876, #34345, #96186, #26745, #19173, #50046, #80999 ),
 .UNSPECIFIED., .F., .T. ) 
 B_SPLINE_CURVE_WITH_KNOTS ( ( 3, 2, 2, 2, 3 ),
 ( 0.7459677419354838745, 0.7473118279569892497, 0.7500000000000000000, 0.7526881720430107503, 0.7540322580645161255 ),
 .UNSPECIFIED. ) 
 CURVE ( )  GEOMETRIC_REPRESENTATION_ITEM ( )  RATIONAL_B_SPLINE_CURVE ( ( 0.9330127018922194093, 0.9330127018922194093, 1.000000000000000000, 0.8660254037844387076, 1.000000000000000000, 0.8660254037844387076, 1.000000000000000000, 0.9330127018922194093, 0.9330127018922194093 ) ) 
 REPRESENTATION_ITEM ( '' )  );
#61689 = CARTESIAN_POINT ( 'NONE',  ( 24.36989474801440636, 191.0024278399160949, 9.188101187500095079 ) ) ;
#61690 = CARTESIAN_POINT ( 'NONE',  ( 50.97302584657637681, 209.4244531367911577, -4.594050593750046652 ) ) ;
#61691 = CARTESIAN_POINT ( 'NONE',  ( 163.9845428888737047, 247.2485266795014240, -6.654263628452329549 ) ) ;
#61693 = ADVANCED_FACE ( 'NONE', ( #56645 ), #57634, .T. ) ;
#61692 = CARTESIAN_POINT ( 'NONE',  ( 88.03872450704908204, 44.00635692270125787, 0.5520354079413645199 ) ) ;
#61694 = CARTESIAN_POINT ( 'NONE',  ( 79.43825615163621023, 50.76615999754224617, -14.96098264411816103 ) ) ;
#61695 = CARTESIAN_POINT ( 'NONE',  ( -4.668846022976054222, 158.1115022471902023, -5.000000000000041744 ) ) ;
#61696 = CARTESIAN_POINT ( 'NONE',  ( -22.42236680055709641, 157.8615022471902591, 0.000000000000000000 ) ) ;
#61697 = CARTESIAN_POINT ( 'NONE',  ( 200.1825662459639261, 270.8510622867177631, -11.52056956463778548 ) ) ;
#61698 = CARTESIAN_POINT ( 'NONE',  ( 18.69336236660381090, 32.83396525600390703, -2.839279412974133887 ) ) ;
#61699 = CARTESIAN_POINT ( 'NONE',  ( -5.101858724868275630, 157.8615022471902023, 5.000000000000051514 ) ) ;
#61700 = CARTESIAN_POINT ( 'NONE',  ( 197.0226655822963551, 289.3937282992477549, -17.28982543158101493 ) ) ;
#61701 = CARTESIAN_POINT ( 'NONE',  ( 11.45782370926791849, 18.56628583063839244, 9.188101187500006262 ) ) ;
#61702 = CARTESIAN_POINT ( 'NONE',  ( 54.73473692032376903, 214.6589784336661637, -6.496448406907676862E-16 ) ) ;
#61703 = CARTESIAN_POINT ( 'NONE',  ( 158.6690659153649676, 256.5285302911307781, -16.39959907094835856 ) ) ;
#61704 = CARTESIAN_POINT ( 'NONE',  ( 175.0401671226080680, 292.0372585584420904, 2.009743414037639120 ) ) ;
#61705 = CARTESIAN_POINT ( 'NONE',  ( 159.8416255366773839, 253.7931787365127434, 16.77980437810719394 ) ) ;
#61706 = CARTESIAN_POINT ( 'NONE',  ( 50.52223126882174142, 206.6427522451419065, 10.00000000000009415 ) ) ;
#61707 = CARTESIAN_POINT ( 'NONE',  ( 153.4268044563982301, 264.9039747690200670, 17.87503003910495636 ) ) ;
#61708 = EDGE_CURVE ( 'NONE', #14070, #58863, #12058, .T. ) ;
#61709 = B_SPLINE_CURVE_WITH_KNOTS ( 'NONE', 3,
 ( #30171, #84411, #90537, #14959, #21109, #45847, #13012, #76770, #43871, #7363, #100093, #13502, #51987, #30679 ),
 .UNSPECIFIED., .F., .F.,
 ( 4, 2, 2, 2, 2, 2, 4 ),
 ( 0.001101397475338417335, 0.001342408758887880284, 0.001583420042437343233, 0.001824431325986806181, 0.002065442609536269347, 0.002547465176635195245, 0.003029487743734121143 ),
 .UNSPECIFIED. ) ;
#61710 =( BOUNDED_CURVE ( )  B_SPLINE_CURVE ( 2, ( #45073, #98808, #60750, #28376, #99298, #50673, #81626, #12199, #75001 ),
 .UNSPECIFIED., .F., .T. ) 
 B_SPLINE_CURVE_WITH_KNOTS ( ( 3, 2, 2, 2, 3 ),
 ( 0.7943548387096773800, 0.7956989247311827551, 0.7983870967741935054, 0.8010752688172042557, 0.8024193548387096309 ),
 .UNSPECIFIED. ) 
 CURVE ( )  GEOMETRIC_REPRESENTATION_ITEM ( )  RATIONAL_B_SPLINE_CURVE ( ( 0.9330127018922194093, 0.9330127018922194093, 1.000000000000000000, 0.8660254037844387076, 1.000000000000000000, 0.8660254037844387076, 1.000000000000000000, 0.9330127018922194093, 0.9330127018922194093 ) ) 
 REPRESENTATION_ITEM ( '' )  );
#61711 = ADVANCED_FACE ( 'NONE', ( #81004 ), #57134, .F. ) ;
#61712 = VECTOR ( 'NONE', #9155, 1000.000000000000000 ) ;
#61713 = CARTESIAN_POINT ( 'NONE',  ( 81.39852127369077550, 54.56569132021830626, -15.77998593897333635 ) ) ;
#61714 = CARTESIAN_POINT ( 'NONE',  ( 111.8115707860309556, 225.3615022471902023, 5.000000000000051514 ) ) ;
#61715 = CARTESIAN_POINT ( 'NONE',  ( 198.1847055346428590, 286.9842163890704683, 16.95145238430053070 ) ) ;
#61716 = CARTESIAN_POINT ( 'NONE',  ( 164.9836323268835940, 244.8869617230113249, -2.696511969808454534 ) ) ;
#61717 = ORIENTED_EDGE ( 'NONE', *, *, #65951, .T. ) ;
#61718 = FACE_OUTER_BOUND ( 'NONE', #47066, .T. ) ;
#61719 = DIRECTION ( 'NONE',  ( 0.4999999999999992784, -0.8660254037844390407, 0.000000000000000000 ) ) ;
#61720 = ORIENTED_EDGE ( 'NONE', *, *, #8345, .T. ) ;
#61721 = CARTESIAN_POINT ( 'NONE',  ( 160.0061168334508750, 253.5082714530983026, -16.02306982074888708 ) ) ;
#61722 = CARTESIAN_POINT ( 'NONE',  ( 186.8219716465515603, 276.5816512141889802, -17.20317318536942963 ) ) ;
#61723 = CARTESIAN_POINT ( 'NONE',  ( 69.52010333882432747, 68.86091139190541810, -7.091978748607149718 ) ) ;
#61724 = EDGE_LOOP ( 'NONE', ( #23116, #6855, #76686, #13769 ) ) ;
#61725 = ORIENTED_EDGE ( 'NONE', *, *, #13960, .F. ) ;
#61726 = CARTESIAN_POINT ( 'NONE',  ( 79.23755946070403411, 46.33870301756119403, -12.78202225028572236 ) ) ;
#61727 = CARTESIAN_POINT ( 'NONE',  ( 194.2389208611690492, 294.2153155915419802, -15.75132567904764791 ) ) ;
#61728 = CARTESIAN_POINT ( 'NONE',  ( 57.60966550219797000, 179.2419560658249225, 17.47570218321536473 ) ) ;
#61729 = VERTEX_POINT ( 'NONE', #19178 ) ;
#61730 = CARTESIAN_POINT ( 'NONE',  ( 24.98947064339976265, 26.37878583063841731, 9.188101187500006262 ) ) ;
#61731 = CARTESIAN_POINT ( 'NONE',  ( 74.73487060833782891, 53.69418506457893869, 16.08953207461605928 ) ) ;
#61732 = PLANE ( 'NONE',  #76016 ) ;
#61733 = CARTESIAN_POINT ( 'NONE',  ( 75.26246398335119636, 66.91264289108335106, -12.84364210877655132 ) ) ;
#61734 = B_SPLINE_CURVE_WITH_KNOTS ( 'NONE', 3,
 ( #82480, #67212, #97647, #82959 ),
 .UNSPECIFIED., .F., .F.,
 ( 4, 4 ),
 ( 0.02668887203020185034, 0.03591784413385134406 ),
 .UNSPECIFIED. ) ;
#61735 = VERTEX_POINT ( 'NONE', #42427 ) ;
#61736 = CARTESIAN_POINT ( 'NONE',  ( -2.330697855141256269, 26.52822386297705393, -10.00000000000000000 ) ) ;
#61737 = DIRECTION ( 'NONE',  ( 0.7490285521785712275, -0.6625377181876314081, 0.000000000000000000 ) ) ;
#61738 = ORIENTED_EDGE ( 'NONE', *, *, #65687, .T. ) ;
#61739 = LINE ( 'NONE', #38939, #84809 ) ;
#61740 = EDGE_CURVE ( 'NONE', #98779, #21265, #36834, .T. ) ;
#61742 = CARTESIAN_POINT ( 'NONE',  ( 68.10299200362963745, 65.62433957351714753, -10.27834201520733615 ) ) ;
#61741 = CARTESIAN_POINT ( 'NONE',  ( 71.63504328546106592, 65.51313058377321852, 12.81449884532781702 ) ) ;
#61743 = CARTESIAN_POINT ( 'NONE',  ( 207.6050568035884680, 271.0644890383991310, -1.456818755242089702 ) ) ;
#61744 = CARTESIAN_POINT ( 'NONE',  ( 204.2556901454867955, 276.8657622634082713, 13.61111001399713949 ) ) ;
#61745 = CARTESIAN_POINT ( 'NONE',  ( 159.9628729326222754, 253.5831720864507588, 15.75051413866357386 ) ) ;
#61746 = CARTESIAN_POINT ( 'NONE',  ( 164.3451451116536077, 265.7028218483132491, -17.76432900134729564 ) ) ;
#61747 = CARTESIAN_POINT ( 'NONE',  ( 142.8531688511554307, 253.2833772461660544, -9.188101187500095079 ) ) ;
#61748 = CARTESIAN_POINT ( 'NONE',  ( 177.2332613454938723, 269.3467744458365587, 16.08370027918090628 ) ) ;
#61749 = CARTESIAN_POINT ( 'NONE',  ( 178.7347573768907125, 257.9333752825167494, 9.867161600535267141 ) ) ;
#61750 = CARTESIAN_POINT ( 'NONE',  ( 73.40858323730823543, 219.3149278399160664, 9.188101187500093303 ) ) ;
#61751 = ORIENTED_EDGE ( 'NONE', *, *, #21436, .F. ) ;
#61752 = CARTESIAN_POINT ( 'NONE',  ( 151.2057546125658973, 268.7509459446807227, 15.78031848731319187 ) ) ;
#61753 = CARTESIAN_POINT ( 'NONE',  ( 79.99999999999997158, 26.16025403784438907, 59.99999999999999289 ) ) ;
#61754 = CARTESIAN_POINT ( 'NONE',  ( -19.65312891409030271, 93.06504152958497400, 10.00000000000000888 ) ) ;
#61755 = ORIENTED_EDGE ( 'NONE', *, *, #36832, .T. ) ;
#61756 = CARTESIAN_POINT ( 'NONE',  ( 195.9908276381054009, 291.1809240437640369, -15.88407441854119995 ) ) ;
#61757 = ORIENTED_EDGE ( 'NONE', *, *, #63923, .F. ) ;
#61758 = VERTEX_POINT ( 'NONE', #53026 ) ;
#61759 = CARTESIAN_POINT ( 'NONE',  ( 66.67403404533332889, 67.50885822679623516, 6.470379398463248499 ) ) ;
#61760 = EDGE_CURVE ( 'NONE', #69710, #20188, #35341, .T. ) ;
#61761 = CARTESIAN_POINT ( 'NONE',  ( 197.6456421031980994, 287.3858497455466932, 17.15283754821559015 ) ) ;
#61763 = B_SPLINE_SURFACE_WITH_KNOTS ( 'NONE', 3, 1, ( 
 ( #87423, #62006 ),
 ( #70626, #54923 ),
 ( #94468, #41214 ),
 ( #8335, #25021 ),
 ( #79782, #86390 ),
 ( #78748, #9336 ),
 ( #17431, #46830 ),
 ( #78247, #23510 ),
 ( #85901, #86896 ),
 ( #71154, #233 ),
 ( #17951, #92957 ),
 ( #48339, #32631 ),
 ( #725, #39696 ),
 ( #15924, #8827 ),
 ( #79285, #9858 ),
 ( #62505, #1236 ),
 ( #52675, #80280 ),
 ( #14198, #29399 ),
 ( #72667, #83636 ),
 ( #97453, #96979 ),
 ( #65037, #27548 ),
 ( #18955, #66526 ),
 ( #50818, #43207 ),
 ( #42707, #73156 ),
 ( #64539, #49832 ),
 ( #88399, #95984 ),
 ( #58415, #33650 ),
 ( #57419, #80790 ),
 ( #95498, #72154 ),
 ( #10846, #26048 ),
 ( #11366, #12341 ),
 ( #3261, #42219 ),
 ( #74150, #65526 ),
 ( #88905, #19467 ) ),
 .UNSPECIFIED., .T., .F., .F.,
 ( 4, 2, 2, 2, 2, 2, 2, 2, 2, 2, 2, 2, 2, 2, 2, 2, 4 ),
 ( 2, 2 ),
 ( 0.000000000000000000, 0.06250000000000000000, 0.1250000000000000000, 0.1875000000000000000, 0.2500000000000000000, 0.3125000000000000000, 0.3750000000000000000, 0.4375000000000000000, 0.5000000000000000000, 0.5625000000000000000, 0.6250000000000000000, 0.6875000000000000000, 0.7500000000000000000, 0.8125000000000000000, 0.8750000000000000000, 0.9375000000000000000, 1.000000000000000000 ),
 ( 0.000000000000000000, 1.000000000000000000 ),
 .UNSPECIFIED. ) ;
#61762 = CARTESIAN_POINT ( 'NONE',  ( -74.22192597045216189, 49.22161114575668250, 10.00000000000000000 ) ) ;
#61764 = DIRECTION ( 'NONE',  ( 0.000000000000000000, 0.000000000000000000, 1.000000000000000000 ) ) ;
#61765 = CARTESIAN_POINT ( 'NONE',  ( 155.2695601165254402, 261.7122283397445131, 16.98599069618989077 ) ) ;
#61766 = CARTESIAN_POINT ( 'NONE',  ( 72.01025194461936962, 68.18098373561990400, 10.06619654333739611 ) ) ;
#61767 = CARTESIAN_POINT ( 'NONE',  ( 70.64795371486285092, 223.8464784336661637, 1.353441290958777327E-15 ) ) ;
#61768 = VERTEX_POINT ( 'NONE', #91079 ) ;
#61769 = ORIENTED_EDGE ( 'NONE', *, *, #84009, .T. ) ;
#61770 = CARTESIAN_POINT ( 'NONE',  ( 18.71539827744147644, 26.50829794293879971, -10.00000000000000355 ) ) ;
#61771 = CARTESIAN_POINT ( 'NONE',  ( 161.3988253665112609, 251.0960295137030300, -12.85133671850337223 ) ) ;
#61772 = EDGE_LOOP ( 'NONE', ( #56462, #85660, #15537, #34800 ) ) ;
#61773 = CARTESIAN_POINT ( 'NONE',  ( 15.24912932961584744, 31.73705186507753950, -3.090169943749475845 ) ) ;
#61774 = B_SPLINE_CURVE_WITH_KNOTS ( 'NONE', 3,
 ( #46978, #77897, #39846, #1393 ),
 .UNSPECIFIED., .F., .F.,
 ( 4, 4 ),
 ( 0.004106122421884165000, 0.008436222502574928020 ),
 .UNSPECIFIED. ) ;
#61775 = CARTESIAN_POINT ( 'NONE',  ( 75.75493378409400691, 65.86437009324527025, -14.07593894684413449 ) ) ;
#61776 = EDGE_CURVE ( 'NONE', #76998, #83448, #35144, .T. ) ;
#61777 = CARTESIAN_POINT ( 'NONE',  ( 187.7317787694285869, 273.6764366694279147, -17.17214744287320372 ) ) ;
#61778 = CARTESIAN_POINT ( 'NONE',  ( 181.4204268205617154, 259.5203828285251006, -11.17471347674236348 ) ) ;
#61779 = DIRECTION ( 'NONE',  ( -0.000000000000000000, 0.000000000000000000, -1.000000000000000000 ) ) ;
#61780 = VERTEX_POINT ( 'NONE', #59620 ) ;
#61781 = CARTESIAN_POINT ( 'NONE',  ( 83.93224464401249918, 43.69151124717017609, -7.184054031788095429 ) ) ;
#61782 = CARTESIAN_POINT ( 'NONE',  ( 32.74284248606149106, 41.83705186507756224, 3.090169943749475401 ) ) ;
#61783 = CARTESIAN_POINT ( 'NONE',  ( 147.9810571718830658, 275.4328967230283070, -5.053263300117055934 ) ) ;
#61784 = CARTESIAN_POINT ( 'NONE',  ( 200.9812045408918380, 282.5373376992193926, -16.61165062382494284 ) ) ;
#61785 = CARTESIAN_POINT ( 'NONE',  ( 79.37421766178685800, 59.09322915855462099, -16.22839383466721230 ) ) ;
#61786 = CARTESIAN_POINT ( 'NONE',  ( 71.77304829242562789, 67.17973620888965058, -10.95076504957269314 ) ) ;
#61787 = EDGE_LOOP ( 'NONE', ( #77461, #87032, #71176, #20092 ) ) ;
#61788 = CARTESIAN_POINT ( 'NONE',  ( 195.9804492347847997, 265.5343886315737905, 4.427495290768495018 ) ) ;
#61789 = DIRECTION ( 'NONE',  ( -0.000000000000000000, -0.000000000000000000, 1.000000000000000000 ) ) ;
#61790 = CARTESIAN_POINT ( 'NONE',  ( 2.672015980952107572, 183.8967562850347122, -4.648177544792955347E-16 ) ) ;
#61791 = DIRECTION ( 'NONE',  ( -2.816764622163176506E-16, -1.626259812849726698E-16, 1.000000000000000000 ) ) ;
#61792 = CARTESIAN_POINT ( 'NONE',  ( 83.43509040966195300, 52.41314640276721804, 14.83374206111990468 ) ) ;
#61793 = DIRECTION ( 'NONE',  ( 0.000000000000000000, -0.000000000000000000, 1.000000000000000000 ) ) ;
#61794 = VERTEX_POINT ( 'NONE', #82981 ) ;
#61795 = CARTESIAN_POINT ( 'NONE',  ( 167.4391039490435844, 267.1861514467046845, 17.82254523450562900 ) ) ;
#61796 = CARTESIAN_POINT ( 'NONE',  ( 202.3139361598622372, 280.2289788223093865, 15.93832709035092421 ) ) ;
#61797 = CARTESIAN_POINT ( 'NONE',  ( 161.2535912560966551, 263.0844709175967182, -17.80682751047658030 ) ) ;
#61799 = CARTESIAN_POINT ( 'NONE',  ( 74.02712935233476799, 55.22068333997034983, 16.12340877065539502 ) ) ;
#61798 = CARTESIAN_POINT ( 'NONE',  ( 194.5051734451974426, 293.7541525883582381, 14.61790433731063921 ) ) ;
#61800 = CARTESIAN_POINT ( 'NONE',  ( 21.98544502579644799, 24.64441083166261137, -10.00000000000000533 ) ) ;
#61801 = CARTESIAN_POINT ( 'NONE',  ( 28.21411888609903684, 175.5494855054051584, -2.679491924311248496 ) ) ;
#61802 = CARTESIAN_POINT ( 'NONE',  ( 166.5910668850809486, 286.3200580136348208, -3.227223869863532713 ) ) ;
#61803 = CARTESIAN_POINT ( 'NONE',  ( -19.65312891409030271, 93.06504152958497400, -10.00000000000000888 ) ) ;
#61804 = DIRECTION ( 'NONE',  ( 0.4999999999999998890, -0.8660254037844385966, 0.000000000000000000 ) ) ;
#61805 = CARTESIAN_POINT ( 'NONE',  ( 152.3523849971420532, 248.7677522451417929, -5.000000000000041744 ) ) ;
#61806 = CARTESIAN_POINT ( 'NONE',  ( 150.5287101026835330, 271.9236214347867531, -12.89083132144543775 ) ) ;
#61807 = ORIENTED_EDGE ( 'NONE', *, *, #37610, .T. ) ;
#61808 = CARTESIAN_POINT ( 'NONE',  ( 66.92722021384717834, 67.66083605152657299, -6.453759971695879116 ) ) ;
#61809 = CARTESIAN_POINT ( 'NONE',  ( 72.67106054446415442, 70.72958228892088073, -7.972900045040099748 ) ) ;
#61810 = PLANE ( 'NONE',  #90647 ) ;
#61811 = CARTESIAN_POINT ( 'NONE',  ( 23.96437920969670898, 175.4548013555409796, -4.594050593750042211 ) ) ;
#61812 = CARTESIAN_POINT ( 'NONE',  ( 75.37455147550954848, 53.49333803353913197, 16.03970701519320841 ) ) ;
#61813 = CARTESIAN_POINT ( 'NONE',  ( 36.60665582185911404, 20.94473085651394584, 1.475505719884397138E-15 ) ) ;
#61814 = CARTESIAN_POINT ( 'NONE',  ( 77.91581387522141711, 57.42368465423609791, 16.60724471479637998 ) ) ;
#61815 = LINE ( 'NONE', #29439, #56033 ) ;
#61816 = CARTESIAN_POINT ( 'NONE',  ( 82.61787247804464585, 43.35655690195848422, 8.757983355685475146 ) ) ;
#61817 = CARTESIAN_POINT ( 'NONE',  ( 188.6570295601639771, 259.3016035056324426, -0.8096508949806298094 ) ) ;
#61818 = EDGE_CURVE ( 'NONE', #33225, #37254, #12190, .T. ) ;
#61819 = EDGE_CURVE ( 'NONE', #16529, #82623, #52526, .T. ) ;
#61820 = CARTESIAN_POINT ( 'NONE',  ( 64.25234236153544032, 221.2365022471903444, 2.944929066748280225E-16 ) ) ;
#61821 = CARTESIAN_POINT ( 'NONE',  ( 82.35975313173908319, 41.41624149291902057, 5.521678208619409389 ) ) ;
#61822 = DIRECTION ( 'NONE',  ( -0.8660254037844387076, -0.4999999999999998890, -0.000000000000000000 ) ) ;
#61823 = ADVANCED_FACE ( 'NONE', ( #68224 ), #4960, .T. ) ;
#61824 = CARTESIAN_POINT ( 'NONE',  ( 31.35205101814392847, 201.1589784336661353, -6.496448406907675876E-16 ) ) ;
#61825 = CARTESIAN_POINT ( 'NONE',  ( 49.51900556837681222, 105.3795262313705763, -10.00000000000000000 ) ) ;
#61826 = EDGE_CURVE ( 'NONE', #57520, #46269, #99318, .T. ) ;
#61827 = CARTESIAN_POINT ( 'NONE',  ( 27.76637506322961002, 39.52903772873361277, -1.583844403245329602 ) ) ;
#61828 = CARTESIAN_POINT ( 'NONE',  ( 206.2026304802515142, 271.4126985892297057, -6.607972036968888574 ) ) ;
#61829 = B_SPLINE_CURVE_WITH_KNOTS ( 'NONE', 3,
 ( #42184, #98902, #59872, #60357, #99398, #6685, #52277, #75595, #5683, #58379, #20913, #51275, #89355, #45173, #68470, #51800, #90337, #97414, #52762, #37561, #27982, #29484, #76111, #5194, #13782, #74109, #44169, #36572, #83724, #89830, #19908 ),
 .UNSPECIFIED., .F., .F.,
 ( 4, 3, 3, 3, 3, 3, 3, 3, 3, 3, 4 ),
 ( 0.000000000000000000, 0.1333490885032447282, 0.3007194338854389248, 0.4699862290245251373, 0.5844252810809574816, 0.6686540514502947730, 0.7354980260655736846, 0.8028463152565851191, 0.8633854507757401375, 0.9437142632667373521, 1.000000000000000000 ),
 .UNSPECIFIED. ) ;
#61830 = CARTESIAN_POINT ( 'NONE',  ( 206.9942764641839688, 270.1223916185117560, -3.431663675821580828 ) ) ;
#61831 = FACE_OUTER_BOUND ( 'NONE', #44847, .T. ) ;
#61832 = CARTESIAN_POINT ( 'NONE',  ( 194.1493756275458793, 294.3704124857528655, 13.94613522129020744 ) ) ;
#61833 = FACE_OUTER_BOUND ( 'NONE', #76984, .T. ) ;
#61834 = CARTESIAN_POINT ( 'NONE',  ( 202.5562236059581664, 279.2319112406736963, -15.43681043966012290 ) ) ;
#61835 = B_SPLINE_CURVE_WITH_KNOTS ( 'NONE', 3,
 ( #84150, #36495, #68390, #22798, #75514, #36995, #14696, #13706, #30393, #98824, #76029, #67398, #6099, #35993, #51720, #5113, #29405, #28915, #98323, #76507, #37479, #91731, #99808, #91231, #92248, #52682, #22295, #53677, #7088, #83644, #61285 ),
 .UNSPECIFIED., .F., .F.,
 ( 4, 3, 3, 3, 3, 3, 3, 3, 3, 3, 4 ),
 ( 0.000000000000000000, 0.1333490885032314888, 0.3007194338854323190, 0.4699862290245113150, 0.5844252810809227316, 0.6686540514502676835, 0.7354980260655422653, 0.8028463152565505911, 0.8633854507757149355, 0.9437142632667404607, 1.000000000000000000 ),
 .UNSPECIFIED. ) ;
#61836 = CARTESIAN_POINT ( 'NONE',  ( 200.1133476818314705, 272.1141633677412415, 12.87458617912082914 ) ) ;
#61837 = CARTESIAN_POINT ( 'NONE',  ( 15.27916758686040488, 29.79752408145592568, -5.678558825948271327 ) ) ;
#61838 = CARTESIAN_POINT ( 'NONE',  ( 189.8314329296643450, 301.8493086226544619, -0.8085564604676659384 ) ) ;
#61839 = CARTESIAN_POINT ( 'NONE',  ( 71.55582279638187515, 59.08747183676958770, 15.32285513291258283 ) ) ;
#61840 = CARTESIAN_POINT ( 'NONE',  ( 187.3962380822248406, 269.0893220905305157, -14.11458629364903672 ) ) ;
#61841 = ORIENTED_EDGE ( 'NONE', *, *, #46025, .F. ) ;
#61842 = FACE_OUTER_BOUND ( 'NONE', #79892, .T. ) ;
#61843 = FACE_OUTER_BOUND ( 'NONE', #969, .T. ) ;
#61844 = CARTESIAN_POINT ( 'NONE',  ( 193.6564271169084464, 262.6014873983580742, -4.146719891036213745 ) ) ;
#61845 = CARTESIAN_POINT ( 'NONE',  ( 81.80089866349948124, 42.11013410072107632, 7.569077868460975189 ) ) ;
#61846 = ORIENTED_EDGE ( 'NONE', *, *, #75091, .T. ) ;
#61847 = CARTESIAN_POINT ( 'NONE',  ( 161.8882824960653579, 250.2482648971885340, -13.83574485983625557 ) ) ;
#61848 = CARTESIAN_POINT ( 'NONE',  ( 72.57160893180984829, 71.52012305816319326, -5.479963803933916466 ) ) ;
#61849 = DIRECTION ( 'NONE',  ( -1.000000000000000000, 0.000000000000000000, 0.000000000000000000 ) ) ;
#61850 = CARTESIAN_POINT ( 'NONE',  ( 181.1761209317502335, 257.6610458391679117, -7.556567974831167156 ) ) ;
#61851 = ORIENTED_EDGE ( 'NONE', *, *, #38899, .F. ) ;
#61852 = ORIENTED_EDGE ( 'NONE', *, *, #22167, .F. ) ;
#61854 = CARTESIAN_POINT ( 'NONE',  ( 85.96141273360541391, 43.06913367483099364, -2.383719173196181540 ) ) ;
#61853 = CYLINDRICAL_SURFACE ( 'NONE', #38938, 17.82106496071139645 ) ;
#61855 = EDGE_LOOP ( 'NONE', ( #46759, #88374, #3713, #20025 ) ) ;
#61856 = CARTESIAN_POINT ( 'NONE',  ( 201.2949053258274148, 281.9939920013367782, -18.04004790210578335 ) ) ;
#61857 = CARTESIAN_POINT ( 'NONE',  ( 31.41726478770819853, 19.10801979619930435, 3.090169943749476733 ) ) ;
#61858 = FACE_OUTER_BOUND ( 'NONE', #98759, .T. ) ;
#61859 = LINE ( 'NONE', #30970, #32152 ) ;
#61860 = VERTEX_POINT ( 'NONE', #98164 ) ;
#61861 = CARTESIAN_POINT ( 'NONE',  ( 148.4049257185216106, 273.6021238924720365, 8.639190357831699529 ) ) ;
#61862 = EDGE_LOOP ( 'NONE', ( #50423, #73000, #76241, #51833 ) ) ;
#61863 = CARTESIAN_POINT ( 'NONE',  ( 81.77599116216271113, 59.08414711118528118, -0.4951340343707851255 ) ) ;
#61864 = CARTESIAN_POINT ( 'NONE',  ( 161.9954662403825978, 266.8975016676487826, 16.59001395411891266 ) ) ;
#61865 = ORIENTED_EDGE ( 'NONE', *, *, #86171, .T. ) ;
#61866 = CARTESIAN_POINT ( 'NONE',  ( 24.28583178621855865, 34.99752408145591431, 5.678558825948277544 ) ) ;
#61867 = CARTESIAN_POINT ( 'NONE',  ( 190.6094661480870798, 300.5017155583701083, 4.598210453186021951 ) ) ;
#61868 = CARTESIAN_POINT ( 'NONE',  ( 78.14698338385944965, 47.61700244333332677, -13.90103454460489019 ) ) ;
#61869 = ORIENTED_EDGE ( 'NONE', *, *, #76233, .T. ) ;
#61870 = CARTESIAN_POINT ( 'NONE',  ( -4.866515740870070772, 77.03598506094434128, 14.21757578985110193 ) ) ;
#61871 = CARTESIAN_POINT ( 'NONE',  ( 150.6533415055477008, 269.7077535128032082, 14.84621632544246062 ) ) ;
#61872 = CARTESIAN_POINT ( 'NONE',  ( -50.36082798260552806, 30.16005589317048674, -10.00000000000000000 ) ) ;
#61873 = CARTESIAN_POINT ( 'NONE',  ( 39.22461576370143632, 27.81029122506297568, 8.090169943749479842 ) ) ;
#61874 = ORIENTED_EDGE ( 'NONE', *, *, #16607, .T. ) ;
#61875 = ORIENTED_EDGE ( 'NONE', *, *, #3648, .F. ) ;
#61876 = FACE_OUTER_BOUND ( 'NONE', #13361, .T. ) ;
#61877 = CARTESIAN_POINT ( 'NONE',  ( -32.04500338604974985, 25.44370296803430520, -10.00000000000000000 ) ) ;
#61878 = CARTESIAN_POINT ( 'NONE',  ( 82.31027433114240921, 53.67166805628564674, 15.82896004337745133 ) ) ;
#61879 = CARTESIAN_POINT ( 'NONE',  ( 190.0550686570564949, 301.4619601804237732, 4.203010638620038542 ) ) ;
#61880 = CARTESIAN_POINT ( 'NONE',  ( 173.9176872785688204, 276.9430746053678263, -15.64548591645994335 ) ) ;
#61881 = CARTESIAN_POINT ( 'NONE',  ( 146.5457113009716466, 276.8223777258335758, 0.3536082318825463644 ) ) ;
#61882 = CARTESIAN_POINT ( 'NONE',  ( 147.0314375879888757, 275.9810751181479986, -5.168577011192616588 ) ) ;
#61883 = EDGE_CURVE ( 'NONE', #93683, #32652, #28743, .T. ) ;
#61884 = CARTESIAN_POINT ( 'NONE',  ( 163.4732498979778086, 257.8043807661392179, 15.53864332294564043 ) ) ;
#61885 = EDGE_CURVE ( 'NONE', #47421, #90587, #52011, .T. ) ;
#61886 = AXIS2_PLACEMENT_3D ( 'NONE', #80849, #73207, #41271 ) ;
#61887 = CARTESIAN_POINT ( 'NONE',  ( 69.47271657258438893, 66.54530737956719122, 10.18805627866735009 ) ) ;
#61888 = AXIS2_PLACEMENT_3D ( 'NONE', #48259, #78675, #72076 ) ;
#61889 = CARTESIAN_POINT ( 'NONE',  ( 91.45997379709659469, 223.6115022471902307, 10.00000000000009592 ) ) ;
#61890 = CARTESIAN_POINT ( 'NONE',  ( 75.70701541337017204, 65.59976764996046938, 13.80433314997810967 ) ) ;
#61891 = CARTESIAN_POINT ( 'NONE',  ( 70.72212250024647062, 65.42481974022895486, -11.87866371874642724 ) ) ;
#61892 = CARTESIAN_POINT ( 'NONE',  ( 78.11787979767646561, 47.76729556080021410, 13.98403596371365687 ) ) ;
#61893 = CARTESIAN_POINT ( 'NONE',  ( 103.8820256808556906, 230.7833772461660544, -9.188101187500095079 ) ) ;
#61894 = VERTEX_POINT ( 'NONE', #38816 ) ;
#61895 = CARTESIAN_POINT ( 'NONE',  ( 147.0721334091522294, 275.9105878882373304, 0.7242168585908188572 ) ) ;
#61896 = CARTESIAN_POINT ( 'NONE',  ( 84.25586279892151254, 41.93059359979653777, -0.3096221969905373905 ) ) ;
#61897 = CARTESIAN_POINT ( 'NONE',  ( -21.43592214265774132, 59.87855815223608147, -10.00000000000000000 ) ) ;
#61898 = VECTOR ( 'NONE', #90451, 1000.000000000000000 ) ;
#61899 = CARTESIAN_POINT ( 'NONE',  ( 154.8545429534089237, 262.4310591522755089, -17.81746354318405778 ) ) ;
#61900 = CARTESIAN_POINT ( 'NONE',  ( 181.7937950796055588, 283.7749071970079626, -15.03297549846545778 ) ) ;
#61901 = CARTESIAN_POINT ( 'NONE',  ( 189.8106237464670585, 301.8853511852161091, -0.6577604834569344971 ) ) ;
#61902 = CARTESIAN_POINT ( 'NONE',  ( 165.3728640525272340, 283.7448754721146429, -8.387219889811008855 ) ) ;
#61903 = ORIENTED_EDGE ( 'NONE', *, *, #98217, .F. ) ;
#61904 = CARTESIAN_POINT ( 'NONE',  ( 207.6523394534040392, 270.9825930866021508, -2.115019688068903392 ) ) ;
#61906 = EDGE_CURVE ( 'NONE', #346, #65763, #10941, .T. ) ;
#61905 = CARTESIAN_POINT ( 'NONE',  ( 72.50757856258960032, 71.58588072324644713, 5.252804842291221021 ) ) ;
#61907 = CARTESIAN_POINT ( 'NONE',  ( 53.62548896571606605, 191.7677522451418213, -5.000000000000041744 ) ) ;
#61908 = CARTESIAN_POINT ( 'NONE',  ( 129.3758220526426044, 239.3768266524159856, -9.188101187500093303 ) ) ;
#61909 = CARTESIAN_POINT ( 'NONE',  ( 150.6438662863770332, 269.7241650738195631, -14.92510732909997628 ) ) ;
#61910 = VECTOR ( 'NONE', #2635, 1000.000000000000000 ) ;
#61911 = CARTESIAN_POINT ( 'NONE',  ( 164.7396270603856294, 269.0037874151494179, 17.61975801440670608 ) ) ;
#61912 = CARTESIAN_POINT ( 'NONE',  ( 196.1241105319816143, 290.9500712997905794, 15.97146679939154268 ) ) ;
#61913 = CARTESIAN_POINT ( 'NONE',  ( 45.14796862286864609, 185.3262482093457493, 3.021315404115420679E-15 ) ) ;
#61914 = CARTESIAN_POINT ( 'NONE',  ( 50.56751030825869009, 193.8768266524160140, 9.188101187500098632 ) ) ;
#61915 = CARTESIAN_POINT ( 'NONE',  ( 85.73738684536749588, 48.47886545727438801, -11.76341085017970656 ) ) ;
#61916 = ORIENTED_EDGE ( 'NONE', *, *, #82743, .F. ) ;
#61917 = CARTESIAN_POINT ( 'NONE',  ( 71.54181076156694985, 65.04745795580406309, 12.54713244084793722 ) ) ;
#61918 = DIRECTION ( 'NONE',  ( 0.000000000000000000, 0.000000000000000000, 1.000000000000000000 ) ) ;
#61919 = FACE_OUTER_BOUND ( 'NONE', #9710, .T. ) ;
#61920 = CARTESIAN_POINT ( 'NONE',  ( 147.5848197185516142, 275.0225891520124151, 4.420251097676741736 ) ) ;
#61921 = CARTESIAN_POINT ( 'NONE',  ( 81.93905738806562056, 41.80096582289180418, -5.620942555805415353 ) ) ;
#61922 = CARTESIAN_POINT ( 'NONE',  ( 152.8642676789094423, 276.0723602830860273, -10.03519574156767469 ) ) ;
#61923 = CARTESIAN_POINT ( 'NONE',  ( 178.5937152032327333, 260.7852093525231680, 13.58383975110821673 ) ) ;
#61924 = CARTESIAN_POINT ( 'NONE',  ( 99.16399144804771026, 241.3927522451419634, 2.944929066748280225E-16 ) ) ;
#61925 = CARTESIAN_POINT ( 'NONE',  ( 15.13540196134234606, 32.23654200823202132, 1.583844403245363353 ) ) ;
#61926 = ORIENTED_EDGE ( 'NONE', *, *, #69640, .T. ) ;
#61927 = CARTESIAN_POINT ( 'NONE',  ( 189.8480911035503880, 301.8204558191226283, -0.8992086515915015399 ) ) ;
#61928 = CARTESIAN_POINT ( 'NONE',  ( 163.4178923001155681, 247.5989030008181260, -10.38047187240561442 ) ) ;
#61929 = CARTESIAN_POINT ( 'NONE',  ( 22.04262502322622908, 183.5333772461660544, 9.188101187500095079 ) ) ;
#61930 = CARTESIAN_POINT ( 'NONE',  ( 8.751641773298651117, 23.79103043416547081, 8.090169943749478065 ) ) ;
#61931 = CARTESIAN_POINT ( 'NONE',  ( 194.8387898011405355, 273.2648853755486016, 14.40873911934531648 ) ) ;
#61932 = CARTESIAN_POINT ( 'NONE',  ( 35.60133525300030755, 191.3615022471902591, -10.00000000000009592 ) ) ;
#61933 = CARTESIAN_POINT ( 'NONE',  ( 73.03023235113748513, 69.68176590430279305, 9.698330045464274463 ) ) ;
#61935 = CARTESIAN_POINT ( 'NONE',  ( 67.67116493723634107, 216.0024278399160664, -9.188101187500093303 ) ) ;
#61934 = CARTESIAN_POINT ( 'NONE',  ( 174.9526703860257726, 286.4149860108961434, 10.48728481691800773 ) ) ;
#61936 = CARTESIAN_POINT ( 'NONE',  ( 161.1611771195837548, 251.5076483517112536, 14.17749514252127163 ) ) ;
#61937 = CARTESIAN_POINT ( 'NONE',  ( 73.12850034369863295, 57.37224303518116386, 15.89072477728744381 ) ) ;
#61938 = CARTESIAN_POINT ( 'NONE',  ( -29.35927996735550494, 95.14472354011699906, 44.59528332425108488 ) ) ;
#61939 = CARTESIAN_POINT ( 'NONE',  ( 8.162811221194553823, 28.21091486745858745, -1.111400068045478839E-16 ) ) ;
#61940 = VERTEX_POINT ( 'NONE', #23115 ) ;
#61941 = CARTESIAN_POINT ( 'NONE',  ( 165.4470874010085026, 269.3013239833477996, 16.98587756655855330 ) ) ;
#61942 = CARTESIAN_POINT ( 'NONE',  ( 30.40518283029366842, 188.3615022471902591, -10.00000000000009592 ) ) ;
#61943 = CARTESIAN_POINT ( 'NONE',  ( 163.8398374448017591, 246.8680725722146008, -5.948785025486735378 ) ) ;
#61944 = CARTESIAN_POINT ( 'NONE',  ( 1.691375130056927079, 159.5327760586659451, 1.948934522072303157E-15 ) ) ;
#61945 = CARTESIAN_POINT ( 'NONE',  ( 29.46033357383057449, 37.98502408145594700, -5.678558825948271327 ) ) ;
#61946 = CARTESIAN_POINT ( 'NONE',  ( -19.65312891409030271, 93.06504152958497400, 10.00000000000000888 ) ) ;
#61947 = EDGE_CURVE ( 'NONE', #72615, #71188, #80951, .T. ) ;
#61948 = CARTESIAN_POINT ( 'NONE',  ( 185.4642089758430927, 260.0334125403911685, 7.310543569370538286 ) ) ;
#61949 = CARTESIAN_POINT ( 'NONE',  ( 205.7867067512454184, 274.2139637150027056, 10.62737868262404106 ) ) ;
#61950 = CARTESIAN_POINT ( 'NONE',  ( 88.47364309043327069, 44.01569472767099711, 2.145854971186520466 ) ) ;
#61951 = CARTESIAN_POINT ( 'NONE',  ( 66.12980561864134188, 68.57555640412795128, 2.249234565191243540 ) ) ;
#61952 = ORIENTED_EDGE ( 'NONE', *, *, #72713, .F. ) ;
#61953 = B_SPLINE_CURVE_WITH_KNOTS ( 'NONE', 3,
 ( #39970, #70905, #23787, #1514 ),
 .UNSPECIFIED., .F., .F.,
 ( 4, 4 ),
 ( 0.03743099264120831882, 0.04603662255807886017 ),
 .UNSPECIFIED. ) ;
#61954 = CARTESIAN_POINT ( 'NONE',  ( 164.1303272795579176, 246.3649294193346009, 8.276858000922496572 ) ) ;
#61955 = CARTESIAN_POINT ( 'NONE',  ( -27.52599651137550651, 146.7012482093459198, -37.49999999999995737 ) ) ;
#61956 = DIRECTION ( 'NONE',  ( -0.1580495287025880657, -0.9874311856918890351, 0.000000000000000000 ) ) ;
#61957 = CARTESIAN_POINT ( 'NONE',  ( 17.90548643172614263, 12.19860640527291373, 2.839279412974134775 ) ) ;
#61958 = ORIENTED_EDGE ( 'NONE', *, *, #89686, .F. ) ;
#61959 = CARTESIAN_POINT ( 'NONE',  ( 160.0298054686767557, 253.4672415333249376, 14.79725849075877520 ) ) ;
#61960 = CARTESIAN_POINT ( 'NONE',  ( 79.99999999999998579, 20.00000000000000000, 59.99999999999999289 ) ) ;
#61961 = CARTESIAN_POINT ( 'NONE',  ( -61.08640853961129835, 36.64444830801922848, 177.5919119679930134 ) ) ;
#61962 = CARTESIAN_POINT ( 'NONE',  ( 178.6603775665675187, 266.7231829388173878, 16.69313589097744455 ) ) ;
#61963 = CARTESIAN_POINT ( 'NONE',  ( 207.8446715390582540, 270.6494641423232679, -2.429516028743652800 ) ) ;
#61964 = CARTESIAN_POINT ( 'NONE',  ( 152.9251141908703175, 265.7729277985770864, -16.20110192949203309 ) ) ;
#61965 = VERTEX_POINT ( 'NONE', #45906 ) ;
#61966 = ORIENTED_EDGE ( 'NONE', *, *, #81441, .T. ) ;
#61967 = CARTESIAN_POINT ( 'NONE',  ( 190.8154370666929367, 280.9968047295526503, 16.65367678528672002 ) ) ;
#61968 = CARTESIAN_POINT ( 'NONE',  ( 151.3011447763744570, 269.1990464485573966, 14.21186556778774168 ) ) ;
#61969 = VERTEX_POINT ( 'NONE', #54007 ) ;
#61970 = CARTESIAN_POINT ( 'NONE',  ( 71.38434165879655779, 70.64309506879222056, 6.834342629426365612 ) ) ;
#61971 = CARTESIAN_POINT ( 'NONE',  ( 85.74237854190519670, 45.04157437062109182, -7.829273241313135401 ) ) ;
#61972 = EDGE_LOOP ( 'NONE', ( #5539, #51144 ) ) ;
#61973 = CARTESIAN_POINT ( 'NONE',  ( 191.4082244002820516, 299.1182256826033949, -8.271837126846561361 ) ) ;
#61974 = CARTESIAN_POINT ( 'NONE',  ( 79.50784967658378832, 59.51503684596524124, -16.19812362877713596 ) ) ;
#61975 = VECTOR ( 'NONE', #66099, 1000.000000000000000 ) ;
#61976 = LINE ( 'NONE', #69598, #91796 ) ;
#61977 = CARTESIAN_POINT ( 'NONE',  ( 69.87354030794955406, 62.76892477261478120, 13.90980553379283968 ) ) ;
#61978 = ORIENTED_EDGE ( 'NONE', *, *, #68316, .T. ) ;
#61979 = CARTESIAN_POINT ( 'NONE',  ( 161.1238074876215478, 251.5723744529297505, 13.42537408252843179 ) ) ;
#61980 = CARTESIAN_POINT ( 'NONE',  ( 191.5451565139252068, 298.8810523045859213, 7.782291334092181323 ) ) ;
#61981 = CARTESIAN_POINT ( 'NONE',  ( 170.6653991834546389, 280.1030447246535005, -15.19489322104400664 ) ) ;
#61982 = B_SPLINE_SURFACE_WITH_KNOTS ( 'NONE', 3, 1, ( 
 ( #60980, #91945 ),
 ( #22496, #17389 ),
 ( #55862, #56386 ),
 ( #80239, #26506 ),
 ( #48809, #48301 ),
 ( #64499, #47773 ),
 ( #73118, #2213 ),
 ( #33603, #88358 ),
 ( #95459, #71617 ),
 ( #96437, #32595 ),
 ( #2716, #26011 ),
 ( #34110, #24984 ),
 ( #18917, #72624 ),
 ( #63493, #63990 ),
 ( #57384, #56882 ),
 ( #79742, #86354 ),
 ( #3225, #49302 ),
 ( #49790, #87865 ),
 ( #33094, #79246 ),
 ( #94431, #9818 ),
 ( #18411, #40679 ),
 ( #86857, #78711 ),
 ( #65002, #10304 ),
 ( #94932, #27001 ),
 ( #95945, #80753 ),
 ( #10806, #72112 ),
 ( #11324, #87382 ),
 ( #42182, #40173 ),
 ( #1713, #25493 ),
 ( #41679, #17911 ),
 ( #41176, #3709 ) ),
 .UNSPECIFIED., .F., .F., .F.,
 ( 4, 3, 3, 3, 3, 3, 3, 3, 3, 3, 4 ),
 ( 2, 2 ),
 ( 0.000000000000000000, 0.1333490885032306283, 0.3007194338854234927, 0.4699862290244963270, 0.5844252810809187348, 0.6686540514502645749, 0.7354980260655307189, 0.8028463152565288308, 0.8633854507756889562, 0.9437142632666959408, 1.000000000000000000 ),
 ( 0.000000000000000000, 1.000000000000000000 ),
 .UNSPECIFIED. ) ;
#61983 = ORIENTED_EDGE ( 'NONE', *, *, #73005, .F. ) ;
#61984 = ORIENTED_EDGE ( 'NONE', *, *, #77782, .F. ) ;
#61985 = ORIENTED_EDGE ( 'NONE', *, *, #61524, .T. ) ;
#61986 = CARTESIAN_POINT ( 'NONE',  ( 160.0205417486836836, 268.7952604174922158, -17.12082356920033277 ) ) ;
#61987 = EDGE_LOOP ( 'NONE', ( #31558, #33670, #10129 ) ) ;
#61988 = CARTESIAN_POINT ( 'NONE',  ( 70.71203917888955459, 71.32383586654306384, 2.333515263935871609 ) ) ;
#61989 = EDGE_LOOP ( 'NONE', ( #57654, #87421, #41599, #57019 ) ) ;
#61990 = CARTESIAN_POINT ( 'NONE',  ( 207.6471633721571379, 270.9915583223058206, 2.196965492132801678 ) ) ;
#61991 =( BOUNDED_CURVE ( )  B_SPLINE_CURVE ( 2, ( #48821, #89725, #96824, #82630, #66374, #27873, #20286, #58269, #13191 ),
 .UNSPECIFIED., .F., .T. ) 
 B_SPLINE_CURVE_WITH_KNOTS ( ( 3, 2, 2, 2, 3 ),
 ( 0.8104838709677418818, 0.8118279569892472569, 0.8145161290322581182, 0.8172043010752688685, 0.8185483870967742437 ),
 .UNSPECIFIED. ) 
 CURVE ( )  GEOMETRIC_REPRESENTATION_ITEM ( )  RATIONAL_B_SPLINE_CURVE ( ( 0.9330127018922194093, 0.9330127018922194093, 1.000000000000000000, 0.8660254037844387076, 1.000000000000000000, 0.8660254037844387076, 1.000000000000000000, 0.9330127018922194093, 0.9330127018922194093 ) ) 
 REPRESENTATION_ITEM ( '' )  );
#61992 = CARTESIAN_POINT ( 'NONE',  ( 81.93576472774982733, 45.45616636752174600, 10.86207910360908180 ) ) ;
#61993 = CARTESIAN_POINT ( 'NONE',  ( 165.0763782876348955, 271.0110069803866963, 16.91995621439599162 ) ) ;
#61994 = CARTESIAN_POINT ( 'NONE',  ( 167.6829735571818674, 281.1103996008106378, 11.56255526439067260 ) ) ;
#61995 = CARTESIAN_POINT ( 'NONE',  ( 148.1632261683078013, 274.0207597936089883, -7.853210555358286271 ) ) ;
#61996 = CARTESIAN_POINT ( 'NONE',  ( 69.46089132522230614, 68.43734353126103542, -7.767842414235587079 ) ) ;
#61997 = CARTESIAN_POINT ( 'NONE',  ( 197.6146187704118802, 288.3684353017289936, -18.03711460092097241 ) ) ;
#61998 = ORIENTED_EDGE ( 'NONE', *, *, #56609, .T. ) ;
#61999 = CARTESIAN_POINT ( 'NONE',  ( 202.1660481100201423, 271.6014475893761073, -11.28653549010346246 ) ) ;
#62000 = CARTESIAN_POINT ( 'NONE',  ( 19.20273687360401027, 16.80170272979925628, 7.433330006724137462 ) ) ;
#62001 = EDGE_CURVE ( 'NONE', #8790, #81989, #61498, .T. ) ;
#62002 = CARTESIAN_POINT ( 'NONE',  ( 198.5695182982529730, 276.9374223074942165, -15.29489990819768686 ) ) ;
#62003 = CARTESIAN_POINT ( 'NONE',  ( 185.6299035038124430, 291.5639447024825586, -13.39789161462089773 ) ) ;
#62005 = ORIENTED_EDGE ( 'NONE', *, *, #67686, .F. ) ;
#62004 = CARTESIAN_POINT ( 'NONE',  ( 206.8218526254527490, 270.5579068801799849, 5.033309423535771820 ) ) ;
#62006 = CARTESIAN_POINT ( 'NONE',  ( 146.6807985088175030, 276.5883998183917925, -3.564129467591749201 ) ) ;
#62007 = CARTESIAN_POINT ( 'NONE',  ( 58.82164138842265544, 204.7677522451418781, 10.00000000000009592 ) ) ;
#62008 = CARTESIAN_POINT ( 'NONE',  ( 159.2122473525774069, 254.8832937285494609, -16.22689353966294590 ) ) ;
#62009 = DIRECTION ( 'NONE',  ( 0.000000000000000000, 0.000000000000000000, 1.000000000000000000 ) ) ;
#62010 = CARTESIAN_POINT ( 'NONE',  ( 83.58300336379315354, 45.77414047968564148, -10.26591261625669738 ) ) ;
#62011 = EDGE_CURVE ( 'NONE', #79361, #22484, #31703, .T. ) ;
#62012 = CARTESIAN_POINT ( 'NONE',  ( 171.4761949442340665, 255.4795810469701109, 11.08406205635473185 ) ) ;
#62013 = CARTESIAN_POINT ( 'NONE',  ( 157.4580857293093743, 281.9160373083212221, 1.421786535070352686 ) ) ;
#62014 = ORIENTED_EDGE ( 'NONE', *, *, #86236, .T. ) ;
#62015 = CARTESIAN_POINT ( 'NONE',  ( 194.1377662266459936, 294.3905205579567905, -15.67343962259168322 ) ) ;
#62016 = CARTESIAN_POINT ( 'NONE',  ( 75.07571136114333399, 67.05229642490533593, -13.12030194816077611 ) ) ;
#62018 = ADVANCED_FACE ( 'NONE', ( #30738 ), #53523, .T. ) ;
#62017 = CARTESIAN_POINT ( 'NONE',  ( -19.65312891409030271, 93.06504152958497400, 40.00000000000000000 ) ) ;
#62019 = CARTESIAN_POINT ( 'NONE',  ( -2.305318362029010082, 176.1427522451419350, -10.00000000000009415 ) ) ;
#62020 = CARTESIAN_POINT ( 'NONE',  ( 85.20852645963621796, 213.8768266524159856, -9.188101187500093303 ) ) ;
#62021 = CARTESIAN_POINT ( 'NONE',  ( 196.0579333247489160, 269.4436101228905613, -10.81265959875389626 ) ) ;
#62022 = CARTESIAN_POINT ( 'NONE',  ( 174.6308490632290500, 282.2634308488150623, -14.29746604333752202 ) ) ;
#62023 = CARTESIAN_POINT ( 'NONE',  ( 170.2443324258450730, 280.7353186831560379, -14.04127619006417582 ) ) ;
#62024 = CARTESIAN_POINT ( 'NONE',  ( 11.39698775767667982, 6.984156793818257825, 1.224646799147354243E-15 ) ) ;
#62026 = CARTESIAN_POINT ( 'NONE',  ( 75.91719666336339856, 65.48793379249461566, 14.32281418338181211 ) ) ;
#62025 = CARTESIAN_POINT ( 'NONE',  ( 2.394500126984267396, 178.3149278399160949, -9.188101187500095079 ) ) ;
#62027 = AXIS2_PLACEMENT_3D ( 'NONE', #53000, #21617, #12028 ) ;
#62028 = CARTESIAN_POINT ( 'NONE',  ( 200.8432122835317841, 282.7763473000181307, 17.15137370990203891 ) ) ;
#62029 = ORIENTED_EDGE ( 'NONE', *, *, #45472, .T. ) ;
#62030 = VERTEX_POINT ( 'NONE', #37816 ) ;
#62031 = CARTESIAN_POINT ( 'NONE',  ( 188.7958840745704663, 260.8248006898061817, -6.220177282829866705 ) ) ;
#62032 = CARTESIAN_POINT ( 'NONE',  ( 67.13635405088328412, 67.13670889057797808, -8.571836668080649702 ) ) ;
#62033 = FACE_OUTER_BOUND ( 'NONE', #72989, .T. ) ;
#62034 = CARTESIAN_POINT ( 'NONE',  ( 161.4250356354754672, 267.9004136800010656, 17.49898951125957680 ) ) ;
#62035 = FACE_OUTER_BOUND ( 'NONE', #49741, .T. ) ;
#62036 = CARTESIAN_POINT ( 'NONE',  ( 19.17374232530777078, 188.0024278399160949, 9.188101187500095079 ) ) ;
#62037 = CARTESIAN_POINT ( 'NONE',  ( 129.3758220526426044, 239.3768266524160140, -9.188101187500091527 ) ) ;
#62038 = DIRECTION ( 'NONE',  ( 0.000000000000000000, 0.000000000000000000, 1.000000000000000000 ) ) ;
#62039 = ORIENTED_EDGE ( 'NONE', *, *, #82639, .F. ) ;
#62040 = CARTESIAN_POINT ( 'NONE',  ( -22.42236680055709641, 157.8615022471902591, 0.000000000000000000 ) ) ;
#62041 = VECTOR ( 'NONE', #75675, 1000.000000000000000 ) ;
#62042 = CARTESIAN_POINT ( 'NONE',  ( 177.2802394469194383, 252.6157282624358231, 1.078711111416747359 ) ) ;
#62043 = CARTESIAN_POINT ( 'NONE',  ( 66.47763888060634940, 67.99612994687967671, 6.463816603905427449 ) ) ;
#62044 = CARTESIAN_POINT ( 'NONE',  ( 80.61729146147543190, 57.24021084763496248, -16.23099362249694266 ) ) ;
#62045 = CARTESIAN_POINT ( 'NONE',  ( 155.6435836392643637, 261.0644005951349982, 17.58841156286628049 ) ) ;
#62046 = CARTESIAN_POINT ( 'NONE',  ( 207.8575108622103755, 270.6272257822888037, -6.381720258959569847 ) ) ;
#62047 = CARTESIAN_POINT ( 'NONE',  ( 83.32573152649015924, 51.37405908170996582, 14.80978086562886631 ) ) ;
#62048 = CARTESIAN_POINT ( 'NONE',  ( 194.9819925439454664, 292.9282776833073285, -15.33279721168237586 ) ) ;
#62049 = EDGE_CURVE ( 'NONE', #9692, #18680, #1039, .T. ) ;
#62050 = EDGE_CURVE ( 'NONE', #60494, #7831, #55381, .T. ) ;
#62051 = CARTESIAN_POINT ( 'NONE',  ( 190.2071741674316456, 263.6913551221517196, 7.843308196823155498 ) ) ;
#62052 = CARTESIAN_POINT ( 'NONE',  ( 169.0861754935146450, 278.6444814197644746, 14.06024944971096957 ) ) ;
#62053 = CARTESIAN_POINT ( 'NONE',  ( 192.6564221164474020, 265.0321580081510433, 8.767841527359648168 ) ) ;
#62054 = CARTESIAN_POINT ( 'NONE',  ( 68.60781884079298720, 68.28949036833112984, 7.135800403798556957 ) ) ;
#62055 = CARTESIAN_POINT ( 'NONE',  ( 190.6036479972031259, 300.5117928913073797, -0.6824572005520307405 ) ) ;
#62056 = CARTESIAN_POINT ( 'NONE',  ( 180.8238051759404073, 266.9217313885388876, -14.75443455289115313 ) ) ;
#62057 = ORIENTED_EDGE ( 'NONE', *, *, #11338, .F. ) ;
#62058 = CARTESIAN_POINT ( 'NONE',  ( -31.59160691316810343, 24.09060609829247568, 10.00000000000000000 ) ) ;
#62059 = ADVANCED_FACE ( 'NONE', ( #3358 ), #80376, .F. ) ;
#62060 = CARTESIAN_POINT ( 'NONE',  ( 207.5583741822599393, 271.1453457103705205, 3.140867606700001424 ) ) ;
#62061 = CARTESIAN_POINT ( 'NONE',  ( 188.7764831123630529, 299.4247982080598263, -5.354475200873774376 ) ) ;
#62062 = CARTESIAN_POINT ( 'NONE',  ( 110.7287787077026451, 243.9244531367911293, -4.594050593750046652 ) ) ;
#62063 = CARTESIAN_POINT ( 'NONE',  ( 16.17343562415726765, 11.19860640527290840, 2.839279412974134775 ) ) ;
#62064 = CARTESIAN_POINT ( 'NONE',  ( 150.8359915840788688, 269.3913942967808453, 15.73449616766854575 ) ) ;
#62065 = ADVANCED_FACE ( 'NONE', ( #40308 ), #25120, .T. ) ;
#62066 = CARTESIAN_POINT ( 'NONE',  ( 75.97421294056728414, 58.33098411539324957, -16.47611980641094931 ) ) ;
#62068 = CARTESIAN_POINT ( 'NONE',  ( 195.6116440902121383, 278.4173475472090900, 16.65080808324301742 ) ) ;
#62067 = DIRECTION ( 'NONE',  ( 0.8434505012732891327, -0.5372068985985168910, 0.000000000000000000 ) ) ;
#62069 = CARTESIAN_POINT ( 'NONE',  ( 191.3034052106035858, 299.2997778447344785, -7.689850778203263459 ) ) ;
#62070 = CARTESIAN_POINT ( 'NONE',  ( 150.6815632051821581, 269.6588720951601772, -14.68790257316217307 ) ) ;
#62071 = CARTESIAN_POINT ( 'NONE',  ( 165.8206990081297931, 283.8978799598649516, 9.576760697357309837 ) ) ;
#62072 = CARTESIAN_POINT ( 'NONE',  ( 80.61430232155159104, 228.8967562850347122, -4.648177544792955347E-16 ) ) ;
#62073 = CARTESIAN_POINT ( 'NONE',  ( 204.1284829764352367, 276.6911759709722105, 13.49772714134504170 ) ) ;
#62074 = CARTESIAN_POINT ( 'NONE',  ( 86.20356499834056763, 47.68669917282567638, 10.81083910437671669 ) ) ;
#62075 = EDGE_LOOP ( 'NONE', ( #48678, #30769, #73363, #25369, #21288, #47877, #64878 ) ) ;
#62076 = CARTESIAN_POINT ( 'NONE',  ( 193.0390622633530029, 267.0550773046203972, 11.36550167083046503 ) ) ;
#62077 = CARTESIAN_POINT ( 'NONE',  ( 34.67812306484450602, 22.94754757982092030, 5.678558825948272215 ) ) ;
#62078 = LINE ( 'NONE', #92539, #81482 ) ;
#62079 = CARTESIAN_POINT ( 'NONE',  ( 200.0400595503645036, 270.0189624897442968, 9.074847133236374930 ) ) ;
#62080 = CARTESIAN_POINT ( 'NONE',  ( 196.6800254274587019, 289.9871984561398222, -17.90749311895638129 ) ) ;
#62081 = EDGE_CURVE ( 'NONE', #26754, #88465, #9973, .T. ) ;
#62082 = EDGE_CURVE ( 'NONE', #13459, #68842, #33226, .T. ) ;
#62083 = ORIENTED_EDGE ( 'NONE', *, *, #94051, .T. ) ;
#62084 = CARTESIAN_POINT ( 'NONE',  ( 152.7893866619400001, 275.1786922041311527, 10.91924690663370612 ) ) ;
#62085 = CARTESIAN_POINT ( 'NONE',  ( 79.16403909620731838, 50.00558055149382852, 14.72677174306799230 ) ) ;
#62086 = CARTESIAN_POINT ( 'NONE',  ( 182.3702127349715738, 264.1602241078386442, -12.99238495943751914 ) ) ;
#62087 = LINE ( 'NONE', #93032, #64660 ) ;
#62088 = CARTESIAN_POINT ( 'NONE',  ( 192.1396999271463812, 297.8512729055811974, 12.32430960859512403 ) ) ;
#62089 = ORIENTED_EDGE ( 'NONE', *, *, #43563, .F. ) ;
#62090 = CARTESIAN_POINT ( 'NONE',  ( 73.49483902118549850, 69.87589544865461733, 9.786909576851130055 ) ) ;
#62091 = CARTESIAN_POINT ( 'NONE',  ( 39.38594668318775405, 31.24335787977766188, -9.188101187500008038 ) ) ;
#62092 = VERTEX_POINT ( 'NONE', #1841 ) ;
#62093 = DIRECTION ( 'NONE',  ( 1.000000000000000000, 0.000000000000000000, 0.000000000000000000 ) ) ;
#62094 = FACE_OUTER_BOUND ( 'NONE', #59514, .T. ) ;
#62095 = VERTEX_POINT ( 'NONE', #63626 ) ;
#62096 = CARTESIAN_POINT ( 'NONE',  ( 86.13921288864840164, 46.97634557790220811, -10.11631737044880808 ) ) ;
#62097 = CARTESIAN_POINT ( 'NONE',  ( 158.9057798085220838, 255.4141110857242154, 17.55677396874652629 ) ) ;
#62098 = FACE_OUTER_BOUND ( 'NONE', #69975, .T. ) ;
#62099 = CARTESIAN_POINT ( 'NONE',  ( 82.26287869091245852, 44.55745556623967474, -10.46805190375325445 ) ) ;
#62100 = CARTESIAN_POINT ( 'NONE',  ( 45.09207854535236493, 28.96004757982094446, -5.678558825948275768 ) ) ;
#62101 = CARTESIAN_POINT ( 'NONE',  ( 80.31877406852532886, 44.32323502835605211, 11.34894536411993471 ) ) ;
#62102 = CARTESIAN_POINT ( 'NONE',  ( 84.87268683136555580, 50.02192652042950982, -13.22765022071786944 ) ) ;
#62103 = CARTESIAN_POINT ( 'NONE',  ( 81.22979812886450190, 55.45288652294036069, -16.34461090620092349 ) ) ;
#62104 = ORIENTED_EDGE ( 'NONE', *, *, #11432, .T. ) ;
#62105 = CARTESIAN_POINT ( 'NONE',  ( 196.0580054393319642, 290.6771910296030796, 16.00258381118181461 ) ) ;
#62106 = ORIENTED_EDGE ( 'NONE', *, *, #49617, .F. ) ;
#62107 = CARTESIAN_POINT ( 'NONE',  ( 77.26467096630975107, 49.18305258566515903, -14.81582409400270350 ) ) ;
#62108 = AXIS2_PLACEMENT_3D ( 'NONE', #66366, #97298, #60234 ) ;
#62109 = ORIENTED_EDGE ( 'NONE', *, *, #35552, .F. ) ;
#62110 = CARTESIAN_POINT ( 'NONE',  ( 87.04951863019347513, 45.82536234993809643, -8.629913247614998895 ) ) ;
#62111 = ORIENTED_EDGE ( 'NONE', *, *, #31753, .T. ) ;
#62112 = CARTESIAN_POINT ( 'NONE',  ( 165.8334311161731023, 274.4591478290780060, -15.12211806599400532 ) ) ;
#62113 = CARTESIAN_POINT ( 'NONE',  ( 206.0316325540811704, 273.7897397804065918, -11.04223638802967322 ) ) ;
#62114 = CARTESIAN_POINT ( 'NONE',  ( 190.6240973886985159, 300.4763735062533669, 2.216935469364557321 ) ) ;
#62115 = CARTESIAN_POINT ( 'NONE',  ( 198.2399221193978462, 285.6735130211258138, -17.04706178669553296 ) ) ;
#62116 = CARTESIAN_POINT ( 'NONE',  ( 48.98810889288134973, 89.24608170897542436, -10.00000000000000000 ) ) ;
#62117 = CARTESIAN_POINT ( 'NONE',  ( 167.7086961934988096, 249.0458231482594158, -5.172654644684703484 ) ) ;
#62118 = CARTESIAN_POINT ( 'NONE',  ( -65.03992292888629834, 39.77302590755693501, 177.5919119679930134 ) ) ;
#62119 = CARTESIAN_POINT ( 'NONE',  ( 186.0598909074496419, 286.3830271726962451, -15.31043294068512672 ) ) ;
#62120 = CARTESIAN_POINT ( 'NONE',  ( 126.3990332750161087, 231.5327760586659736, 1.948934522072303157E-15 ) ) ;
#62121 = CARTESIAN_POINT ( 'NONE',  ( 70.57165604962446537, 60.75797888666558322, -14.54259087274441953 ) ) ;
#62122 = CARTESIAN_POINT ( 'NONE',  ( 33.95706010830453181, 41.64646525600393545, -2.839279412974133887 ) ) ;
#62123 = CARTESIAN_POINT ( 'NONE',  ( 177.4031824437115574, 288.8941654109167416, -9.335669202574084835 ) ) ;
#62124 = ORIENTED_EDGE ( 'NONE', *, *, #39597, .F. ) ;
#62125 = ADVANCED_FACE ( 'NONE', ( #48938 ), #10436, .F. ) ;
#62126 = DIRECTION ( 'NONE',  ( 1.000000000000000000, 0.000000000000000000, 0.000000000000000000 ) ) ;
#62127 = CARTESIAN_POINT ( 'NONE',  ( 177.6201654249851174, 253.7431718786475869, 1.360499885134917708 ) ) ;
#62128 = APPLICATION_CONTEXT ( 'automotive_design' ) ;
#62129 = EDGE_CURVE ( 'NONE', #32844, #73648, #27645, .T. ) ;
#62130 = CARTESIAN_POINT ( 'NONE',  ( 171.0924760015939512, 287.7303114454449542, -4.798180175186202767 ) ) ;
#62131 = CARTESIAN_POINT ( 'NONE',  ( 146.6795228420702983, 276.5906093380114612, 3.172940435457009656 ) ) ;
#62132 = CARTESIAN_POINT ( 'NONE',  ( 72.72789744706139459, 64.44696951616786862, 13.39283383340056588 ) ) ;
#62133 = CARTESIAN_POINT ( 'NONE',  ( 153.0927037754837556, 265.4826541232073964, -16.15085267704102634 ) ) ;
#62134 = CARTESIAN_POINT ( 'NONE',  ( 177.2355366647990991, 288.8864627520729869, -9.231742449898762359 ) ) ;
#62135 = EDGE_LOOP ( 'NONE', ( #56675, #60931, #90709, #23509 ) ) ;
#62136 = CARTESIAN_POINT ( 'NONE',  ( 194.7489730912498658, 293.3318792145281009, 16.23511080478873225 ) ) ;
#62137 = LINE ( 'NONE', #12720, #4395 ) ;
#62138 = ORIENTED_EDGE ( 'NONE', *, *, #95871, .F. ) ;
#62139 = CARTESIAN_POINT ( 'NONE',  ( 194.6356465353167948, 293.5281665672507643, -16.13180903283129197 ) ) ;
#62140 = CARTESIAN_POINT ( 'NONE',  ( 165.8841617674041515, 247.6200161724019324, -6.929307956321339113 ) ) ;
#62141 = ORIENTED_EDGE ( 'NONE', *, *, #67135, .F. ) ;
#62143 = EDGE_CURVE ( 'NONE', #42238, #97169, #85801, .T. ) ;
#62142 = CARTESIAN_POINT ( 'NONE',  ( 191.6390250992932920, 267.7947042169313931, -12.26094334802855812 ) ) ;
#62144 = CARTESIAN_POINT ( 'NONE',  ( 156.8824101620476483, 276.5798998049355646, 10.22994899405466640 ) ) ;
#62145 = CARTESIAN_POINT ( 'NONE',  ( 193.4656735081794068, 262.7486161809156897, 4.740984612795180908 ) ) ;
#62146 = CARTESIAN_POINT ( 'NONE',  ( 149.7162292714551199, 271.3308795146458010, 12.12826134257344357 ) ) ;
#62147 = CARTESIAN_POINT ( 'NONE',  ( 202.8499463704053198, 279.3005819042728604, 17.04674939340617001 ) ) ;
#62149 = CARTESIAN_POINT ( 'NONE',  ( 156.8098655126457572, 280.3055410020735962, 5.930865079079680413 ) ) ;
#62148 = CARTESIAN_POINT ( 'NONE',  ( 153.3701107251964402, 270.1885625906204496, 14.06860214899441530 ) ) ;
#62150 = CARTESIAN_POINT ( 'NONE',  ( 199.9276962100341564, 267.5423408568639161, 6.196014648939567770 ) ) ;
#62151 = ORIENTED_EDGE ( 'NONE', *, *, #98949, .T. ) ;
#62152 = CARTESIAN_POINT ( 'NONE',  ( 146.8201187048455267, 276.3470901603510015, 4.112223577763169047 ) ) ;
#62153 = CARTESIAN_POINT ( 'NONE',  ( 73.09495692854210347, 67.84340929558865696, 11.06288556080568597 ) ) ;
#62154 = CARTESIAN_POINT ( 'NONE',  ( 186.7460581780939322, 262.7394680154919229, -8.960597522048372454 ) ) ;
#62155 = CARTESIAN_POINT ( 'NONE',  ( 168.8563211758018099, 286.0187424789903048, -9.056861680415359217 ) ) ;
#62156 = CARTESIAN_POINT ( 'NONE',  ( 147.3907811248416238, 249.2365022471901739, -10.00000000000009237 ) ) ;
#62157 = EDGE_CURVE ( 'NONE', #78498, #77729, #17050, .T. ) ;
#62158 = CARTESIAN_POINT ( 'NONE',  ( 186.5739769617673289, 297.4340541020540059, -4.270514905203655509 ) ) ;
#62159 = EDGE_CURVE ( 'NONE', #25883, #34337, #69100, .T. ) ;
#62160 = CARTESIAN_POINT ( 'NONE',  ( 192.2431834237441706, 297.6720342317289578, 11.07782187406058938 ) ) ;
#62161 = CARTESIAN_POINT ( 'NONE',  ( 22.93021583062070690, 14.20801979619928623, -3.090169943749474069 ) ) ;
#62162 = CARTESIAN_POINT ( 'NONE',  ( 194.4263876777154394, 293.8906135405502482, 15.23185943445137802 ) ) ;
#62163 = CARTESIAN_POINT ( 'NONE',  ( 191.1334016331724399, 283.3379655378311099, -16.58600049649699670 ) ) ;
#62164 = CARTESIAN_POINT ( 'NONE',  ( 70.02394384298496277, 66.60507294567733538, -11.13771036556853744 ) ) ;
#62165 = CARTESIAN_POINT ( 'NONE',  ( 73.67938972387338481, 213.3458772461660544, 9.188101187500095079 ) ) ;
#62166 = DIRECTION ( 'NONE',  ( -0.8660254037844387076, -0.4999999999999998890, -0.000000000000000000 ) ) ;
#62167 = CARTESIAN_POINT ( 'NONE',  ( 147.5540328368684300, 275.0759135952944234, -4.750028533202499403 ) ) ;
#62168 = CARTESIAN_POINT ( 'NONE',  ( 55.08690683815017763, 202.6115022471902591, 10.00000000000009592 ) ) ;
#62169 = CARTESIAN_POINT ( 'NONE',  ( 47.49582885874515625, 78.29235751436857527, -10.00000000000000000 ) ) ;
#62170 = FACE_OUTER_BOUND ( 'NONE', #38073, .T. ) ;
#62171 = CARTESIAN_POINT ( 'NONE',  ( 84.88661097013314816, 50.13767530291475794, -13.29087463649034007 ) ) ;
#62172 = CARTESIAN_POINT ( 'NONE',  ( 80.44215978124604760, 58.39441083166273216, 0.000000000000000000 ) ) ;
#62174 = CARTESIAN_POINT ( 'NONE',  ( 76.13141603458973350, 51.16231187342496867, 16.09112476300021655 ) ) ;
#62173 = CARTESIAN_POINT ( 'NONE',  ( 73.40082382908687464, 69.73317320774677341, -9.891058063621702701 ) ) ;
#62175 = CARTESIAN_POINT ( 'NONE',  ( 161.8677343474444683, 250.2838553346012986, 14.13526557951369433 ) ) ;
#62176 = ADVANCED_FACE ( 'NONE', ( #66622 ), #58511, .F. ) ;
#62177 = CARTESIAN_POINT ( 'NONE',  ( 161.3523358740237938, 251.5903407549832593, 13.23360137856301932 ) ) ;
#62178 = CARTESIAN_POINT ( 'NONE',  ( 157.6673516573649181, 257.5591315650518141, 16.79781451397666103 ) ) ;
#62179 = CARTESIAN_POINT ( 'NONE',  ( 35.15122015938992917, 74.24965902719526412, 59.99999999999999289 ) ) ;
#62180 = VECTOR ( 'NONE', #75427, 1000.000000000000000 ) ;
#62181 = EDGE_CURVE ( 'NONE', #25628, #52271, #97074, .T. ) ;
#62182 = CARTESIAN_POINT ( 'NONE',  ( 49.83688814775681664, 190.3923013555410080, 4.594050593750050204 ) ) ;
#62183 = CARTESIAN_POINT ( 'NONE',  ( 56.60219097117523290, 212.6744531367911293, 4.594050593750047540 ) ) ;
#62184 = FACE_OUTER_BOUND ( 'NONE', #78830, .T. ) ;
#62186 = CARTESIAN_POINT ( 'NONE',  ( 88.52345208173723279, 43.89072024811925843, -0.4439432684152972430 ) ) ;
#62185 = VECTOR ( 'NONE', #96691, 1000.000000000000000 ) ;
#62187 = EDGE_CURVE ( 'NONE', #91328, #19784, #66353, .T. ) ;
#62188 = CARTESIAN_POINT ( 'NONE',  ( 163.6024448037938157, 257.9599251185455273, 15.55702952704531761 ) ) ;
#62189 = CARTESIAN_POINT ( 'NONE',  ( 142.6906155400633622, 259.3149278399160380, -9.188101187500095079 ) ) ;
#62190 = CARTESIAN_POINT ( 'NONE',  ( 67.39295136396972907, 69.98592323009434324, -1.247867760768429646 ) ) ;
#62191 = CARTESIAN_POINT ( 'NONE',  ( 196.7067773240564748, 268.6313083337223588, -10.65017239398339655 ) ) ;
#62192 = CARTESIAN_POINT ( 'NONE',  ( 26.50621139815082472, 30.70171378149920471, -9.188101187500004485 ) ) ;
#62193 = CARTESIAN_POINT ( 'NONE',  ( 198.9225589249066957, 286.1030165008847916, -17.03502353404871883 ) ) ;
#62194 = CARTESIAN_POINT ( 'NONE',  ( 82.80780985081015899, 47.11681503041204877, -11.90565482037006539 ) ) ;
#62195 = CARTESIAN_POINT ( 'NONE',  ( 16.34664070491415444, 11.29860640527290983, -2.839279412974138328 ) ) ;
#62196 = CARTESIAN_POINT ( 'NONE',  ( 55.84441874286383722, 212.2369531367911293, -4.594050593750048428 ) ) ;
#62197 = CARTESIAN_POINT ( 'NONE',  ( 77.21750963125948886, 63.47318699979658163, 15.10190582221587263 ) ) ;
#62198 = LINE ( 'NONE', #15600, #41365 ) ;
#62199 = EDGE_CURVE ( 'NONE', #81391, #35343, #12004, .T. ) ;
#62200 = CARTESIAN_POINT ( 'NONE',  ( 198.4264492142971221, 286.9623037257889564, 17.00126466006521397 ) ) ;
#62201 = CARTESIAN_POINT ( 'NONE',  ( 56.72874666261028409, 196.8927522451418497, 10.00000000000009948 ) ) ;
#62202 = CARTESIAN_POINT ( 'NONE',  ( 201.4399981830169111, 281.7426838008692584, 17.62180968337201392 ) ) ;
#62203 = EDGE_CURVE ( 'NONE', #72620, #7391, #25264, .T. ) ;
#62204 = CARTESIAN_POINT ( 'NONE',  ( 82.56047309644807797, 54.07683023134062239, -15.52634518316282630 ) ) ;
#62205 = CARTESIAN_POINT ( 'NONE',  ( 109.1413257910288479, 240.4865022471902876, 10.00000000000009237 ) ) ;
#62206 = DIRECTION ( 'NONE',  ( 0.9997716407803077798, -0.02136975178731510827, 0.000000000000000000 ) ) ;
#62207 = CARTESIAN_POINT ( 'NONE',  ( 207.1059763530604698, 271.9289217357780899, 6.370907250589925575 ) ) ;
#62208 = ORIENTED_EDGE ( 'NONE', *, *, #74348, .F. ) ;
#62209 = CARTESIAN_POINT ( 'NONE',  ( 48.53010236944518851, 101.9116055364396090, 10.00000000000000000 ) ) ;
#62210 = CARTESIAN_POINT ( 'NONE',  ( 82.35193903712398367, 53.76144841737797719, 15.84691369965403318 ) ) ;
#62211 = ORIENTED_EDGE ( 'NONE', *, *, #2526, .F. ) ;
#62212 = CARTESIAN_POINT ( 'NONE',  ( 206.3018347371251195, 273.3217358710584790, -9.309724106897926177 ) ) ;
#62213 = CARTESIAN_POINT ( 'NONE',  ( 188.4547781097711834, 277.6015940764860375, -16.57049336306976883 ) ) ;
#62214 = CARTESIAN_POINT ( 'NONE',  ( 164.6063343576543048, 274.4739709976624908, 16.17759516952312637 ) ) ;
#62215 = ORIENTED_EDGE ( 'NONE', *, *, #73533, .T. ) ;
#62216 = PLANE ( 'NONE',  #28912 ) ;
#62217 = ORIENTED_EDGE ( 'NONE', *, *, #38710, .F. ) ;
#62218 = CARTESIAN_POINT ( 'NONE',  ( 66.29454943693275482, 69.24199052626691753, -2.144636311159408226 ) ) ;
#62219 = CARTESIAN_POINT ( 'NONE',  ( 148.3253847707240141, 273.7398928553401447, -9.074433450356286457 ) ) ;
#62220 = CARTESIAN_POINT ( 'NONE',  ( 82.16322555321710297, 45.01969389507814157, 10.99933557872955525 ) ) ;
#62221 = ORIENTED_EDGE ( 'NONE', *, *, #18327, .F. ) ;
#62222 = CARTESIAN_POINT ( 'NONE',  ( 28.38260615371904905, 22.10170272979928185, -7.433330006724141015 ) ) ;
#62223 = CARTESIAN_POINT ( 'NONE',  ( 79.75048646024721677, 44.95318393210929742, 11.52289528432964438 ) ) ;
#62224 = LINE ( 'NONE', #93176, #95426 ) ;
#62225 = CARTESIAN_POINT ( 'NONE',  ( 75.31212634066369560, 66.58130303916082937, -13.09031499722823710 ) ) ;
#62226 = VERTEX_POINT ( 'NONE', #95905 ) ;
#62227 = LINE ( 'NONE', #31831, #33638 ) ;
#62228 = CARTESIAN_POINT ( 'NONE',  ( -0.4807448425718762741, 158.9824982072973683, 3.021315404115420679E-15 ) ) ;
#62229 = EDGE_LOOP ( 'NONE', ( #28351, #59794, #88142, #22387 ) ) ;
#62230 = CARTESIAN_POINT ( 'NONE',  ( 171.3153268440470356, 284.6697624753109039, 10.75620792707900009 ) ) ;
#62232 = CARTESIAN_POINT ( 'NONE',  ( 67.99201013372248781, 65.53178319986331246, -10.30868045286246115 ) ) ;
#62231 = CARTESIAN_POINT ( 'NONE',  ( 67.77717145076422867, 65.67792780390388430, 10.77137413574873825 ) ) ;
#62233 = DIRECTION ( 'NONE',  ( -0.000000000000000000, -0.000000000000000000, -1.000000000000000000 ) ) ;
#62234 = CARTESIAN_POINT ( 'NONE',  ( 204.9768178125733016, 275.6167325052707611, 13.98665089523138505 ) ) ;
#62235 = FACE_OUTER_BOUND ( 'NONE', #85720, .T. ) ;
#62236 = CARTESIAN_POINT ( 'NONE',  ( 204.9658583905037688, 275.6357147811169170, -12.57240504404813564 ) ) ;
#62237 = CARTESIAN_POINT ( 'NONE',  ( 138.1979352100490530, 262.8464784336661637, 1.353441290958777525E-15 ) ) ;
#62238 = CARTESIAN_POINT ( 'NONE',  ( 206.4634061315404665, 270.6220774564198450, 2.471500839510567094 ) ) ;
#62239 = CARTESIAN_POINT ( 'NONE',  ( 182.5855175857635686, 259.4356802941314299, 9.332393434239792285 ) ) ;
#62240 = CARTESIAN_POINT ( 'NONE',  ( 78.52397964811635234, 206.9548013555409796, -4.594050593750042211 ) ) ;
#62241 = ORIENTED_EDGE ( 'NONE', *, *, #19789, .T. ) ;
#62242 = CARTESIAN_POINT ( 'NONE',  ( 150.6571681785161445, 269.7011255207979730, 15.24894850018880454 ) ) ;
#62243 = CARTESIAN_POINT ( 'NONE',  ( 74.58922631747108767, 66.95469429158355013, 12.55546573254311937 ) ) ;
#62244 = CARTESIAN_POINT ( 'NONE',  ( 78.18406947592188772, 61.66846224198985027, -16.12704840749690050 ) ) ;
#62245 = ORIENTED_EDGE ( 'NONE', *, *, #58135, .T. ) ;
#62246 = CARTESIAN_POINT ( 'NONE',  ( 195.8873709255798587, 291.3601163262420641, -15.74573728859107646 ) ) ;
#62247 = ORIENTED_EDGE ( 'NONE', *, *, #75734, .T. ) ;
#62248 = VERTEX_POINT ( 'NONE', #48765 ) ;
#62249 = CARTESIAN_POINT ( 'NONE',  ( 80.05820879288631886, 44.42019321735476467, -10.88558367697336848 ) ) ;
#62250 = CARTESIAN_POINT ( 'NONE',  ( 73.70645301951556405, 223.3615022471903160, 5.000000000000046185 ) ) ;
#62251 = CARTESIAN_POINT ( 'NONE',  ( 191.8456210280128005, 298.3606325003146367, -9.135603544929113085 ) ) ;
#62252 = DIRECTION ( 'NONE',  ( -0.8660254037844387076, -0.4999999999999998890, -0.000000000000000000 ) ) ;
#62253 = CARTESIAN_POINT ( 'NONE',  ( 79.81928979513558886, 48.51125504466014604, -13.89558333913432087 ) ) ;
#62254 = CARTESIAN_POINT ( 'NONE',  ( 207.8833583980453739, 270.5824565369721313, 1.564926904161892285 ) ) ;
#62255 = CARTESIAN_POINT ( 'NONE',  ( 75.84410613756948294, 226.8464784336661353, 1.353441290958777327E-15 ) ) ;
#62256 = ORIENTED_EDGE ( 'NONE', *, *, #51234, .F. ) ;
#62257 = ORIENTED_EDGE ( 'NONE', *, *, #3849, .T. ) ;
#62258 = CARTESIAN_POINT ( 'NONE',  ( 161.2850924390880323, 251.2930207224935373, -13.14774649685070074 ) ) ;
#62259 = VERTEX_POINT ( 'NONE', #42628 ) ;
#62260 = CARTESIAN_POINT ( 'NONE',  ( 24.06687416953986514, 14.86426979415089633, -3.090169943749474069 ) ) ;
#62262 = ADVANCED_FACE ( 'NONE', ( #96389 ), #73557, .F. ) ;
#62261 = AXIS2_PLACEMENT_3D ( 'NONE', #12280, #82714, #97389 ) ;
#62263 = CARTESIAN_POINT ( 'NONE',  ( 76.16798847255994076, 65.32953285235316798, -14.06901634343885021 ) ) ;
#62264 = CARTESIAN_POINT ( 'NONE',  ( 165.0087721269838710, 244.8434183119457543, 2.604344609212914108 ) ) ;
#62265 = CARTESIAN_POINT ( 'NONE',  ( 161.5502493243027402, 284.0868935703256852, 0.5284661774659209499 ) ) ;
#62266 = LINE ( 'NONE', #55170, #88228 ) ;
#62267 = CARTESIAN_POINT ( 'NONE',  ( -19.65312891409030271, 93.06504152958497400, 177.5919119679930134 ) ) ;
#62268 = CARTESIAN_POINT ( 'NONE',  ( 83.81371460731152467, 43.68598234505141420, -7.289791965750151981 ) ) ;
#62269 = CARTESIAN_POINT ( 'NONE',  ( 32.45591003703110999, 42.23654200823204974, 1.583844403245397769 ) ) ;
#62270 = CARTESIAN_POINT ( 'NONE',  ( 154.7823760652066198, 279.7145020948755700, 5.599380836552000140 ) ) ;
#62272 = ADVANCED_FACE ( 'NONE', ( #3668 ), #3186, .T. ) ;
#62271 = CARTESIAN_POINT ( 'NONE',  ( 152.6873874250818517, 266.1846826352417565, -16.66598363829485763 ) ) ;
#62273 = B_SPLINE_CURVE_WITH_KNOTS ( 'NONE', 3,
 ( #44853, #28668, #68161, #37750, #51978, #60051, #13003, #59552, #21578, #90529, #43863, #7355, #75793, #44362, #52463, #45837, #5382, #6379, #76289, #82917, #6861, #99087, #29669, #13492, #60546, #91503, #75295, #52963, #14476, #24058, #84898, #86929, #69154, #93498, #7873, #15439, #61551, #23042, #46338, #78778, #23540, #8858, #1779, #92497, #30671, #69653 ),
 .UNSPECIFIED., .F., .F.,
 ( 4, 1, 2, 2, 1, 2, 2, 1, 1, 2, 2, 1, 1, 2, 2, 1, 1, 2, 2, 1, 1, 1, 2, 2, 1, 1, 1, 2, 2, 4 ),
 ( 0.000000000000000000, 0.06249999999999282518, 0.09374999999998952227, 0.1249999999999862332, 0.1874999999999796274, 0.2187499999999759637, 0.2499999999999722999, 0.3124999999999658051, 0.3437499999999626965, 0.3593749999999617528, 0.3749999999999607536, 0.4374999999999629741, 0.4687499999999648614, 0.4843749999999655831, 0.4999999999999663602, 0.5624999999999700240, 0.5937499999999719114, 0.6093749999999720224, 0.6249999999999721334, 0.6874999999999705791, 0.7187499999999698019, 0.7343749999999689138, 0.7421874999999691358, 0.7499999999999692468, 0.8124999999999721334, 0.8437499999999744649, 0.8593749999999756861, 0.8671874999999771294, 0.8749999999999785727, 1.000000000000000000 ),
 .UNSPECIFIED. ) ;
#62274 = CARTESIAN_POINT ( 'NONE',  ( 72.49654942766741783, 70.83148394934322312, 7.643478247317299967 ) ) ;
#62275 = EDGE_CURVE ( 'NONE', #14058, #62875, #57339, .T. ) ;
#62276 = CARTESIAN_POINT ( 'NONE',  ( 70.75328031780846061, 67.31962847426909491, -10.19312708527341371 ) ) ;
#62277 = VERTEX_POINT ( 'NONE', #26953 ) ;
#62278 = CYLINDRICAL_SURFACE ( 'NONE', #34827, 17.82106496071139645 ) ;
#62279 =( BOUNDED_CURVE ( )  B_SPLINE_CURVE ( 2, ( #7901, #39261, #38270, #38776, #54979, #780, #39753, #86450, #70682 ),
 .UNSPECIFIED., .F., .T. ) 
 B_SPLINE_CURVE_WITH_KNOTS ( ( 3, 2, 2, 2, 3 ),
 ( 0.01209677419354838850, 0.01344086021505376365, 0.01612903225806451568, 0.01881720430107526945, 0.02016129032258064807 ),
 .UNSPECIFIED. ) 
 CURVE ( )  GEOMETRIC_REPRESENTATION_ITEM ( )  RATIONAL_B_SPLINE_CURVE ( ( 0.9330127018922194093, 0.9330127018922194093, 1.000000000000000000, 0.8660254037844387076, 1.000000000000000000, 0.8660254037844387076, 1.000000000000000000, 0.9330127018922191873, 0.9330127018922192983 ) ) 
 REPRESENTATION_ITEM ( '' )  );
#62280 = CARTESIAN_POINT ( 'NONE',  ( 181.6597933908766436, 291.8373067516729407, 10.47321924421550321 ) ) ;
#62281 = CARTESIAN_POINT ( 'NONE',  ( 12.22230530498202050, 30.55466486950698624, -1.111400068045478839E-16 ) ) ;
#62282 = PLANE ( 'NONE',  #97812 ) ;
#62283 = CARTESIAN_POINT ( 'NONE',  ( 83.70690788325238429, 51.99575818335755173, 14.97781791391902928 ) ) ;
#62284 = CARTESIAN_POINT ( 'NONE',  ( -19.65312891409030271, 93.06504152958497400, 59.99999999999999289 ) ) ;
#62285 = ORIENTED_EDGE ( 'NONE', *, *, #87657, .F. ) ;
#62286 = DIRECTION ( 'NONE',  ( 0.000000000000000000, -1.000000000000000000, 0.000000000000000000 ) ) ;
#62287 = CARTESIAN_POINT ( 'NONE',  ( 84.14312167556933275, 48.98415679381830756, 0.000000000000000000 ) ) ;
#62288 = AXIS2_PLACEMENT_3D ( 'NONE', #82587, #91659, #36921 ) ;
#62289 = FACE_OUTER_BOUND ( 'NONE', #43206, .T. ) ;
#62291 = CARTESIAN_POINT ( 'NONE',  ( 73.63433810907314125, 55.41313869502708656, 16.11241297416459872 ) ) ;
#62290 = DIRECTION ( 'NONE',  ( -0.000000000000000000, 0.000000000000000000, 1.000000000000000000 ) ) ;
#62292 = FACE_OUTER_BOUND ( 'NONE', #91313, .T. ) ;
#62293 = CARTESIAN_POINT ( 'NONE',  ( 35.05457148360284236, 21.20801979619930933, -3.090169943749474069 ) ) ;
#62294 = CARTESIAN_POINT ( 'NONE',  ( 172.0916398547322785, 275.0630559527974697, 16.92144769315549979 ) ) ;
#62295 = CARTESIAN_POINT ( 'NONE',  ( 163.2303979562223333, 283.9008525415044346, -3.773057203759900169 ) ) ;
#62296 = DIRECTION ( 'NONE',  ( 1.000000000000000000, 0.000000000000000000, 0.000000000000000000 ) ) ;
#62297 = CARTESIAN_POINT ( 'NONE',  ( 192.0195900110790319, 262.3135081745301704, 2.967184076358189593 ) ) ;
#62298 = EDGE_CURVE ( 'NONE', #45554, #51698, #4141, .T. ) ;
#62299 = CARTESIAN_POINT ( 'NONE',  ( 0.1211834420501121806, 177.0024278399160949, -9.188101187500093303 ) ) ;
#62300 = CYLINDRICAL_SURFACE ( 'NONE', #93802, 10.00000000000010658 ) ;
#62301 = VERTEX_POINT ( 'NONE', #57836 ) ;
#62302 = CARTESIAN_POINT ( 'NONE',  ( 178.3300713922748457, 256.8661311210547638, 8.413408369093348327 ) ) ;
#62303 = EDGE_CURVE ( 'NONE', #11947, #51377, #19732, .T. ) ;
#62304 = CARTESIAN_POINT ( 'NONE',  ( 35.21268636174862365, 20.73415679381824006, 1.333680081654574804E-15 ) ) ;
#62305 = CARTESIAN_POINT ( 'NONE',  ( 161.9296067209906198, 272.1511200004533180, 16.47594105373750750 ) ) ;
#62306 = CARTESIAN_POINT ( 'NONE',  ( 20.95974617273066443, 195.1589784336661637, -6.496448406907676862E-16 ) ) ;
#62307 = CARTESIAN_POINT ( 'NONE',  ( -61.61048871844075592, 38.59675092633816007, -10.00000000000000000 ) ) ;
#62308 = CARTESIAN_POINT ( 'NONE',  ( 27.80420065655628648, 34.79103043416550634, 8.090169943749478065 ) ) ;
#62309 = CARTESIAN_POINT ( 'NONE',  ( 85.03485922901262484, 42.43661927826852320, -1.488589828080878252 ) ) ;
#62310 = CARTESIAN_POINT ( 'NONE',  ( 191.8456210280128005, 298.3606325003146367, -9.135603544929113085 ) ) ;
#62311 = CARTESIAN_POINT ( 'NONE',  ( 81.60179630412660856, 55.93049734755844327, 16.03035934503441240 ) ) ;
#62312 = EDGE_CURVE ( 'NONE', #26530, #13530, #97772, .T. ) ;
#62313 = CARTESIAN_POINT ( 'NONE',  ( 84.74131058565687624, 48.42447779055156332, 12.64580013056608898 ) ) ;
#62314 = CARTESIAN_POINT ( 'NONE',  ( 188.0081030067536858, 260.0748169616455243, -0.7643377115716368797 ) ) ;
#62315 = CIRCLE ( 'NONE', #85016, 0.1418229129684263345 ) ;
#62316 = B_SPLINE_CURVE_WITH_KNOTS ( 'NONE', 3,
 ( #62631, #9967, #25143, #23631 ),
 .UNSPECIFIED., .F., .F.,
 ( 4, 4 ),
 ( 0.01247596805550315810, 0.01873461069493020936 ),
 .UNSPECIFIED. ) ;
#62317 = CARTESIAN_POINT ( 'NONE',  ( 62.88113547221008304, 217.1115022471903160, -5.000000000000047962 ) ) ;
#62318 = DIRECTION ( 'NONE',  ( 0.000000000000000000, 0.7457702847286216130, -0.6662031840330625565 ) ) ;
#62319 = DIRECTION ( 'NONE',  ( 1.000000000000000000, -7.137148015447434001E-15, 0.000000000000000000 ) ) ;
#62320 = CARTESIAN_POINT ( 'NONE',  ( 32.38097682878547090, 183.3768266524159856, 9.188101187500098632 ) ) ;
#62321 = CARTESIAN_POINT ( 'NONE',  ( 67.43464856002299257, 69.65467215062919593, -3.403559293901139871 ) ) ;
#62322 = B_SPLINE_CURVE_WITH_KNOTS ( 'NONE', 3,
 ( #29129, #67108, #99527, #97547, #68108, #52904, #59996, #90965, #44303, #36700, #37207, #28610 ),
 .UNSPECIFIED., .F., .F.,
 ( 4, 2, 2, 2, 2, 4 ),
 ( 0.001941519080533212534, 0.002048514964777567709, 0.002155510849021922883, 0.002369502617510633666, 0.002797486154488115079, 0.003653453228443075736 ),
 .UNSPECIFIED. ) ;
#62323 = CARTESIAN_POINT ( 'NONE',  ( 29.61202869050421427, 35.83478043621390441, -8.090169943749479842 ) ) ;
#62324 = CARTESIAN_POINT ( 'NONE',  ( 65.47921168356340615, 218.6115022471903160, -5.000000000000047962 ) ) ;
#62325 = CARTESIAN_POINT ( 'NONE',  ( 151.4376533647338476, 268.3492855237141725, -15.16853828792834236 ) ) ;
#62326 = AXIS2_PLACEMENT_3D ( 'NONE', #28972, #66953, #36548 ) ;
#62327 = CARTESIAN_POINT ( 'NONE',  ( 50.00170217996128486, 86.12209509027381671, 177.5919119679930134 ) ) ;
#62328 = CARTESIAN_POINT ( 'NONE',  ( -105.0000000000000000, 9.999999999999998224, 59.99999999999999289 ) ) ;
#62329 = B_SPLINE_CURVE_WITH_KNOTS ( 'NONE', 3,
 ( #59419, #30032, #60918, #37622 ),
 .UNSPECIFIED., .F., .F.,
 ( 4, 4 ),
 ( 0.01532915748665746730, 0.02410358160937203786 ),
 .UNSPECIFIED. ) ;
#62330 = CARTESIAN_POINT ( 'NONE',  ( 202.7787896891747721, 278.0581983447742118, -15.29768258928314317 ) ) ;
#62331 = B_SPLINE_CURVE_WITH_KNOTS ( 'NONE', 3,
 ( #77560, #30442, #56, #46119, #53725, #54217, #8645, #84684, #15224, #54725 ),
 .UNSPECIFIED., .F., .F.,
 ( 4, 2, 2, 2, 4 ),
 ( 0.000000000000000000, 0.0002622400424272925377, 0.0005244800848545850755, 0.0007867201272818776132, 0.001048960169709170151 ),
 .UNSPECIFIED. ) ;
#62332 = DIRECTION ( 'NONE',  ( -0.9403255362191098587, 0.3402761906661169733, 0.000000000000000000 ) ) ;
#62333 = CARTESIAN_POINT ( 'NONE',  ( 23.32475077058400004, 14.26216523072494446, -2.296566073217252530E-15 ) ) ;
#62334 = CARTESIAN_POINT ( 'NONE',  ( 147.6300909839706321, 274.9441770201837585, 8.328755691084779755 ) ) ;
#62335 = CARTESIAN_POINT ( 'NONE',  ( 71.66445348058819320, 59.04578686578420132, 15.85137124283286170 ) ) ;
#62336 = DIRECTION ( 'NONE',  ( -1.000000000000000000, 0.000000000000000000, 0.000000000000000000 ) ) ;
#62337 = ORIENTED_EDGE ( 'NONE', *, *, #50360, .F. ) ;
#62338 = CARTESIAN_POINT ( 'NONE',  ( 8.149503075528279794, 26.74646525600388358, 2.839279412974139660 ) ) ;
#62339 = CARTESIAN_POINT ( 'NONE',  ( 78.42229082697367915, 57.96928826923493716, -16.21819880184166252 ) ) ;
#62340 = CARTESIAN_POINT ( 'NONE',  ( 88.19071408691713998, 44.34108068381398482, 2.666398900887132939 ) ) ;
#62341 = ORIENTED_EDGE ( 'NONE', *, *, #34632, .T. ) ;
#62342 = PLANE ( 'NONE',  #19845 ) ;
#62343 = CARTESIAN_POINT ( 'NONE',  ( 70.02460195589141279, 70.89239522396498216, -2.258892735534246743 ) ) ;
#62344 = CARTESIAN_POINT ( 'NONE',  ( 150.6931560952953646, 269.6387926204777727, 14.65021044537114037 ) ) ;
#62345 = CARTESIAN_POINT ( 'NONE',  ( 180.9708674785521794, 257.0886412231608347, -7.749587717661919228 ) ) ;
#62346 = ADVANCED_FACE ( 'NONE', ( #71570 ), #74886, .T. ) ;
#62347 = VERTEX_POINT ( 'NONE', #28949 ) ;
#62348 = ORIENTED_EDGE ( 'NONE', *, *, #58561, .T. ) ;
#62349 = CARTESIAN_POINT ( 'NONE',  ( 189.6768609436964539, 274.4077930505946483, -17.07046811116321550 ) ) ;
#62350 = ORIENTED_EDGE ( 'NONE', *, *, #51786, .F. ) ;
#62351 = CARTESIAN_POINT ( 'NONE',  ( 153.4613150239306094, 264.8442007126561748, -16.86932470306368259 ) ) ;
#62352 = FACE_OUTER_BOUND ( 'NONE', #77114, .T. ) ;
#62353 = CARTESIAN_POINT ( 'NONE',  ( 72.70498915057306988, 57.04919252086779835, -16.38563882821832607 ) ) ;
#62354 = DIRECTION ( 'NONE',  ( -0.8660254037844378194, -0.5000000000000014433, -0.000000000000000000 ) ) ;
#62355 = EDGE_CURVE ( 'NONE', #48577, #13530, #74571, .T. ) ;
#62356 = CARTESIAN_POINT ( 'NONE',  ( 147.6618183892331331, 274.8892235422768522, 8.990680574201936892 ) ) ;
#62357 = AXIS2_PLACEMENT_3D ( 'NONE', #54174, #85143, #15689 ) ;
#62358 = ORIENTED_EDGE ( 'NONE', *, *, #69634, .F. ) ;
#62359 = CARTESIAN_POINT ( 'NONE',  ( 19.39689925177878749, 34.96947112835014337, 177.5919119679930134 ) ) ;
#62360 = CARTESIAN_POINT ( 'NONE',  ( 162.0988651326803165, 266.7229752693668274, 16.74775755896888896 ) ) ;
#62361 = ORIENTED_EDGE ( 'NONE', *, *, #44670, .T. ) ;
#62362 = CARTESIAN_POINT ( 'NONE',  ( 35.07444006175263240, 22.11110640527294535, -2.839279412974138328 ) ) ;
#62363 = CARTESIAN_POINT ( 'NONE',  ( 190.4249800432324662, 300.8212548652687133, 3.085047376053959400 ) ) ;
#62364 = CARTESIAN_POINT ( 'NONE',  ( 78.24241764518251330, 47.43171081316724980, -14.32955934271819665 ) ) ;
#62365 = VERTEX_POINT ( 'NONE', #44121 ) ;
#62366 = CARTESIAN_POINT ( 'NONE',  ( 179.6160012257981862, 295.0481727651569486, 1.085779272287555663 ) ) ;
#62367 = CARTESIAN_POINT ( 'NONE',  ( 24.34666095796415419, 37.55466486950700755, 7.012934429366973338E-14 ) ) ;
#62368 = CARTESIAN_POINT ( 'NONE',  ( 150.7576929667484080, 269.5270114801595582, 13.75028158740543205 ) ) ;
#62369 = VECTOR ( 'NONE', #7460, 1000.000000000000000 ) ;
#62370 = CARTESIAN_POINT ( 'NONE',  ( 34.40128339993918871, 35.56454794089043503, 10.00000000000000355 ) ) ;
#62371 = EDGE_LOOP ( 'NONE', ( #1170, #76600, #27964, #96459 ) ) ;
#62372 = ORIENTED_EDGE ( 'NONE', *, *, #11655, .T. ) ;
#62373 = CARTESIAN_POINT ( 'NONE',  ( -19.83262083840137180, 133.3759306620404459, -30.52142883766495629 ) ) ;
#62374 = CARTESIAN_POINT ( 'NONE',  ( 82.59969462453734934, 42.72094940597061452, -6.768182983292747146 ) ) ;
#62375 = CARTESIAN_POINT ( 'NONE',  ( 172.3935366929414954, 290.1034599593647840, 4.993860462594684080 ) ) ;
#62376 = CARTESIAN_POINT ( 'NONE',  ( 189.8136646974935786, 301.8800841035353528, -0.6430783927310335102 ) ) ;
#62377 = VERTEX_POINT ( 'NONE', #36030 ) ;
#62378 = CARTESIAN_POINT ( 'NONE',  ( 190.4163244163388242, 300.8362468508201459, 4.691083071570470331 ) ) ;
#62379 = CARTESIAN_POINT ( 'NONE',  ( 90.04477061917849312, 44.76220097505219542, 0.000000000000000000 ) ) ;
#62380 = FACE_OUTER_BOUND ( 'NONE', #45651, .T. ) ;
#62381 = CARTESIAN_POINT ( 'NONE',  ( 146.8312060062178830, 276.3278863910550172, -4.807241325481028227 ) ) ;
#62382 = CARTESIAN_POINT ( 'NONE',  ( 159.9495225368867466, 255.4964586287468080, 16.29484429292893566 ) ) ;
#62383 = CARTESIAN_POINT ( 'NONE',  ( 68.85038956537171373, 65.11612515096180687, 11.21264051096888004 ) ) ;
#62384 = CARTESIAN_POINT ( 'NONE',  ( 164.3022921857394749, 246.0670774647090582, 1.862798784958315856 ) ) ;
#62385 = CARTESIAN_POINT ( 'NONE',  ( 42.87900647455834502, 24.75620593066997444, -1.732050807568748407 ) ) ;
#62386 = CARTESIAN_POINT ( 'NONE',  ( 71.82406175789866154, 65.23099472832208789, -12.52007583028708559 ) ) ;
#62387 = CARTESIAN_POINT ( 'NONE',  ( 78.73346053687757262, 47.61223242048821191, 14.27696141479210468 ) ) ;
#62388 = CARTESIAN_POINT ( 'NONE',  ( 115.5733686319456126, 237.5333772461660544, 9.188101187500095079 ) ) ;
#62389 = ORIENTED_EDGE ( 'NONE', *, *, #70720, .F. ) ;
#62390 = CARTESIAN_POINT ( 'NONE',  ( 146.6363376198206652, 276.6654083370839885, -0.5879280619134327202 ) ) ;
#62391 = CARTESIAN_POINT ( 'NONE',  ( 83.45882455891384666, 41.54361669290386772, -1.301328012872986717 ) ) ;
#62392 = CARTESIAN_POINT ( 'NONE',  ( 87.35668359673078953, 44.84080960044052944, -6.701380392922970053 ) ) ;
#62393 = CARTESIAN_POINT ( 'NONE',  ( 155.6328838216860220, 261.0829332228125850, -17.51014940606912518 ) ) ;
#62394 = EDGE_CURVE ( 'NONE', #76267, #40576, #6135, .T. ) ;
#62395 = AXIS2_PLACEMENT_3D ( 'NONE', #25945, #11254, #26439 ) ;
#62396 = CARTESIAN_POINT ( 'NONE',  ( 204.5730103890532519, 276.3161474792809145, 14.88139715235883109 ) ) ;
#62397 = EDGE_CURVE ( 'NONE', #61231, #39956, #52228, .T. ) ;
#62398 = CARTESIAN_POINT ( 'NONE',  ( 83.89856196509347797, 51.66380357613086005, -14.40442690555789618 ) ) ;
#62399 = CARTESIAN_POINT ( 'NONE',  ( 165.4745112603759196, 283.5991399024592852, -8.288623825315429627 ) ) ;
#62400 = EDGE_LOOP ( 'NONE', ( #56150, #81378, #30350, #27665 ) ) ;
#62401 = CARTESIAN_POINT ( 'NONE',  ( 162.6341128535665064, 248.9564488241690299, -10.63508949045170660 ) ) ;
#62402 = CARTESIAN_POINT ( 'NONE',  ( 72.59841233342120859, 71.52691570274980393, 5.510137056446514414 ) ) ;
#62403 = CARTESIAN_POINT ( 'NONE',  ( -75.57215499213535281, 50.95729256953105590, 177.5919119679930134 ) ) ;
#62404 = AXIS2_PLACEMENT_3D ( 'NONE', #87365, #19406, #89334 ) ;
#62405 = CARTESIAN_POINT ( 'NONE',  ( 27.58098951138967436, 43.10352854649765675, 10.00000000000000000 ) ) ;
#62406 = CARTESIAN_POINT ( 'NONE',  ( 186.3568650544643788, 297.0301385972502999, 4.669442245733694818 ) ) ;
#62407 = CARTESIAN_POINT ( 'NONE',  ( 157.4177733328310467, 257.9914139036126812, 18.29188238796808363 ) ) ;
#62408 = DIRECTION ( 'NONE',  ( 0.000000000000000000, 0.000000000000000000, 1.000000000000000000 ) ) ;
#62409 = CARTESIAN_POINT ( 'NONE',  ( 56.62968813474974894, 197.3768266524160140, -9.188101187500091527 ) ) ;
#62410 = CARTESIAN_POINT ( 'NONE',  ( 85.74775437209392237, 48.65322352004045570, -12.36257617231559891 ) ) ;
#62411 = ORIENTED_EDGE ( 'NONE', *, *, #93233, .F. ) ;
#62412 = CARTESIAN_POINT ( 'NONE',  ( 87.74907107289484998, 44.16117455547062320, -4.521424286948808380 ) ) ;
#62413 = DIRECTION ( 'NONE',  ( -0.000000000000000000, 0.000000000000000000, -1.000000000000000000 ) ) ;
#62414 = CARTESIAN_POINT ( 'NONE',  ( -36.26652983198114555, 26.35523046909639788, -10.00000000000000000 ) ) ;
#62415 = CARTESIAN_POINT ( 'NONE',  ( 174.5460195235792185, 262.1449155284953463, 14.31061777505408550 ) ) ;
#62416 = CARTESIAN_POINT ( 'NONE',  ( 82.22868350776323609, 41.49786495964391264, -5.893870365715465631 ) ) ;
#62417 = CARTESIAN_POINT ( 'NONE',  ( 154.9048824156581361, 262.3438686460345366, -17.40627786727128168 ) ) ;
#62418 = CARTESIAN_POINT ( 'NONE',  ( 9.458193372709603253, 186.2677522451419065, -5.000000000000047962 ) ) ;
#62419 = EDGE_CURVE ( 'NONE', #75738, #92597, #40988, .T. ) ;
#62420 = CARTESIAN_POINT ( 'NONE',  ( 106.9582200821077578, 225.8927522451417929, -10.00000000000009059 ) ) ;
#62421 = PLANE ( 'NONE',  #62868 ) ;
#62422 = ORIENTED_EDGE ( 'NONE', *, *, #12183, .T. ) ;
#62423 = CARTESIAN_POINT ( 'NONE',  ( 147.6857584380539095, 274.8477581613835810, 8.112022437684441201 ) ) ;
#62424 = DIRECTION ( 'NONE',  ( 0.4999999999999992784, -0.8660254037844390407, 0.000000000000000000 ) ) ;
#62425 = AXIS2_PLACEMENT_3D ( 'NONE', #100187, #52555, #22169 ) ;
#62426 = CARTESIAN_POINT ( 'NONE',  ( 26.88721494746919660, 177.1423013555409796, -4.594050593750043987 ) ) ;
#62427 = CARTESIAN_POINT ( 'NONE',  ( 17.13867093926436169, 10.86426979415088567, -3.090169943749474069 ) ) ;
#62428 = CARTESIAN_POINT ( 'NONE',  ( 71.47468121884192271, 223.6199935810940929, 2.679491924311251605 ) ) ;
#62429 = CARTESIAN_POINT ( 'NONE',  ( 73.95758533133535195, 54.98678301060776619, -16.60461700056748313 ) ) ;
#62431 = CARTESIAN_POINT ( 'NONE',  ( 70.10703493326258240, 211.2833772461660544, -9.188101187500095079 ) ) ;
#62430 = FACE_OUTER_BOUND ( 'NONE', #12151, .T. ) ;
#62432 = CARTESIAN_POINT ( 'NONE',  ( 200.2631011806900005, 283.7811292041749311, 18.23377125296567058 ) ) ;
#62433 = CARTESIAN_POINT ( 'NONE',  ( 73.16563970766678437, 57.31928544487961830, 16.38500887864065803 ) ) ;
#62434 = CARTESIAN_POINT ( 'NONE',  ( 72.46511837996447980, 71.56249752072032777, 6.234640293157904800 ) ) ;
#62435 = CARTESIAN_POINT ( 'NONE',  ( 66.67307728759789143, 68.37645106841958409, -4.361463599803915514 ) ) ;
#62436 = EDGE_LOOP ( 'NONE', ( #61869, #19279, #92938 ) ) ;
#62437 = VECTOR ( 'NONE', #48951, 1000.000000000000114 ) ;
#62438 = CARTESIAN_POINT ( 'NONE',  ( 25.13686162393831225, 191.9865022471903444, -10.00000000000009415 ) ) ;
#62439 = CARTESIAN_POINT ( 'NONE',  ( 202.7865629936218284, 279.4103651332174536, 17.10878160033216133 ) ) ;
#62440 = CARTESIAN_POINT ( 'NONE',  ( -2.449395605728673875, 160.2048013555409796, 4.594050593750051981 ) ) ;
#62441 = CARTESIAN_POINT ( 'NONE',  ( 29.64435718874111458, 29.06628583063843152, -9.188101187500006262 ) ) ;
#62442 = CARTESIAN_POINT ( 'NONE',  ( 187.0083344850037008, 268.0836409071914090, -15.22627500120235133 ) ) ;
#62443 = CARTESIAN_POINT ( 'NONE',  ( 185.2872327023346486, 260.3622127835997162, 6.490969198090009051 ) ) ;
#62444 = CARTESIAN_POINT ( 'NONE',  ( 205.9642072045669465, 273.9065239114831911, 10.22128930895731536 ) ) ;
#62445 = CARTESIAN_POINT ( 'NONE',  ( 187.1191678700340049, 259.2397217809819381, -2.406884300832496493 ) ) ;
#62446 = CARTESIAN_POINT ( 'NONE',  ( 66.24548473545846150, 68.62659743099872856, 2.338129593227180614 ) ) ;
#62447 = ORIENTED_EDGE ( 'NONE', *, *, #25630, .T. ) ;
#62448 = DIRECTION ( 'NONE',  ( 0.000000000000000000, 0.000000000000000000, 1.000000000000000000 ) ) ;
#62449 =( NAMED_UNIT ( * ) SI_UNIT ( $, .STERADIAN. ) SOLID_ANGLE_UNIT ( ) );
#62450 = EDGE_CURVE ( 'NONE', #46528, #66065, #28857, .T. ) ;
#62451 = CARTESIAN_POINT ( 'NONE',  ( 178.8256996136875046, 285.6663809771316096, 13.03525068864620629 ) ) ;
#62452 = CARTESIAN_POINT ( 'NONE',  ( 66.97748580466556234, 68.05911003901715617, 6.908000617270676713 ) ) ;
#62453 = CARTESIAN_POINT ( 'NONE',  ( 13.11890841201833169, 13.28920272979925166, -7.433330006724141015 ) ) ;
#62454 = VERTEX_POINT ( 'NONE', #47123 ) ;
#62455 = CARTESIAN_POINT ( 'NONE',  ( 206.6658056343182182, 272.6913197846437242, 8.075000410244337345 ) ) ;
#62456 = VECTOR ( 'NONE', #38583, 1000.000000000000227 ) ;
#62457 = CARTESIAN_POINT ( 'NONE',  ( 198.2505066714982149, 285.2670451491296149, 0.000000000000000000 ) ) ;
#62458 = CARTESIAN_POINT ( 'NONE',  ( -15.61417992190811077, 23.18166087982998391, 177.5919119679930134 ) ) ;
#62459 = FACE_OUTER_BOUND ( 'NONE', #43204, .T. ) ;
#62460 = VECTOR ( 'NONE', #65305, 1000.000000000000000 ) ;
#62461 = CARTESIAN_POINT ( 'NONE',  ( -19.65312891409030271, 93.06504152958497400, 177.5919119679930134 ) ) ;
#62462 = CARTESIAN_POINT ( 'NONE',  ( 162.6341128535665064, 248.9564488241690299, -10.63508949045170660 ) ) ;
#62463 = CARTESIAN_POINT ( 'NONE',  ( 152.7691010214056462, 266.0431505347400503, -16.40662330462167162 ) ) ;
#62464 = ORIENTED_EDGE ( 'NONE', *, *, #67698, .T. ) ;
#62465 = VERTEX_POINT ( 'NONE', #39502 ) ;
#62466 = LINE ( 'NONE', #26010, #42202 ) ;
#62467 = CARTESIAN_POINT ( 'NONE',  ( 191.3455589609127117, 293.0590026861491424, 14.61618767810703368 ) ) ;
#62468 = ORIENTED_EDGE ( 'NONE', *, *, #58622, .F. ) ;
#62469 = CARTESIAN_POINT ( 'NONE',  ( 26.55243232390424879, 15.73415679381822585, 1.333680081654574804E-15 ) ) ;
#62470 = LINE ( 'NONE', #72115, #3134 ) ;
#62471 = ORIENTED_EDGE ( 'NONE', *, *, #28439, .F. ) ;
#62472 = DIRECTION ( 'NONE',  ( -0.8660254037844387076, -0.4999999999999998890, -0.000000000000000000 ) ) ;
#62473 = DIRECTION ( 'NONE',  ( -0.8660254037844387076, -0.4999999999999998890, -0.000000000000000000 ) ) ;
#62474 = B_SPLINE_CURVE_WITH_KNOTS ( 'NONE', 3,
 ( #50587, #66303, #80045, #64812 ),
 .UNSPECIFIED., .F., .F.,
 ( 4, 4 ),
 ( 0.01047594276644663036, 0.01576736478584307016 ),
 .UNSPECIFIED. ) ;
#62475 = CARTESIAN_POINT ( 'NONE',  ( 149.6191398986701415, 271.4990432411842676, -11.66821883946526839 ) ) ;
#62476 = CARTESIAN_POINT ( 'NONE',  ( -19.56945998093726047, 92.95052843746097437, 59.99999999999999289 ) ) ;
#62477 = CARTESIAN_POINT ( 'NONE',  ( 69.42765538681520354, 62.69932690130006137, 13.22847919835291997 ) ) ;
#62478 = ORIENTED_EDGE ( 'NONE', *, *, #1243, .F. ) ;
#62479 = CARTESIAN_POINT ( 'NONE',  ( 203.5973318405936823, 278.0060722970681582, 15.26090353908968211 ) ) ;
#62480 = CARTESIAN_POINT ( 'NONE',  ( 182.1983635332545646, 295.7656116556308916, 4.955917269626422872 ) ) ;
#62481 = CARTESIAN_POINT ( 'NONE',  ( 191.2645787786270262, 299.3670271975948367, 7.309947121636420242 ) ) ;
#62482 = DIRECTION ( 'NONE',  ( -0.8660254037844378194, -0.5000000000000014433, -0.000000000000000000 ) ) ;
#62483 = ORIENTED_EDGE ( 'NONE', *, *, #66634, .T. ) ;
#62484 = ORIENTED_EDGE ( 'NONE', *, *, #95995, .F. ) ;
#62485 = ORIENTED_EDGE ( 'NONE', *, *, #86480, .T. ) ;
#62486 = CARTESIAN_POINT ( 'NONE',  ( 72.49386282319785835, 57.57572440859879492, 15.80166580940835885 ) ) ;
#62487 = VERTEX_POINT ( 'NONE', #7124 ) ;
#62488 = DIRECTION ( 'NONE',  ( -0.9874733399847777093, -0.1577859398657163736, 0.000000000000000000 ) ) ;
#62489 = ORIENTED_EDGE ( 'NONE', *, *, #63745, .T. ) ;
#62490 = CARTESIAN_POINT ( 'NONE',  ( 163.7183543885751078, 247.0784873978576854, -6.786164904910574336 ) ) ;
#62491 = CARTESIAN_POINT ( 'NONE',  ( 83.77234465117980733, 51.52744445023363795, 14.35368014269928771 ) ) ;
#62492 = CARTESIAN_POINT ( 'NONE',  ( 167.0546803224166297, 282.1702852132879684, 12.27869116404093752 ) ) ;
#62493 = CARTESIAN_POINT ( 'NONE',  ( 194.6943296385021824, 293.4265244509877562, -16.10917128197217352 ) ) ;
#62494 = CARTESIAN_POINT ( 'NONE',  ( 82.39556149134112673, 53.49063599510539291, -15.76428462505608330 ) ) ;
#62495 = DIRECTION ( 'NONE',  ( 0.000000000000000000, 0.000000000000000000, 1.000000000000000000 ) ) ;
#62496 = CARTESIAN_POINT ( 'NONE',  ( 78.91703011957858394, 55.68952724942787569, -16.53731823143577628 ) ) ;
#62497 = CARTESIAN_POINT ( 'NONE',  ( 18.92729281690869314, 22.87878583063841020, -9.188101187500006262 ) ) ;
#62498 = VECTOR ( 'NONE', #47586, 1000.000000000000000 ) ;
#62499 = CARTESIAN_POINT ( 'NONE',  ( 199.1397118623803522, 277.8245601848594220, -15.39428571812815960 ) ) ;
#62500 = B_SPLINE_CURVE_WITH_KNOTS ( 'NONE', 3,
 ( #60821, #68934, #99860, #69441, #62834, #46121, #1564, #56233, #31931, #86204 ),
 .UNSPECIFIED., .F., .F.,
 ( 4, 2, 2, 2, 4 ),
 ( 0.000000000000000000, 0.2500000000000000000, 0.5000000000000000000, 0.7500000000000000000, 1.000000000000000000 ),
 .UNSPECIFIED. ) ;
#62501 = CARTESIAN_POINT ( 'NONE',  ( 80.71776722511965829, 57.44908488972237848, 16.57971273854667515 ) ) ;
#62503 = ORIENTED_EDGE ( 'NONE', *, *, #95305, .T. ) ;
#62502 = CARTESIAN_POINT ( 'NONE',  ( 206.9717321439337070, 271.7310522289461119, 5.619150226236434342 ) ) ;
#62504 = VECTOR ( 'NONE', #83004, 1000.000000000000000 ) ;
#62505 = CARTESIAN_POINT ( 'NONE',  ( 191.1000974364045533, 299.6519172392214614, 6.286483878122098190 ) ) ;
#62506 = DIRECTION ( 'NONE',  ( 0.4999999999999992784, -0.8660254037844390407, 0.000000000000000000 ) ) ;
#62507 = CARTESIAN_POINT ( 'NONE',  ( 159.2536436069973718, 254.8115933126508992, -15.76697951715411250 ) ) ;
#62508 = FACE_OUTER_BOUND ( 'NONE', #31846, .T. ) ;
#62509 = EDGE_CURVE ( 'NONE', #34846, #24668, #65099, .T. ) ;
#62510 = AXIS2_PLACEMENT_3D ( 'NONE', #76264, #6836, #27672 ) ;
#62511 = CARTESIAN_POINT ( 'NONE',  ( 82.74931449563905517, 45.88034904727371099, -10.83867196349580375 ) ) ;
#62512 = CARTESIAN_POINT ( 'NONE',  ( 161.4844649541891499, 250.9476973967054789, 12.93553496455142415 ) ) ;
#62513 = EDGE_CURVE ( 'NONE', #33184, #93443, #43376, .T. ) ;
#62514 = CARTESIAN_POINT ( 'NONE',  ( 71.81026643095458439, 59.04125517816913771, 15.87515779228373525 ) ) ;
#62515 = ORIENTED_EDGE ( 'NONE', *, *, #27586, .F. ) ;
#62516 = CARTESIAN_POINT ( 'NONE',  ( 194.0381243828431650, 294.5631052939833125, -15.60241059258410345 ) ) ;
#62517 = CARTESIAN_POINT ( 'NONE',  ( 74.96814850772597083, 66.86370092720996183, -13.20453066047568846 ) ) ;
#62518 = CARTESIAN_POINT ( 'NONE',  ( -46.31994871380127421, 28.06264584988120347, 10.00000000000000000 ) ) ;
#62519 = EDGE_CURVE ( 'NONE', #77581, #941, #99031, .T. ) ;
#62520 = CARTESIAN_POINT ( 'NONE',  ( 21.07736754015083491, 189.6427522451419350, -10.00000000000009415 ) ) ;
#62521 = CARTESIAN_POINT ( 'NONE',  ( 86.31820828217628616, 211.4548013555409796, -4.594050593750042211 ) ) ;
#62522 = CARTESIAN_POINT ( 'NONE',  ( 82.35750029267607886, 40.37841760621454057, -1.251208198262858229 ) ) ;
#62523 = B_SPLINE_CURVE_WITH_KNOTS ( 'NONE', 3,
 ( #718, #30125, #61518, #53905, #31606, #61008, #8329, #1230, #15405, #62496, #70109, #46299, #91980, #24018, #77746, #22530 ),
 .UNSPECIFIED., .F., .F.,
 ( 4, 1, 2, 2, 2, 1, 2, 2, 4 ),
 ( 0.000000000000000000, 0.1250000000000004996, 0.1874999999999985290, 0.2499999999999965583, 0.4999999999999943379, 0.6249999999999932276, 0.6874999999999927836, 0.7499999999999922284, 1.000000000000000000 ),
 .UNSPECIFIED. ) ;
#62524 = DIRECTION ( 'NONE',  ( -0.8660254037844387076, -0.4999999999999998890, -0.000000000000000000 ) ) ;
#62525 = CARTESIAN_POINT ( 'NONE',  ( 167.0653908164138386, 277.9579550851513545, -13.96737994587077125 ) ) ;
#62526 = CARTESIAN_POINT ( 'NONE',  ( 72.94747830045673709, 70.90780099059745112, 7.943658523256111437 ) ) ;
#62528 = CARTESIAN_POINT ( 'NONE',  ( 75.51640727855378543, 65.37558461351387962, 13.86249185021059738 ) ) ;
#62527 = CARTESIAN_POINT ( 'NONE',  ( 16.17015057563676450, 170.9548013555409796, -4.594050593750042211 ) ) ;
#62529 = CARTESIAN_POINT ( 'NONE',  ( 200.5438717407500917, 283.2948203288816558, 18.39667691545567152 ) ) ;
#62530 = VECTOR ( 'NONE', #84297, 1000.000000000000000 ) ;
#62531 = VERTEX_POINT ( 'NONE', #95787 ) ;
#62532 = AXIS2_PLACEMENT_3D ( 'NONE', #91471, #36234, #59521 ) ;
#62533 = ORIENTED_EDGE ( 'NONE', *, *, #55089, .F. ) ;
#62534 = DIRECTION ( 'NONE',  ( 0.4330127018922195758, 0.2500000000000004441, 0.8660254037844384856 ) ) ;
#62535 = CARTESIAN_POINT ( 'NONE',  ( 199.5099933602457725, 266.9753653439566392, -2.851387091630914750 ) ) ;
#62536 = CARTESIAN_POINT ( 'NONE',  ( 82.03968029452317978, 46.65024194024377380, -11.88741162480429381 ) ) ;
#62537 = VECTOR ( 'NONE', #30931, 1000.000000000000000 ) ;
#62538 = CARTESIAN_POINT ( 'NONE',  ( 207.1572261440131797, 271.8401544939704877, -5.633070628900782140 ) ) ;
#62539 = CARTESIAN_POINT ( 'NONE',  ( 154.2853090730916676, 265.4170011543745886, 17.16471700533586642 ) ) ;
#62540 = CARTESIAN_POINT ( 'NONE',  ( 74.13858531873714242, 68.40778981217252408, -11.66187469989377767 ) ) ;
#62541 = CARTESIAN_POINT ( 'NONE',  ( 39.44458330234355969, 184.3923013555410080, 4.594050593750050204 ) ) ;
#62542 = CARTESIAN_POINT ( 'NONE',  ( 199.4811141560337830, 277.5223964234930349, 15.18207637411607713 ) ) ;
#62543 = ORIENTED_EDGE ( 'NONE', *, *, #60560, .F. ) ;
#62544 = CARTESIAN_POINT ( 'NONE',  ( 152.7370761390478719, 273.3427822079428324, -11.76210696558454494 ) ) ;
#62545 = CARTESIAN_POINT ( 'NONE',  ( 182.5577216196124368, 260.8327824712812344, -10.71828994691334991 ) ) ;
#62546 = CARTESIAN_POINT ( 'NONE',  ( -15.46727382606978374, 168.0024278399160664, -9.188101187500093303 ) ) ;
#62547 = DIRECTION ( 'NONE',  ( 0.000000000000000000, 0.000000000000000000, 1.000000000000000000 ) ) ;
#62548 = CARTESIAN_POINT ( 'NONE',  ( 155.4812142336614329, 261.3456326552338282, 18.45193178807985745 ) ) ;
#62549 = CARTESIAN_POINT ( 'NONE',  ( 161.8839333999304415, 250.2557977526613229, -13.90128376743482441 ) ) ;
#62550 = CARTESIAN_POINT ( 'NONE',  ( 186.2937303235093509, 283.1136418602877143, 16.27610940549458363 ) ) ;
#62551 = CARTESIAN_POINT ( 'NONE',  ( 194.6356465353167948, 293.5281665672507643, -16.13180903283129197 ) ) ;
#62552 = CARTESIAN_POINT ( 'NONE',  ( 188.2775767336528077, 300.0131076322000467, 1.527577962863595928 ) ) ;
#62553 = CARTESIAN_POINT ( 'NONE',  ( 168.6822647293072919, 279.1257522418852659, 15.04337825401500872 ) ) ;
#62554 = CARTESIAN_POINT ( 'NONE',  ( 192.9401904040553575, 264.5424255672033382, 8.944766451130574225 ) ) ;
#62555 = CARTESIAN_POINT ( 'NONE',  ( 191.0862225170008628, 299.6759493045793192, -9.402218231374108726 ) ) ;
#62556 = CARTESIAN_POINT ( 'NONE',  ( 189.8123550829396891, 301.8823524224806647, -0.5679054518196169354 ) ) ;
#62557 = CARTESIAN_POINT ( 'NONE',  ( 152.8593402092683959, 275.2840601128194749, 10.96293945604634068 ) ) ;
#62558 = ORIENTED_EDGE ( 'NONE', *, *, #20338, .T. ) ;
#62559 = DIRECTION ( 'NONE',  ( 0.000000000000000000, 0.000000000000000000, 1.000000000000000000 ) ) ;
#62560 = DIRECTION ( 'NONE',  ( 0.2091919045418403900, 0.9778746070300412541, 0.000000000000000000 ) ) ;
#62561 = CARTESIAN_POINT ( 'NONE',  ( 117.8198823448352499, 229.6423013555409796, -4.594050593750043987 ) ) ;
#62562 = CARTESIAN_POINT ( 'NONE',  ( 10.75418485208671981, 27.18502408145590010, 5.678558825948277544 ) ) ;
#62563 = CARTESIAN_POINT ( 'NONE',  ( 191.5694344253287511, 298.8390017285333897, 8.250976118904059575 ) ) ;
#62564 = FACE_OUTER_BOUND ( 'NONE', #84517, .T. ) ;
#62566 = CARTESIAN_POINT ( 'NONE',  ( 195.4573685308723725, 278.6848871218847989, 16.36961590483237927 ) ) ;
#62565 = CARTESIAN_POINT ( 'NONE',  ( 196.0727848089514964, 291.0389700598140621, 17.56388901715066808 ) ) ;
#62567 = CARTESIAN_POINT ( 'NONE',  ( 150.9461593943442494, 269.2005780520424878, -15.05333791105169183 ) ) ;
#62568 = CARTESIAN_POINT ( 'NONE',  ( 192.8878213245067741, 263.8246972048095245, -4.383899104128338386 ) ) ;
#62569 = CARTESIAN_POINT ( 'NONE',  ( -19.65312891409030271, 93.06504152958497400, 10.00000000000000888 ) ) ;
#62571 = EDGE_CURVE ( 'NONE', #25248, #1860, #25851, .T. ) ;
#62570 = AXIS2_PLACEMENT_3D ( 'NONE', #43192, #4729, #97437 ) ;
#62572 = LINE ( 'NONE', #94036, #88032 ) ;
#62573 = CARTESIAN_POINT ( 'NONE',  ( 192.4172326059820648, 297.3705722050773943, -12.52563289807247848 ) ) ;
#62574 = CARTESIAN_POINT ( 'NONE',  ( 86.06077315872715872, 47.66653318574839204, 10.87392282977397784 ) ) ;
#62575 = ORIENTED_EDGE ( 'NONE', *, *, #67570, .F. ) ;
#62576 = CARTESIAN_POINT ( 'NONE',  ( 192.2904205063093457, 267.0998989569302466, 11.00927096432294405 ) ) ;
#62577 = CARTESIAN_POINT ( 'NONE',  ( 178.5783945668096635, 280.6919621351586898, 16.55962231343580982 ) ) ;
#62578 = VECTOR ( 'NONE', #7952, 1000.000000000000000 ) ;
#62579 = CARTESIAN_POINT ( 'NONE',  ( 198.5628662595931928, 269.3592121023095274, 9.255750010703465591 ) ) ;
#62580 = ORIENTED_EDGE ( 'NONE', *, *, #93453, .T. ) ;
#62581 = B_SPLINE_CURVE_WITH_KNOTS ( 'NONE', 3,
 ( #68578, #38674, #54872, #7275 ),
 .UNSPECIFIED., .F., .F.,
 ( 4, 4 ),
 ( 0.000000000000000000, 0.0004986248048571736676 ),
 .UNSPECIFIED. ) ;
#62582 = B_SPLINE_SURFACE_WITH_KNOTS ( 'NONE', 3, 1, ( 
 ( #13230, #51723 ),
 ( #90763, #44085 ),
 ( #29409, #92253 ),
 ( #52192, #60278 ),
 ( #84636, #14207 ),
 ( #37483, #68394 ),
 ( #60772, #21313 ),
 ( #45584, #76033 ),
 ( #6610, #13 ),
 ( #53199, #98326 ),
 ( #83648, #99814 ),
 ( #99319, #82666 ),
 ( #29899, #91736 ),
 ( #68887, #75027 ),
 ( #5607, #28919 ),
 ( #22299, #76511 ),
 ( #7094, #30397 ),
 ( #15176, #76989 ),
 ( #7596, #38483 ),
 ( #69397, #30897 ),
 ( #92731, #54171 ),
 ( #70392, #17706 ),
 ( #85140, #15687 ),
 ( #63294, #55669 ),
 ( #62274, #93229 ),
 ( #23283, #54674 ),
 ( #46580, #16696 ),
 ( #77517, #24303 ),
 ( #8108, #38983 ),
 ( #500, #69888 ),
 ( #87172, #1003 ) ),
 .UNSPECIFIED., .F., .F., .F.,
 ( 4, 3, 3, 3, 3, 3, 3, 3, 3, 3, 4 ),
 ( 2, 2 ),
 ( 0.000000000000000000, 0.1333490885032278528, 0.3007194338854267679, 0.4699862290245069296, 0.5844252810809245080, 0.6686540514502667953, 0.7354980260655522573, 0.8028463152565803451, 0.8633854507757331431, 0.9437142632667367970, 1.000000000000000000 ),
 ( 0.000000000000000000, 1.000000000000000000 ),
 .UNSPECIFIED. ) ;
#62583 = CARTESIAN_POINT ( 'NONE',  ( 75.89038410296754478, 65.15355031958958421, -14.48133090960389069 ) ) ;
#62585 = EDGE_CURVE ( 'NONE', #27498, #32613, #48232, .T. ) ;
#62584 = CARTESIAN_POINT ( 'NONE',  ( 179.9482942753538737, 262.6328355063881190, -12.71399655598229472 ) ) ;
#62586 = CARTESIAN_POINT ( 'NONE',  ( 72.39511741677974044, 71.78066914166659274, -5.650358525013035482 ) ) ;
#62587 = CARTESIAN_POINT ( 'NONE',  ( 149.9888573361949398, 250.7365022471902023, -10.00000000000009059 ) ) ;
#62588 = CIRCLE ( 'NONE', #96643, 70.00000000000001421 ) ;
#62589 =( BOUNDED_CURVE ( )  B_SPLINE_CURVE ( 2, ( #70983, #69461, #32468, #9168, #8663, #54235, #55241, #85205, #93809 ),
 .UNSPECIFIED., .F., .T. ) 
 B_SPLINE_CURVE_WITH_KNOTS ( ( 3, 2, 2, 2, 3 ),
 ( 0.2056451612903225923, 0.2069892473118279674, 0.2096774193548387177, 0.2123655913978494680, 0.2137096774193548432 ),
 .UNSPECIFIED. ) 
 CURVE ( )  GEOMETRIC_REPRESENTATION_ITEM ( )  RATIONAL_B_SPLINE_CURVE ( ( 0.9330127018922194093, 0.9330127018922194093, 1.000000000000000000, 0.8660254037844387076, 1.000000000000000000, 0.8660254037844387076, 1.000000000000000000, 0.9330127018922194093, 0.9330127018922194093 ) ) 
 REPRESENTATION_ITEM ( '' )  );
#62590 = VERTEX_POINT ( 'NONE', #27828 ) ;
#62591 = CARTESIAN_POINT ( 'NONE',  ( 73.22997076551303053, 69.87431308930813145, 9.604659174840600500 ) ) ;
#62592 = AXIS2_PLACEMENT_3D ( 'NONE', #5891, #90545, #35291 ) ;
#62593 = CARTESIAN_POINT ( 'NONE',  ( 33.72069078606260462, 37.65586893147758474, -7.433330006724137462 ) ) ;
#62594 = ORIENTED_EDGE ( 'NONE', *, *, #41133, .T. ) ;
#62595 = CARTESIAN_POINT ( 'NONE',  ( 167.6412282369280433, 249.8708500537493933, 6.876476337372752212 ) ) ;
#62596 = EDGE_CURVE ( 'NONE', #74262, #44920, #76066, .T. ) ;
#62597 = DIRECTION ( 'NONE',  ( -0.8660254037844380415, -0.5000000000000009992, 0.000000000000000000 ) ) ;
#62598 = CARTESIAN_POINT ( 'NONE',  ( 81.68695031315317578, 44.07415216466816332, -10.32458475606733650 ) ) ;
#62599 = ORIENTED_EDGE ( 'NONE', *, *, #69580, .F. ) ;
#62600 = CARTESIAN_POINT ( 'NONE',  ( 86.48326989762649930, 47.07371192975631402, -10.55119608217691507 ) ) ;
#62601 = CARTESIAN_POINT ( 'NONE',  ( 159.1291222501505445, 255.0272706293370106, 16.74886675395809021 ) ) ;
#62602 = CARTESIAN_POINT ( 'NONE',  ( 192.5550983588679514, 297.1317817164552935, -12.35927356157043278 ) ) ;
#62603 = CARTESIAN_POINT ( 'NONE',  ( 27.95316317257044858, 17.10801979619929725, 3.090169943749476733 ) ) ;
#62604 = CARTESIAN_POINT ( 'NONE',  ( 42.85004829832549689, 33.24335787977766898, -9.188101187500008038 ) ) ;
#62605 = VECTOR ( 'NONE', #81495, 1000.000000000000000 ) ;
#62606 = CARTESIAN_POINT ( 'NONE',  ( 203.1705638993064156, 278.7452560544191442, -15.08126533799095093 ) ) ;
#62607 = VERTEX_POINT ( 'NONE', #98749 ) ;
#62608 = VERTEX_POINT ( 'NONE', #27339 ) ;
#62609 = CARTESIAN_POINT ( 'NONE',  ( 175.1299035677911036, 258.4933098028565155, 12.91181667424501711 ) ) ;
#62610 = ORIENTED_EDGE ( 'NONE', *, *, #62050, .T. ) ;
#62611 = CARTESIAN_POINT ( 'NONE',  ( 77.18140344432271149, 49.55420220550890065, -15.47549763322615668 ) ) ;
#62612 = ORIENTED_EDGE ( 'NONE', *, *, #20214, .F. ) ;
#62613 = CARTESIAN_POINT ( 'NONE',  ( 162.7505971618529088, 252.7026393492068905, 14.43551447597413961 ) ) ;
#62614 = CARTESIAN_POINT ( 'NONE',  ( 203.5477091018662748, 278.0920214017542662, -16.09930363698006062 ) ) ;
#62615 = ORIENTED_EDGE ( 'NONE', *, *, #17566, .F. ) ;
#62616 = FACE_BOUND ( 'NONE', #99193, .T. ) ;
#62617 = CARTESIAN_POINT ( 'NONE',  ( 206.1670584421323724, 273.5551752616418639, -11.23038754588519694 ) ) ;
#62618 = CARTESIAN_POINT ( 'NONE',  ( 147.9200371497832123, 274.4419755295365917, -6.891776270191406262 ) ) ;
#62619 = FACE_OUTER_BOUND ( 'NONE', #9559, .T. ) ;
#62620 = CARTESIAN_POINT ( 'NONE',  ( 82.39843561648048365, 40.93538189525752813, 1.011552965053796438 ) ) ;
#62621 = CARTESIAN_POINT ( 'NONE',  ( 190.1758200331204876, 279.2204749713225169, -17.78067544974210890 ) ) ;
#62622 = CARTESIAN_POINT ( 'NONE',  ( 55.54027346828191725, 191.3262482093457777, 3.021315404115420679E-15 ) ) ;
#62623 = CARTESIAN_POINT ( 'NONE',  ( 156.1956445759811345, 280.1375863634569328, 2.096082644243150384 ) ) ;
#62624 = CARTESIAN_POINT ( 'NONE',  ( 118.6312605172356598, 248.4869531367911293, 4.594050593750046652 ) ) ;
#62625 = CARTESIAN_POINT ( 'NONE',  ( 187.1031252671867833, 262.0538351896231575, -10.23227223353319992 ) ) ;
#62626 = CARTESIAN_POINT ( 'NONE',  ( 41.28156676870083430, 26.76004757982093452, 5.678558825948272215 ) ) ;
#62627 = VERTEX_POINT ( 'NONE', #58220 ) ;
#62628 = CARTESIAN_POINT ( 'NONE',  ( 27.43138059761190206, 24.03677371833803278, 10.00000000000000533 ) ) ;
#62629 = CARTESIAN_POINT ( 'NONE',  ( 203.6365213803127574, 276.2628368528385749, 13.36267271551829339 ) ) ;
#62630 = EDGE_CURVE ( 'NONE', #77358, #11342, #12646, .T. ) ;
#62631 = CARTESIAN_POINT ( 'NONE',  ( 170.9811431790156462, 280.9458665424763240, 14.82329785628973440 ) ) ;
#62632 = PLANE ( 'NONE',  #88489 ) ;
#62633 = CARTESIAN_POINT ( 'NONE',  ( 69.93330931759959412, 71.50341667604121199, 8.155205941333377477E-06 ) ) ;
#62634 = CARTESIAN_POINT ( 'NONE',  ( -13.11024591527734451, 0.000000000000000000, -20.00000000000000000 ) ) ;
#62635 = CARTESIAN_POINT ( 'NONE',  ( 41.50249547274756878, 124.4848494355456836, -10.00000000000000000 ) ) ;
#62636 = CARTESIAN_POINT ( 'NONE',  ( 79.23761817010250752, 56.43779631686524567, 16.57197305649037844 ) ) ;
#62637 = CARTESIAN_POINT ( 'NONE',  ( 173.5810627320022945, 281.9567074468304213, 15.04350262901273361 ) ) ;
#62638 = LINE ( 'NONE', #86520, #38368 ) ;
#62639 = VERTEX_POINT ( 'NONE', #19747 ) ;
#62640 = CARTESIAN_POINT ( 'NONE',  ( 148.3025927079438304, 273.7793698660844939, -8.046026357031887954 ) ) ;
#62641 = CARTESIAN_POINT ( 'NONE',  ( 12.62566161797914077, 166.5494855054052152, -2.679491924311248496 ) ) ;
#62642 = VERTEX_POINT ( 'NONE', #67314 ) ;
#62643 = EDGE_CURVE ( 'NONE', #54972, #49538, #33718, .T. ) ;
#62644 = CARTESIAN_POINT ( 'NONE',  ( 188.0677593861371122, 266.1968029486987461, -11.81955941906698726 ) ) ;
#62645 = EDGE_CURVE ( 'NONE', #3137, #9601, #7125, .T. ) ;
#62646 = EDGE_CURVE ( 'NONE', #91958, #9648, #19198, .T. ) ;
#62647 = CARTESIAN_POINT ( 'NONE',  ( 160.1665334620766430, 278.8148693431429592, 10.49729549887374525 ) ) ;
#62648 = CARTESIAN_POINT ( 'NONE',  ( 152.5070194032087727, 266.4970892131865980, -16.37820007917167686 ) ) ;
#62649 = FACE_OUTER_BOUND ( 'NONE', #51932, .T. ) ;
#62650 = AXIS2_PLACEMENT_3D ( 'NONE', #22586, #36784, #59571 ) ;
#62651 = DIRECTION ( 'NONE',  ( -0.7511915808658203852, -0.6600842437418951159, 0.000000000000000000 ) ) ;
#62653 = CARTESIAN_POINT ( 'NONE',  ( 160.6618029133832408, 282.0177171234115576, 6.619462234459586369 ) ) ;
#62652 = CARTESIAN_POINT ( 'NONE',  ( 163.4583656713151356, 282.7452325144295742, -6.635438818464283628 ) ) ;
#62654 = CARTESIAN_POINT ( 'NONE',  ( 153.1627746953036535, 265.3612877299463548, -17.72069958822647351 ) ) ;
#62655 = ORIENTED_EDGE ( 'NONE', *, *, #84547, .T. ) ;
#62657 = CARTESIAN_POINT ( 'NONE',  ( 146.8881680668833951, 276.2292252078784145, 4.973452195244782104 ) ) ;
#62656 = VECTOR ( 'NONE', #92203, 1000.000000000000000 ) ;
#62658 = FACE_BOUND ( 'NONE', #37647, .T. ) ;
#62659 = CARTESIAN_POINT ( 'NONE',  ( 72.63364946472314898, 61.52540385496723019, 15.23333689719127548 ) ) ;
#62660 = CARTESIAN_POINT ( 'NONE',  ( 191.0481485323713571, 274.9721303180398877, -15.73758095991607853 ) ) ;
#62661 = CARTESIAN_POINT ( 'NONE',  ( 9.242171499132833645, 29.30720582267293750, -10.00000000000000000 ) ) ;
#62662 = CARTESIAN_POINT ( 'NONE',  ( 188.5479317267626698, 298.6910045167662133, -3.988169708390922885 ) ) ;
#62663 = CARTESIAN_POINT ( 'NONE',  ( 204.1633547645365638, 275.3510256380408237, 13.36249479004741580 ) ) ;
#62664 = CARTESIAN_POINT ( 'NONE',  ( 74.41008358870023187, 68.25813196090381041, 11.92500230979621634 ) ) ;
#62665 = MECHANICAL_DESIGN_GEOMETRIC_PRESENTATION_REPRESENTATION (  '', ( #98349 ), #1224 ) ;
#62666 = CARTESIAN_POINT ( 'NONE',  ( 74.19679258280018530, 68.60443047759615354, 11.01698511858023721 ) ) ;
#62667 = CARTESIAN_POINT ( 'NONE',  ( 68.77417503162503465, 70.33503179494164215, 0.5183767665663540081 ) ) ;
#62668 = CARTESIAN_POINT ( 'NONE',  ( -2.639098984630277922, 169.2833772461660828, -9.188101187500095079 ) ) ;
#62669 = CARTESIAN_POINT ( 'NONE',  ( 96.71051312758956442, 217.4548013555409511, -4.594050593750042211 ) ) ;
#62670 = DIRECTION ( 'NONE',  ( 0.6833540297821638632, -0.7300871660154544251, 0.000000000000000000 ) ) ;
#62671 = CARTESIAN_POINT ( 'NONE',  ( 147.1034852426517148, 275.8562849197056153, -3.648177088342072327 ) ) ;
#62672 = DIRECTION ( 'NONE',  ( 1.000000000000000000, 0.000000000000000000, 0.000000000000000000 ) ) ;
#62673 = CARTESIAN_POINT ( 'NONE',  ( -27.42236680055714260, 166.5217562850347406, 1.224646799147364892E-15 ) ) ;
#62674 = DIRECTION ( 'NONE',  ( 0.4472135954999574836, 0.7745966692414836263, 0.4472135954999578722 ) ) ;
#62675 = CARTESIAN_POINT ( 'NONE',  ( 84.88336942958184750, 50.06956966849930524, -13.25211461007744695 ) ) ;
#62676 = VECTOR ( 'NONE', #66857, 1000.000000000000227 ) ;
#62677 = CARTESIAN_POINT ( 'NONE',  ( 160.8600223638921705, 264.2357221146763777, 17.82164827449318523 ) ) ;
#62679 = CARTESIAN_POINT ( 'NONE',  ( 76.29262445978407925, 51.36595510716406920, 15.62292352366308634 ) ) ;
#62678 = CARTESIAN_POINT ( 'NONE',  ( 73.36513840663161545, 69.69468182635826281, -9.911920066630193205 ) ) ;
#62680 = CARTESIAN_POINT ( 'NONE',  ( 179.0414368791381321, 290.1589939638860187, 9.426711296681993701 ) ) ;
#62681 = CARTESIAN_POINT ( 'NONE',  ( 165.9936732699065658, 249.2531922495258812, -9.278618579411492817 ) ) ;
#62682 = CARTESIAN_POINT ( 'NONE',  ( 205.5916367843585135, 274.5518348086813489, -12.90939787341577372 ) ) ;
#62683 = CARTESIAN_POINT ( 'NONE',  ( 196.3021893095863959, 290.6416298092292436, 17.45656988653421138 ) ) ;
#62684 = DIRECTION ( 'NONE',  ( -0.8660254037844387076, -0.4999999999999998890, -0.000000000000000000 ) ) ;
#62685 = CARTESIAN_POINT ( 'NONE',  ( 207.7666684749232786, 270.7845694125510931, -6.630926507062123498 ) ) ;
#62686 = CARTESIAN_POINT ( 'NONE',  ( 34.27488675591641965, 202.8464784336661353, 1.353441290958777327E-15 ) ) ;
#62687 = AXIS2_PLACEMENT_3D ( 'NONE', #69307, #52596, #21226 ) ;
#62688 = CARTESIAN_POINT ( 'NONE',  ( 62.31280629920263436, 206.7833772461660828, -9.188101187500095079 ) ) ;
#62689 = DIRECTION ( 'NONE',  ( 0.5778974349098237040, 0.4186690413702433000, -0.7005360722495078685 ) ) ;
#62690 = CARTESIAN_POINT ( 'NONE',  ( 88.33576385398527009, 44.18506255568602370, -0.1374804814267040487 ) ) ;
#62691 = CARTESIAN_POINT ( 'NONE',  ( 85.51062282364698319, 48.96702101389664108, -12.23238128493630583 ) ) ;
#62692 = CARTESIAN_POINT ( 'NONE',  ( -17.22621437785049636, 170.8615022471903160, 5.000000000000046185 ) ) ;
#62693 = CARTESIAN_POINT ( 'NONE',  ( 71.64316818921393804, 72.05741665177616539, -3.509880912999890690 ) ) ;
#62694 = CARTESIAN_POINT ( 'NONE',  ( 14.08495376150009371, 190.4860189848785126, -2.679491924311252493 ) ) ;
#62695 = EDGE_CURVE ( 'NONE', #84442, #62377, #37274, .T. ) ;
#62696 = CARTESIAN_POINT ( 'NONE',  ( 30.35763184873497877, 26.03085787977764198, 9.188101187500006262 ) ) ;
#62697 = CARTESIAN_POINT ( 'NONE',  ( 198.5970767652345899, 286.6667681383942181, -17.17073100918929640 ) ) ;
#62698 = CARTESIAN_POINT ( 'NONE',  ( 196.4501996009505831, 290.3852684645433442, -17.82325615854289680 ) ) ;
#62699 = CARTESIAN_POINT ( 'NONE',  ( 8.146472837920740062, 20.10171378149916777, 9.188101187500008038 ) ) ;
#62700 = CARTESIAN_POINT ( 'NONE',  ( 68.75404378773188796, 204.3768266524160140, 9.188101187500096856 ) ) ;
#62701 = CARTESIAN_POINT ( 'NONE',  ( 77.07103148522583069, 63.64506183647083759, 15.39324216548719626 ) ) ;
#62702 = LINE ( 'NONE', #40401, #70434 ) ;
#62703 = CARTESIAN_POINT ( 'NONE',  ( 159.6610344727618269, 254.1059716346071866, 15.33388637456589620 ) ) ;
#62704 = CARTESIAN_POINT ( 'NONE',  ( 69.81582973455007846, 63.14295414310246457, -13.67321376818635059 ) ) ;
#62705 = CARTESIAN_POINT ( 'NONE',  ( -33.75225536883274913, 24.49963747467413810, 10.00000000000000000 ) ) ;
#62706 = EDGE_CURVE ( 'NONE', #24773, #16945, #85052, .T. ) ;
#62707 = CARTESIAN_POINT ( 'NONE',  ( 117.0077232087375734, 228.3615022471901739, 5.000000000000051514 ) ) ;
#62708 = CARTESIAN_POINT ( 'NONE',  ( 200.6129772034685175, 283.1751261563724142, 18.36811917402039640 ) ) ;
#62709 = CARTESIAN_POINT ( 'NONE',  ( 207.3502731283117555, 271.5057873089173768, 6.280625384230454245 ) ) ;
#62710 = VERTEX_POINT ( 'NONE', #45992 ) ;
#62711 = CARTESIAN_POINT ( 'NONE',  ( 77.52094420404428377, 49.23844290216526787, 15.29553459438156793 ) ) ;
#62712 = AXIS2_PLACEMENT_3D ( 'NONE', #66787, #30281, #77392 ) ;
#62713 = CARTESIAN_POINT ( 'NONE',  ( 184.8664429911153206, 271.3566499112901624, 16.06020675104017670 ) ) ;
#62714 = ORIENTED_EDGE ( 'NONE', *, *, #22537, .F. ) ;
#62715 = CARTESIAN_POINT ( 'NONE',  ( 206.3454060440500086, 273.2462681537123785, -9.268083217908118954 ) ) ;
#62716 = CARTESIAN_POINT ( 'NONE',  ( 187.6832578813660177, 277.1412041823390382, -16.69151914137464487 ) ) ;
#62717 = ADVANCED_FACE ( 'NONE', ( #23699 ), #67587, .T. ) ;
#62718 = CARTESIAN_POINT ( 'NONE',  ( 67.67030795740730298, 68.61334932093440386, -5.327093496892230107 ) ) ;
#62719 = VERTEX_POINT ( 'NONE', #18126 ) ;
#62720 = CARTESIAN_POINT ( 'NONE',  ( 175.5613651706662210, 252.8860800517080918, -0.2536904810274192013 ) ) ;
#62721 = ORIENTED_EDGE ( 'NONE', *, *, #52257, .T. ) ;
#62722 = CARTESIAN_POINT ( 'NONE',  ( 76.67567146729665239, 63.34086528488000312, -15.41964329106466103 ) ) ;
#62723 = CARTESIAN_POINT ( 'NONE',  ( 148.2670916631250861, 273.8408594794321971, -7.980554973576580835 ) ) ;
#62724 = CARTESIAN_POINT ( 'NONE',  ( 206.9413969004818057, 271.3616952779818234, -5.376728341096632668 ) ) ;
#62725 = AXIS2_PLACEMENT_3D ( 'NONE', #88290, #57813, #18346 ) ;
#62726 = ORIENTED_EDGE ( 'NONE', *, *, #96617, .F. ) ;
#62727 = CARTESIAN_POINT ( 'NONE',  ( 29.70508255828911004, 19.01110640527293327, 2.839279412974134775 ) ) ;
#62728 = CARTESIAN_POINT ( 'NONE',  ( 202.5650245025327081, 277.7940810556053179, -15.59262966521933791 ) ) ;
#62729 = CARTESIAN_POINT ( 'NONE',  ( -15.61417992190811788, 23.18166087982996970, 10.00000000000000000 ) ) ;
#62730 = EDGE_CURVE ( 'NONE', #31854, #91585, #49027, .T. ) ;
#62731 = ORIENTED_EDGE ( 'NONE', *, *, #76077, .F. ) ;
#62732 = CARTESIAN_POINT ( 'NONE',  ( -13.11024591527734451, 6.000000000000000000, 40.00000000000000000 ) ) ;
#62733 = ADVANCED_FACE ( 'NONE', ( #25736 ), #1434, .F. ) ;
#62734 = CARTESIAN_POINT ( 'NONE',  ( -10.89340361622470610, 174.5177522451419350, 5.000000000000046185 ) ) ;
#62735 = ORIENTED_EDGE ( 'NONE', *, *, #62509, .T. ) ;
#62736 = DIRECTION ( 'NONE',  ( 0.3851501363289905333, -0.9228539280329037808, 0.000000000000000000 ) ) ;
#62737 = AXIS2_PLACEMENT_3D ( 'NONE', #42784, #51912, #4301 ) ;
#62739 = CARTESIAN_POINT ( 'NONE',  ( 67.81340710963647211, 65.98316596844472315, -10.47555129015767683 ) ) ;
#62738 = CARTESIAN_POINT ( 'NONE',  ( 67.85199900019571828, 65.46856307543899334, 10.29293294925176738 ) ) ;
#62740 = CARTESIAN_POINT ( 'NONE',  ( 81.75198846930985042, 55.31526633232800094, -15.92433154267821394 ) ) ;
#62741 = CARTESIAN_POINT ( 'NONE',  ( 193.9401685343300699, 294.7327698005063326, 14.01047396938887069 ) ) ;
#62742 = CARTESIAN_POINT ( 'NONE',  ( 185.1491161497484370, 292.9437783688060222, -11.97406807593424993 ) ) ;
#62743 = CARTESIAN_POINT ( 'NONE',  ( 157.3029956111992362, 258.1902147490555421, -18.22269824972649843 ) ) ;
#62744 = CARTESIAN_POINT ( 'NONE',  ( 141.5541307454787727, 252.5333772461660260, 9.188101187500095079 ) ) ;
#62745 = CARTESIAN_POINT ( 'NONE',  ( 162.7006039569504594, 261.3497057169571463, 17.57720365097131676 ) ) ;
#62746 = AXIS2_PLACEMENT_3D ( 'NONE', #2982, #34348, #55625 ) ;
#62747 = CARTESIAN_POINT ( 'NONE',  ( 179.7049408000989956, 258.9102790531361507, 9.610927518812550474 ) ) ;
#62748 = CARTESIAN_POINT ( 'NONE',  ( 80.71549903385694336, 229.6589784336661637, -6.496448406907675876E-16 ) ) ;
#62749 = ORIENTED_EDGE ( 'NONE', *, *, #62199, .T. ) ;
#62750 = CARTESIAN_POINT ( 'NONE',  ( 190.7779368023172708, 300.2099158256590385, 8.142228434510803581 ) ) ;
#62751 = CARTESIAN_POINT ( 'NONE',  ( -64.74139798177010618, 41.16849083240310847, -10.00000000000000000 ) ) ;
#62752 = ORIENTED_EDGE ( 'NONE', *, *, #88375, .F. ) ;
#62753 = CARTESIAN_POINT ( 'NONE',  ( 195.4107521409361539, 292.1856442770869080, -15.96705206423837353 ) ) ;
#62754 = VERTEX_POINT ( 'NONE', #79961 ) ;
#62755 = ORIENTED_EDGE ( 'NONE', *, *, #62181, .T. ) ;
#62756 = EDGE_CURVE ( 'NONE', #86705, #55644, #2277, .T. ) ;
#62757 = CARTESIAN_POINT ( 'NONE',  ( 80.25975942986622158, 44.70959520753981309, -11.72582774008359152 ) ) ;
#62758 = CARTESIAN_POINT ( 'NONE',  ( 81.57285043722427531, 211.2365022471902023, 10.00000000000009948 ) ) ;
#62759 = CARTESIAN_POINT ( 'NONE',  ( 191.6823192895500370, 298.6434794082964572, -8.424208857102787107 ) ) ;
#62760 = LINE ( 'NONE', #16672, #4610 ) ;
#62761 = CARTESIAN_POINT ( 'NONE',  ( 83.27207070336380923, 47.65589845134895342, -12.15996375230644233 ) ) ;
#62762 = CARTESIAN_POINT ( 'NONE',  ( 156.0507216674837707, 279.5060275253360373, 7.618106348741741307 ) ) ;
#62763 = CARTESIAN_POINT ( 'NONE',  ( 78.84873917453550973, 207.1423013555409796, -4.594050593750043987 ) ) ;
#62764 = ORIENTED_EDGE ( 'NONE', *, *, #44773, .F. ) ;
#62765 = EDGE_CURVE ( 'NONE', #52745, #9204, #2953, .T. ) ;
#62766 = VECTOR ( 'NONE', #33221, 1000.000000000000000 ) ;
#62767 = ORIENTED_EDGE ( 'NONE', *, *, #58669, .F. ) ;
#62768 = CARTESIAN_POINT ( 'NONE',  ( 161.7519069501884132, 250.4844742715573886, -14.24248196453219073 ) ) ;
#62769 = ORIENTED_EDGE ( 'NONE', *, *, #75270, .F. ) ;
#62770 = CARTESIAN_POINT ( 'NONE',  ( 15.04662694159776670, 32.18528772668517490, -1.583844403245363575 ) ) ;
#62771 = EDGE_CURVE ( 'NONE', #89587, #73274, #95679, .T. ) ;
#62772 = EDGE_CURVE ( 'NONE', #68451, #49174, #90636, .T. ) ;
#62773 = CARTESIAN_POINT ( 'NONE',  ( 183.8966011539753254, 275.3119708187981018, 16.41707298570698725 ) ) ;
#62774 = EDGE_CURVE ( 'NONE', #85165, #64642, #17626, .T. ) ;
#62775 = CARTESIAN_POINT ( 'NONE',  ( 161.6130071796497418, 284.2796802195229020, 0.5328386277561626416 ) ) ;
#62776 = CARTESIAN_POINT ( 'NONE',  ( 22.87549206224920084, 39.05096577487528720, 10.00000000000000000 ) ) ;
#62777 = CARTESIAN_POINT ( 'NONE',  ( 87.52536710082529225, 44.57545605528624577, 4.902363546664118665 ) ) ;
#62778 = ORIENTED_EDGE ( 'NONE', *, *, #47417, .T. ) ;
#62779 = CARTESIAN_POINT ( 'NONE',  ( 82.01543408846627869, 43.66070079000877513, -8.773935687765517244 ) ) ;
#62780 = ADVANCED_FACE ( 'NONE', ( #9539 ), #58950, .T. ) ;
#62781 = CARTESIAN_POINT ( 'NONE',  ( 36.13333420750807079, 36.56454794089044924, 10.00000000000000355 ) ) ;
#62782 = CARTESIAN_POINT ( 'NONE',  ( 159.6962080797732710, 254.0450491601782232, -15.33973334987084947 ) ) ;
#62783 = ADVANCED_FACE ( 'NONE', ( #70825 ), #71842, .T. ) ;
#62784 = FACE_OUTER_BOUND ( 'NONE', #84309, .T. ) ;
#62785 = DIRECTION ( 'NONE',  ( 0.4999999999999992784, -0.8660254037844390407, 0.000000000000000000 ) ) ;
#62786 = B_SPLINE_CURVE_WITH_KNOTS ( 'NONE', 3,
 ( #44304, #59997, #90966, #52407, #83353, #71125, #85877, #31094 ),
 .UNSPECIFIED., .F., .F.,
 ( 4, 2, 2, 4 ),
 ( 0.4503330015877973214, 0.7251665007938997709, 0.8625832503969499410, 1.000000000000000000 ),
 .UNSPECIFIED. ) ;
#62787 = CARTESIAN_POINT ( 'NONE',  ( 111.2365322456207224, 223.4824982072973683, 3.021315404115420679E-15 ) ) ;
#62788 = CARTESIAN_POINT ( 'NONE',  ( -19.15453390681661716, 24.31945705462846163, -10.00000000000000000 ) ) ;
#62789 = ORIENTED_EDGE ( 'NONE', *, *, #45572, .F. ) ;
#62790 = CARTESIAN_POINT ( 'NONE',  ( 189.7493380202622291, 294.8126471784881915, -12.68491631734921299 ) ) ;
#62791 = CARTESIAN_POINT ( 'NONE',  ( 200.1103929410127762, 284.0456276340304953, 17.67835211026828901 ) ) ;
#62792 = CARTESIAN_POINT ( 'NONE',  ( 85.10088869340128781, 43.69823583396123468, 5.977407741011665721 ) ) ;
#62793 = VECTOR ( 'NONE', #89061, 1000.000000000000000 ) ;
#62794 = CARTESIAN_POINT ( 'NONE',  ( 169.4846735095618442, 250.9656555291483357, 6.963129758109078082 ) ) ;
#62795 = CARTESIAN_POINT ( 'NONE',  ( 83.95452371275135306, 51.84303909528517806, 14.85259985614520062 ) ) ;
#62796 = CARTESIAN_POINT ( 'NONE',  ( 155.8025440274901428, 271.6998552528711457, 14.08447433373405921 ) ) ;
#62797 = ORIENTED_EDGE ( 'NONE', *, *, #64311, .F. ) ;
#62798 = CARTESIAN_POINT ( 'NONE',  ( -14.12737304691700402, 103.0317842862404518, 44.13135102960670508 ) ) ;
#62799 = CIRCLE ( 'NONE', #51459, 0.1418229129684228651 ) ;
#62800 = VECTOR ( 'NONE', #52412, 1000.000000000000227 ) ;
#62801 = CARTESIAN_POINT ( 'NONE',  ( 207.6900289502458179, 270.9173129631602706, 7.178327969100043227 ) ) ;
#62803 = FACE_BOUND ( 'NONE', #60985, .T. ) ;
#62802 = CARTESIAN_POINT ( 'NONE',  ( 155.3017250444513024, 261.6565170503553190, 18.58368563027307374 ) ) ;
#62804 = CARTESIAN_POINT ( 'NONE',  ( 199.1275226280280890, 281.8858470971437100, -16.59877271873514459 ) ) ;
#62805 = CARTESIAN_POINT ( 'NONE',  ( 30.82863370761418054, 19.92755873383627119, 6.180339887498953466 ) ) ;
#62806 = CARTESIAN_POINT ( 'NONE',  ( 165.8896735243662306, 286.5189455822670652, -3.328331710570921143 ) ) ;
#62807 = DIRECTION ( 'NONE',  ( 0.09248003802711829424, -0.9957145386939485476, 0.000000000000000000 ) ) ;
#62808 = CARTESIAN_POINT ( 'NONE',  ( 163.8003088823192286, 260.8948240748503054, -17.39314492925268141 ) ) ;
#62809 = CARTESIAN_POINT ( 'NONE',  ( 195.1808244021223686, 265.5951289396304560, -7.339755448317591302 ) ) ;
#62810 = VECTOR ( 'NONE', #14300, 1000.000000000000000 ) ;
#62811 = CARTESIAN_POINT ( 'NONE',  ( -8.782727014549898570, 174.9244531367911293, -4.594050593750046652 ) ) ;
#62812 = CARTESIAN_POINT ( 'NONE',  ( 73.95673202641080479, 225.0530062829863311, -4.648177544792955347E-16 ) ) ;
#62813 = ORIENTED_EDGE ( 'NONE', *, *, #68461, .F. ) ;
#62814 = AXIS2_PLACEMENT_3D ( 'NONE', #31109, #32111, #79276 ) ;
#62815 = CARTESIAN_POINT ( 'NONE',  ( 178.1796287192598527, 256.8239042684534184, 8.391128143578042042 ) ) ;
#62816 = DIRECTION ( 'NONE',  ( 0.8660254037844387076, 0.4999999999999998890, 0.000000000000000000 ) ) ;
#62817 = CARTESIAN_POINT ( 'NONE',  ( 182.0442112598040580, 290.9601537038038259, 12.16457704577017829 ) ) ;
#62818 = CARTESIAN_POINT ( 'NONE',  ( 23.53136650780448491, 175.2048013555409796, 4.594050593750051981 ) ) ;
#62819 = CARTESIAN_POINT ( 'NONE',  ( 62.88113547221008304, 217.1115022471903160, -5.000000000000047962 ) ) ;
#62820 = CARTESIAN_POINT ( 'NONE',  ( 35.76051414856368638, 25.81029122506296858, 8.090169943749479842 ) ) ;
#62821 = CARTESIAN_POINT ( 'NONE',  ( 78.11027170948028697, 58.64888375189529768, 16.54994857808256015 ) ) ;
#62822 = CARTESIAN_POINT ( 'NONE',  ( 146.7818291168261453, 276.4134096722012828, -0.7617065417431535534 ) ) ;
#62823 = CARTESIAN_POINT ( 'NONE',  ( 135.3927208396967785, 255.6427522451419065, -10.00000000000009592 ) ) ;
#62824 = B_SPLINE_SURFACE_WITH_KNOTS ( 'NONE', 3, 1, ( 
 ( #21112, #5396 ),
 ( #67179, #35788 ),
 ( #50482, #58091 ),
 ( #11519, #89073 ),
 ( #43378, #27203 ),
 ( #51484, #19122 ),
 ( #80953, #65682 ),
 ( #20603, #35288 ),
 ( #19624, #59057 ),
 ( #42864, #81436 ),
 ( #51990, #97139 ),
 ( #66684, #4390 ),
 ( #82452, #90541 ),
 ( #26697, #57582 ),
 ( #58575, #88556 ),
 ( #50978, #13015 ),
 ( #73308, #59566 ),
 ( #36280, #43874 ),
 ( #96638, #44374 ),
 ( #74817, #28185 ),
 ( #74322, #49996 ),
 ( #12006, #98103 ),
 ( #28682, #5887 ),
 ( #82929, #73798 ),
 ( #42375, #27707 ),
 ( #65193, #13505 ),
 ( #89548, #20109 ),
 ( #75306, #96139 ),
 ( #81931, #3899 ),
 ( #34780, #12507 ),
 ( #4905, #97618 ),
 ( #90028, #100098 ),
 ( #46871, #14489 ),
 ( #15969, #77795 ) ),
 .UNSPECIFIED., .T., .F., .F.,
 ( 4, 2, 2, 2, 2, 2, 2, 2, 2, 2, 2, 2, 2, 2, 2, 2, 4 ),
 ( 2, 2 ),
 ( 0.000000000000000000, 0.06250000000000000000, 0.1250000000000000000, 0.1875000000000000000, 0.2500000000000000000, 0.3125000000000000000, 0.3750000000000000000, 0.4375000000000000000, 0.5000000000000000000, 0.5625000000000000000, 0.6250000000000000000, 0.6875000000000000000, 0.7500000000000000000, 0.8125000000000000000, 0.8750000000000000000, 0.9375000000000000000, 1.000000000000000000 ),
 ( 0.000000000000000000, 1.000000000000000000 ),
 .UNSPECIFIED. ) ;
#62825 = CARTESIAN_POINT ( 'NONE',  ( 186.6562845357111087, 296.1148510662804370, -8.718888755099150956 ) ) ;
#62826 = CARTESIAN_POINT ( 'NONE',  ( 187.7495819260542476, 259.1541535816100463, -0.7945162718502817301 ) ) ;
#62827 = CARTESIAN_POINT ( 'NONE',  ( 67.64427519302456915, 199.8615022471901739, 5.000000000000051514 ) ) ;
#62828 = CARTESIAN_POINT ( 'NONE',  ( 68.90019008890776320, 66.82522398943339681, -9.471753670772901756 ) ) ;
#62829 = AXIS2_PLACEMENT_3D ( 'NONE', #84096, #14648, #68334 ) ;
#62830 = CARTESIAN_POINT ( 'NONE',  ( 204.2047590417662093, 270.4847546024170697, 6.040547820020366387 ) ) ;
#62831 = CARTESIAN_POINT ( 'NONE',  ( 39.55283647781661216, 184.4548013555409796, -4.594050593750042211 ) ) ;
#62832 = CARTESIAN_POINT ( 'NONE',  ( 67.86617404580020718, 69.78291350440201768, -3.870024980962481820 ) ) ;
#62833 = CARTESIAN_POINT ( 'NONE',  ( -86.81108781737714253, -8.000000000000000000, -14.21260523776213347 ) ) ;
#62834 = CARTESIAN_POINT ( 'NONE',  ( 77.11858699210218049, 49.43661330258253628, -14.93544102205281554 ) ) ;
#62835 = CARTESIAN_POINT ( 'NONE',  ( 199.1216527653377000, 285.7581758537840528, -18.37739894744384728 ) ) ;
#62836 = EDGE_CURVE ( 'NONE', #73010, #36208, #2440, .T. ) ;
#62837 = PLANE ( 'NONE',  #90411 ) ;
#62838 = CARTESIAN_POINT ( 'NONE',  ( 194.1011995340913074, 294.4538559273262877, 13.93949783759920713 ) ) ;
#62839 = CARTESIAN_POINT ( 'NONE',  ( 73.08094384907833785, 54.14441083166271795, 0.000000000000000000 ) ) ;
#62840 = CARTESIAN_POINT ( 'NONE',  ( 162.6725657724230700, 281.1335366253323400, -10.40723503984205500 ) ) ;
#62841 = CARTESIAN_POINT ( 'NONE',  ( -17.42236680055705023, 149.2012482093457777, 0.000000000000000000 ) ) ;
#62842 = CARTESIAN_POINT ( 'NONE',  ( 16.91979795264450459, 27.95586893147755347, 7.433330006724141015 ) ) ;
#62843 = CARTESIAN_POINT ( 'NONE',  ( 202.2576150004249200, 280.3265299319959354, 16.24828394350762295 ) ) ;
#62844 = CARTESIAN_POINT ( 'NONE',  ( 196.7823306783968746, 289.8100005636337073, -17.85370042640856170 ) ) ;
#62845 = CARTESIAN_POINT ( 'NONE',  ( 185.6575085028373451, 267.5770612294242596, -14.83682210475602581 ) ) ;
#62846 = VERTEX_POINT ( 'NONE', #71337 ) ;
#62847 = CARTESIAN_POINT ( 'NONE',  ( 9.248262631489305718, 13.84335787977760823, 9.188101187500006262 ) ) ;
#62848 = DIRECTION ( 'NONE',  ( -0.8660254037844378194, -0.5000000000000013323, -0.000000000000000000 ) ) ;
#62849 = CARTESIAN_POINT ( 'NONE',  ( 79.25711091567707456, 57.60615597753891137, -16.24568049410854442 ) ) ;
#62850 = CARTESIAN_POINT ( 'NONE',  ( 71.70445494439258027, 72.46184198916859032, -1.357087204883099751 ) ) ;
#62851 = EDGE_CURVE ( 'NONE', #94448, #18147, #56316, .T. ) ;
#62852 = ORIENTED_EDGE ( 'NONE', *, *, #61202, .T. ) ;
#62853 = CARTESIAN_POINT ( 'NONE',  ( 72.27803260052462520, 71.63036165027699553, -5.844549976855538453 ) ) ;
#62854 = DIRECTION ( 'NONE',  ( 0.000000000000000000, 0.000000000000000000, -1.000000000000000000 ) ) ;
#62855 = EDGE_CURVE ( 'NONE', #53789, #78498, #68566, .T. ) ;
#62856 = CARTESIAN_POINT ( 'NONE',  ( 180.6644785651033658, 257.6587254813057370, -7.431609338059112169 ) ) ;
#62857 = ORIENTED_EDGE ( 'NONE', *, *, #21528, .T. ) ;
#62858 = ORIENTED_EDGE ( 'NONE', *, *, #88511, .F. ) ;
#62860 = CARTESIAN_POINT ( 'NONE',  ( 85.86466870016465691, 43.03755298354901981, -2.506393329082034160 ) ) ;
#62859 = CARTESIAN_POINT ( 'NONE',  ( 189.7042809424692393, 274.2741113227406800, -15.67635319055484366 ) ) ;
#62861 = ORIENTED_EDGE ( 'NONE', *, *, #8000, .T. ) ;
#62862 = CARTESIAN_POINT ( 'NONE',  ( 200.8665851640556070, 282.7358642834317948, -16.69422397739980823 ) ) ;
#62863 = CIRCLE ( 'NONE', #70993, 70.00000000000001421 ) ;
#62864 = LINE ( 'NONE', #71495, #65839 ) ;
#62865 = DIRECTION ( 'NONE',  ( 0.5000000000000014433, -0.8660254037844378194, 0.000000000000000000 ) ) ;
#62866 = CARTESIAN_POINT ( 'NONE',  ( 185.2570508126727873, 282.0811717828997303, -17.42469797758589678 ) ) ;
#62867 = CARTESIAN_POINT ( 'NONE',  ( 148.2267527339363369, 273.9107285543102535, 7.913369084260907016 ) ) ;
#62868 = AXIS2_PLACEMENT_3D ( 'NONE', #30042, #60930, #22446 ) ;
#62869 = VECTOR ( 'NONE', #47575, 1000.000000000000000 ) ;
#62870 = CARTESIAN_POINT ( 'NONE',  ( 184.0985169280008620, 289.0250432102490663, -13.04961936838414971 ) ) ;
#62871 = ORIENTED_EDGE ( 'NONE', *, *, #41241, .F. ) ;
#62872 = CARTESIAN_POINT ( 'NONE',  ( 195.8627871995700502, 291.4026965887302936, 17.41145040657729481 ) ) ;
#62873 = AXIS2_PLACEMENT_3D ( 'NONE', #17131, #32830, #69829 ) ;
#62874 = CARTESIAN_POINT ( 'NONE',  ( 160.0114177933981523, 266.1051921132770417, 16.66372494280312111 ) ) ;
#62875 = VERTEX_POINT ( 'NONE', #84318 ) ;
#62876 = CARTESIAN_POINT ( 'NONE',  ( 25.14222138719033595, 29.91421378149919974, 9.188101187500008038 ) ) ;
#62877 = CYLINDRICAL_SURFACE ( 'NONE', #19673, 17.82106496071139645 ) ;
#62878 = CARTESIAN_POINT ( 'NONE',  ( 153.6392919293977002, 266.5359356698173769, -16.75038546547492402 ) ) ;
#62879 = CARTESIAN_POINT ( 'NONE',  ( 61.28457468009112574, 200.0643266524160140, 9.188101187500095079 ) ) ;
#62880 = ORIENTED_EDGE ( 'NONE', *, *, #2424, .T. ) ;
#62881 = CARTESIAN_POINT ( 'NONE',  ( 74.32474745866193189, 68.52230083288840490, 11.65590001247777252 ) ) ;
#62882 = CARTESIAN_POINT ( 'NONE',  ( 92.93017357788669131, 158.0650415295850735, 36.50000000000000000 ) ) ;
#62883 = FACE_OUTER_BOUND ( 'NONE', #55751, .T. ) ;
#62884 = CARTESIAN_POINT ( 'NONE',  ( 175.7055711947306520, 272.7582102363617764, 17.70512484591946034 ) ) ;
#62885 = VERTEX_POINT ( 'NONE', #29094 ) ;
#62886 = CIRCLE ( 'NONE', #90428, 70.00000000000001421 ) ;
#62887 =( BOUNDED_CURVE ( )  B_SPLINE_CURVE ( 2, ( #67379, #26901, #91216, #30381, #52668, #67888, #68866, #84618, #83120 ),
 .UNSPECIFIED., .F., .F. ) 
 B_SPLINE_CURVE_WITH_KNOTS ( ( 3, 2, 2, 2, 3 ),
 ( 0.5604838709677418818, 0.5618279569892472569, 0.5645161290322581182, 0.5672043010752688685, 0.5685483870967742437 ),
 .UNSPECIFIED. ) 
 CURVE ( )  GEOMETRIC_REPRESENTATION_ITEM ( )  RATIONAL_B_SPLINE_CURVE ( ( 0.9330127018922194093, 0.9330127018922194093, 1.000000000000000000, 0.8660254037844387076, 1.000000000000000000, 0.8660254037844387076, 1.000000000000000000, 0.9330127018922194093, 0.9330127018922194093 ) ) 
 REPRESENTATION_ITEM ( '' )  );
#62888 = EDGE_CURVE ( 'NONE', #79874, #7443, #30071, .T. ) ;
#62889 = CARTESIAN_POINT ( 'NONE',  ( 190.4456243223121987, 299.4994646951487880, 6.453196029206972995 ) ) ;
#62890 = CARTESIAN_POINT ( 'NONE',  ( -169.5327448629461742, 46.94652375874896677, 30.52142883766498827 ) ) ;
#62891 = CARTESIAN_POINT ( 'NONE',  ( 172.6727388731993358, 285.6664956175675911, 12.05044444168489548 ) ) ;
#62892 = ORIENTED_EDGE ( 'NONE', *, *, #93761, .T. ) ;
#62893 = CARTESIAN_POINT ( 'NONE',  ( 171.7219487607086990, 259.3602272249703447, -13.79533293788550985 ) ) ;
#62894 = CARTESIAN_POINT ( 'NONE',  ( 140.8234218128096700, 242.1115022471902023, -5.000000000000041744 ) ) ;
#62895 = CARTESIAN_POINT ( 'NONE',  ( 161.8807657183444064, 250.2612843381103573, -13.52770735624900311 ) ) ;
#62896 = CARTESIAN_POINT ( 'NONE',  ( 192.5284579606305613, 297.1779242397361713, -13.15228012403107272 ) ) ;
#62897 = EDGE_CURVE ( 'NONE', #95476, #86521, #15206, .T. ) ;
#62898 = EDGE_CURVE ( 'NONE', #97214, #55984, #69597, .T. ) ;
#62899 = CARTESIAN_POINT ( 'NONE',  ( 190.0340467409721441, 301.4983712071542641, 4.077645795029533282 ) ) ;
#62900 = CARTESIAN_POINT ( 'NONE',  ( 178.1116250315744196, 269.9460939148322041, 16.11468309730568294 ) ) ;
#62901 = AXIS2_PLACEMENT_3D ( 'NONE', #87944, #27083, #17990 ) ;
#62902 = CARTESIAN_POINT ( 'NONE',  ( 206.3907062969896060, 273.1678058140250300, 11.56942460516550675 ) ) ;
#62903 = CARTESIAN_POINT ( 'NONE',  ( 76.10657944533755881, 65.44108555233269442, 13.99905362479801951 ) ) ;
#62904 = CARTESIAN_POINT ( 'NONE',  ( 45.66470909604093720, 114.5311720768849995, -10.00000000000000000 ) ) ;
#62905 = CARTESIAN_POINT ( 'NONE',  ( 163.8398374448017591, 246.8680725722146008, -5.948785025486735378 ) ) ;
#62906 = CARTESIAN_POINT ( 'NONE',  ( 116.3314879560220163, 225.7202760586659736, -5.415160957724236172E-17 ) ) ;
#62907 = VERTEX_POINT ( 'NONE', #45268 ) ;
#62908 = CARTESIAN_POINT ( 'NONE',  ( 146.6138605399200117, 276.7043397814778132, -0.5394499176159462950 ) ) ;
#62909 = CARTESIAN_POINT ( 'NONE',  ( 65.36586985908992631, 182.5653022007868458, 0.000000000000000000 ) ) ;
#62910 = EDGE_CURVE ( 'NONE', #67256, #34021, #30274, .T. ) ;
#62911 = ADVANCED_FACE ( 'NONE', ( #76201 ), #99992, .T. ) ;
#62912 = CARTESIAN_POINT ( 'NONE',  ( 202.8535267948003593, 279.2943804273081696, -15.36804658072946062 ) ) ;
#62913 = CARTESIAN_POINT ( 'NONE',  ( 204.6780326111993986, 276.1342436545999703, 14.85609018352459287 ) ) ;
#62914 = DIRECTION ( 'NONE',  ( 0.4999999999999998890, -0.8660254037844385966, 0.000000000000000000 ) ) ;
#62915 = CARTESIAN_POINT ( 'NONE',  ( 68.45344762042827824, 64.57392882346940155, 12.12708197196866600 ) ) ;
#62916 = ORIENTED_EDGE ( 'NONE', *, *, #77834, .F. ) ;
#62917 = CARTESIAN_POINT ( 'NONE',  ( 207.7625791259561652, 270.7916523727319031, -1.015623356719550063 ) ) ;
#62918 = CARTESIAN_POINT ( 'NONE',  ( 85.41673846469936393, 44.62557248619319950, -7.387197001228601678 ) ) ;
#62919 = CARTESIAN_POINT ( 'NONE',  ( 185.5294769923299327, 262.0336625405320206, 9.760107401958277862 ) ) ;
#62920 = CARTESIAN_POINT ( 'NONE',  ( 165.0604371780248982, 244.7539318185670822, -1.421758703131883017 ) ) ;
#62921 = CARTESIAN_POINT ( 'NONE',  ( 127.9681836757279001, 250.8149278399160949, 9.188101187500093303 ) ) ;
#62922 = CARTESIAN_POINT ( 'NONE',  ( 198.5954523381739989, 286.6695817285962562, -18.45134152028667174 ) ) ;
#62923 = CARTESIAN_POINT ( 'NONE',  ( 189.1621392246859443, 299.6514946570117104, 4.921827439568769336 ) ) ;
#62924 = CARTESIAN_POINT ( 'NONE',  ( 196.4677418905696129, 290.3548843276421394, 17.08610552292358520 ) ) ;
#62925 = CARTESIAN_POINT ( 'NONE',  ( 42.76202708541288899, 64.24573752441608576, -10.00000000000000000 ) ) ;
#62926 = CARTESIAN_POINT ( 'NONE',  ( 56.25097556847656932, 191.0327760586659451, 1.948934522072303157E-15 ) ) ;
#62927 = CARTESIAN_POINT ( 'NONE',  ( 85.53665298850141596, 48.34007191699684114, -12.21196891364053450 ) ) ;
#62928 = VERTEX_POINT ( 'NONE', #44759 ) ;
#62929 = CARTESIAN_POINT ( 'NONE',  ( 72.14622295904345606, 66.92643202321383455, 11.38291742270067530 ) ) ;
#62930 = FACE_OUTER_BOUND ( 'NONE', #23363, .T. ) ;
#62931 =( NAMED_UNIT ( * ) PLANE_ANGLE_UNIT ( ) SI_UNIT ( $, .RADIAN. ) );
#62932 = CARTESIAN_POINT ( 'NONE',  ( 175.0809028706871118, 261.2525943152746208, 15.25527675994286092 ) ) ;
#62933 = CARTESIAN_POINT ( 'NONE',  ( 151.2652836043610876, 278.4243225337131662, -1.677173973228833548 ) ) ;
#62934 = CARTESIAN_POINT ( 'NONE',  ( -5.362061845104276081, 24.53938646500537146, -10.00000000000000000 ) ) ;
#62935 = CARTESIAN_POINT ( 'NONE',  ( 178.6782777294722848, 260.6412425082613709, 13.57969907341511551 ) ) ;
#62936 = CARTESIAN_POINT ( 'NONE',  ( 122.4023397829302553, 228.1427522451417360, 1.119607411625061291E-15 ) ) ;
#62937 = VECTOR ( 'NONE', #77763, 1000.000000000000000 ) ;
#62938 = CARTESIAN_POINT ( 'NONE',  ( -89.11465314115665137, 93.37593066204027537, -37.49999999999999289 ) ) ;
#62939 = ORIENTED_EDGE ( 'NONE', *, *, #71320, .T. ) ;
#62940 = ADVANCED_FACE ( 'NONE', ( #82341 ), #97995, .F. ) ;
#62941 = CARTESIAN_POINT ( 'NONE',  ( 147.8503508990560533, 274.5626756563852950, 7.845851077393495743 ) ) ;
#62942 = CARTESIAN_POINT ( 'NONE',  ( 20.42956747364522485, 12.76426979415089313, 3.090169943749476733 ) ) ;
#62943 = VECTOR ( 'NONE', #26680, 1000.000000000000000 ) ;
#62944 = CARTESIAN_POINT ( 'NONE',  ( 33.57176175898906934, 184.0643266524159856, -9.188101187500093303 ) ) ;
#62945 = CIRCLE ( 'NONE', #79198, 17.82106496071138935 ) ;
#62946 = CARTESIAN_POINT ( 'NONE',  ( 17.03907575219864867, 18.03677371833801502, 10.00000000000000533 ) ) ;
#62947 = CARTESIAN_POINT ( 'NONE',  ( 84.03077106726578904, 48.73883679912442801, -13.14056060433543038 ) ) ;
#62948 = DIRECTION ( 'NONE',  ( -0.000000000000000000, -0.000000000000000000, -1.000000000000000000 ) ) ;
#62949 = CARTESIAN_POINT ( 'NONE',  ( 66.84345300777175680, 68.16924383811607413, -6.541651360653301772 ) ) ;
#62951 = CARTESIAN_POINT ( 'NONE',  ( 69.21394623383595501, 200.7677522451417929, -5.000000000000041744 ) ) ;
#62950 = CARTESIAN_POINT ( 'NONE',  ( 198.1618177255134015, 277.6368070017157947, -15.56499484391458843 ) ) ;
#62952 = DIRECTION ( 'NONE',  ( -0.5000000000000003331, 0.8660254037844383745, 0.000000000000000000 ) ) ;
#62953 = CARTESIAN_POINT ( 'NONE',  ( 163.1794579292409253, 256.1406810980501518, -15.00038027609048363 ) ) ;
#62954 = CARTESIAN_POINT ( 'NONE',  ( 205.4029933437358295, 274.8785748323546159, -13.50815392427034922 ) ) ;
#62955 = CARTESIAN_POINT ( 'NONE',  ( 162.0223120223976423, 251.6753896847266958, -12.96689075600689911 ) ) ;
#62956 = ORIENTED_EDGE ( 'NONE', *, *, #2424, .F. ) ;
#62957 = B_SPLINE_CURVE_WITH_KNOTS ( 'NONE', 3,
 ( #87830, #16850, #78674, #33566, #12134, #63952, #4520, #25454, #47738, #41136, #93396, #72075, #42996, #73934, #86819, #79205, #35421, #23947, #9265, #16357, #39629, #1677, #70550, #40136, #1166, #32560, #63458, #24947, #55825, #9779, #51108, #28825, #67823, #14122, #75432, #98745, #91648, #67311, #45003, #5032, #58701, #97743, #13140, #53112, #12643, #43997, #27825, #37401, #6016, #74939, #59708, #66326 ),
 .UNSPECIFIED., .F., .F.,
 ( 4, 2, 2, 2, 2, 2, 2, 2, 2, 2, 2, 2, 2, 2, 2, 2, 2, 2, 2, 2, 2, 2, 2, 2, 2, 4 ),
 ( 9.655427817053376463E-05, 0.001108321745685109366, 0.001361263612563711704, 0.001614205479442313608, 0.001740676412881614777, 0.001867147346320915946, 0.001993618279760217115, 0.002120089213199518284, 0.002373031080078007431, 0.002625972946956497012, 0.003131856680713594569, 0.004143624148227681263, 0.005155391615741768824, 0.005661275349498765333, 0.005914217216377265322, 0.006040688149816550445, 0.006167159083255834701, 0.006230394549975405705, 0.006293630016694975841, 0.006420100950134061471, 0.006673042817012199771, 0.006925984683890338937, 0.007178926550768477237, 0.007431868417646616404, 0.007684810284524755571, 0.008190694018281138855 ),
 .UNSPECIFIED. ) ;
#62958 = AXIS2_PLACEMENT_3D ( 'NONE', #66488, #28480, #11327 ) ;
#62959 = CARTESIAN_POINT ( 'NONE',  ( 22.61095419623372038, 183.8615022471902591, -10.00000000000009592 ) ) ;
#62960 = CARTESIAN_POINT ( 'NONE',  ( 143.5566409438477820, 259.8149278399160949, 9.188101187500093303 ) ) ;
#62961 = DIRECTION ( 'NONE',  ( 0.000000000000000000, -1.000000000000000000, 0.000000000000000000 ) ) ;
#62962 = CARTESIAN_POINT ( 'NONE',  ( -9.188242552867592394, 159.3768266524160140, 9.188101187500098632 ) ) ;
#62963 = CARTESIAN_POINT ( 'NONE',  ( 32.94607225727562394, 21.94754757982091675, 5.678558825948272215 ) ) ;
#62965 = CARTESIAN_POINT ( 'NONE',  ( 169.3931091469603984, 263.1051856239939184, 15.88219003239466431 ) ) ;
#62964 = CARTESIAN_POINT ( 'NONE',  ( 164.1063306464232596, 260.5560046979782669, -16.15882112840923668 ) ) ;
#62966 = CARTESIAN_POINT ( 'NONE',  ( 188.9967343574858489, 261.2041156289865285, 6.779708859182053793 ) ) ;
#62967 = CARTESIAN_POINT ( 'NONE',  ( 164.2572333502590709, 246.1451216570909253, 2.155809084027023204 ) ) ;
#62968 = EDGE_CURVE ( 'NONE', #35128, #46853, #74712, .T. ) ;
#62969 = CARTESIAN_POINT ( 'NONE',  ( 183.8752768387326171, 258.1900781452185356, -2.303537087110122616 ) ) ;
#62970 = CARTESIAN_POINT ( 'NONE',  ( 65.88354372152944904, 68.95778724155981365, 2.436355252633338520 ) ) ;
#62971 = EDGE_LOOP ( 'NONE', ( #5799, #10608, #34163, #13091 ) ) ;
#62972 = B_SPLINE_CURVE_WITH_KNOTS ( 'NONE', 3,
 ( #894, #62677, #31774, #78923 ),
 .UNSPECIFIED., .F., .F.,
 ( 4, 4 ),
 ( 0.002549164959714402164, 0.01048964830214099697 ),
 .UNSPECIFIED. ) ;
#62973 = CARTESIAN_POINT ( 'NONE',  ( -19.42194755839791753, 24.31068691715150010, -10.00000000000000000 ) ) ;
#62974 = CARTESIAN_POINT ( 'NONE',  ( 178.4184685675666628, 285.5228835851044096, 12.97023324045351345 ) ) ;
#62975 = CARTESIAN_POINT ( 'NONE',  ( 168.8231301974613530, 288.1409873211621857, 0.5233980140626269817 ) ) ;
#62976 = CARTESIAN_POINT ( 'NONE',  ( 8.474262601947446072, 26.93396525600388713, 2.839279412974139660 ) ) ;
#62977 = VECTOR ( 'NONE', #8886, 1000.000000000000114 ) ;
#62978 = CARTESIAN_POINT ( 'NONE',  ( 159.0854911330092420, 259.4224917152533294, 16.69341444665720076 ) ) ;
#62979 = CARTESIAN_POINT ( 'NONE',  ( 159.5050723400634638, 254.3761059724978679, -15.34938048045353298 ) ) ;
#62980 = CARTESIAN_POINT ( 'NONE',  ( 55.08690683815012790, 212.6115022471903444, -5.000000000000047962 ) ) ;
#62981 = EDGE_CURVE ( 'NONE', #28238, #29044, #52371, .T. ) ;
#62982 = CARTESIAN_POINT ( 'NONE',  ( 192.1396999271463812, 297.8512729055811974, 12.32430960859512403 ) ) ;
#62983 = DIRECTION ( 'NONE',  ( -0.8660254037844387076, -0.4999999999999998890, -0.000000000000000000 ) ) ;
#62984 = CARTESIAN_POINT ( 'NONE',  ( 191.2827847134780654, 298.6246597018299553, 8.274781095337747416 ) ) ;
#62985 = EDGE_CURVE ( 'NONE', #67772, #63278, #5776, .T. ) ;
#62986 = CARTESIAN_POINT ( 'NONE',  ( 208.3764315856425640, 269.7284287242038658, -1.833640725398759441 ) ) ;
#62987 = CARTESIAN_POINT ( 'NONE',  ( 194.1011995340913074, 294.4538559273262877, 13.93949783759920713 ) ) ;
#62988 = ORIENTED_EDGE ( 'NONE', *, *, #74365, .T. ) ;
#62989 = EDGE_CURVE ( 'NONE', #59756, #14425, #89597, .T. ) ;
#62990 = ORIENTED_EDGE ( 'NONE', *, *, #52257, .F. ) ;
#62991 = CARTESIAN_POINT ( 'NONE',  ( 131.6579862894242581, 253.4865022471902876, -10.00000000000009592 ) ) ;
#62992 = CARTESIAN_POINT ( 'NONE',  ( 73.06582205585958434, 70.62793229939931905, 7.756361730470036520 ) ) ;
#62993 = VERTEX_POINT ( 'NONE', #78690 ) ;
#62994 = CARTESIAN_POINT ( 'NONE',  ( -5.362061845104276081, 24.53938646500537146, 10.00000000000000000 ) ) ;
#62995 = DIRECTION ( 'NONE',  ( -1.000000000000000000, 0.000000000000000000, 0.000000000000000000 ) ) ;
#62997 = VERTEX_POINT ( 'NONE', #94908 ) ;
#62996 = B_SPLINE_CURVE_WITH_KNOTS ( 'NONE', 3,
 ( #404, #9001, #93133, #8018 ),
 .UNSPECIFIED., .F., .F.,
 ( 4, 4 ),
 ( 0.003861517607683099228, 0.009339119252991781930 ),
 .UNSPECIFIED. ) ;
#62998 = CARTESIAN_POINT ( 'NONE',  ( 162.7752149807717785, 250.7913148208739074, -13.06579887205573165 ) ) ;
#62999 = CARTESIAN_POINT ( 'NONE',  ( 79.33413028100275710, 59.08315638148421556, -16.22733909814880704 ) ) ;
#63000 = FACE_OUTER_BOUND ( 'NONE', #60137, .T. ) ;
#63001 = FACE_OUTER_BOUND ( 'NONE', #63269, .T. ) ;
#63002 = ORIENTED_EDGE ( 'NONE', *, *, #76521, .T. ) ;
#63003 = CARTESIAN_POINT ( 'NONE',  ( 200.3134965941964651, 283.6938417875134064, 18.29802468362849766 ) ) ;
#63004 = CARTESIAN_POINT ( 'NONE',  ( 151.0715479399129606, 268.9833987204304435, 14.24612252017116987 ) ) ;
#63005 = CARTESIAN_POINT ( 'NONE',  ( 151.2990042328006552, 274.9136309945131416, -8.631800923121661029 ) ) ;
#63006 = B_SPLINE_CURVE_WITH_KNOTS ( 'NONE', 3,
 ( #32701, #49405, #80352, #41794, #56500, #3333, #71224, #32199, #1817, #63601, #94541, #72228, #34211, #9922, #79357, #11436, #40782, #71730, #95054, #10416, #87974, #2835, #79851, #33724 ),
 .UNSPECIFIED., .F., .F.,
 ( 4, 2, 2, 2, 2, 2, 2, 2, 2, 2, 2, 4 ),
 ( 0.000000000000000000, 0.1249999999999974742, 0.2499999999999949485, 0.3749999999999924505, 0.4374999999999911737, 0.4999999999999898970, 0.5624999999999886757, 0.6249999999999873435, 0.6874999999999861222, 0.7499999999999849010, 0.8749999999999924505, 1.000000000000000000 ),
 .UNSPECIFIED. ) ;
#63007 = VERTEX_POINT ( 'NONE', #8773 ) ;
#63008 = ORIENTED_EDGE ( 'NONE', *, *, #54624, .T. ) ;
#63009 = ORIENTED_EDGE ( 'NONE', *, *, #90829, .T. ) ;
#63010 = CARTESIAN_POINT ( 'NONE',  ( 73.14366643852760319, 60.29835623558181368, 15.26756996240958131 ) ) ;
#63011 = ORIENTED_EDGE ( 'NONE', *, *, #33774, .F. ) ;
#63012 = DIRECTION ( 'NONE',  ( 0.5000000000000002220, -0.8660254037844387076, -0.000000000000000000 ) ) ;
#63013 = VERTEX_POINT ( 'NONE', #1691 ) ;
#63014 = CARTESIAN_POINT ( 'NONE',  ( 208.2764314485352770, 269.9016340424377063, 2.433736665191914117 ) ) ;
#63015 = EDGE_CURVE ( 'NONE', #74347, #14902, #93917, .T. ) ;
#63016 = DIRECTION ( 'NONE',  ( -0.8660254037844378194, -0.5000000000000013323, -0.000000000000000000 ) ) ;
#63017 = LINE ( 'NONE', #85367, #75422 ) ;
#63018 = CARTESIAN_POINT ( 'NONE',  ( 147.6054094044680198, 274.9869267698931594, -8.596541856229405809 ) ) ;
#63020 = CARTESIAN_POINT ( 'NONE',  ( 82.79952076536555694, 53.35385224299954388, -15.29414667009053197 ) ) ;
#63019 = VECTOR ( 'NONE', #49890, 1000.000000000000000 ) ;
#63021 = DIRECTION ( 'NONE',  ( -0.000000000000000000, -0.000000000000000000, -1.000000000000000000 ) ) ;
#63022 = CARTESIAN_POINT ( 'NONE',  ( 51.80235952159637236, 80.00000000000000000, 59.99999999999999289 ) ) ;
#63023 = CARTESIAN_POINT ( 'NONE',  ( 15.62557774837418023, 29.99752408145591076, 5.678558825948277544 ) ) ;
#63024 = CARTESIAN_POINT ( 'NONE',  ( 198.7255116566313404, 276.6639372973349964, -15.44186690118796790 ) ) ;
#63025 = CARTESIAN_POINT ( 'NONE',  ( 205.7829192689729325, 274.2205238267313234, 11.21202327925415254 ) ) ;
#63026 = AXIS2_PLACEMENT_3D ( 'NONE', #28170, #83402, #90524 ) ;
#63028 = VERTEX_POINT ( 'NONE', #32576 ) ;
#63027 = CARTESIAN_POINT ( 'NONE',  ( 198.1300353965528984, 287.4757075181870505, 18.48278456664528946 ) ) ;
#63029 = PLANE ( 'NONE',  #65997 ) ;
#63030 = CARTESIAN_POINT ( 'NONE',  ( 168.2217537332210782, 256.9393902984222109, -14.62648326016065425 ) ) ;
#63031 = CARTESIAN_POINT ( 'NONE',  ( 206.2313482792274328, 273.4438219973828268, -9.403385562213845361 ) ) ;
#63032 = CARTESIAN_POINT ( 'NONE',  ( 137.7719789713245291, 261.8967562850346553, -4.648177544792955347E-16 ) ) ;
#63033 = B_SPLINE_CURVE_WITH_KNOTS ( 'NONE', 3,
 ( #27265, #97194, #26266, #11079, #58148, #97679, #11577, #95718, #58633, #81498 ),
 .UNSPECIFIED., .F., .F.,
 ( 4, 2, 2, 2, 4 ),
 ( 0.001426788465073381296, 0.001827427548930433184, 0.002228066632787485506, 0.002628705716644537393, 0.003029344800501589281 ),
 .UNSPECIFIED. ) ;
#63034 = CARTESIAN_POINT ( 'NONE',  ( 161.8289209813647176, 250.3510820566641257, 13.28523796267037937 ) ) ;
#63035 = CARTESIAN_POINT ( 'NONE',  ( 191.3965809556215731, 262.3234640945070737, -0.7488543785338046543 ) ) ;
#63036 = VECTOR ( 'NONE', #53987, 1000.000000000000227 ) ;
#63037 = ORIENTED_EDGE ( 'NONE', *, *, #98689, .T. ) ;
#63038 = DIRECTION ( 'NONE',  ( 0.4999999999999998890, -0.8660254037844385966, 0.000000000000000000 ) ) ;
#63039 = CARTESIAN_POINT ( 'NONE',  ( 153.4232513496498598, 270.1086993216917449, 15.21047082690287588 ) ) ;
#63040 = CARTESIAN_POINT ( 'NONE',  ( -58.10760318826260118, 36.06970723555269842, 10.00000000000000000 ) ) ;
#63041 = CARTESIAN_POINT ( 'NONE',  ( 15.95338390109293059, 180.0177522451418497, -10.00000000000009592 ) ) ;
#63042 = CARTESIAN_POINT ( 'NONE',  ( 89.53865347855843027, 216.3768266524160140, 9.188101187500096856 ) ) ;
#63043 = CARTESIAN_POINT ( 'NONE',  ( 82.10452652000643070, 40.74900335645702398, -0.8276724821365912810 ) ) ;
#63044 = B_SPLINE_CURVE_WITH_KNOTS ( 'NONE', 3,
 ( #39332, #35979, #13695, #93079, #100180, #12714, #70247, #77874, #46435, #15535 ),
 .UNSPECIFIED., .F., .F.,
 ( 4, 2, 2, 2, 4 ),
 ( 0.000000000000000000, 0.2500000000000000000, 0.5000000000000000000, 0.7500000000000000000, 1.000000000000000000 ),
 .UNSPECIFIED. ) ;
#63045 = CARTESIAN_POINT ( 'NONE',  ( 45.05588048050944394, 66.36777381976860113, -10.00000000000000000 ) ) ;
#63046 = CARTESIAN_POINT ( 'NONE',  ( 167.7942470979873235, 278.7647128809718993, -13.37312110774118068 ) ) ;
#63047 = EDGE_CURVE ( 'NONE', #81989, #38189, #49804, .T. ) ;
#63049 = CARTESIAN_POINT ( 'NONE',  ( 75.69998711193903773, 65.59611928177264417, 13.80412242752735708 ) ) ;
#63048 = CARTESIAN_POINT ( 'NONE',  ( -1.935626891937928917, 175.8149278399160664, 9.188101187500093303 ) ) ;
#63050 = PRESENTATION_LAYER_ASSIGNMENT (  '', '', ( #56542 ) ) ;
#63051 = CARTESIAN_POINT ( 'NONE',  ( 188.9177621428281952, 297.3148466342770462, 9.216719020081887592 ) ) ;
#63052 = VERTEX_POINT ( 'NONE', #33071 ) ;
#63053 = ORIENTED_EDGE ( 'NONE', *, *, #60741, .T. ) ;
#63054 = LINE ( 'NONE', #63550, #79281 ) ;
#63055 = CARTESIAN_POINT ( 'NONE',  ( 188.9943711983743242, 261.4777017766879794, -6.044221521033104061 ) ) ;
#63056 = CIRCLE ( 'NONE', #32320, 70.00000000000001421 ) ;
#63057 = DIRECTION ( 'NONE',  ( -0.8660254037844377084, -0.5000000000000014433, -0.000000000000000000 ) ) ;
#63058 = CARTESIAN_POINT ( 'NONE',  ( 84.81383324307122962, 44.91740293199559630, 8.403696530403449216 ) ) ;
#63059 = CARTESIAN_POINT ( 'NONE',  ( 207.1770866921659717, 271.8057550155037347, -5.569195235244989384 ) ) ;
#63060 = CARTESIAN_POINT ( 'NONE',  ( 185.2008289883677321, 286.4076746189350615, 16.12297053898278421 ) ) ;
#63061 = CARTESIAN_POINT ( 'NONE',  ( 74.46849378157413923, 68.15278936780924823, -11.56277540856588537 ) ) ;
#63062 = CARTESIAN_POINT ( 'NONE',  ( 34.68144358152915174, 181.6423013555409796, -4.594050593750043987 ) ) ;
#63063 = CARTESIAN_POINT ( 'NONE',  ( 78.37938175722123901, 209.3927522451418213, -10.00000000000009059 ) ) ;
#63064 = PLANE ( 'NONE',  #46330 ) ;
#63065 = VERTEX_POINT ( 'NONE', #63472 ) ;
#63066 = DIRECTION ( 'NONE',  ( -0.4386133837897802090, -0.6599160945941812129, 0.6100238090894836152 ) ) ;
#63067 = CARTESIAN_POINT ( 'NONE',  ( 182.0886690003881370, 260.7994180317198811, -10.55243971876994635 ) ) ;
#63068 = CARTESIAN_POINT ( 'NONE',  ( 195.7578697689113199, 291.5844189092309193, 17.18796537138345215 ) ) ;
#63069 = CARTESIAN_POINT ( 'NONE',  ( 68.62314303196725973, 64.18211696513540687, -12.51050211285727087 ) ) ;
#63070 = CARTESIAN_POINT ( 'NONE',  ( 207.2683629543511756, 271.6476598918739001, -6.694388351944108528 ) ) ;
#63071 = CARTESIAN_POINT ( 'NONE',  ( 186.6830932896762931, 282.6891639578413447, 16.18349308428762257 ) ) ;
#63072 = CARTESIAN_POINT ( 'NONE',  ( 68.90560621877192204, 63.79076715805910425, -12.30144644517788421 ) ) ;
#63073 = CARTESIAN_POINT ( 'NONE',  ( 189.7132495166375747, 263.2796367915959195, 7.902202450138100964 ) ) ;
#63074 = CARTESIAN_POINT ( 'NONE',  ( 163.8990931530087494, 246.7654386749614162, 5.873176884778091633 ) ) ;
#63075 = DIRECTION ( 'NONE',  ( -0.5000000000000014433, 0.8660254037844378194, 0.000000000000000000 ) ) ;
#63076 = CARTESIAN_POINT ( 'NONE',  ( 146.7373254022577100, 276.4904923669593586, -0.7242168585908188572 ) ) ;
#63077 = CARTESIAN_POINT ( 'NONE',  ( 189.9052851100924215, 301.7213928939034986, -1.077181946533001256 ) ) ;
#63078 = ORIENTED_EDGE ( 'NONE', *, *, #48859, .F. ) ;
#63079 = CARTESIAN_POINT ( 'NONE',  ( 207.0624025450594843, 270.0043937851150417, -2.644299678167422840 ) ) ;
#63080 = CARTESIAN_POINT ( 'NONE',  ( 207.5792673731680793, 271.1091576421853233, 2.359198794924813214 ) ) ;
#63081 = CARTESIAN_POINT ( 'NONE',  ( 181.2378726859789140, 268.0551774814318833, 15.16452475098612140 ) ) ;
#63082 = CARTESIAN_POINT ( 'NONE',  ( 107.5083335113205578, 239.0024278399160949, 9.188101187500095079 ) ) ;
#63083 = CARTESIAN_POINT ( 'NONE',  ( 11.39049277451480080, 29.68290643055186706, 3.479690158560446702E-15 ) ) ;
#63084 = CARTESIAN_POINT ( 'NONE',  ( -19.65312891409030271, 93.06504152958497400, 177.5919119679930134 ) ) ;
#63086 = CARTESIAN_POINT ( 'NONE',  ( 71.47384123275857348, 72.35069954344788812, 1.100233114707620530 ) ) ;
#63085 = CARTESIAN_POINT ( 'NONE',  ( 157.7529601300917363, 257.4108533407307959, 16.91445305439664892 ) ) ;
#63087 = CARTESIAN_POINT ( 'NONE',  ( 152.8894687064977234, 278.3516875449029158, -6.243347624783317507 ) ) ;
#63088 = CARTESIAN_POINT ( 'NONE',  ( 29.44299306155908624, 19.12755873383627403, -6.180339887498949025 ) ) ;
#63089 = CARTESIAN_POINT ( 'NONE',  ( 196.9098758191317700, 289.5890858996224324, -16.54412079817003800 ) ) ;
#63090 = CARTESIAN_POINT ( 'NONE',  ( 161.3261849411383650, 273.2032229615781489, 15.91718547624222957 ) ) ;
#63091 = CARTESIAN_POINT ( 'NONE',  ( 146.9129474150286683, 276.1863061179126930, -5.016087650759920358 ) ) ;
#63092 = DIRECTION ( 'NONE',  ( -0.000000000000000000, 0.000000000000000000, -1.000000000000000000 ) ) ;
#63093 = ORIENTED_EDGE ( 'NONE', *, *, #80875, .T. ) ;
#63094 = CARTESIAN_POINT ( 'NONE',  ( 189.5250749145859857, 265.8481487713520437, 10.75668547210380410 ) ) ;
#63095 = LINE ( 'NONE', #54472, #42583 ) ;
#63096 = CARTESIAN_POINT ( 'NONE',  ( 157.7498836780145268, 278.8187344995880039, 10.12965930615278509 ) ) ;
#63097 = EDGE_LOOP ( 'NONE', ( #34722, #89012, #52712, #66525, #24401 ) ) ;
#63098 = ADVANCED_FACE ( 'NONE', ( #63965 ), #59469, .F. ) ;
#63099 = CARTESIAN_POINT ( 'NONE',  ( 82.21410988452117863, 40.73976263626466476, 3.762362152834606732 ) ) ;
#63100 = CARTESIAN_POINT ( 'NONE',  ( 182.3161647400480092, 256.3089014165817616, 4.988711622375854304 ) ) ;
#63101 = EDGE_CURVE ( 'NONE', #28370, #62030, #42645, .T. ) ;
#63102 = CARTESIAN_POINT ( 'NONE',  ( 79.14312167556931854, 57.64441083166269664, 0.000000000000000000 ) ) ;
#63103 = VECTOR ( 'NONE', #44851, 1000.000000000000000 ) ;
#63104 = CARTESIAN_POINT ( 'NONE',  ( 148.1575212202267551, 275.3167594263540536, 5.922338269673835143 ) ) ;
#63105 = ORIENTED_EDGE ( 'NONE', *, *, #80451, .T. ) ;
#63106 = CARTESIAN_POINT ( 'NONE',  ( 190.4441833906855379, 280.6464714971045282, 16.63408401792300495 ) ) ;
#63107 = B_SPLINE_SURFACE_WITH_KNOTS ( 'NONE', 3, 1, ( 
 ( #70576, #63484 ),
 ( #62982, #78198 ),
 ( #31567, #8784 ),
 ( #54357, #1192 ),
 ( #41167, #93927 ),
 ( #47764, #32070 ),
 ( #23466, #78702 ),
 ( #94924, #25485 ),
 ( #40164, #15874 ),
 ( #46786, #56376 ),
 ( #24977, #79733 ),
 ( #55853, #86848 ),
 ( #17381, #10294 ),
 ( #72104, #31072 ),
 ( #77706, #8291 ),
 ( #39156, #81229 ),
 ( #81720, #74096 ),
 ( #4689, #35581 ),
 ( #50769, #57877 ),
 ( #3702, #26991 ),
 ( #43155, #51264 ),
 ( #66476, #26496 ),
 ( #33595, #97402 ),
 ( #27499, #64490 ),
 ( #58849, #34102 ),
 ( #41672, #12296 ),
 ( #20394, #73594 ),
 ( #95451, #19898 ),
 ( #96427, #26003 ),
 ( #88348, #10799 ),
 ( #50276, #82230 ),
 ( #11804, #57375 ),
 ( #27970, #3219 ),
 ( #88855, #73109 ) ),
 .UNSPECIFIED., .T., .F., .F.,
 ( 4, 2, 2, 2, 2, 2, 2, 2, 2, 2, 2, 2, 2, 2, 2, 2, 4 ),
 ( 2, 2 ),
 ( 0.000000000000000000, 0.06250000000000000000, 0.1250000000000000000, 0.1875000000000000000, 0.2500000000000000000, 0.3125000000000000000, 0.3750000000000000000, 0.4375000000000000000, 0.5000000000000000000, 0.5625000000000000000, 0.6250000000000000000, 0.6875000000000000000, 0.7500000000000000000, 0.8125000000000000000, 0.8750000000000000000, 0.9375000000000000000, 1.000000000000000000 ),
 ( 0.000000000000000000, 1.000000000000000000 ),
 .UNSPECIFIED. ) ;
#63108 = EDGE_CURVE ( 'NONE', #35157, #64789, #30059, .T. ) ;
#63109 = CARTESIAN_POINT ( 'NONE',  ( 37.97985170016632850, 33.87878583063844928, -9.188101187500006262 ) ) ;
#63110 = CARTESIAN_POINT ( 'NONE',  ( 177.2690896250785215, 274.8578734701023905, -17.19570748498711765 ) ) ;
#63111 = ORIENTED_EDGE ( 'NONE', *, *, #4915, .F. ) ;
#63112 = CARTESIAN_POINT ( 'NONE',  ( 78.01910789048406514, 61.79390329888819622, 16.07883194446994324 ) ) ;
#63113 = EDGE_CURVE ( 'NONE', #44653, #74347, #50752, .T. ) ;
#63114 = DIRECTION ( 'NONE',  ( 3.755686162884236985E-16, -2.795463207713249976E-32, -1.000000000000000000 ) ) ;
#63115 = DIRECTION ( 'NONE',  ( -0.000000000000000000, 1.000000000000000000, -0.000000000000000000 ) ) ;
#63116 = EDGE_LOOP ( 'NONE', ( #54335, #12797, #25353 ) ) ;
#63117 = CARTESIAN_POINT ( 'NONE',  ( 86.53491854233801917, 47.25312861645894458, -10.16653990104887484 ) ) ;
#63118 = CARTESIAN_POINT ( 'NONE',  ( 166.6173964342836484, 252.1147280582555084, 12.30655765920312028 ) ) ;
#63119 = LINE ( 'NONE', #57383, #94680 ) ;
#63120 = LINE ( 'NONE', #24120, #62766 ) ;
#63121 = CYLINDRICAL_SURFACE ( 'NONE', #38088, 45.00000000000000000 ) ;
#63122 = FACE_OUTER_BOUND ( 'NONE', #29754, .T. ) ;
#63123 = CYLINDRICAL_SURFACE ( 'NONE', #89939, 7.499999999999992895 ) ;
#63124 = ORIENTED_EDGE ( 'NONE', *, *, #97668, .F. ) ;
#63125 = ORIENTED_EDGE ( 'NONE', *, *, #91497, .F. ) ;
#63126 = CARTESIAN_POINT ( 'NONE',  ( 175.0450529704226028, 258.5646980256989309, 12.79576524686047634 ) ) ;
#63127 = ORIENTED_EDGE ( 'NONE', *, *, #75286, .T. ) ;
#63128 = CARTESIAN_POINT ( 'NONE',  ( 77.25514995865366075, 49.69881203954133042, -14.99743653824481093 ) ) ;
#63129 = ORIENTED_EDGE ( 'NONE', *, *, #81797, .F. ) ;
#63130 = CARTESIAN_POINT ( 'NONE',  ( 74.83300825804853673, 57.97047224133282128, 15.96654120040242830 ) ) ;
#63131 = CARTESIAN_POINT ( 'NONE',  ( 79.13079929454947603, 52.80933996073559911, 15.63716892723882701 ) ) ;
#63132 = ORIENTED_EDGE ( 'NONE', *, *, #62081, .F. ) ;
#63133 = CARTESIAN_POINT ( 'NONE',  ( 205.9281787291064347, 273.9689270615001533, -10.62323193457751458 ) ) ;
#63134 = CARTESIAN_POINT ( 'NONE',  ( 147.1831281302520154, 275.7183393919203809, -6.957138126403704881 ) ) ;
#63135 = CARTESIAN_POINT ( 'NONE',  ( 196.2063030037021747, 284.5084424747770413, -17.41934349069538257 ) ) ;
#63136 = CARTESIAN_POINT ( 'NONE',  ( 77.86555730066851311, 62.20866292688850052, -15.95979438352862090 ) ) ;
#63137 = CARTESIAN_POINT ( 'NONE',  ( 167.6597423760104846, 249.1366150583754404, -5.304815820813105987 ) ) ;
#63138 = CARTESIAN_POINT ( 'NONE',  ( -53.24159167507352208, 52.03622613587658208, 59.99999999999999289 ) ) ;
#63139 = CARTESIAN_POINT ( 'NONE',  ( 154.6182242168042933, 279.6024264367558771, 2.136621738763494704 ) ) ;
#63140 = CARTESIAN_POINT ( 'NONE',  ( 135.6816562978893330, 239.9548013555409796, -4.594050593750042211 ) ) ;
#63141 = VERTEX_POINT ( 'NONE', #80725 ) ;
#63142 = CARTESIAN_POINT ( 'NONE',  ( 70.45245543053056281, 60.92432115798627024, -14.97201685956949646 ) ) ;
#63143 = CARTESIAN_POINT ( 'NONE',  ( 42.48198750171711424, 33.03085787977767041, 9.188101187500006262 ) ) ;
#63144 = EDGE_LOOP ( 'NONE', ( #11714, #11897, #96209, #38150 ) ) ;
#63146 = ORIENTED_EDGE ( 'NONE', *, *, #71672, .F. ) ;
#63145 = CARTESIAN_POINT ( 'NONE',  ( 85.72965280032694579, 48.53761792183082946, -12.28028246049512262 ) ) ;
#63147 = CARTESIAN_POINT ( 'NONE',  ( 200.1076438251647289, 273.8820182500477358, 13.66411480140315504 ) ) ;
#63148 = CARTESIAN_POINT ( 'NONE',  ( 180.9880944519944990, 255.9245501647149297, 0.6744818687597132767 ) ) ;
#63149 = LINE ( 'NONE', #16052, #7486 ) ;
#63150 = CARTESIAN_POINT ( 'NONE',  ( 190.5133192800734605, 300.2599720837126824, 2.418563999166301492 ) ) ;
#63151 = CARTESIAN_POINT ( 'NONE',  ( 72.62875423623682991, 64.07121235873044895, 13.57049568789011218 ) ) ;
#63152 = CARTESIAN_POINT ( 'NONE',  ( 81.29539683296886210, 43.25976067974499273, 9.624898955577574355 ) ) ;
#63153 = CARTESIAN_POINT ( 'NONE',  ( 78.15243512869371045, 51.09092126905193254, 15.77939321497872172 ) ) ;
#63154 = CARTESIAN_POINT ( 'NONE',  ( 36.02478613032081967, 22.92755873383628540, 6.180339887498953466 ) ) ;
#63155 = CARTESIAN_POINT ( 'NONE',  ( 178.5657226154280863, 254.2359737251016440, -5.272414496410398499 ) ) ;
#63156 = VERTEX_POINT ( 'NONE', #3205 ) ;
#63158 = CARTESIAN_POINT ( 'NONE',  ( 147.9311236323648870, 274.4227731784279172, -7.799459659034405412 ) ) ;
#63157 = B_SPLINE_CURVE_WITH_KNOTS ( 'NONE', 3,
 ( #70294, #31784, #79449, #904, #24206, #24696, #87072, #86074, #70810, #8019 ),
 .UNSPECIFIED., .F., .F.,
 ( 4, 2, 2, 2, 4 ),
 ( 0.000000000000000000, 0.2500000000000000000, 0.5000000000000000000, 0.7500000000000000000, 1.000000000000000000 ),
 .UNSPECIFIED. ) ;
#63159 = CARTESIAN_POINT ( 'NONE',  ( 65.76755514393656199, 69.09664133051965962, -0.2187238748589619697 ) ) ;
#63160 = ORIENTED_EDGE ( 'NONE', *, *, #26638, .T. ) ;
#63161 = DIRECTION ( 'NONE',  ( 0.8660254037844377084, 0.5000000000000015543, -0.000000000000000000 ) ) ;
#63162 = AXIS2_PLACEMENT_3D ( 'NONE', #23092, #30712, #7397 ) ;
#63163 = CARTESIAN_POINT ( 'NONE',  ( 159.6062986900120393, 279.1035829519316849, 10.91088360456809880 ) ) ;
#63164 = CARTESIAN_POINT ( 'NONE',  ( 152.2699040063036477, 266.9077851278831872, -16.94750107875206524 ) ) ;
#63165 = LINE ( 'NONE', #47951, #25149 ) ;
#63166 = EDGE_CURVE ( 'NONE', #59506, #52122, #44257, .T. ) ;
#63167 = CARTESIAN_POINT ( 'NONE',  ( 71.23113041218663000, 71.96307377266813887, -2.934963719734108967 ) ) ;
#63169 = CARTESIAN_POINT ( 'NONE',  ( 151.4916375207045860, 274.9412589285112745, -8.761911672441238252 ) ) ;
#63168 = CARTESIAN_POINT ( 'NONE',  ( 161.4752606922666018, 281.4891156921501079, -6.619806771727822614 ) ) ;
#63170 = CARTESIAN_POINT ( 'NONE',  ( 160.1291429304770872, 283.8063366971030064, -1.115091271670870077 ) ) ;
#63171 = VERTEX_POINT ( 'NONE', #89329 ) ;
#63172 = CARTESIAN_POINT ( 'NONE',  ( 146.8058449195592061, 276.3718130816831149, 4.181814292810413392 ) ) ;
#63173 = CARTESIAN_POINT ( 'NONE',  ( 72.04273812837080015, 59.28583566120335746, 15.84548535902080246 ) ) ;
#63174 = CARTESIAN_POINT ( 'NONE',  ( 193.0787258475831720, 275.9904400578145669, -16.13630732494317499 ) ) ;
#63175 = CARTESIAN_POINT ( 'NONE',  ( -32.64350997085663408, 85.56504152958521559, 0.000000000000000000 ) ) ;
#63176 = CARTESIAN_POINT ( 'NONE',  ( 184.6784730347474976, 297.3114112913945632, -4.489973865576921241 ) ) ;
#63177 = CARTESIAN_POINT ( 'NONE',  ( 192.0712386031329686, 297.9698513971258649, 12.12276320360788873 ) ) ;
#63178 = CARTESIAN_POINT ( 'NONE',  ( 73.77733668265750566, 68.41783923479601981, 11.46675506585084925 ) ) ;
#63179 = CIRCLE ( 'NONE', #58323, 0.1418229129680863287 ) ;
#63180 = CARTESIAN_POINT ( 'NONE',  ( -8.565960340006073537, 165.8615022471902591, -10.00000000000009592 ) ) ;
#63181 = CARTESIAN_POINT ( 'NONE',  ( 71.22043767567281236, 71.52608235244971979, -2.909787917308754857 ) ) ;
#63182 = CARTESIAN_POINT ( 'NONE',  ( -4.722712290662820500, 158.8923013555410080, 4.594050593750050204 ) ) ;
#63183 = CARTESIAN_POINT ( 'NONE',  ( 85.53293889029040997, 226.3149278399160949, -9.188101187500095079 ) ) ;
#63184 = LINE ( 'NONE', #61675, #29806 ) ;
#63185 = CARTESIAN_POINT ( 'NONE',  ( 87.87167583597285159, 44.45939398776243223, -3.944263742802939010 ) ) ;
#63186 = CARTESIAN_POINT ( 'NONE',  ( 148.0908005895309714, 275.9119617183158084, 5.017397701950214284 ) ) ;
#63187 = EDGE_CURVE ( 'NONE', #66923, #20951, #91343, .T. ) ;
#63188 = CARTESIAN_POINT ( 'NONE',  ( 78.26604366595239526, 47.45132970578329434, 14.33273657485265318 ) ) ;
#63189 = CARTESIAN_POINT ( 'NONE',  ( 77.96474761936472930, 54.41649311639740461, 16.03208068940686459 ) ) ;
#63190 = CARTESIAN_POINT ( 'NONE',  ( 84.47860975560725194, 49.82577972120142817, -13.24615549146050952 ) ) ;
#63191 = CARTESIAN_POINT ( 'NONE',  ( 77.66178915777496172, 61.94839236767001722, 15.64246823995104130 ) ) ;
#63193 = CARTESIAN_POINT ( 'NONE',  ( 75.97174564027631050, 51.49815502093342445, 16.18122344262006251 ) ) ;
#63192 = CARTESIAN_POINT ( 'NONE',  ( 67.19266499973009843, 66.86638716927541282, 8.992916727549332023 ) ) ;
#63194 = CARTESIAN_POINT ( 'NONE',  ( 161.4331051045346612, 251.0366552657761190, 12.80125893768088652 ) ) ;
#63195 = B_SPLINE_CURVE_WITH_KNOTS ( 'NONE', 3,
 ( #52928, #46826, #15408, #92954, #62501, #91468, #6830, #23014, #93469, #83880, #14442, #45324, #45807, #46303, #54400, #37231, #30129, #38716, #39200, #24022, #7324, #61521, #77228, #100049, #29639, #38204, #70112, #68625, #85376, #15921, #77749 ),
 .UNSPECIFIED., .F., .F.,
 ( 4, 3, 3, 3, 3, 3, 3, 3, 3, 3, 4 ),
 ( 0.000000000000000000, 0.1333490885032399820, 0.3007194338854488058, 0.4699862290245400698, 0.5844252810809538179, 0.6686540514502882226, 0.7354980260655652469, 0.8028463152565959993, 0.8633854507757408037, 0.9437142632667595565, 1.000000000000000000 ),
 .UNSPECIFIED. ) ;
#63196 = CARTESIAN_POINT ( 'NONE',  ( -0.9341114727035790821, 160.2677522451418213, -5.000000000000041744 ) ) ;
#63197 = FILL_AREA_STYLE_COLOUR ( '', #83838 ) ;
#63198 =( BOUNDED_CURVE ( )  B_SPLINE_CURVE ( 2, ( #44409, #33456, #41540, #64352, #13050, #59094, #95316, #18268, #52509 ),
 .UNSPECIFIED., .F., .T. ) 
 B_SPLINE_CURVE_WITH_KNOTS ( ( 3, 2, 2, 2, 3 ),
 ( 0.6411290322580645018, 0.6424731182795698770, 0.6451612903225806273, 0.6478494623655913776, 0.6491935483870967527 ),
 .UNSPECIFIED. ) 
 CURVE ( )  GEOMETRIC_REPRESENTATION_ITEM ( )  RATIONAL_B_SPLINE_CURVE ( ( 0.9330127018922194093, 0.9330127018922194093, 1.000000000000000000, 0.8660254037844387076, 1.000000000000000000, 0.8660254037844387076, 1.000000000000000000, 0.9330127018922194093, 0.9330127018922194093 ) ) 
 REPRESENTATION_ITEM ( '' )  );
#63199 = CARTESIAN_POINT ( 'NONE',  ( 195.8947060313465443, 291.3474115503753410, 16.07878593000791767 ) ) ;
#63200 = CARTESIAN_POINT ( 'NONE',  ( -5.560871861494070423, 156.0494855054051868, -2.679491924311250717 ) ) ;
#63201 = CARTESIAN_POINT ( 'NONE',  ( 161.7412967960748915, 250.5028515975580774, -14.36228887024421041 ) ) ;
#63203 =( BOUNDED_CURVE ( )  B_SPLINE_CURVE ( 2, ( #74476, #92191, #22744, #53623, #28334, #84579, #43535, #5054, #35934 ),
 .UNSPECIFIED., .F., .T. ) 
 B_SPLINE_CURVE_WITH_KNOTS ( ( 3, 2, 2, 2, 3 ),
 ( 0.4879032258064516236, 0.4892473118279569988, 0.4919354838709677491, 0.4946236559139784994, 0.4959677419354838745 ),
 .UNSPECIFIED. ) 
 CURVE ( )  GEOMETRIC_REPRESENTATION_ITEM ( )  RATIONAL_B_SPLINE_CURVE ( ( 0.9330127018922194093, 0.9330127018922194093, 1.000000000000000000, 0.8660254037844387076, 1.000000000000000000, 0.8660254037844387076, 1.000000000000000000, 0.9330127018922194093, 0.9330127018922194093 ) ) 
 REPRESENTATION_ITEM ( '' )  );
#63202 = CARTESIAN_POINT ( 'NONE',  ( 42.82723471405275717, 195.5333772461660544, 9.188101187500095079 ) ) ;
#63204 = CARTESIAN_POINT ( 'NONE',  ( 68.02342162723002161, 200.8923013555409796, 4.594050593750050204 ) ) ;
#63205 = CARTESIAN_POINT ( 'NONE',  ( 81.52103558181507026, 206.3262482093457777, 3.021315404115420679E-15 ) ) ;
#63206 = CARTESIAN_POINT ( 'NONE',  ( 88.50942844660002606, 43.88426665780151836, -0.4971503815960300887 ) ) ;
#63207 = CARTESIAN_POINT ( 'NONE',  ( 4.698709606056801213, 26.21091486745858390, -1.111400068045478839E-16 ) ) ;
#63209 = LINE ( 'NONE', #76901, #52204 ) ;
#63208 = CARTESIAN_POINT ( 'NONE',  ( 86.04433559121571307, 43.25845178644564726, -4.809067209069766591 ) ) ;
#63210 = CARTESIAN_POINT ( 'NONE',  ( 200.0411626275569574, 270.6720010161316736, -11.59284015024147152 ) ) ;
#63211 = CARTESIAN_POINT ( 'NONE',  ( 30.43941648770709207, 23.28920272979928541, -7.433330006724141015 ) ) ;
#63212 = DIRECTION ( 'NONE',  ( 0.4755282581475757664, -0.8236391035463335175, -0.3090169943749448977 ) ) ;
#63213 = CARTESIAN_POINT ( 'NONE',  ( 196.3174919959537306, 290.6151247789487684, -17.61248417473235151 ) ) ;
#63214 = CARTESIAN_POINT ( 'NONE',  ( 13.72994409607376731, 16.43085787977761569, -9.188101187500008038 ) ) ;
#63215 = CARTESIAN_POINT ( 'NONE',  ( 65.12704176573704729, 220.6589784336661637, -6.496448406907676862E-16 ) ) ;
#63216 = CARTESIAN_POINT ( 'NONE',  ( 90.95479231155565003, 229.9865022471903160, 10.00000000000009415 ) ) ;
#63217 = CARTESIAN_POINT ( 'NONE',  ( 203.0026270830780675, 279.0361311525880978, -16.61345826058821373 ) ) ;
#63218 = CARTESIAN_POINT ( 'NONE',  ( 197.9952413503812352, 287.7091776547143809, 17.17611241386010690 ) ) ;
#63219 = CARTESIAN_POINT ( 'NONE',  ( 189.4608361404499703, 260.4689339591389512, -5.099727369828423562 ) ) ;
#63220 = CARTESIAN_POINT ( 'NONE',  ( 202.1048707099531612, 280.5910908036593128, 17.24634036681479898 ) ) ;
#63221 = ADVANCED_FACE ( 'NONE', ( #67955 ), #45144, .F. ) ;
#63222 = CARTESIAN_POINT ( 'NONE',  ( 79.42436089683208422, 55.33937033912253156, -16.05718545809815367 ) ) ;
#63223 = CARTESIAN_POINT ( 'NONE',  ( 87.67135465677671391, 44.96834575157770075, -6.594061650049633627 ) ) ;
#63224 = CARTESIAN_POINT ( 'NONE',  ( 116.2138665886018458, 231.2365022471901739, -10.00000000000009059 ) ) ;
#63225 = CARTESIAN_POINT ( 'NONE',  ( -32.94356256989595977, 94.88921800892812541, 36.50000000000000000 ) ) ;
#63226 = CARTESIAN_POINT ( 'NONE',  ( 207.1601050488701503, 271.8351680844880889, 6.320235450527015075 ) ) ;
#63227 = ORIENTED_EDGE ( 'NONE', *, *, #22069, .F. ) ;
#63228 = CARTESIAN_POINT ( 'NONE',  ( 77.61293579238375173, 49.29402822633370818, 15.29643791220711257 ) ) ;
#63229 = CARTESIAN_POINT ( 'NONE',  ( 185.3033850351416163, 271.6740437919646070, 15.89117118174857701 ) ) ;
#63230 = VERTEX_POINT ( 'NONE', #59845 ) ;
#63231 = CARTESIAN_POINT ( 'NONE',  ( 206.0930919633010774, 273.6832889610345774, -9.866500005465628220 ) ) ;
#63232 = CARTESIAN_POINT ( 'NONE',  ( 147.4047294057049271, 275.3345147238139248, 0.000000000000000000 ) ) ;
#63233 = CYLINDRICAL_SURFACE ( 'NONE', #72602, 10.00000000000010658 ) ;
#63234 = ADVANCED_FACE ( 'NONE', ( #90309 ), #29453, .F. ) ;
#63235 = ORIENTED_EDGE ( 'NONE', *, *, #54384, .T. ) ;
#63236 = CARTESIAN_POINT ( 'NONE',  ( 176.8706069101428113, 252.4357694602331037, -0.2696942673409187252 ) ) ;
#63237 = VERTEX_POINT ( 'NONE', #76083 ) ;
#63238 = CARTESIAN_POINT ( 'NONE',  ( 79.48743557011087546, 46.24584566380116968, -13.22586493812016961 ) ) ;
#63239 = B_SPLINE_CURVE_WITH_KNOTS ( 'NONE', 3,
 ( #77484, #29869, #22265, #7560 ),
 .UNSPECIFIED., .F., .F.,
 ( 4, 4 ),
 ( 0.02524676605399324425, 0.03021559084467593387 ),
 .UNSPECIFIED. ) ;
#63240 = CARTESIAN_POINT ( 'NONE',  ( 167.7537490005853726, 248.2253239148561192, 3.510291536348892905 ) ) ;
#63241 = B_SPLINE_CURVE_WITH_KNOTS ( 'NONE', 3,
 ( #81641, #73027, #41082, #2623, #33512, #41591, #72533, #34024, #64912, #31737, #51183, #69753, #856, #38848, #93084, #82656 ),
 .UNSPECIFIED., .F., .F.,
 ( 4, 1, 2, 2, 2, 1, 2, 2, 4 ),
 ( 0.000000000000000000, 0.1250000000000028311, 0.1875000000000019706, 0.2500000000000011102, 0.4999999999999938938, 0.6249999999999916733, 0.6874999999999928946, 0.7499999999999941158, 1.000000000000000000 ),
 .UNSPECIFIED. ) ;
#63242 = DIRECTION ( 'NONE',  ( -0.8452030915256492083, -0.5344452582589588330, 0.000000000000000000 ) ) ;
#63243 = VERTEX_POINT ( 'NONE', #13751 ) ;
#63244 = CARTESIAN_POINT ( 'NONE',  ( 20.47532000956703158, 32.79752408145593279, -5.678558825948271327 ) ) ;
#63245 = FACE_OUTER_BOUND ( 'NONE', #58386, .T. ) ;
#63246 = CARTESIAN_POINT ( 'NONE',  ( 74.76064909570827410, 66.79516745633127073, -13.17056974000816183 ) ) ;
#63247 = CARTESIAN_POINT ( 'NONE',  ( -110.0000000000000000, 0.000000000000000000, 59.99999999999999289 ) ) ;
#63248 = ORIENTED_EDGE ( 'NONE', *, *, #4083, .T. ) ;
#63249 = CYLINDRICAL_SURFACE ( 'NONE', #6128, 10.00000000000001066 ) ;
#63250 = ORIENTED_EDGE ( 'NONE', *, *, #10980, .T. ) ;
#63251 = AXIS2_PLACEMENT_3D ( 'NONE', #68146, #82423, #67153 ) ;
#63252 = CARTESIAN_POINT ( 'NONE',  ( 174.6327531315653516, 286.2036907333609292, 10.50852000950855114 ) ) ;
#63254 = CARTESIAN_POINT ( 'NONE',  ( 68.10759289738595612, 66.09109068389082609, -10.54117928085663536 ) ) ;
#63253 = FACE_OUTER_BOUND ( 'NONE', #27643, .T. ) ;
#63255 = CARTESIAN_POINT ( 'NONE',  ( 81.50264768554443151, 55.96797772595287057, -16.03733208502487173 ) ) ;
#63256 = CARTESIAN_POINT ( 'NONE',  ( 194.2199708651012600, 294.2481379475345875, 15.50834247347371253 ) ) ;
#63257 = CARTESIAN_POINT ( 'NONE',  ( 41.58988463324670448, 24.41603393254329646, -1.583844403245396437 ) ) ;
#63258 = CARTESIAN_POINT ( 'NONE',  ( 204.7242223814549504, 276.0542406257275161, -13.93608974681376189 ) ) ;
#63259 = DIRECTION ( 'NONE',  ( 8.673617379884076887E-16, 0.000000000000000000, -1.000000000000000000 ) ) ;
#63260 = LINE ( 'NONE', #9582, #72824 ) ;
#63261 = CARTESIAN_POINT ( 'NONE',  ( 79.06677544641175359, 59.81915678714237572, 16.49560342610751107 ) ) ;
#63262 = CARTESIAN_POINT ( 'NONE',  ( 95.60083130504949622, 219.8768266524159856, -9.188101187500091527 ) ) ;
#63263 = ORIENTED_EDGE ( 'NONE', *, *, #93065, .F. ) ;
#63264 = CARTESIAN_POINT ( 'NONE',  ( 191.4484954869714954, 299.0484741143815199, 8.684991747358081327 ) ) ;
#63265 = CARTESIAN_POINT ( 'NONE',  ( -21.44506416300749407, 94.09961582791768819, -54.99999999999999289 ) ) ;
#63266 = CARTESIAN_POINT ( 'NONE',  ( 77.86555730066851311, 62.20866292688850052, -15.95979438352862090 ) ) ;
#63267 = ORIENTED_EDGE ( 'NONE', *, *, #58039, .F. ) ;
#63268 = CARTESIAN_POINT ( 'NONE',  ( 156.8233863690425949, 259.0209223242507619, -17.03117928572234163 ) ) ;
#63269 = EDGE_LOOP ( 'NONE', ( #84244, #56524, #49812, #71642 ) ) ;
#63270 = ORIENTED_EDGE ( 'NONE', *, *, #42849, .T. ) ;
#63271 = CARTESIAN_POINT ( 'NONE',  ( 80.02650856630110354, 44.34150727177379991, -11.51959576634213889 ) ) ;
#63272 = CARTESIAN_POINT ( 'NONE',  ( 9.894862028763428796, 29.21091486745858745, -1.111400068045478839E-16 ) ) ;
#63273 = CARTESIAN_POINT ( 'NONE',  ( 27.54669006335486614, 38.83705186507756224, 3.090169943749475401 ) ) ;
#63274 = CARTESIAN_POINT ( 'NONE',  ( 80.14541552094489418, 48.42908552485922513, -13.75865811180872633 ) ) ;
#63275 = CARTESIAN_POINT ( 'NONE',  ( 207.5987293781265919, 271.0754484607800237, 1.965225377555418484 ) ) ;
#63276 = CARTESIAN_POINT ( 'NONE',  ( 82.58295308470839302, 227.6744531367911293, 4.594050593750047540 ) ) ;
#63277 = ORIENTED_EDGE ( 'NONE', *, *, #8287, .F. ) ;
#63278 = VERTEX_POINT ( 'NONE', #99369 ) ;
#63279 = CARTESIAN_POINT ( 'NONE',  ( -19.75605576492141324, 93.16261100237599635, 59.99999999999999289 ) ) ;
#63280 = CARTESIAN_POINT ( 'NONE',  ( 161.3190080243304294, 251.2342772056852596, -13.92386533781515823 ) ) ;
#63281 = ORIENTED_EDGE ( 'NONE', *, *, #76180, .F. ) ;
#63282 = CARTESIAN_POINT ( 'NONE',  ( 76.19947903059282623, 64.78545985970092147, -14.35372622111362340 ) ) ;
#63283 = EDGE_CURVE ( 'NONE', #33600, #48389, #99906, .T. ) ;
#63284 = CARTESIAN_POINT ( 'NONE',  ( 161.8153693897043581, 283.8862103938810719, 0.5193901413821779833 ) ) ;
#63285 = CARTESIAN_POINT ( 'NONE',  ( 188.6301707762981152, 265.0060877223691591, -12.46499516475016733 ) ) ;
#63286 = CARTESIAN_POINT ( 'NONE',  ( 87.97302621401057365, 44.79893962918851713, 4.797252263720211296 ) ) ;
#63287 = VERTEX_POINT ( 'NONE', #90807 ) ;
#63288 = CARTESIAN_POINT ( 'NONE',  ( 85.64888316943795132, 43.83034633356992060, -5.532248923516708494 ) ) ;
#63289 = CARTESIAN_POINT ( 'NONE',  ( 78.41477381122238910, 47.32040575024741713, -14.22103711499937262 ) ) ;
#63290 = CARTESIAN_POINT ( 'NONE',  ( 206.7893622945242385, 272.4773133715531230, -10.52881283832460291 ) ) ;
#63291 = EDGE_CURVE ( 'NONE', #37083, #9585, #51769, .T. ) ;
#63292 = DIRECTION ( 'NONE',  ( -0.9607486656258009683, -0.2774202615135436534, 0.000000000000000000 ) ) ;
#63293 = CARTESIAN_POINT ( 'NONE',  ( 174.8907460544039907, 283.7088854317884739, 13.39808451214262597 ) ) ;
#63294 = CARTESIAN_POINT ( 'NONE',  ( 72.51358964696871112, 70.84733833069179809, 7.633428234268400558 ) ) ;
#63295 = CARTESIAN_POINT ( 'NONE',  ( -37.33262083840145351, 163.6868197944958467, 37.49999999999998579 ) ) ;
#63296 = EDGE_LOOP ( 'NONE', ( #9536, #34266, #32210, #66480, #13456, #31455 ) ) ;
#63297 = CARTESIAN_POINT ( 'NONE',  ( -71.61465314115659453, 63.06504152958490295, 10.00000000000000888 ) ) ;
#63298 = CARTESIAN_POINT ( 'NONE',  ( 161.7101619467568980, 250.5567787384628389, 13.05644392949610655 ) ) ;
#63299 = CARTESIAN_POINT ( 'NONE',  ( 82.41089694499171969, 41.02494636910944337, 1.928000225379814747 ) ) ;
#63300 = CARTESIAN_POINT ( 'NONE',  ( 187.8346858434329931, 266.3636700819703265, -12.51853185516833200 ) ) ;
#63301 = CARTESIAN_POINT ( 'NONE',  ( 83.50089166959301679, 52.39794543819676420, 14.81166283256270688 ) ) ;
#63302 = CYLINDRICAL_SURFACE ( 'NONE', #90009, 10.00000000000001066 ) ;
#63303 = EDGE_CURVE ( 'NONE', #21633, #66853, #82711, .T. ) ;
#63304 = CARTESIAN_POINT ( 'NONE',  ( 153.3235868295895443, 270.3046677488850378, 13.98602533532146808 ) ) ;
#63305 = ORIENTED_EDGE ( 'NONE', *, *, #92013, .T. ) ;
#63306 = CARTESIAN_POINT ( 'NONE',  ( 162.8996025780091941, 248.4966071325470125, 11.23567065566008516 ) ) ;
#63307 = CARTESIAN_POINT ( 'NONE',  ( 76.03928946417400425, 63.29995371072659793, -14.91268113313668131 ) ) ;
#63309 = FACE_BOUND ( 'NONE', #36867, .T. ) ;
#63308 = CARTESIAN_POINT ( 'NONE',  ( 180.4959160764321950, 267.2319826678609047, -15.69780135396540288 ) ) ;
#63310 = CARTESIAN_POINT ( 'NONE',  ( 79.93310189433655921, 56.55788664210029992, 16.55897019584611840 ) ) ;
#63311 = CARTESIAN_POINT ( 'NONE',  ( 30.64569906364082641, 29.64441083166262558, -10.00000000000000533 ) ) ;
#63312 = EDGE_CURVE ( 'NONE', #31364, #76961, #10999, .T. ) ;
#63313 = CARTESIAN_POINT ( 'NONE',  ( 169.5324435264030285, 273.3137144743971021, 15.97368087251608770 ) ) ;
#63314 = CYLINDRICAL_SURFACE ( 'NONE', #96669, 17.82106496071139645 ) ;
#63315 = CARTESIAN_POINT ( 'NONE',  ( 79.27712787825650764, 45.82676469203064329, -12.41914995154098911 ) ) ;
#63316 = CARTESIAN_POINT ( 'NONE',  ( 188.2302642645468325, 260.8303285139414243, 3.048995242728016031 ) ) ;
#63317 = AXIS2_PLACEMENT_3D ( 'NONE', #71985, #70464, #1078 ) ;
#63318 = CARTESIAN_POINT ( 'NONE',  ( 195.2504147615859722, 265.4741584869784674, -7.388824739121020890 ) ) ;
#63319 = CARTESIAN_POINT ( 'NONE',  ( 1.528821818964843482, 165.5643266524160140, 9.188101187500095079 ) ) ;
#63320 = CARTESIAN_POINT ( 'NONE',  ( 81.76792596524467172, 46.55419044997203315, 11.93009829901677143 ) ) ;
#63321 = EDGE_LOOP ( 'NONE', ( #6089, #637, #10315, #8103 ) ) ;
#63322 = CARTESIAN_POINT ( 'NONE',  ( 178.6359886761176767, 256.9051424919618398, 8.482123690867066301 ) ) ;
#63323 = DIRECTION ( 'NONE',  ( -0.4999999999999998890, 0.8660254037844387076, 0.000000000000000000 ) ) ;
#63324 = CARTESIAN_POINT ( 'NONE',  ( 203.1492446519190196, 274.7365285824323564, -12.75106828035650430 ) ) ;
#63325 = DIRECTION ( 'NONE',  ( 1.000000000000000000, 0.000000000000000000, 0.000000000000000000 ) ) ;
#63326 = CARTESIAN_POINT ( 'NONE',  ( 30.27021345494340565, 176.0327760586659736, 1.948934522072302763E-15 ) ) ;
#63327 = DIRECTION ( 'NONE',  ( -0.000000000000000000, -0.000000000000000000, 1.000000000000000000 ) ) ;
#63328 = CARTESIAN_POINT ( 'NONE',  ( 38.33870662942799612, 21.94473085651394939, 1.475505719884397138E-15 ) ) ;
#63329 = CARTESIAN_POINT ( 'NONE',  ( 120.4718248238752523, 250.3615022471903444, 5.000000000000046185 ) ) ;
#63330 = CARTESIAN_POINT ( 'NONE',  ( 191.8453338867844877, 298.3611298435110371, -9.039024722281077118 ) ) ;
#63331 = CARTESIAN_POINT ( 'NONE',  ( 81.68874591563863419, 55.69259006457333783, 15.98051127425669016 ) ) ;
#63332 = CARTESIAN_POINT ( 'NONE',  ( 98.24615118885414233, 215.9824982072973683, 3.021315404115420679E-15 ) ) ;
#63333 = EDGE_CURVE ( 'NONE', #3950, #76357, #78037, .T. ) ;
#63334 = EDGE_CURVE ( 'NONE', #26223, #14773, #79339, .T. ) ;
#63335 = CARTESIAN_POINT ( 'NONE',  ( 186.8249449129527875, 295.8321347383906073, -7.822565083202927205 ) ) ;
#63336 = DIRECTION ( 'NONE',  ( 0.9874311856918873698, -0.1580495287025983631, 0.000000000000000000 ) ) ;
#63337 = EDGE_CURVE ( 'NONE', #15749, #38318, #52733, .T. ) ;
#63338 = CARTESIAN_POINT ( 'NONE',  ( 193.0683888610418251, 295.7999875024635799, -12.37974131660941168 ) ) ;
#63339 = CARTESIAN_POINT ( 'NONE',  ( 59.77787777531585789, 211.9865022471903160, 10.00000000000009237 ) ) ;
#63340 = CARTESIAN_POINT ( 'NONE',  ( 68.67969803741280543, 66.83109073523215216, -9.305244569184894843 ) ) ;
#63341 = CARTESIAN_POINT ( 'NONE',  ( 185.6249487197370627, 277.7860891304547408, -17.37263783417377283 ) ) ;
#63342 = CARTESIAN_POINT ( 'NONE',  ( 204.0146600430397825, 270.3923057891465760, 6.034712041982294828 ) ) ;
#63343 = CARTESIAN_POINT ( 'NONE',  ( 28.75397480679061246, 199.6589784336661637, -6.496448406907675876E-16 ) ) ;
#63344 = CARTESIAN_POINT ( 'NONE',  ( 159.4230536986738400, 254.5181664265525683, 16.83068086755798376 ) ) ;
#63345 = CARTESIAN_POINT ( 'NONE',  ( 203.3078925370309094, 270.2142520429687806, -6.437359224241015809 ) ) ;
#63346 = CARTESIAN_POINT ( 'NONE',  ( 45.56181175559624563, 118.5014625327306135, 10.00000000000000000 ) ) ;
#63347 = CARTESIAN_POINT ( 'NONE',  ( 67.38141398091791245, 66.37704590880964872, -8.922811476558264232 ) ) ;
#63348 = EDGE_CURVE ( 'NONE', #26065, #5345, #17401, .T. ) ;
#63349 = ORIENTED_EDGE ( 'NONE', *, *, #23207, .F. ) ;
#63350 = CARTESIAN_POINT ( 'NONE',  ( 181.4954090331713417, 255.0423029034424189, 0.9094182891644410072 ) ) ;
#63351 = CARTESIAN_POINT ( 'NONE',  ( -16.97593537095525917, 172.5530062829863027, 9.296355089585912665E-16 ) ) ;
#63352 = CARTESIAN_POINT ( 'NONE',  ( 160.6748876787037261, 279.0008800672539451, -9.788185859664068289 ) ) ;
#63353 = CARTESIAN_POINT ( 'NONE',  ( -17.26243516413818924, 24.35187462261283997, -10.00000000000000000 ) ) ;
#63354 = CARTESIAN_POINT ( 'NONE',  ( 27.86299091144838869, 21.80170272979927404, 7.433330006724137462 ) ) ;
#63355 = CARTESIAN_POINT ( 'NONE',  ( 163.4260108471723640, 247.5848412648317662, 10.45113099391573108 ) ) ;
#63356 = CARTESIAN_POINT ( 'NONE',  ( 149.2923684163597784, 272.0650280510108701, -12.99082738998495756 ) ) ;
#63357 = CARTESIAN_POINT ( 'NONE',  ( 188.8822098553512774, 269.9998124647885334, -14.09010591559789560 ) ) ;
#63358 = ORIENTED_EDGE ( 'NONE', *, *, #6276, .F. ) ;
#63359 = CARTESIAN_POINT ( 'NONE',  ( 4.886862741447147052, 23.79752408145590081, -5.678558825948271327 ) ) ;
#63360 = EDGE_CURVE ( 'NONE', #95735, #22875, #35683, .T. ) ;
#63361 = CARTESIAN_POINT ( 'NONE',  ( 77.07948589789764071, 58.51398417617086523, -16.11007920833352003 ) ) ;
#63362 = CARTESIAN_POINT ( 'NONE',  ( 71.94004515418134815, 72.62285878051592647, -1.062404765500833070 ) ) ;
#63363 = EDGE_CURVE ( 'NONE', #72251, #98005, #24839, .T. ) ;
#63364 = VERTEX_POINT ( 'NONE', #92779 ) ;
#63365 = CARTESIAN_POINT ( 'NONE',  ( 27.80710661894035596, 186.8615022471902591, -10.00000000000009592 ) ) ;
#63366 = CARTESIAN_POINT ( 'NONE',  ( 178.9192782167860400, 282.6651468670382883, 15.91033708812528857 ) ) ;
#63367 = FACE_OUTER_BOUND ( 'NONE', #14419, .T. ) ;
#63368 = CARTESIAN_POINT ( 'NONE',  ( 177.9916226237585022, 256.4884131028754268, -7.270326030790868366 ) ) ;
#63369 = CARTESIAN_POINT ( 'NONE',  ( 190.1190668544949460, 301.3511120508678118, 4.410340539513557090 ) ) ;
#63370 = VERTEX_POINT ( 'NONE', #63346 ) ;
#63371 = ORIENTED_EDGE ( 'NONE', *, *, #50742, .T. ) ;
#63373 = CARTESIAN_POINT ( 'NONE',  ( 28.00427808217457937, 41.79349426999505113, 177.5919119679930134 ) ) ;
#63372 = CARTESIAN_POINT ( 'NONE',  ( 189.6356796452440960, 274.2048668380136291, -15.66483313100485297 ) ) ;
#63374 = ORIENTED_EDGE ( 'NONE', *, *, #47420, .T. ) ;
#63375 = CARTESIAN_POINT ( 'NONE',  ( 201.0732166862245549, 282.3779679885897167, -18.18766936363638820 ) ) ;
#63376 = CARTESIAN_POINT ( 'NONE',  ( 71.64316818921395225, 72.05741665177615118, -3.509880912999884917 ) ) ;
#63377 = CARTESIAN_POINT ( 'NONE',  ( 72.80497836564586578, 57.33751094343604393, -15.86650228098510773 ) ) ;
#63378 = CARTESIAN_POINT ( 'NONE',  ( -13.11024591527723615, 27.99999999999999645, -32.50000000000017053 ) ) ;
#63379 = CARTESIAN_POINT ( 'NONE',  ( 157.8043799545718286, 257.3217915922150496, -17.97575562758749257 ) ) ;
#63380 = CARTESIAN_POINT ( 'NONE',  ( 95.57333414147498729, 235.1744531367911293, 4.594050593750047540 ) ) ;
#63381 = CARTESIAN_POINT ( 'NONE',  ( 180.6932115607800711, 287.5180014335019791, -14.02160881230857825 ) ) ;
#63382 = ORIENTED_EDGE ( 'NONE', *, *, #47322, .F. ) ;
#63383 = CARTESIAN_POINT ( 'NONE',  ( 164.4405316900629259, 245.8276396196081350, -6.144538123479245328 ) ) ;
#63384 = ORIENTED_EDGE ( 'NONE', *, *, #4123, .T. ) ;
#63385 = CARTESIAN_POINT ( 'NONE',  ( 24.44940106416278169, 29.51421378149920116, -9.188101187500004485 ) ) ;
#63386 = CARTESIAN_POINT ( 'NONE',  ( 157.2050054949160085, 258.7463102223470628, 16.83784704105675090 ) ) ;
#63387 = CARTESIAN_POINT ( 'NONE',  ( 204.8570393888089711, 275.3272488847674708, -12.22745498495193139 ) ) ;
#63388 = CARTESIAN_POINT ( 'NONE',  ( 52.08270766911643079, 207.0024278399160949, -9.188101187500093303 ) ) ;
#63389 = ORIENTED_EDGE ( 'NONE', *, *, #63976, .T. ) ;
#63390 = CARTESIAN_POINT ( 'NONE',  ( 74.24116255903008721, 68.58322516222325760, 11.05893809163644725 ) ) ;
#63391 = CARTESIAN_POINT ( 'NONE',  ( 31.49087468139936874, 26.38052372038642446, 10.00000000000000533 ) ) ;
#63392 = DIRECTION ( 'NONE',  ( 0.4999999999999998890, -0.8660254037844385966, 0.000000000000000000 ) ) ;
#63393 = CARTESIAN_POINT ( 'NONE',  ( 176.2490144399759799, 273.0463910110868255, 16.82721827330342990 ) ) ;
#63394 = AXIS2_PLACEMENT_3D ( 'NONE', #3078, #94282, #18257 ) ;
#63395 = ORIENTED_EDGE ( 'NONE', *, *, #5945, .F. ) ;
#63396 = CARTESIAN_POINT ( 'NONE',  ( 87.01921871845581791, 46.46248764730437131, 8.883936319678571891 ) ) ;
#63397 = CARTESIAN_POINT ( 'NONE',  ( 84.88073312764632306, 43.04194891362699593, -4.562917901942581622 ) ) ;
#63398 = CARTESIAN_POINT ( 'NONE',  ( 190.7403173041394950, 300.2750747078583800, -4.254144485856557800 ) ) ;
#63399 = CARTESIAN_POINT ( 'NONE',  ( -19.65312891409030271, 93.06504152958497400, -10.00000000000000888 ) ) ;
#63400 = VERTEX_POINT ( 'NONE', #70443 ) ;
#63401 = CARTESIAN_POINT ( 'NONE',  ( 171.6923735590184776, 259.4456783946538394, -13.83651731890436842 ) ) ;
#63402 = CARTESIAN_POINT ( 'NONE',  ( 66.54075137518580618, 68.81555626029071959, -2.231460399992863497 ) ) ;
#63403 = CARTESIAN_POINT ( 'NONE',  ( 148.3005007218871754, 275.7829932922234093, 6.053100225771809839 ) ) ;
#63404 = CARTESIAN_POINT ( 'NONE',  ( 193.1977289678065404, 296.0187128512746995, -12.37159405312863925 ) ) ;
#63405 = CARTESIAN_POINT ( 'NONE',  ( 149.0359194785865498, 272.5092106407810206, 12.76357969772040590 ) ) ;
#63406 = CARTESIAN_POINT ( 'NONE',  ( 177.4464577649037267, 269.5727937689871965, 16.09739030304116625 ) ) ;
#63407 = ADVANCED_FACE ( 'NONE', ( #17238 ), #79088, .T. ) ;
#63408 = CARTESIAN_POINT ( 'NONE',  ( 87.60644657549313763, 43.46191668553660747, -1.868725964739645473 ) ) ;
#63409 = CARTESIAN_POINT ( 'NONE',  ( 67.52176836666478721, 67.08338768382488126, 8.956287543224618730 ) ) ;
#63410 = CARTESIAN_POINT ( 'NONE',  ( 75.35830705743131830, 64.29999869705460469, -14.30093840670493677 ) ) ;
#63411 = CARTESIAN_POINT ( 'NONE',  ( 173.2798715285074991, 281.8114527337138497, 15.08241540710736750 ) ) ;
#63412 = CARTESIAN_POINT ( 'NONE',  ( 103.3675627755349353, 239.6744531367911577, 4.594050593750047540 ) ) ;
#63413 = ORIENTED_EDGE ( 'NONE', *, *, #4513, .F. ) ;
#63414 = CARTESIAN_POINT ( 'NONE',  ( 191.7934382699952494, 298.4510156884799699, -8.680100145728863126 ) ) ;
#63415 = CARTESIAN_POINT ( 'NONE',  ( 69.84840267283668425, 64.12174718186125233, 12.47111010752439775 ) ) ;
#63416 = EDGE_CURVE ( 'NONE', #54608, #29477, #61156, .T. ) ;
#63417 = CARTESIAN_POINT ( 'NONE',  ( 155.5066938333533528, 261.3015006940112244, -18.40036130547566273 ) ) ;
#63418 = B_SPLINE_CURVE_WITH_KNOTS ( 'NONE', 3,
 ( #11690, #5562, #72999, #50170 ),
 .UNSPECIFIED., .F., .F.,
 ( 4, 4 ),
 ( 0.03543422572240963880, 0.04418364752788525585 ),
 .UNSPECIFIED. ) ;
#63419 = CARTESIAN_POINT ( 'NONE',  ( 192.3022390788198948, 296.3001551186897018, 12.15446248225496362 ) ) ;
#63420 = CARTESIAN_POINT ( 'NONE',  ( 83.86862482182540646, 51.60241004480363358, -14.38537263802609800 ) ) ;
#63421 = CARTESIAN_POINT ( 'NONE',  ( 76.15170329134147664, 51.05213637843759500, -15.57434085608729468 ) ) ;
#63422 = ORIENTED_EDGE ( 'NONE', *, *, #84540, .T. ) ;
#63423 = CARTESIAN_POINT ( 'NONE',  ( 80.42785451945398734, 57.51445601405281138, -16.58998511169260937 ) ) ;
#63424 = CARTESIAN_POINT ( 'NONE',  ( 155.0578869440801668, 273.4002611782738654, -12.96254817455158026 ) ) ;
#63425 = CARTESIAN_POINT ( 'NONE',  ( 182.1222588711129049, 260.5114411684929223, 9.510826267769539655 ) ) ;
#63426 = CARTESIAN_POINT ( 'NONE',  ( 164.8329707752360491, 245.1479151852119855, -0.9471001479485156027 ) ) ;
#63427 = CARTESIAN_POINT ( 'NONE',  ( 131.1886288721100300, 255.7369531367911293, -4.594050593750048428 ) ) ;
#63428 = EDGE_CURVE ( 'NONE', #94311, #43056, #55715, .T. ) ;
#63429 = CARTESIAN_POINT ( 'NONE',  ( 150.7850480413316632, 269.4796311011364764, -14.43114374163211089 ) ) ;
#63430 = CARTESIAN_POINT ( 'NONE',  ( 58.97569090598252473, 178.8759306620404175, 18.47570218321542868 ) ) ;
#63431 = CARTESIAN_POINT ( 'NONE',  ( 189.1715903421739711, 282.2647416125370796, -16.61583580824111905 ) ) ;
#63432 = CARTESIAN_POINT ( 'NONE',  ( 71.85042758235270810, 71.69843285251393183, -3.789477364735254650 ) ) ;
#63433 = CARTESIAN_POINT ( 'NONE',  ( 42.50247518763358556, 195.3458772461660544, 9.188101187500095079 ) ) ;
#63434 = AXIS2_PLACEMENT_3D ( 'NONE', #50645, #27366, #66848 ) ;
#63435 = CARTESIAN_POINT ( 'NONE',  ( 85.37327613081673405, 48.30298695785122476, -11.79049452454833613 ) ) ;
#63436 = LINE ( 'NONE', #54824, #28634 ) ;
#63437 = ADVANCED_FACE ( 'NONE', ( #22845 ), #13413, .F. ) ;
#63438 = B_SPLINE_SURFACE_WITH_KNOTS ( 'NONE', 3, 1, ( 
 ( #6772, #91912 ),
 ( #29572, #14378 ),
 ( #5770, #37651 ),
 ( #92406, #76671 ),
 ( #54338, #99487 ),
 ( #99986, #15343 ),
 ( #30571, #85310 ),
 ( #38660, #52861 ),
 ( #46239, #44753 ),
 ( #45262, #13872 ),
 ( #91403, #61943 ),
 ( #37167, #77165 ),
 ( #36659, #83310 ),
 ( #29089, #76196 ),
 ( #44262, #6272 ),
 ( #68065, #7766 ),
 ( #22954, #31054 ),
 ( #98989, #53362 ),
 ( #60449, #21968 ),
 ( #68561, #7258 ),
 ( #67565, #83811 ),
 ( #92895, #30065 ),
 ( #59955, #60954 ),
 ( #38141, #84312 ),
 ( #69563, #61456 ),
 ( #23448, #22468 ),
 ( #14859, #53843 ),
 ( #84803, #45746 ),
 ( #170, #75195 ),
 ( #98499, #90927 ),
 ( #21477, #52364 ),
 ( #17881, #46763 ),
 ( #86322, #8767 ),
 ( #79214, #56852 ) ),
 .UNSPECIFIED., .T., .F., .F.,
 ( 4, 2, 2, 2, 2, 2, 2, 2, 2, 2, 2, 2, 2, 2, 2, 2, 4 ),
 ( 2, 2 ),
 ( 0.000000000000000000, 0.06250000000000000000, 0.1250000000000000000, 0.1875000000000000000, 0.2500000000000000000, 0.3125000000000000000, 0.3750000000000000000, 0.4375000000000000000, 0.5000000000000000000, 0.5625000000000000000, 0.6250000000000000000, 0.6875000000000000000, 0.7500000000000000000, 0.8125000000000000000, 0.8750000000000000000, 0.9375000000000000000, 1.000000000000000000 ),
 ( 0.000000000000000000, 1.000000000000000000 ),
 .UNSPECIFIED. ) ;
#63439 = CARTESIAN_POINT ( 'NONE',  ( 80.27865570437573695, 44.72452793390266379, -11.72932060911959518 ) ) ;
#63440 = EDGE_CURVE ( 'NONE', #39976, #81025, #64856, .T. ) ;
#63441 = CARTESIAN_POINT ( 'NONE',  ( 171.2286470186971599, 260.0105123088750361, 14.87178018877357211 ) ) ;
#63442 = FACE_OUTER_BOUND ( 'NONE', #1695, .T. ) ;
#63443 = CARTESIAN_POINT ( 'NONE',  ( 178.8762406774828833, 291.7387019793334275, -6.276231018507565373 ) ) ;
#63444 = CARTESIAN_POINT ( 'NONE',  ( 155.5066938333533528, 261.3015006940112244, -18.40036130547566273 ) ) ;
#63445 = CARTESIAN_POINT ( 'NONE',  ( 156.9489656246467177, 270.6608685179890585, -14.74928785623654548 ) ) ;
#63446 = CARTESIAN_POINT ( 'NONE',  ( 113.3812418268422562, 246.2677522451419065, -5.000000000000047962 ) ) ;
#63447 = CARTESIAN_POINT ( 'NONE',  ( 82.97379378944903294, 51.10958875718078076, -14.34435646701223099 ) ) ;
#63448 = ORIENTED_EDGE ( 'NONE', *, *, #22897, .F. ) ;
#63449 = FACE_OUTER_BOUND ( 'NONE', #93058, .T. ) ;
#63450 = CARTESIAN_POINT ( 'NONE',  ( -22.42236680055709641, 157.8615022471902591, 0.000000000000000000 ) ) ;
#63451 = CARTESIAN_POINT ( 'NONE',  ( 30.10766014385131939, 182.0643266524160424, 9.188101187500095079 ) ) ;
#63452 = CARTESIAN_POINT ( 'NONE',  ( 14.65590419365400976, 24.16454794089040448, -10.00000000000000355 ) ) ;
#63453 = CARTESIAN_POINT ( 'NONE',  ( 77.00817486789587463, 215.2677522451418497, 10.00000000000009592 ) ) ;
#63454 = CARTESIAN_POINT ( 'NONE',  ( 190.1858949294064871, 301.2353624297489887, -5.249932979468886707 ) ) ;
#63455 = CARTESIAN_POINT ( 'NONE',  ( 40.60966550219796289, 208.6868197944957330, 17.47570218321536473 ) ) ;
#63457 = CARTESIAN_POINT ( 'NONE',  ( 49.80054343233469893, 212.8927522451419350, 2.944929066748280225E-16 ) ) ;
#63456 = CARTESIAN_POINT ( 'NONE',  ( 188.5781848808776431, 266.4637148640482565, 13.66955406155852515 ) ) ;
#63458 = CARTESIAN_POINT ( 'NONE',  ( 172.0085750275486305, 287.0065044570835653, 7.467149297792258444 ) ) ;
#63459 = CARTESIAN_POINT ( 'NONE',  ( 181.0892345485566750, 256.4416356510156447, 1.320446355720552134 ) ) ;
#63460 = CARTESIAN_POINT ( 'NONE',  ( 1.826344505407192287, 171.8615022471902591, -10.00000000000009592 ) ) ;
#63461 = CARTESIAN_POINT ( 'NONE',  ( 66.39359272226485587, 68.79637079869742422, -4.330331651545298755 ) ) ;
#63462 = ORIENTED_EDGE ( 'NONE', *, *, #11655, .F. ) ;
#63463 = ADVANCED_FACE ( 'NONE', ( #96282 ), #23161, .F. ) ;
#63464 = CARTESIAN_POINT ( 'NONE',  ( 26.00288702772274618, 192.4865022471903160, 10.00000000000009237 ) ) ;
#63465 = CARTESIAN_POINT ( 'NONE',  ( 199.1165320752825494, 285.7670451491295580, 0.000000000000000000 ) ) ;
#63466 = DIRECTION ( 'NONE',  ( -0.2588190451025239591, -0.9659258262890673130, -6.735114559760606617E-15 ) ) ;
#63467 = CARTESIAN_POINT ( 'NONE',  ( 141.9056932439424372, 261.9244531367911577, -4.594050593750046652 ) ) ;
#63468 = CARTESIAN_POINT ( 'NONE',  ( 30.81771801958594281, 39.83396525600392835, -2.839279412974133887 ) ) ;
#63470 = CARTESIAN_POINT ( 'NONE',  ( 170.3374160014410563, 263.6467931189878868, 15.82539456636149566 ) ) ;
#63469 = CARTESIAN_POINT ( 'NONE',  ( 80.37385980795637863, 57.92309568092906602, -16.24750533957013587 ) ) ;
#63471 = DIRECTION ( 'NONE',  ( -0.000000000000000000, -0.000000000000000000, -1.000000000000000000 ) ) ;
#63472 = CARTESIAN_POINT ( 'NONE',  ( 205.8099205723994203, 269.1131406545866298, -1.356034389334280776 ) ) ;
#63473 = CARTESIAN_POINT ( 'NONE',  ( 183.2877288483369966, 257.5383218783772463, -1.784234248563232317 ) ) ;
#63474 = EDGE_CURVE ( 'NONE', #79225, #20045, #94939, .T. ) ;
#63475 = FACE_OUTER_BOUND ( 'NONE', #65549, .T. ) ;
#63476 = ORIENTED_EDGE ( 'NONE', *, *, #31199, .T. ) ;
#63477 = DIRECTION ( 'NONE',  ( 0.7691052716734860795, 0.08748735329024150131, -0.6331058711608366085 ) ) ;
#63478 = CARTESIAN_POINT ( 'NONE',  ( 178.5703031916296766, 285.5232265560228484, 13.02254804488858753 ) ) ;
#63479 = CARTESIAN_POINT ( 'NONE',  ( 153.4041778544338399, 277.7584533569226437, -5.214878617845980280 ) ) ;
#63480 = CARTESIAN_POINT ( 'NONE',  ( 5.558032429380089567, 24.18502408145589655, 5.678558825948276656 ) ) ;
#63481 = CARTESIAN_POINT ( 'NONE',  ( 160.4502686134403007, 252.7389780038842844, 16.14074205763531111 ) ) ;
#63482 = EDGE_CURVE ( 'NONE', #17038, #1077, #12746, .T. ) ;
#63483 = CARTESIAN_POINT ( 'NONE',  ( 160.0061168334508750, 253.5082714530983026, -16.02306982074888708 ) ) ;
#63484 = CARTESIAN_POINT ( 'NONE',  ( 152.7153488183568300, 266.1362520814392951, 17.33540622643059237 ) ) ;
#63485 = CARTESIAN_POINT ( 'NONE',  ( -13.82959147685579104, 104.2312461070085021, 43.93259070532315036 ) ) ;
#63486 = CARTESIAN_POINT ( 'NONE',  ( 191.0568446278853116, 298.2033705976817828, 9.492902989315558315 ) ) ;
#63487 = CARTESIAN_POINT ( 'NONE',  ( 208.2124092825819162, 270.0125236866795149, -2.339659020816897694 ) ) ;
#63488 = CARTESIAN_POINT ( 'NONE',  ( 155.3738696901333469, 261.5315588585399951, 17.02116401938635804 ) ) ;
#63489 = ORIENTED_EDGE ( 'NONE', *, *, #23185, .T. ) ;
#63490 =( BOUNDED_CURVE ( )  B_SPLINE_CURVE ( 2, ( #5811, #35215, #67105, #13914, #74744, #5324, #21039, #13434, #98536 ),
 .UNSPECIFIED., .F., .T. ) 
 B_SPLINE_CURVE_WITH_KNOTS ( ( 3, 2, 2, 2, 3 ),
 ( 0.4153225806451613100, 0.4166666666666666852, 0.4193548387096774355, 0.4220430107526881858, 0.4233870967741935609 ),
 .UNSPECIFIED. ) 
 CURVE ( )  GEOMETRIC_REPRESENTATION_ITEM ( )  RATIONAL_B_SPLINE_CURVE ( ( 0.9330127018922194093, 0.9330127018922194093, 1.000000000000000000, 0.8660254037844387076, 1.000000000000000000, 0.8660254037844387076, 1.000000000000000000, 0.9330127018922194093, 0.9330127018922194093 ) ) 
 REPRESENTATION_ITEM ( '' )  );
#63491 = ORIENTED_EDGE ( 'NONE', *, *, #90513, .F. ) ;
#63492 = DIRECTION ( 'NONE',  ( -0.4527707594502665689, -0.8916269620120450545, 0.000000000000000000 ) ) ;
#63493 = CARTESIAN_POINT ( 'NONE',  ( 86.44281908042910345, 47.25702098485090374, 10.76508247627446302 ) ) ;
#63494 = VERTEX_POINT ( 'NONE', #45026 ) ;
#63495 = CARTESIAN_POINT ( 'NONE',  ( 69.40701071331325522, 66.80176887165785615, 10.58398152440570783 ) ) ;
#63496 = FACE_OUTER_BOUND ( 'NONE', #40808, .T. ) ;
#63497 = VERTEX_POINT ( 'NONE', #75451 ) ;
#63498 = CARTESIAN_POINT ( 'NONE',  ( 68.76720517553677325, 63.84246230342036199, -12.20210122296020216 ) ) ;
#63499 = CARTESIAN_POINT ( 'NONE',  ( 84.96125173846019152, 48.42999138336367082, -12.07229602349086584 ) ) ;
#63500 = DIRECTION ( 'NONE',  ( -0.8660254037844359321, -0.5000000000000051070, -0.000000000000000000 ) ) ;
#63501 = ORIENTED_EDGE ( 'NONE', *, *, #92550, .T. ) ;
#63502 = CARTESIAN_POINT ( 'NONE',  ( 200.8432122835317841, 282.7763473000181307, 17.15137370990203891 ) ) ;
#63503 = CARTESIAN_POINT ( 'NONE',  ( 40.41628377845468378, 57.12529113016346827, 177.5919119679930134 ) ) ;
#63504 = CARTESIAN_POINT ( 'NONE',  ( 151.3589047706063582, 268.4856820897672378, 14.56544807350869419 ) ) ;
#63505 = DIRECTION ( 'NONE',  ( 0.000000000000000000, 0.000000000000000000, 1.000000000000000000 ) ) ;
#63506 = VERTEX_POINT ( 'NONE', #36930 ) ;
#63507 = CARTESIAN_POINT ( 'NONE',  ( -19.15453390681661716, 24.31945705462845453, -10.00000000000000000 ) ) ;
#63508 = CARTESIAN_POINT ( 'NONE',  ( 163.1484656051875106, 248.0655637253488806, 9.714247672444804138 ) ) ;
#63509 = VECTOR ( 'NONE', #11316, 1000.000000000000000 ) ;
#63510 = ORIENTED_EDGE ( 'NONE', *, *, #218, .T. ) ;
#63511 = ORIENTED_EDGE ( 'NONE', *, *, #23905, .F. ) ;
#63512 = CARTESIAN_POINT ( 'NONE',  ( 74.58922631747108767, 66.95469429158355013, 12.55546573254311937 ) ) ;
#63513 = ORIENTED_EDGE ( 'NONE', *, *, #19029, .T. ) ;
#63514 = CARTESIAN_POINT ( 'NONE',  ( -22.42236680055709641, 157.8615022471902591, 0.000000000000000000 ) ) ;
#63515 = ORIENTED_EDGE ( 'NONE', *, *, #1153, .F. ) ;
#63516 = CARTESIAN_POINT ( 'NONE',  ( 83.08735981439933482, 48.59651280663791084, 12.88586852374721126 ) ) ;
#63518 = ADVANCED_FACE ( 'NONE', ( #75969 ), #58719, .F. ) ;
#63517 = CARTESIAN_POINT ( 'NONE',  ( 70.50418369191052648, 67.51709059444762318, 9.786528338479930866 ) ) ;
#63519 = DIRECTION ( 'NONE',  ( 0.000000000000000000, -1.000000000000000000, 0.000000000000000000 ) ) ;
#63520 = CARTESIAN_POINT ( 'NONE',  ( 174.7053765443823465, 290.4798731644879695, 6.449017960443486963 ) ) ;
#63521 = CARTESIAN_POINT ( 'NONE',  ( -27.42236680055714260, 166.5217562850347406, 1.224646799147364892E-15 ) ) ;
#63522 = EDGE_LOOP ( 'NONE', ( #45294, #19710, #96945, #97308 ) ) ;
#63523 = CARTESIAN_POINT ( 'NONE',  ( 187.1869727329149100, 258.4604987923206068, 2.244340846906317299 ) ) ;
#63524 = CARTESIAN_POINT ( 'NONE',  ( 22.39139443204644664, 24.87878583063842086, -9.188101187500006262 ) ) ;
#63525 = CARTESIAN_POINT ( 'NONE',  ( 164.2572333502590709, 246.1451216570909253, 2.155809084027023204 ) ) ;
#63527 = ORIENTED_EDGE ( 'NONE', *, *, #8680, .F. ) ;
#63526 = CARTESIAN_POINT ( 'NONE',  ( 159.4889735931715222, 254.4039898200529706, 16.88104032092801887 ) ) ;
#63528 = FACE_OUTER_BOUND ( 'NONE', #8205, .T. ) ;
#63529 = CARTESIAN_POINT ( 'NONE',  ( 157.0239713899953244, 269.7369771206523978, 16.31777668093047851 ) ) ;
#63530 = CARTESIAN_POINT ( 'NONE',  ( 206.6298919378964740, 272.7535241315335384, -9.267551915974392429 ) ) ;
#63531 = CYLINDRICAL_SURFACE ( 'NONE', #31176, 49.99999999999999289 ) ;
#63532 = CARTESIAN_POINT ( 'NONE',  ( 200.1102648775588193, 284.0458494464393198, 17.54251420653697835 ) ) ;
#63533 = FACE_OUTER_BOUND ( 'NONE', #46278, .T. ) ;
#63534 = VERTEX_POINT ( 'NONE', #82595 ) ;
#63535 = CARTESIAN_POINT ( 'NONE',  ( 193.9864735853334707, 294.6525670995212067, -15.54227678654798694 ) ) ;
#63536 = DIRECTION ( 'NONE',  ( -0.9890802632347809320, 0.1473778574936430164, 0.000000000000000000 ) ) ;
#63537 = CARTESIAN_POINT ( 'NONE',  ( 54.63354020801842381, 213.8967562850347122, -4.648177544792955347E-16 ) ) ;
#63538 = CARTESIAN_POINT ( 'NONE',  ( 16.81940930487741426, 170.5177522451417929, 5.000000000000051514 ) ) ;
#63539 = CARTESIAN_POINT ( 'NONE',  ( 79.22710464504368133, 225.7369531367911293, -4.594050593750048428 ) ) ;
#63540 = EDGE_CURVE ( 'NONE', #2381, #20300, #95125, .T. ) ;
#63541 = CARTESIAN_POINT ( 'NONE',  ( 82.14352512031462084, 40.76412825037346721, -0.7169653898824394078 ) ) ;
#63542 = DIRECTION ( 'NONE',  ( -0.5000000000000006661, 0.8660254037844382635, -1.877843081442121204E-16 ) ) ;
#63543 = CARTESIAN_POINT ( 'NONE',  ( -50.41871976035449165, 31.58591985673634639, -10.00000000000000000 ) ) ;
#63545 = CARTESIAN_POINT ( 'NONE',  ( 75.84977083960791333, 65.49147256048033228, 14.30114164871031335 ) ) ;
#63544 = CARTESIAN_POINT ( 'NONE',  ( 7.428446334363822956, 175.0958772461660544, -9.188101187500095079 ) ) ;
#63546 = CARTESIAN_POINT ( 'NONE',  ( -17.33262083840142509, 129.0458036431182904, -21.50000000000003197 ) ) ;
#63547 = ORIENTED_EDGE ( 'NONE', *, *, #2899, .F. ) ;
#63549 = VERTEX_POINT ( 'NONE', #63232 ) ;
#63548 = PRODUCT_DEFINITION_CONTEXT ( 'detailed design', #5180, 'design' ) ;
#63550 = CARTESIAN_POINT ( 'NONE',  ( 1.396987757676509734, 24.30466486950695071, 0.000000000000000000 ) ) ;
#63551 = CARTESIAN_POINT ( 'NONE',  ( 187.9019955452718023, 260.0457317612239194, -6.306085470763082235 ) ) ;
#63552 = EDGE_CURVE ( 'NONE', #83741, #73589, #81663, .T. ) ;
#63553 = CARTESIAN_POINT ( 'NONE',  ( 88.22357128540845395, 44.11249832625940570, 0.5032066602140912170 ) ) ;
#63554 = B_SPLINE_CURVE_WITH_KNOTS ( 'NONE', 3,
 ( #78911, #1894, #85538, #16080, #39852, #24185, #94123, #39358, #71302, #86544, #17075, #62666, #46985, #55068, #70272, #47965, #86053, #16578, #15562, #32276, #883, #47476, #87050, #31762 ),
 .UNSPECIFIED., .F., .F.,
 ( 4, 2, 2, 2, 2, 2, 2, 2, 2, 2, 2, 4 ),
 ( 0.000000000000000000, 0.1249999999999993894, 0.2499999999999987788, 0.3749999999999981681, 0.4374999999999897304, 0.4999999999999812372, 0.5624999999999726885, 0.6249999999999642508, 0.6874999999999557021, 0.7499999999999471534, 0.8749999999999735767, 1.000000000000000000 ),
 .UNSPECIFIED. ) ;
#63555 = EDGE_CURVE ( 'NONE', #8043, #41536, #11666, .T. ) ;
#63556 = CARTESIAN_POINT ( 'NONE',  ( 33.14931559527707350, 20.10801979619930435, 3.090169943749476733 ) ) ;
#63557 = CARTESIAN_POINT ( 'NONE',  ( 161.8807657183444064, 250.2612843381103573, -13.52770735624900311 ) ) ;
#63558 = CARTESIAN_POINT ( 'NONE',  ( 185.7234768551323896, 286.5997348792201933, 15.91907032080574780 ) ) ;
#63559 = CARTESIAN_POINT ( 'NONE',  ( 74.20878020607858616, 68.72316200637693839, -11.41572480156362879 ) ) ;
#63560 = CARTESIAN_POINT ( 'NONE',  ( 43.09804120061789945, 189.5643266524160140, 9.188101187500095079 ) ) ;
#63561 = CARTESIAN_POINT ( 'NONE',  ( 86.02927282398381692, 207.1427522451417644, 1.119607411625061291E-15 ) ) ;
#63562 = CARTESIAN_POINT ( 'NONE',  ( 198.1145155272607212, 276.7736982920383753, 15.18375391169536393 ) ) ;
#63563 = ORIENTED_EDGE ( 'NONE', *, *, #75650, .F. ) ;
#63564 = CARTESIAN_POINT ( 'NONE',  ( 82.68335232665059209, 44.33947160102358964, 9.174560444508216506 ) ) ;
#63565 = CARTESIAN_POINT ( 'NONE',  ( 175.1244175801234348, 281.4242832285925147, -15.54073688850160018 ) ) ;
#63566 = CIRCLE ( 'NONE', #19914, 17.82106496071138224 ) ;
#63567 = CARTESIAN_POINT ( 'NONE',  ( -9.134289513013563067, 165.5333772461660828, 9.188101187500095079 ) ) ;
#63568 = CARTESIAN_POINT ( 'NONE',  ( 25.34687108590969729, 93.06504152958497400, 20.00000000000000355 ) ) ;
#63569 = CARTESIAN_POINT ( 'NONE',  ( 151.2964716097791325, 268.5938194963972592, -15.66250187539618111 ) ) ;
#63570 = CARTESIAN_POINT ( 'NONE',  ( 187.2161039051867704, 282.9898844212582958, 16.21219487239775958 ) ) ;
#63571 = CARTESIAN_POINT ( 'NONE',  ( 194.8432095198904221, 293.1686569321988145, -14.74101036184996616 ) ) ;
#63572 = VECTOR ( 'NONE', #65821, 1000.000000000000000 ) ;
#63573 = CARTESIAN_POINT ( 'NONE',  ( 189.5675921607796965, 262.4732863060856971, 8.237194270739541579 ) ) ;
#63574 = CARTESIAN_POINT ( 'NONE',  ( 204.2556901454867955, 276.8657622634082713, 13.61111001399713949 ) ) ;
#63575 = CARTESIAN_POINT ( 'NONE',  ( 147.0721334091522294, 275.9105878882373304, 0.7242168585908188572 ) ) ;
#63576 = CARTESIAN_POINT ( 'NONE',  ( 190.1730848958311810, 301.2575500587478814, 0.2415986433272204748 ) ) ;
#63577 = ORIENTED_EDGE ( 'NONE', *, *, #85775, .T. ) ;
#63578 = EDGE_CURVE ( 'NONE', #44048, #59643, #38177, .T. ) ;
#63579 = CARTESIAN_POINT ( 'NONE',  ( 163.9354095869165633, 246.7025367662834014, -7.289870401565430313 ) ) ;
#63580 = CARTESIAN_POINT ( 'NONE',  ( 181.1268834691935297, 268.2382088362665513, 15.85390869987196538 ) ) ;
#63581 = CARTESIAN_POINT ( 'NONE',  ( 101.8248682511026573, 241.8464784336661353, 1.353441290958777327E-15 ) ) ;
#63582 = CARTESIAN_POINT ( 'NONE',  ( 10.31635424878816742, 24.14336893147753926, 7.433330006724141015 ) ) ;
#63583 = CARTESIAN_POINT ( 'NONE',  ( 73.03004930954443807, 60.83881918362380503, -15.55364876364052051 ) ) ;
#63584 = DIRECTION ( 'NONE',  ( 0.4999999999999992784, -0.8660254037844390407, 0.000000000000000000 ) ) ;
#63585 = AXIS2_PLACEMENT_3D ( 'NONE', #86707, #25345, #92422 ) ;
#63587 = LINE ( 'NONE', #94528, #39240 ) ;
#63586 = CARTESIAN_POINT ( 'NONE',  ( 196.0395593785976018, 291.0965181932902510, 15.97855489120023087 ) ) ;
#63588 = CARTESIAN_POINT ( 'NONE',  ( 151.4352206443128068, 277.3697824090307336, -6.572806124296932673 ) ) ;
#63589 = CARTESIAN_POINT ( 'NONE',  ( 20.88255934282640425, 35.55466486950700045, -1.111400068045478839E-16 ) ) ;
#63590 = CARTESIAN_POINT ( 'NONE',  ( 196.6288634187112052, 290.0758136547079289, -16.31544900032282186 ) ) ;
#63591 = CARTESIAN_POINT ( 'NONE',  ( 41.76871284172324295, 36.06628583063844928, -9.188101187500006262 ) ) ;
#63592 = CARTESIAN_POINT ( 'NONE',  ( 203.8165033694633621, 276.7299672189732291, 13.95262359560297583 ) ) ;
#63593 = DIRECTION ( 'NONE',  ( -0.4493970231495795775, 0.7783784768652820540, -0.4383711467890876734 ) ) ;
#63594 = ORIENTED_EDGE ( 'NONE', *, *, #62851, .F. ) ;
#63595 = CARTESIAN_POINT ( 'NONE',  ( 189.3573010603350895, 265.1416018912782420, 12.05679781153855323 ) ) ;
#63596 = LINE ( 'NONE', #48404, #60432 ) ;
#63597 = CARTESIAN_POINT ( 'NONE',  ( 197.8518484210461281, 268.8967432528903032, 9.285919980081231984 ) ) ;
#63598 = ADVANCED_FACE ( 'NONE', ( #32331 ), #33862, .T. ) ;
#63599 = ORIENTED_EDGE ( 'NONE', *, *, #22163, .T. ) ;
#63600 = CARTESIAN_POINT ( 'NONE',  ( 79.24255149360672590, 50.29911346356186641, 14.82443660399750485 ) ) ;
#63601 = CARTESIAN_POINT ( 'NONE',  ( 83.91397729048109966, 51.84092357031820342, -14.47588020021706612 ) ) ;
#63602 = FACE_OUTER_BOUND ( 'NONE', #26420, .T. ) ;
#63603 = CARTESIAN_POINT ( 'NONE',  ( 153.3920560952016956, 264.9641606960921649, 16.50453917291963535 ) ) ;
#63604 = ORIENTED_EDGE ( 'NONE', *, *, #80555, .F. ) ;
#63605 = PLANE ( 'NONE',  #98987 ) ;
#63606 = CARTESIAN_POINT ( 'NONE',  ( 31.85034293892215018, 41.49540643055189548, 3.479690158560446702E-15 ) ) ;
#63607 = CARTESIAN_POINT ( 'NONE',  ( 195.2456755912178323, 290.2219180048303429, -16.53585882530188655 ) ) ;
#63608 = ORIENTED_EDGE ( 'NONE', *, *, #3840, .F. ) ;
#63609 = B_SPLINE_CURVE_WITH_KNOTS ( 'NONE', 3,
 ( #86569, #17101, #36789, #89558 ),
 .UNSPECIFIED., .F., .F.,
 ( 4, 4 ),
 ( 0.03111358529414371549, 0.04015756546154605061 ),
 .UNSPECIFIED. ) ;
#63610 = CARTESIAN_POINT ( 'NONE',  ( 166.8963927329958494, 280.5591284459779331, 11.67036085821709612 ) ) ;
#63611 = CARTESIAN_POINT ( 'NONE',  ( 148.0346525705264469, 274.2434557974783615, -9.381294579651672905 ) ) ;
#63612 = CARTESIAN_POINT ( 'NONE',  ( 193.9979983253333842, 262.2552985615510579, -0.8131695963413709816 ) ) ;
#63613 = ORIENTED_EDGE ( 'NONE', *, *, #54575, .T. ) ;
#63614 = CARTESIAN_POINT ( 'NONE',  ( 86.33167747996513697, 46.96304910452010262, -10.52679092302836317 ) ) ;
#63615 = CYLINDRICAL_SURFACE ( 'NONE', #92901, 17.82106496071139645 ) ;
#63616 = B_SPLINE_CURVE_WITH_KNOTS ( 'NONE', 3,
 ( #66399, #20312, #4097, #5596 ),
 .UNSPECIFIED., .F., .F.,
 ( 4, 4 ),
 ( 0.008060310584812914458, 0.01415263866924437036 ),
 .UNSPECIFIED. ) ;
#63617 = CARTESIAN_POINT ( 'NONE',  ( 72.14936367153653407, 200.9155109091896065, 2.679491924311254714 ) ) ;
#63618 = CARTESIAN_POINT ( 'NONE',  ( 25.96360177180014972, 20.15404122711134249, 8.090169943749479842 ) ) ;
#63619 = LINE ( 'NONE', #72757, #81838 ) ;
#63620 = CYLINDRICAL_SURFACE ( 'NONE', #85869, 70.00000000000002842 ) ;
#63621 = CARTESIAN_POINT ( 'NONE',  ( 80.24672568527826400, 44.80204066275088337, 11.13114128994728524 ) ) ;
#63622 = CARTESIAN_POINT ( 'NONE',  ( 84.85099494643192486, 49.96072780641430455, -13.19879633021795939 ) ) ;
#63623 = CARTESIAN_POINT ( 'NONE',  ( 203.0862352702880003, 278.8913175244117610, -15.09542727681365015 ) ) ;
#63624 = VERTEX_POINT ( 'NONE', #11554 ) ;
#63625 = ORIENTED_EDGE ( 'NONE', *, *, #31534, .T. ) ;
#63626 = CARTESIAN_POINT ( 'NONE',  ( 202.6051175132338926, 273.9538057854381350, -13.19822448684500849 ) ) ;
#63627 = EDGE_LOOP ( 'NONE', ( #44162, #34018, #19949 ) ) ;
#63628 = CARTESIAN_POINT ( 'NONE',  ( 77.28539951127001473, 49.71994323448210196, -14.99865734462259148 ) ) ;
#63630 = ORIENTED_EDGE ( 'NONE', *, *, #508, .F. ) ;
#63629 = EDGE_CURVE ( 'NONE', #43398, #61969, #89070, .T. ) ;
#63631 = CARTESIAN_POINT ( 'NONE',  ( 173.1389949595530311, 270.9080448422716927, 16.48212318985030578 ) ) ;
#63632 = CARTESIAN_POINT ( 'NONE',  ( 78.19591265575934358, 48.92920433772970057, 14.51337752615410359 ) ) ;
#63633 = ORIENTED_EDGE ( 'NONE', *, *, #68378, .T. ) ;
#63634 = CARTESIAN_POINT ( 'NONE',  ( 184.8055014132766303, 281.5399926389359280, -16.29175395855951791 ) ) ;
#63635 = CARTESIAN_POINT ( 'NONE',  ( 165.0748171242677245, 244.7290250210644729, -1.867635796467185028 ) ) ;
#63636 = CARTESIAN_POINT ( 'NONE',  ( 190.4843783887033055, 300.7183739130279037, 3.438264421829949402 ) ) ;
#63637 = DIRECTION ( 'NONE',  ( 0.8660254037844395958, 0.4999999999999985567, 0.000000000000000000 ) ) ;
#63638 = CARTESIAN_POINT ( 'NONE',  ( 79.01390229250786490, 46.15383090619681639, 12.74691942439358350 ) ) ;
#63640 = EDGE_CURVE ( 'NONE', #1592, #54743, #25228, .T. ) ;
#63639 = CARTESIAN_POINT ( 'NONE',  ( 153.1961624462112752, 265.3034584490234806, -16.19494717845262954 ) ) ;
#63641 = FACE_OUTER_BOUND ( 'NONE', #6963, .T. ) ;
#63642 = CARTESIAN_POINT ( 'NONE',  ( 154.0986224399686648, 280.1916420498395155, 2.233781007141098396 ) ) ;
#63643 = CARTESIAN_POINT ( 'NONE',  ( 126.9399520566163773, 244.0958772461660544, -9.188101187500095079 ) ) ;
#63644 = CARTESIAN_POINT ( 'NONE',  ( 70.70263562602700347, 60.54883119609748832, -14.66132127786565142 ) ) ;
#63645 = CARTESIAN_POINT ( 'NONE',  ( 44.43411998782967487, 26.44966523072497822, -2.296566073217252530E-15 ) ) ;
#63646 = VERTEX_POINT ( 'NONE', #49529 ) ;
#63648 = VERTEX_POINT ( 'NONE', #88598 ) ;
#63647 = CARTESIAN_POINT ( 'NONE',  ( 86.59925754919576946, 43.68706288513137537, -5.068886987635317531 ) ) ;
#63649 = CARTESIAN_POINT ( 'NONE',  ( 203.6418419907373902, 276.2461351259622688, 13.34765691815280952 ) ) ;
#63650 = DIRECTION ( 'NONE',  ( -0.5000000000000014433, 0.8660254037844377084, 0.000000000000000000 ) ) ;
#63651 = CARTESIAN_POINT ( 'NONE',  ( 171.5263804624986790, 288.0246480763028671, -4.629733576150550256 ) ) ;
#63652 = CARTESIAN_POINT ( 'NONE',  ( 192.7575593570047090, 296.7811089811312399, 12.30688046782918121 ) ) ;
#63653 = CARTESIAN_POINT ( 'NONE',  ( 72.38627258597001912, 63.15220171016905226, 13.97079549884010596 ) ) ;
#63654 = CARTESIAN_POINT ( 'NONE',  ( 194.8644079090977357, 267.3518508506872990, 11.26063562417210484 ) ) ;
#63655 = CARTESIAN_POINT ( 'NONE',  ( 175.6817329609027354, 287.9557713606999982, -9.344572807206340315 ) ) ;
#63656 = CARTESIAN_POINT ( 'NONE',  ( 28.39959312520600676, 35.13478043621390157, 8.090169943749478065 ) ) ;
#63657 = CARTESIAN_POINT ( 'NONE',  ( 177.1731152019401350, 256.0265825107734372, -7.293953335171803332 ) ) ;
#63658 = ORIENTED_EDGE ( 'NONE', *, *, #67437, .T. ) ;
#63659 = CARTESIAN_POINT ( 'NONE',  ( 147.6054094044680198, 274.9869267698931594, -8.596541856229405809 ) ) ;
#63660 = CARTESIAN_POINT ( 'NONE',  ( 3.692648916086829658, 184.4860189848785410, -2.679491924311252493 ) ) ;
#63661 = VECTOR ( 'NONE', #47389, 999.9999999999998863 ) ;
#63662 = VERTEX_POINT ( 'NONE', #1942 ) ;
#63663 = CARTESIAN_POINT ( 'NONE',  ( 168.1726423428391399, 255.4859975196775963, 14.21197738914692366 ) ) ;
#63664 = AXIS2_PLACEMENT_3D ( 'NONE', #85343, #61491, #201 ) ;
#63665 = CARTESIAN_POINT ( 'NONE',  ( 190.9492529716546017, 283.2944616250604213, -16.57272652201862329 ) ) ;
#63666 = CARTESIAN_POINT ( 'NONE',  ( 13.01414456110373052, 45.20707939394876007, 59.99999999999999289 ) ) ;
#63667 = CARTESIAN_POINT ( 'NONE',  ( 149.6676065383367416, 271.4150965588098074, 11.80358707172367261 ) ) ;
#63668 = CARTESIAN_POINT ( 'NONE',  ( 202.6070187115982719, 279.7213449518906145, 15.56322169823762280 ) ) ;
#63670 = CARTESIAN_POINT ( 'NONE',  ( 154.4470374439381146, 277.6591429590598068, -9.115886381272481742 ) ) ;
#63669 = CARTESIAN_POINT ( 'NONE',  ( 164.6578333510718721, 283.8482461527818259, -6.790344748163971822 ) ) ;
#63671 = CARTESIAN_POINT ( 'NONE',  ( 153.0308080659177392, 265.5898606369461277, -17.74682723936668438 ) ) ;
#63672 = VERTEX_POINT ( 'NONE', #2969 ) ;
#63673 = CARTESIAN_POINT ( 'NONE',  ( 166.4230964287024506, 281.1278175241628787, -10.97197584377154200 ) ) ;
#63674 = B_SPLINE_SURFACE_WITH_KNOTS ( 'NONE', 3, 1, ( 
 ( #83765, #15296 ),
 ( #45214, #13825 ),
 ( #76152, #44704 ),
 ( #37605, #86780 ),
 ( #70513, #54293 ),
 ( #32525, #32003 ),
 ( #63914, #78134 ),
 ( #16813, #8721 ),
 ( #23404, #33015 ),
 ( #31503, #85263 ),
 ( #47700, #15808 ),
 ( #33525, #79667 ),
 ( #17314, #55787 ),
 ( #86277, #62398 ),
 ( #2638, #622 ),
 ( #56305, #63420 ),
 ( #92851, #41098 ),
 ( #79166, #93353 ),
 ( #94853, #48218 ),
 ( #1642, #78638 ),
 ( #8225, #48733 ),
 ( #40098, #17834 ),
 ( #24420, #9745 ),
 ( #46713, #54810 ),
 ( #39592, #40603 ),
 ( #77641, #71539 ),
 ( #2132, #25413 ),
 ( #87301, #10229 ),
 ( #72034, #47211 ),
 ( #93864, #39094 ),
 ( #70007, #23910 ) ),
 .UNSPECIFIED., .F., .F., .F.,
 ( 4, 3, 3, 3, 3, 3, 3, 3, 3, 3, 4 ),
 ( 2, 2 ),
 ( 0.000000000000000000, 0.1333490885032327655, 0.3007194338854324855, 0.4699862290245073182, 0.5844252810809297261, 0.6686540514502762322, 0.7354980260655518132, 0.8028463152565620264, 0.8633854507757146024, 0.9437142632667205877, 1.000000000000000000 ),
 ( 0.000000000000000000, 1.000000000000000000 ),
 .UNSPECIFIED. ) ;
#63675 = CARTESIAN_POINT ( 'NONE',  ( 187.4171132689631634, 261.5282790321019206, -9.397869408254909018 ) ) ;
#63676 = DIRECTION ( 'NONE',  ( -0.8660254037844359321, -0.5000000000000051070, -0.000000000000000000 ) ) ;
#63677 = FACE_OUTER_BOUND ( 'NONE', #59874, .T. ) ;
#63678 = EDGE_CURVE ( 'NONE', #41092, #99018, #17128, .T. ) ;
#63679 = CARTESIAN_POINT ( 'NONE',  ( -19.42194755839791753, 24.31068691715150010, 10.00000000000000000 ) ) ;
#63680 = CARTESIAN_POINT ( 'NONE',  ( 204.2465476932143531, 275.5256217290955192, 13.24663835785611710 ) ) ;
#63681 = EDGE_CURVE ( 'NONE', #18286, #67256, #19161, .T. ) ;
#63682 = CARTESIAN_POINT ( 'NONE',  ( 41.37327796571899796, 124.7191351846657028, -10.00000000000000000 ) ) ;
#63683 = CARTESIAN_POINT ( 'NONE',  ( 155.1376601545389917, 261.9406857754215707, 18.55063430030667959 ) ) ;
#63684 = CARTESIAN_POINT ( 'NONE',  ( 167.2415451205598345, 247.5609011665888772, -4.849568200425117048 ) ) ;
#63685 = EDGE_CURVE ( 'NONE', #72572, #96097, #63736, .T. ) ;
#63686 = CARTESIAN_POINT ( 'NONE',  ( 93.00275509369619442, 218.3768266524159856, -9.188101187500091527 ) ) ;
#63687 = LINE ( 'NONE', #55564, #16855 ) ;
#63688 = CARTESIAN_POINT ( 'NONE',  ( 146.9700173529739970, 276.0874580858064746, -5.099093031535578469 ) ) ;
#63689 = CARTESIAN_POINT ( 'NONE',  ( 148.0447915602865976, 275.7505707160540283, 4.987173999238420308 ) ) ;
#63690 = EDGE_CURVE ( 'NONE', #4764, #5671, #92604, .T. ) ;
#63691 = CARTESIAN_POINT ( 'NONE',  ( 155.2193237801463113, 261.7992402267395846, -18.58295809893692407 ) ) ;
#63692 = CARTESIAN_POINT ( 'NONE',  ( 77.57362400355269472, 52.51412412160524923, 15.74026747803791437 ) ) ;
#63693 = CARTESIAN_POINT ( 'NONE',  ( 36.38358746446922254, 51.11404133282111673, 10.00000000000000000 ) ) ;
#63694 = CARTESIAN_POINT ( 'NONE',  ( 77.93222884788742988, 62.01307363188976751, 15.66297058137760345 ) ) ;
#63697 = CARTESIAN_POINT ( 'NONE',  ( 76.61699804220991439, 51.35236863086766590, 16.07092595041460470 ) ) ;
#63696 = B_SPLINE_CURVE_WITH_KNOTS ( 'NONE', 3,
 ( #69005, #30015, #23402, #99438, #85262, #91863, #38094, #83258, #99935, #83764, #15295, #92360, #52807, #14325, #29527, #76151 ),
 .UNSPECIFIED., .F., .F.,
 ( 4, 2, 2, 2, 2, 2, 2, 4 ),
 ( 3.103167691559091397E-17, 0.0003787177898467000204, 0.0007574355796933690326, 0.001136153369540038099, 0.001514871159386707057, 0.001893588949233376015, 0.002272306739080045407, 0.003029742318773331715 ),
 .UNSPECIFIED. ) ;
#63695 = DIRECTION ( 'NONE',  ( 0.4330127018922195758, 0.2500000000000004441, 0.8660254037844384856 ) ) ;
#63698 = CARTESIAN_POINT ( 'NONE',  ( 178.8990464802429017, 290.1033400482242541, 9.442229793486959011 ) ) ;
#63699 = CARTESIAN_POINT ( 'NONE',  ( 169.2468562361510465, 252.1710243214491527, -8.924574812386079969 ) ) ;
#63700 = CARTESIAN_POINT ( 'NONE',  ( 172.4419760422836134, 290.9306500000749907, -0.6531725299933459628 ) ) ;
#63701 = CARTESIAN_POINT ( 'NONE',  ( 75.85550969639162133, 55.85942037733559573, -16.16270098209340489 ) ) ;
#63702 = CARTESIAN_POINT ( 'NONE',  ( -10.02737821244022776, 165.0177522451418781, -10.00000000000009592 ) ) ;
#63703 = CARTESIAN_POINT ( 'NONE',  ( 73.67568143663486069, 69.57707014568420334, 9.664179533016600487 ) ) ;
#63704 = CARTESIAN_POINT ( 'NONE',  ( 42.55642822748761489, 201.5024278399160949, 9.188101187500095079 ) ) ;
#63705 = EDGE_CURVE ( 'NONE', #46236, #35455, #10545, .T. ) ;
#63706 = DIRECTION ( 'NONE',  ( 1.000000000000000000, 0.000000000000000000, 0.000000000000000000 ) ) ;
#63707 = CARTESIAN_POINT ( 'NONE',  ( 72.16419236301562989, 200.2202760586659736, -5.415160957724236172E-17 ) ) ;
#63708 = CARTESIAN_POINT ( 'NONE',  ( 164.1344181360771870, 246.9811661530827962, -5.863116506140533701 ) ) ;
#63709 = PLANE ( 'NONE',  #65392 ) ;
#63710 = DIRECTION ( 'NONE',  ( -0.000000000000000000, -0.000000000000000000, -1.000000000000000000 ) ) ;
#63712 = CARTESIAN_POINT ( 'NONE',  ( 74.67000616351420206, 66.81477949400924388, -13.12245706047550797 ) ) ;
#63711 = PLANE ( 'NONE',  #11269 ) ;
#63713 = CARTESIAN_POINT ( 'NONE',  ( 11.71892835771565800, 189.1199935810941213, 2.679491924311251605 ) ) ;
#63714 = CARTESIAN_POINT ( 'NONE',  ( 25.62156559687931434, 36.83396525600391413, -2.839279412974133887 ) ) ;
#63715 = DIRECTION ( 'NONE',  ( -0.9825923819316307872, -0.1857746241280658905, 0.000000000000000000 ) ) ;
#63716 = CARTESIAN_POINT ( 'NONE',  ( 196.2379679265050925, 290.7528645076583871, -16.93678934971137906 ) ) ;
#63717 = ORIENTED_EDGE ( 'NONE', *, *, #20664, .T. ) ;
#63718 = CARTESIAN_POINT ( 'NONE',  ( 15.51250667149479590, 27.14336893147754992, 7.433330006724141015 ) ) ;
#63719 = CARTESIAN_POINT ( 'NONE',  ( 72.21814540286966633, 206.3768266524159571, -9.188101187500093303 ) ) ;
#63720 = CARTESIAN_POINT ( 'NONE',  ( 76.53355563625230218, 63.67723833686833501, 14.89832570204743156 ) ) ;
#63721 = CARTESIAN_POINT ( 'NONE',  ( 155.5066938333533528, 261.3015006940112244, -18.40036130547566273 ) ) ;
#63722 = CARTESIAN_POINT ( 'NONE',  ( 172.9367659230471190, 289.5787789514328097, -1.054365525152276772 ) ) ;
#63723 = DIRECTION ( 'NONE',  ( -0.06415622980648827411, 0.9979398670145497308, 0.000000000000000000 ) ) ;
#63724 = CARTESIAN_POINT ( 'NONE',  ( 201.5239699368452193, 281.5972404568383354, 17.74311413406459792 ) ) ;
#63725 = VECTOR ( 'NONE', #81121, 999.9999999999998863 ) ;
#63726 = CARTESIAN_POINT ( 'NONE',  ( 87.56524498856292382, 45.09937575355993999, -6.113837049084305697 ) ) ;
#63727 = CARTESIAN_POINT ( 'NONE',  ( 123.1420698188773315, 235.2365022471902023, 10.00000000000009592 ) ) ;
#63728 = DIRECTION ( 'NONE',  ( -0.000000000000000000, -1.000000000000000000, -0.000000000000000000 ) ) ;
#63729 = CARTESIAN_POINT ( 'NONE',  ( 164.6649740431187183, 245.4388940607451843, -1.430729255012818557 ) ) ;
#63730 = VERTEX_POINT ( 'NONE', #32828 ) ;
#63731 = VECTOR ( 'NONE', #88063, 1000.000000000000114 ) ;
#63732 = CARTESIAN_POINT ( 'NONE',  ( 149.0466799873937020, 273.2901661242311206, -9.699341834421078445 ) ) ;
#63733 = CARTESIAN_POINT ( 'NONE',  ( 187.9132866086108891, 273.2693441326987340, 15.64203133854969963 ) ) ;
#63734 = VERTEX_POINT ( 'NONE', #41930 ) ;
#63735 = CARTESIAN_POINT ( 'NONE',  ( 202.2712651538608668, 280.3028871727136675, 16.13191389836473988 ) ) ;
#63736 = LINE ( 'NONE', #96174, #1280 ) ;
#63737 = CARTESIAN_POINT ( 'NONE',  ( 71.86256228778262312, 72.60615528678948749, -0.5650332253008888417 ) ) ;
#63738 = VERTEX_POINT ( 'NONE', #26735 ) ;
#63739 = CARTESIAN_POINT ( 'NONE',  ( 176.7648174719832639, 252.3281646357263241, -0.2701238880731380854 ) ) ;
#63741 = ORIENTED_EDGE ( 'NONE', *, *, #80079, .T. ) ;
#63740 = CIRCLE ( 'NONE', #99330, 70.00000000000001421 ) ;
#63742 = CARTESIAN_POINT ( 'NONE',  ( 72.48128350488923388, 71.72257018173657173, 5.902110541236701202 ) ) ;
#63743 = CARTESIAN_POINT ( 'NONE',  ( 170.6258808213388249, 250.4240718389760332, 3.381858602187873153 ) ) ;
#63744 = CARTESIAN_POINT ( 'NONE',  ( 159.5606259118165724, 264.0648208006689401, -17.79391822139266566 ) ) ;
#63745 = EDGE_CURVE ( 'NONE', #66781, #49648, #36934, .T. ) ;
#63746 = ORIENTED_EDGE ( 'NONE', *, *, #11228, .F. ) ;
#63747 = CARTESIAN_POINT ( 'NONE',  ( 25.85549604718420014, 26.87878583063842797, -9.188101187500006262 ) ) ;
#63748 = CARTESIAN_POINT ( 'NONE',  ( 80.11408820379499218, 44.30976117890687505, 11.44504534144087415 ) ) ;
#63749 = CARTESIAN_POINT ( 'NONE',  ( 84.55537670905214043, 50.62155581810768012, -14.09136642048690646 ) ) ;
#63750 = CARTESIAN_POINT ( 'NONE',  ( 50.60128122559382291, 92.19983735941717384, 10.00000000000000000 ) ) ;
#63751 = FACE_OUTER_BOUND ( 'NONE', #25963, .T. ) ;
#63752 = CARTESIAN_POINT ( 'NONE',  ( -19.65312891409030271, 93.06504152958497400, 177.5919119679930134 ) ) ;
#63753 = ORIENTED_EDGE ( 'NONE', *, *, #63360, .T. ) ;
#63754 = ORIENTED_EDGE ( 'NONE', *, *, #63853, .T. ) ;
#63755 = CARTESIAN_POINT ( 'NONE',  ( 186.3453228331337073, 298.4577095622237835, 1.059573036266669765 ) ) ;
#63757 = CARTESIAN_POINT ( 'NONE',  ( 148.1974503712686158, 273.9614817352322120, -7.884397846570731616 ) ) ;
#63756 = CARTESIAN_POINT ( 'NONE',  ( 67.64202414628154258, 65.88146472340838500, 10.47854541773734738 ) ) ;
#63758 = LINE ( 'NONE', #39430, #59417 ) ;
#63759 = CARTESIAN_POINT ( 'NONE',  ( 155.4186054393023255, 261.4540742680644598, 17.05753227160644769 ) ) ;
#63760 = CARTESIAN_POINT ( 'NONE',  ( 185.4122142602475378, 292.4855490106422735, -11.52758158381046449 ) ) ;
#63761 = CARTESIAN_POINT ( 'NONE',  ( 157.4211152037729562, 257.9856256133486454, -16.71526195140576831 ) ) ;
#63762 = CARTESIAN_POINT ( 'NONE',  ( 164.7117522571876123, 245.3578718172906292, 5.414774406097063064 ) ) ;
#63763 = CARTESIAN_POINT ( 'NONE',  ( 206.6977975800406284, 270.2202961249453779, 3.296240252125988146 ) ) ;
#63764 = LINE ( 'NONE', #96203, #74278 ) ;
#63765 = CARTESIAN_POINT ( 'NONE',  ( 87.80660267098954819, 215.3768266524160140, -9.188101187500091527 ) ) ;
#63766 = VERTEX_POINT ( 'NONE', #48542 ) ;
#63767 = CARTESIAN_POINT ( 'NONE',  ( 191.5544531425776427, 298.8649500714207647, 8.366689293739112188 ) ) ;
#63768 = CARTESIAN_POINT ( 'NONE',  ( 179.0110060009473045, 253.5811209532878934, 0.3050717900565249607 ) ) ;
#63769 = VERTEX_POINT ( 'NONE', #40908 ) ;
#63770 = CARTESIAN_POINT ( 'NONE',  ( 156.6814027994969933, 259.2668450805435896, -17.66460052862722918 ) ) ;
#63771 = VERTEX_POINT ( 'NONE', #79481 ) ;
#63772 = CARTESIAN_POINT ( 'NONE',  ( 187.0997774576600534, 269.0605681235749671, -15.68935166958139149 ) ) ;
#63773 = PLANE ( 'NONE',  #17116 ) ;
#63774 = DIRECTION ( 'NONE',  ( -0.5000000000000013323, 0.8660254037844379305, 0.000000000000000000 ) ) ;
#63775 = CARTESIAN_POINT ( 'NONE',  ( 164.2083349707763489, 249.9453208731862048, 10.14950949454277485 ) ) ;
#63776 = CARTESIAN_POINT ( 'NONE',  ( 81.06232478827473642, 48.19955485970237419, -13.34453326799301465 ) ) ;
#63777 = CARTESIAN_POINT ( 'NONE',  ( 98.14495447654879001, 215.2202760586659167, -5.415160957724236172E-17 ) ) ;
#63778 = ORIENTED_EDGE ( 'NONE', *, *, #83384, .F. ) ;
#63779 = ORIENTED_EDGE ( 'NONE', *, *, #12401, .F. ) ;
#63780 = CARTESIAN_POINT ( 'NONE',  ( 161.2672255145357383, 251.3239671435932223, -13.23747325324243995 ) ) ;
#63781 = ORIENTED_EDGE ( 'NONE', *, *, #64816, .T. ) ;
#63782 = CARTESIAN_POINT ( 'NONE',  ( 76.15759952524373944, 64.74876932168429278, -14.35981515594801117 ) ) ;
#63783 = LINE ( 'NONE', #50571, #85650 ) ;
#63784 = CARTESIAN_POINT ( 'NONE',  ( 207.2384045602068454, 270.5804084916183001, -2.409301690515441408 ) ) ;
#63785 = FACE_OUTER_BOUND ( 'NONE', #83905, .T. ) ;
#63786 = EDGE_LOOP ( 'NONE', ( #93201, #12206 ) ) ;
#63787 = CARTESIAN_POINT ( 'NONE',  ( 190.8806404710506399, 295.7339764775937851, 11.26209325552490448 ) ) ;
#63788 = CARTESIAN_POINT ( 'NONE',  ( 160.4728670955267944, 275.6021364759136532, 12.83076506165803465 ) ) ;
#63789 = DIRECTION ( 'NONE',  ( 0.4999999999999998890, -0.8660254037844385966, 0.000000000000000000 ) ) ;
#63790 = CARTESIAN_POINT ( 'NONE',  ( 147.9515918652886342, 275.3690718889737923, -4.989113661445183645 ) ) ;
#63791 = DIRECTION ( 'NONE',  ( -0.000000000000000000, -0.000000000000000000, 1.000000000000000000 ) ) ;
#63792 =( BOUNDED_CURVE ( )  B_SPLINE_CURVE ( 2, ( #46174, #77094, #23382, #7696, #39568, #38588, #47189, #54272, #78110 ),
 .UNSPECIFIED., .F., .T. ) 
 B_SPLINE_CURVE_WITH_KNOTS ( ( 3, 2, 2, 2, 3 ),
 ( 0.5282258064516128782, 0.5295698924731182533, 0.5322580645161290036, 0.5349462365591397539, 0.5362903225806451291 ),
 .UNSPECIFIED. ) 
 CURVE ( )  GEOMETRIC_REPRESENTATION_ITEM ( )  RATIONAL_B_SPLINE_CURVE ( ( 0.9330127018922194093, 0.9330127018922194093, 1.000000000000000000, 0.8660254037844387076, 1.000000000000000000, 0.8660254037844387076, 1.000000000000000000, 0.9330127018922194093, 0.9330127018922194093 ) ) 
 REPRESENTATION_ITEM ( '' )  );
#63793 = EDGE_CURVE ( 'NONE', #59464, #57165, #10045, .T. ) ;
#63794 = CARTESIAN_POINT ( 'NONE',  ( -22.42236680055709641, 157.8615022471902591, 0.000000000000000000 ) ) ;
#63795 = AXIS2_PLACEMENT_3D ( 'NONE', #20223, #3050, #49609 ) ;
#63796 = DIRECTION ( 'NONE',  ( -0.000000000000000000, 1.000000000000000000, -0.000000000000000000 ) ) ;
#63797 = ORIENTED_EDGE ( 'NONE', *, *, #42285, .F. ) ;
#63798 = ADVANCED_FACE ( 'NONE', ( #25752 ), #18142, .F. ) ;
#63799 = CARTESIAN_POINT ( 'NONE',  ( 203.6072550072871081, 277.2840265471566568, -14.24554571798122460 ) ) ;
#63800 = CARTESIAN_POINT ( 'NONE',  ( 200.4403816905005158, 283.4740703539914648, 16.81798557643505987 ) ) ;
#63801 = CARTESIAN_POINT ( 'NONE',  ( 83.61997526984366402, 42.04153653030706295, 3.612101932814229865 ) ) ;
#63802 = CARTESIAN_POINT ( 'NONE',  ( 188.2118626355560025, 265.7141890007951019, -13.18290805338666694 ) ) ;
#63803 = FACE_OUTER_BOUND ( 'NONE', #21030, .T. ) ;
#63804 = CARTESIAN_POINT ( 'NONE',  ( 109.6465072765697641, 244.1115022471903160, -5.000000000000047962 ) ) ;
#63805 = CYLINDRICAL_SURFACE ( 'NONE', #49474, 17.82106496071139645 ) ;
#63806 = ADVANCED_FACE ( 'NONE', ( #52512 ), #28730, .T. ) ;
#63807 = ORIENTED_EDGE ( 'NONE', *, *, #50652, .T. ) ;
#63808 = VECTOR ( 'NONE', #59115, 1000.000000000000114 ) ;
#63809 = DIRECTION ( 'NONE',  ( 0.000000000000000000, 0.000000000000000000, 1.000000000000000000 ) ) ;
#63810 = CARTESIAN_POINT ( 'NONE',  ( 207.0200405408487541, 272.0777669287182334, 6.494273599193515878 ) ) ;
#63811 = CARTESIAN_POINT ( 'NONE',  ( 185.6955650132851758, 265.8818490688272504, 13.06349922320766410 ) ) ;
#63812 = CARTESIAN_POINT ( 'NONE',  ( 199.3598424642473219, 281.4464541862251394, -16.65811581254586926 ) ) ;
#63813 = CARTESIAN_POINT ( 'NONE',  ( 34.62385580964452458, 25.15404122711136026, 8.090169943749479842 ) ) ;
#63814 = DIRECTION ( 'NONE',  ( 0.4999999999999992784, -0.8660254037844390407, 0.000000000000000000 ) ) ;
#63815 = CARTESIAN_POINT ( 'NONE',  ( 182.4040233711584449, 274.1968787646982264, 16.41695686085575190 ) ) ;
#63816 = CARTESIAN_POINT ( 'NONE',  ( 85.48133813011057214, 42.12748250430919938, 0.7844986839966693326 ) ) ;
#63817 = CARTESIAN_POINT ( 'NONE',  ( 191.4759666451473947, 261.1522761069668945, 3.097452836964068812 ) ) ;
#63818 = CARTESIAN_POINT ( 'NONE',  ( 207.7320178805681508, 270.8445860024863237, -5.379955943374661764 ) ) ;
#63819 = CARTESIAN_POINT ( 'NONE',  ( 1.258015332399702757, 171.5333772461660828, 9.188101187500095079 ) ) ;
#63820 = CARTESIAN_POINT ( 'NONE',  ( 85.93470712620026575, 48.23248545518190866, 11.93606436224419909 ) ) ;
#63821 = EDGE_LOOP ( 'NONE', ( #64166, #19143, #84997, #27659 ) ) ;
#63822 = CARTESIAN_POINT ( 'NONE',  ( 161.0189972650558445, 253.0741054593400179, -14.82454529635133333 ) ) ;
#63823 = CARTESIAN_POINT ( 'NONE',  ( -34.16292631813981728, 25.86630820016799248, -10.00000000000000000 ) ) ;
#63824 = CARTESIAN_POINT ( 'NONE',  ( 82.05688055765639888, 41.79543639811913636, 5.447568203553421640 ) ) ;
#63825 = CARTESIAN_POINT ( 'NONE',  ( 25.45277359850996390, 179.3768266524159856, -9.188101187500093303 ) ) ;
#63826 = CARTESIAN_POINT ( 'NONE',  ( 149.8083888948594335, 271.5779462620446338, 11.70101749353969645 ) ) ;
#63827 = CARTESIAN_POINT ( 'NONE',  ( 34.73240388683179702, 38.79103043416552765, 8.090169943749478065 ) ) ;
#63828 = CARTESIAN_POINT ( 'NONE',  ( 179.1815112968807568, 292.0126970491061229, 6.085306834880822358 ) ) ;
#63829 = CARTESIAN_POINT ( 'NONE',  ( 191.4852287632733123, 298.9848502134979071, -9.870565261052552941 ) ) ;
#63830 = CARTESIAN_POINT ( 'NONE',  ( 196.5969449268226299, 290.1310981043597508, 16.37092889558107345 ) ) ;
#63831 = CARTESIAN_POINT ( 'NONE',  ( -6.662747857324052170, 100.5650415295849029, 1.836970198720989751E-15 ) ) ;
#63832 = DIRECTION ( 'NONE',  ( -0.3103181967972223343, 0.9506327454577401248, 0.000000000000000000 ) ) ;
#63833 = CARTESIAN_POINT ( 'NONE',  ( 87.02632046633624441, 46.40069582530824022, -8.775412300074195926 ) ) ;
#63834 = FACE_OUTER_BOUND ( 'NONE', #78101, .T. ) ;
#63835 = CARTESIAN_POINT ( 'NONE',  ( 193.0625067496444558, 295.7221012308248760, -12.50071909232508460 ) ) ;
#63836 = CARTESIAN_POINT ( 'NONE',  ( 81.06766895168330223, 227.6115022471903160, -5.000000000000047962 ) ) ;
#63837 = CARTESIAN_POINT ( 'NONE',  ( 70.65091078760467269, 66.69545628194936171, -10.73269157464200063 ) ) ;
#63838 = CARTESIAN_POINT ( 'NONE',  ( 156.6812872898450735, 261.2670451491295012, 0.000000000000000000 ) ) ;
#63839 = DIRECTION ( 'NONE',  ( -0.000000000000000000, -0.000000000000000000, -1.000000000000000000 ) ) ;
#63840 = CARTESIAN_POINT ( 'NONE',  ( 52.54321753458319932, 191.9548013555410080, -4.594050593750042211 ) ) ;
#63841 = DIRECTION ( 'NONE',  ( 1.000000000000000000, 0.000000000000000000, 0.000000000000000000 ) ) ;
#63842 = LINE ( 'NONE', #77562, #15757 ) ;
#63843 = CARTESIAN_POINT ( 'NONE',  ( 190.2510882691990730, 301.1224442529128851, -5.480893437181090455 ) ) ;
#63844 = CARTESIAN_POINT ( 'NONE',  ( -14.83894680564148238, 24.48641780169619508, -10.00000000000000000 ) ) ;
#63845 = ORIENTED_EDGE ( 'NONE', *, *, #42069, .F. ) ;
#63846 = FACE_OUTER_BOUND ( 'NONE', #71133, .T. ) ;
#63847 = CARTESIAN_POINT ( 'NONE',  ( -16.85990996717081813, 172.6199935810941213, 2.679491924311252049 ) ) ;
#63848 = CARTESIAN_POINT ( 'NONE',  ( 193.2843052833196111, 295.8687582740735138, 14.08193878756009632 ) ) ;
#63849 = CARTESIAN_POINT ( 'NONE',  ( 204.7200661083698776, 274.0614395018808978, 12.25436898028725530 ) ) ;
#63850 = CARTESIAN_POINT ( 'NONE',  ( 21.59633513308047270, 30.65586893147756697, -7.433330006724137462 ) ) ;
#63851 = CARTESIAN_POINT ( 'NONE',  ( 162.8042930031641049, 248.6616881586264469, 11.14389129512055554 ) ) ;
#63852 = CARTESIAN_POINT ( 'NONE',  ( 149.3629284598386278, 271.9428144707212027, -12.99253781774931049 ) ) ;
#63853 = EDGE_CURVE ( 'NONE', #2203, #90942, #68329, .T. ) ;
#63854 = CARTESIAN_POINT ( 'NONE',  ( 188.8413990936387279, 270.2136967773887477, -14.28180970089109714 ) ) ;
#63855 = ORIENTED_EDGE ( 'NONE', *, *, #49809, .F. ) ;
#63856 = CARTESIAN_POINT ( 'NONE',  ( 8.534987971495436199, 16.87878583063839599, -9.188101187500006262 ) ) ;
#63857 = PLANE ( 'NONE',  #77162 ) ;
#63858 = CARTESIAN_POINT ( 'NONE',  ( 70.80322137413752159, 60.50400129575321273, -14.70302039727343413 ) ) ;
#63859 = CARTESIAN_POINT ( 'NONE',  ( 20.67738335769525904, 35.85097175740956743, 10.00000000000000000 ) ) ;
#63860 = ORIENTED_EDGE ( 'NONE', *, *, #79300, .T. ) ;
#63861 = CARTESIAN_POINT ( 'NONE',  ( 72.43677597718138372, 71.19342475292700101, -6.085942204204715544 ) ) ;
#63862 = CARTESIAN_POINT ( 'NONE',  ( 85.32021429529936540, 49.09450955528861726, 12.43078529658329501 ) ) ;
#63863 = FACE_OUTER_BOUND ( 'NONE', #10074, .T. ) ;
#63864 = CARTESIAN_POINT ( 'NONE',  ( 190.8187029736043883, 300.1393067457597681, 3.941064102378585954 ) ) ;
#63865 = AXIS2_PLACEMENT_3D ( 'NONE', #29151, #6831, #38718 ) ;
#63866 = EDGE_CURVE ( 'NONE', #90587, #86729, #4279, .T. ) ;
#63867 = VERTEX_POINT ( 'NONE', #75848 ) ;
#63868 = ORIENTED_EDGE ( 'NONE', *, *, #71457, .T. ) ;
#63870 = FACE_OUTER_BOUND ( 'NONE', #96575, .T. ) ;
#63869 = CARTESIAN_POINT ( 'NONE',  ( 187.7049306102153139, 273.0437162969578822, -15.74079531760049910 ) ) ;
#63871 = EDGE_LOOP ( 'NONE', ( #87500, #6461, #71637, #87166 ) ) ;
#63872 = CARTESIAN_POINT ( 'NONE',  ( 35.07028576228009342, 43.18080186712595747, 3.090169943749475401 ) ) ;
#63873 = CARTESIAN_POINT ( 'NONE',  ( 71.98986200492696241, 72.23686350399877654, -3.591898176886850980 ) ) ;
#63874 = CARTESIAN_POINT ( 'NONE',  ( 72.84182891927886772, 57.62769808626433843, -16.30833842344255302 ) ) ;
#63875 = LINE ( 'NONE', #24871, #35409 ) ;
#63876 = ADVANCED_FACE ( 'NONE', ( #27242 ), #5925, .T. ) ;
#63877 = CARTESIAN_POINT ( 'NONE',  ( 204.6235849755581455, 276.2285497258825444, -13.59355699282649432 ) ) ;
#63879 = CARTESIAN_POINT ( 'NONE',  ( 92.97525793012167128, 233.6744531367911293, 4.594050593750047540 ) ) ;
#63878 = AXIS2_PLACEMENT_3D ( 'NONE', #10769, #16355, #94393 ) ;
#63880 = CARTESIAN_POINT ( 'NONE',  ( 180.3582177101254729, 287.0947775038071654, -13.76116533618757742 ) ) ;
#63881 = VERTEX_POINT ( 'NONE', #36816 ) ;
#63882 = CARTESIAN_POINT ( 'NONE',  ( 160.6949176047705805, 266.4836554915148099, 16.57512223367676185 ) ) ;
#63883 = ORIENTED_EDGE ( 'NONE', *, *, #65844, .F. ) ;
#63884 = CARTESIAN_POINT ( 'NONE',  ( 27.58754685475307156, 27.87878583063842797, -9.188101187500006262 ) ) ;
#63885 = CARTESIAN_POINT ( 'NONE',  ( 43.53831125515428369, 65.97156238185917232, 10.00000000000000000 ) ) ;
#63886 = CARTESIAN_POINT ( 'NONE',  ( 68.84404707066741480, 70.34727783162064441, -3.881443619315931404 ) ) ;
#63887 = CARTESIAN_POINT ( 'NONE',  ( 65.85835811776894388, 199.6423013555410080, -4.594050593750043987 ) ) ;
#63888 = CARTESIAN_POINT ( 'NONE',  ( 73.89028189157257032, 68.56231543382321547, 11.39439152759357832 ) ) ;
#63889 = CARTESIAN_POINT ( 'NONE',  ( 191.5544531425776427, 298.8649500714207647, 8.366689293739112188 ) ) ;
#63890 = CARTESIAN_POINT ( 'NONE',  ( 198.0355408163131585, 287.6393769322024241, 18.20720360189982756 ) ) ;
#63891 = PLANE ( 'NONE',  #56025 ) ;
#63892 = EDGE_LOOP ( 'NONE', ( #27111, #30759, #29662, #76099 ) ) ;
#63893 = CARTESIAN_POINT ( 'NONE',  ( 77.90651215622740722, 57.43855308693908768, -16.18645963951878031 ) ) ;
#63894 = CARTESIAN_POINT ( 'NONE',  ( 177.8972298254044802, 288.9764328270704823, 11.11871301495054531 ) ) ;
#63895 = CARTESIAN_POINT ( 'NONE',  ( 77.80402915230507688, 52.55141458490561490, 16.18111265596900594 ) ) ;
#63896 = ORIENTED_EDGE ( 'NONE', *, *, #15269, .F. ) ;
#63897 = CARTESIAN_POINT ( 'NONE',  ( 175.4772207271338686, 261.2202791896218628, -14.50271330228049926 ) ) ;
#63898 = CARTESIAN_POINT ( 'NONE',  ( 66.68553331399648698, 68.87473950154989666, -2.393764034506348004 ) ) ;
#63899 = CARTESIAN_POINT ( 'NONE',  ( 161.2488013048736377, 251.3558788108169040, -13.10044423494716170 ) ) ;
#63900 = CARTESIAN_POINT ( 'NONE',  ( 193.2053309019613891, 296.0055459150826778, -12.79465285318189061 ) ) ;
#63901 = LINE ( 'NONE', #3142, #17039 ) ;
#63902 = CARTESIAN_POINT ( 'NONE',  ( 180.9036116742409206, 271.3736204808990919, 16.91026336658080709 ) ) ;
#63903 = VECTOR ( 'NONE', #78200, 1000.000000000000114 ) ;
#63904 = CARTESIAN_POINT ( 'NONE',  ( 83.45583532732622700, 42.49119406076365379, -6.508603157797417715 ) ) ;
#63905 = CARTESIAN_POINT ( 'NONE',  ( 67.68597986140046885, 66.81033470680795006, 8.568866250934442874 ) ) ;
#63906 = CARTESIAN_POINT ( 'NONE',  ( 69.41227148360343335, 65.59617998781489234, -11.06349461743358376 ) ) ;
#63907 = DIRECTION ( 'NONE',  ( -0.5000000000000014433, 0.8660254037844379305, 0.000000000000000000 ) ) ;
#63908 = CARTESIAN_POINT ( 'NONE',  ( 106.6423081075360813, 238.5024278399160949, -9.188101187500093303 ) ) ;
#63909 = ORIENTED_EDGE ( 'NONE', *, *, #59052, .F. ) ;
#63910 = CARTESIAN_POINT ( 'NONE',  ( 191.7741832257749195, 298.4843664033717801, -8.615487418695501276 ) ) ;
#63911 = CARTESIAN_POINT ( 'NONE',  ( 83.80819523040570118, 41.96166617173753366, 2.742002955682231846 ) ) ;
#63912 = CARTESIAN_POINT ( 'NONE',  ( 203.0498946958275326, 278.9542612457532869, -15.11479947333269003 ) ) ;
#63913 = CARTESIAN_POINT ( 'NONE',  ( 164.2059258710715994, 246.2339888178522926, 7.329631442356459914 ) ) ;
#63914 = CARTESIAN_POINT ( 'NONE',  ( 83.77593207218663451, 52.15966500954240104, -15.02877900679588130 ) ) ;
#63915 = CARTESIAN_POINT ( 'NONE',  ( 175.9918762399839238, 254.0358301690074825, 4.937466140392421821 ) ) ;
#63916 = ORIENTED_EDGE ( 'NONE', *, *, #5956, .T. ) ;
#63917 = CARTESIAN_POINT ( 'NONE',  ( 80.41821068662579819, 57.11076416847725312, -16.23042426913554692 ) ) ;
#63918 = CARTESIAN_POINT ( 'NONE',  ( 158.0762504856774342, 274.7363926669914349, -12.55549483934156640 ) ) ;
#63919 = CARTESIAN_POINT ( 'NONE',  ( 185.4471331129824705, 262.0162576244363208, 9.741638050158547557 ) ) ;
#63920 = CARTESIAN_POINT ( 'NONE',  ( 206.0061733044583434, 273.8338364942757153, -9.988470584493322590 ) ) ;
#63921 = CARTESIAN_POINT ( 'NONE',  ( 139.9303331133829715, 251.5958772461660544, -9.188101187500095079 ) ) ;
#63922 = CARTESIAN_POINT ( 'NONE',  ( 189.9884557574413293, 294.6014195808287468, -12.37837975822646186 ) ) ;
#63923 = EDGE_CURVE ( 'NONE', #64236, #23117, #11496, .T. ) ;
#63924 = CARTESIAN_POINT ( 'NONE',  ( 185.8673354792971111, 296.7643724201381588, 4.550508980395866487 ) ) ;
#63925 = CARTESIAN_POINT ( 'NONE',  ( -40.08433460452723551, 25.84155934987275671, -10.00000000000000000 ) ) ;
#63926 = EDGE_CURVE ( 'NONE', #70875, #17814, #46523, .T. ) ;
#63927 = CARTESIAN_POINT ( 'NONE',  ( 53.67935523340274528, 210.9869531367911009, 4.594050593750046652 ) ) ;
#63928 = CARTESIAN_POINT ( 'NONE',  ( 85.42558612123971784, 48.32295466858820987, -12.24938428992806116 ) ) ;
#63929 = CARTESIAN_POINT ( 'NONE',  ( 157.7733463334721478, 257.3755434007023268, -16.94489513499352995 ) ) ;
#63930 = CARTESIAN_POINT ( 'NONE',  ( 88.07866424057203858, 44.70482641456190009, -4.324981154599603528 ) ) ;
#63931 = CARTESIAN_POINT ( 'NONE',  ( 69.58738856513491555, 70.56840624901691683, -2.716338601311397483 ) ) ;
#63932 = CARTESIAN_POINT ( 'NONE',  ( 174.4487186589523731, 262.1766023258701352, 14.34670417327684255 ) ) ;
#63933 = CARTESIAN_POINT ( 'NONE',  ( 191.2278159864466431, 297.4307022214792937, -10.96893880474589267 ) ) ;
#63934 = CARTESIAN_POINT ( 'NONE',  ( 178.4999909733569154, 292.3696688670564185, -7.228411343512463283 ) ) ;
#63935 = VECTOR ( 'NONE', #34388, 1000.000000000000000 ) ;
#63936 = CARTESIAN_POINT ( 'NONE',  ( 203.3740894404336927, 278.3927394765486838, -15.19753795879846869 ) ) ;
#63937 = CARTESIAN_POINT ( 'NONE',  ( 178.4492094125899087, 261.1672851353984584, 12.23577833629752831 ) ) ;
#63938 = CARTESIAN_POINT ( 'NONE',  ( 123.3405339703633672, 232.0177522451417929, 5.000000000000051514 ) ) ;
#63939 = B_SPLINE_SURFACE_WITH_KNOTS ( 'NONE', 3, 1, ( 
 ( #96009, #43236 ),
 ( #66552, #36138 ),
 ( #74178, #57445 ),
 ( #28046, #82308 ),
 ( #18985, #12879 ),
 ( #4250, #27069 ),
 ( #43737, #74682 ),
 ( #57952, #19496 ),
 ( #50350, #81305 ),
 ( #11876, #42731 ),
 ( #73669, #22440 ),
 ( #67540, #91888 ),
 ( #83279, #59930 ),
 ( #13847, #61920 ),
 ( #30544, #31031 ),
 ( #23422, #53816 ),
 ( #69032, #21450 ),
 ( #29547, #38114 ),
 ( #7741, #77660 ),
 ( #21940, #38627 ),
 ( #53334, #68536 ),
 ( #68042, #84288 ),
 ( #44724, #76172 ),
 ( #76645, #75657 ),
 ( #14834, #14347 ),
 ( #8248, #60421 ),
 ( #45722, #98964 ),
 ( #84779, #52338 ),
 ( #99459, #91377 ),
 ( #54313, #69537 ),
 ( #6749, #98470 ),
 ( #7230, #6242 ),
 ( #90900, #37137 ),
 ( #92869, #145 ) ),
 .UNSPECIFIED., .T., .F., .F.,
 ( 4, 2, 2, 2, 2, 2, 2, 2, 2, 2, 2, 2, 2, 2, 2, 2, 4 ),
 ( 2, 2 ),
 ( 0.000000000000000000, 0.06250000000000000000, 0.1250000000000000000, 0.1875000000000000000, 0.2500000000000000000, 0.3125000000000000000, 0.3750000000000000000, 0.4375000000000000000, 0.5000000000000000000, 0.5625000000000000000, 0.6250000000000000000, 0.6875000000000000000, 0.7500000000000000000, 0.8125000000000000000, 0.8750000000000000000, 0.9375000000000000000, 1.000000000000000000 ),
 ( 0.000000000000000000, 1.000000000000000000 ),
 .UNSPECIFIED. ) ;
#63940 = CARTESIAN_POINT ( 'NONE',  ( 80.15537031803718548, 52.05204710506983190, -15.26801063640590783 ) ) ;
#63941 = ORIENTED_EDGE ( 'NONE', *, *, #55435, .F. ) ;
#63942 = CARTESIAN_POINT ( 'NONE',  ( 148.2980785574368952, 273.7871886041155562, 9.134436720559454770 ) ) ;
#63943 = LINE ( 'NONE', #86306, #80698 ) ;
#63944 = CARTESIAN_POINT ( 'NONE',  ( 30.18841615574984516, 197.4244531367911293, -4.594050593750046652 ) ) ;
#63945 = CARTESIAN_POINT ( 'NONE',  ( 17.05992553822454383, 21.80066082961421259, 10.00000000000000533 ) ) ;
#63946 = CARTESIAN_POINT ( 'NONE',  ( 85.94199290331987129, 48.36193870280315110, 12.04004775853120357 ) ) ;
#63947 = CARTESIAN_POINT ( 'NONE',  ( 85.02181358025761426, 48.43635879085736207, -12.52173728460538982 ) ) ;
#63948 = CARTESIAN_POINT ( 'NONE',  ( 147.5848197185516142, 275.0225891520124151, 4.420251097676741736 ) ) ;
#63949 = CARTESIAN_POINT ( 'NONE',  ( 71.76351473723394747, 71.84897031608997509, 2.971691788643012977 ) ) ;
#63951 = CARTESIAN_POINT ( 'NONE',  ( 58.82164138842261991, 214.7677522451419350, -5.000000000000047962 ) ) ;
#63950 = DIRECTION ( 'NONE',  ( -0.9599109957006575211, -0.2803049773603249473, 0.000000000000000000 ) ) ;
#63952 = CARTESIAN_POINT ( 'NONE',  ( 174.1683193666472960, 289.3678892813664447, 7.962606529223953622 ) ) ;
#63953 = LINE ( 'NONE', #48260, #37529 ) ;
#63954 = DIRECTION ( 'NONE',  ( 0.000000000000000000, 0.000000000000000000, 1.000000000000000000 ) ) ;
#63955 = ORIENTED_EDGE ( 'NONE', *, *, #53150, .F. ) ;
#63956 = CARTESIAN_POINT ( 'NONE',  ( 29.10614472461697133, 197.6115022471903160, -5.000000000000047962 ) ) ;
#63957 = DIRECTION ( 'NONE',  ( 0.9634819383873026721, -0.2491829092639719911, 0.09803281150813247802 ) ) ;
#63958 = CARTESIAN_POINT ( 'NONE',  ( 202.2712651538608668, 280.3028871727136675, 16.13191389836473988 ) ) ;
#63959 = CARTESIAN_POINT ( 'NONE',  ( -6.860972828079417773, 166.8458772461660544, 9.188101187500095079 ) ) ;
#63960 = CARTESIAN_POINT ( 'NONE',  ( 35.00289615805098009, 41.18502408145595695, 5.678558825948277544 ) ) ;
#63962 = CARTESIAN_POINT ( 'NONE',  ( 170.7811188501789559, 263.0771675258006894, 15.96733366579245583 ) ) ;
#63961 = CARTESIAN_POINT ( 'NONE',  ( 164.3425516374517201, 252.4759456939266613, 13.51613706407178306 ) ) ;
#63963 = CARTESIAN_POINT ( 'NONE',  ( 192.7944000592152634, 296.7172990131160759, 11.44860011299869740 ) ) ;
#63964 = CARTESIAN_POINT ( 'NONE',  ( 32.94607225727562394, 21.94754757982091675, 5.678558825948272215 ) ) ;
#63965 = FACE_OUTER_BOUND ( 'NONE', #41843, .T. ) ;
#63966 = CARTESIAN_POINT ( 'NONE',  ( 183.3546644584063472, 257.9009421642305142, -2.296804517617567321 ) ) ;
#63967 = CARTESIAN_POINT ( 'NONE',  ( 65.96121609362643312, 68.98813676735653644, 2.519541258661097682 ) ) ;
#63968 = ORIENTED_EDGE ( 'NONE', *, *, #99216, .T. ) ;
#63969 = PLANE ( 'NONE',  #52584 ) ;
#63970 = DIRECTION ( 'NONE',  ( 0.000000000000000000, 0.000000000000000000, 1.000000000000000000 ) ) ;
#63971 = CARTESIAN_POINT ( 'NONE',  ( 8.697374518098678564, 25.99752408145590366, 5.678558825948277544 ) ) ;
#63972 = CARTESIAN_POINT ( 'NONE',  ( 168.1557382078134424, 288.1736776346151601, 0.5343211543652907070 ) ) ;
#63973 = CARTESIAN_POINT ( 'NONE',  ( 17.84595736030643920, 25.70171378149918695, -9.188101187500004485 ) ) ;
#63974 = LINE ( 'NONE', #9286, #26337 ) ;
#63976 = EDGE_CURVE ( 'NONE', #48299, #93959, #510, .T. ) ;
#63975 = VECTOR ( 'NONE', #20833, 1000.000000000000000 ) ;
#63977 = CARTESIAN_POINT ( 'NONE',  ( 84.70579481679399692, 49.94286076369812832, -13.65556694543043825 ) ) ;
#63978 = CARTESIAN_POINT ( 'NONE',  ( 88.09947609552301628, 44.13539611768646864, -1.715919295570225822 ) ) ;
#63979 = EDGE_CURVE ( 'NONE', #64017, #45286, #88871, .T. ) ;
#63980 = ORIENTED_EDGE ( 'NONE', *, *, #51690, .F. ) ;
#63981 = DIRECTION ( 'NONE',  ( 0.000000000000000000, 0.000000000000000000, -1.000000000000000000 ) ) ;
#63982 = CARTESIAN_POINT ( 'NONE',  ( 207.6860335175200589, 270.9242332556395922, 6.913225035677485586 ) ) ;
#63983 = AXIS2_PLACEMENT_3D ( 'NONE', #89050, #96616, #65658 ) ;
#63984 = CARTESIAN_POINT ( 'NONE',  ( 66.04918351466359638, 68.55101183580894997, 4.476786609762311464 ) ) ;
#63985 = CARTESIAN_POINT ( 'NONE',  ( -33.92913075610074003, 36.15268528101246659, 59.99999999999999289 ) ) ;
#63986 = CARTESIAN_POINT ( 'NONE',  ( 194.2321518193436987, 294.2270399159019121, 13.98132384850917020 ) ) ;
#63987 = ORIENTED_EDGE ( 'NONE', *, *, #60365, .F. ) ;
#63988 = EDGE_LOOP ( 'NONE', ( #69454, #50038, #58272, #20769 ) ) ;
#63989 = CARTESIAN_POINT ( 'NONE',  ( 158.0371712374162882, 277.6164995809708103, -9.872139935335178862 ) ) ;
#63990 = CARTESIAN_POINT ( 'NONE',  ( 86.19418860658703352, 47.68766159785528913, 10.81734670790828368 ) ) ;
#63991 = VERTEX_POINT ( 'NONE', #809 ) ;
#63992 = CARTESIAN_POINT ( 'NONE',  ( 77.78144776439313546, 57.65517096718075862, 16.17772494993696242 ) ) ;
#63993 = CARTESIAN_POINT ( 'NONE',  ( 188.8073495538124575, 297.5103159715075662, 7.738326755456107264 ) ) ;
#63995 = ADVANCED_FACE ( 'NONE', ( #15002 ), #45890, .T. ) ;
#63994 = ORIENTED_EDGE ( 'NONE', *, *, #58563, .T. ) ;
#63996 = CARTESIAN_POINT ( 'NONE',  ( 78.39750752953510471, 61.37713215747155004, -15.85865527802526564 ) ) ;
#63997 = LINE ( 'NONE', #86361, #28159 ) ;
#63998 = CARTESIAN_POINT ( 'NONE',  ( 84.40523410500765067, 47.35716185244744025, -11.94365264890164546 ) ) ;
#63999 = CARTESIAN_POINT ( 'NONE',  ( 173.0837253472800796, 264.8280141993791972, 17.07053884509587860 ) ) ;
#64000 = VERTEX_POINT ( 'NONE', #61603 ) ;
#64001 = CARTESIAN_POINT ( 'NONE',  ( 200.7583183585857967, 282.9233878912788214, 16.96937806979494212 ) ) ;
#64002 = CARTESIAN_POINT ( 'NONE',  ( 168.4098293865724827, 275.5469783040978200, -15.30805618485334385 ) ) ;
#64003 = VECTOR ( 'NONE', #39, 1000.000000000000000 ) ;
#64004 = LINE ( 'NONE', #41187, #81271 ) ;
#64005 = CARTESIAN_POINT ( 'NONE',  ( 150.8987980144153767, 274.7068622528165633, -8.647764889241976505 ) ) ;
#64006 = EDGE_LOOP ( 'NONE', ( #2349, #50840 ) ) ;
#64007 = CARTESIAN_POINT ( 'NONE',  ( 200.5039526449628795, 267.3497397166782434, 6.370409075474873006 ) ) ;
#64008 = FACE_OUTER_BOUND ( 'NONE', #7161, .T. ) ;
#64009 = EDGE_CURVE ( 'NONE', #3513, #59744, #6620, .T. ) ;
#64010 = ORIENTED_EDGE ( 'NONE', *, *, #48738, .T. ) ;
#64011 = EDGE_CURVE ( 'NONE', #24668, #73177, #30839, .T. ) ;
#64012 = ORIENTED_EDGE ( 'NONE', *, *, #61176, .F. ) ;
#64013 = CARTESIAN_POINT ( 'NONE',  ( 156.9907511051827385, 266.1419335827932287, -16.70578678711312293 ) ) ;
#64014 = VECTOR ( 'NONE', #20058, 1000.000000000000000 ) ;
#64015 = ORIENTED_EDGE ( 'NONE', *, *, #7091, .T. ) ;
#64016 = DIRECTION ( 'NONE',  ( -0.8660254037844387076, -0.4999999999999998890, -0.000000000000000000 ) ) ;
#64017 = VERTEX_POINT ( 'NONE', #32207 ) ;
#64018 = CARTESIAN_POINT ( 'NONE',  ( 168.0637158183493227, 272.4661608228503837, 15.99915743202654284 ) ) ;
#64019 = CARTESIAN_POINT ( 'NONE',  ( 193.3392202435183549, 295.7736427729139450, 14.53615558183985534 ) ) ;
#64020 = DIRECTION ( 'NONE',  ( -0.8263106059122556912, -0.5632146860273805622, 0.000000000000000000 ) ) ;
#64021 = CARTESIAN_POINT ( 'NONE',  ( 71.37153584347667845, 69.28727247378522236, 8.201935042734072923 ) ) ;
#64022 = DIRECTION ( 'NONE',  ( -0.4145187862775162602, 0.7179675985244458047, -0.5591929034707565638 ) ) ;
#64023 = CARTESIAN_POINT ( 'NONE',  ( 175.0213034474378446, 290.8364490856844213, 6.509122669734152211 ) ) ;
#64024 = DIRECTION ( 'NONE',  ( -0.8660254037844377084, -0.5000000000000014433, -0.000000000000000000 ) ) ;
#64025 = VERTEX_POINT ( 'NONE', #94056 ) ;
#64026 = CARTESIAN_POINT ( 'NONE',  ( 45.11483101423404918, 69.99284853207299761, 10.00000000000000000 ) ) ;
#64027 = CARTESIAN_POINT ( 'NONE',  ( 20.93478768117288524, 17.80170272979926338, 7.433330006724137462 ) ) ;
#64028 = CARTESIAN_POINT ( 'NONE',  ( 206.4768661561222984, 273.0185725604343361, 11.39716120335626925 ) ) ;
#64029 = CARTESIAN_POINT ( 'NONE',  ( 206.4537138826727301, 273.0586734743599209, 11.45643784582899016 ) ) ;
#64031 = EDGE_LOOP ( 'NONE', ( #98829, #69609, #36950, #86948 ) ) ;
#64030 = CARTESIAN_POINT ( 'NONE',  ( 198.0792648159935538, 287.5636447432459022, 17.04758482866669667 ) ) ;
#64032 = ORIENTED_EDGE ( 'NONE', *, *, #39960, .F. ) ;
#64033 = EDGE_CURVE ( 'NONE', #46582, #28117, #3058, .T. ) ;
#64034 = CARTESIAN_POINT ( 'NONE',  ( 169.2275080599221440, 257.9151911612065078, -14.10194183318204963 ) ) ;
#64035 = CARTESIAN_POINT ( 'NONE',  ( 206.2041691044954348, 273.4908977089264113, -9.455375957961031474 ) ) ;
#64036 = DIRECTION ( 'NONE',  ( 0.4999999999999998890, -0.8660254037844385966, 0.000000000000000000 ) ) ;
#64037 = B_SPLINE_CURVE_WITH_KNOTS ( 'NONE', 3,
 ( #13089, #83502, #44450, #5472, #13579, #75383, #6471, #68252, #99177, #17556, #56030, #94591 ),
 .UNSPECIFIED., .F., .F.,
 ( 4, 2, 2, 2, 2, 4 ),
 ( 0.000000000000000000, 0.2315728839045457232, 0.3473593258568164477, 0.4631457678090872276, 0.6947186517136287875, 0.9262915356181703475 ),
 .UNSPECIFIED. ) ;
#64038 = CARTESIAN_POINT ( 'NONE',  ( 161.3644539559160478, 251.1555625431813894, 12.97746593258196413 ) ) ;
#64039 = CARTESIAN_POINT ( 'NONE',  ( 171.3171204526115616, 271.4791138034659070, -17.75561031716327420 ) ) ;
#64040 = ORIENTED_EDGE ( 'NONE', *, *, #23855, .F. ) ;
#64042 = EDGE_CURVE ( 'NONE', #14427, #50922, #58976, .T. ) ;
#64041 = DIRECTION ( 'NONE',  ( -0.8492021815265757834, 0.5280678506503729830, 0.000000000000000000 ) ) ;
#64043 = PLANE ( 'NONE',  #52823 ) ;
#64044 = CARTESIAN_POINT ( 'NONE',  ( -1.501377777706596639, 158.3932355074535678, -2.679491924311248496 ) ) ;
#64045 = CARTESIAN_POINT ( 'NONE',  ( 15.08735849730845402, 189.5177522451419065, 5.000000000000046185 ) ) ;
#64046 = CARTESIAN_POINT ( 'NONE',  ( 94.46399941469991290, 225.3458772461660544, 9.188101187500095079 ) ) ;
#64047 = CARTESIAN_POINT ( 'NONE',  ( 196.3535209228541021, 269.2310135407589655, -12.05999164192846074 ) ) ;
#64048 = EDGE_CURVE ( 'NONE', #51005, #93753, #44094, .T. ) ;
#64049 = CARTESIAN_POINT ( 'NONE',  ( 175.7882114856885210, 291.4026636951798537, -6.622811550496607857 ) ) ;
#64050 = CARTESIAN_POINT ( 'NONE',  ( 207.8040920112677270, 270.7197499462034784, 3.100718407159808176 ) ) ;
#64051 = CARTESIAN_POINT ( 'NONE',  ( 14.68175618682350780, 167.0327760586659451, 1.948934522072303157E-15 ) ) ;
#64053 = EDGE_CURVE ( 'NONE', #4321, #37845, #43293, .T. ) ;
#64052 = AXIS2_PLACEMENT_3D ( 'NONE', #97796, #21283, #99286 ) ;
#64054 = DIRECTION ( 'NONE',  ( -0.000000000000000000, -0.000000000000000000, 1.000000000000000000 ) ) ;
#64055 = ORIENTED_EDGE ( 'NONE', *, *, #36522, .T. ) ;
#64056 = ORIENTED_EDGE ( 'NONE', *, *, #62187, .T. ) ;
#64057 = EDGE_CURVE ( 'NONE', #47928, #75148, #96018, .T. ) ;
#64058 = CARTESIAN_POINT ( 'NONE',  ( 197.5569596757523811, 265.3403027263088916, -2.927114525079438589 ) ) ;
#64059 = ADVANCED_FACE ( 'NONE', ( #51402 ), #88990, .T. ) ;
#64060 = CARTESIAN_POINT ( 'NONE',  ( 67.24282661209741718, 68.88379657313680582, 3.801344451262675950 ) ) ;
#64061 = VECTOR ( 'NONE', #97084, 1000.000000000000000 ) ;
#64062 = CARTESIAN_POINT ( 'NONE',  ( 71.71174882302004505, 58.93038559421764688, -15.88944412480316970 ) ) ;
#64063 = CARTESIAN_POINT ( 'NONE',  ( 193.0560632045236673, 263.9002708199371909, -4.325864479350134850 ) ) ;
#64064 = CARTESIAN_POINT ( 'NONE',  ( 161.4816992964961742, 250.9524876563463067, -12.92750327687364198 ) ) ;
#64065 = CARTESIAN_POINT ( 'NONE',  ( 184.2146915786734098, 285.2824563773917816, 15.08884348642498452 ) ) ;
#64066 = CARTESIAN_POINT ( 'NONE',  ( 74.15402199957247831, 68.42859570829774896, -11.65141325894000879 ) ) ;
#64067 = CARTESIAN_POINT ( 'NONE',  ( 31.67681054456310719, 201.3464784336661637, 1.353441290958777525E-15 ) ) ;
#64068 = CARTESIAN_POINT ( 'NONE',  ( 85.30758498749676733, 213.3927522451418213, 10.00000000000009592 ) ) ;
#64069 = CARTESIAN_POINT ( 'NONE',  ( 199.5024589829807837, 277.4988332975255503, 15.16960785487432162 ) ) ;
#64070 = ORIENTED_EDGE ( 'NONE', *, *, #34381, .T. ) ;
#64071 = CARTESIAN_POINT ( 'NONE',  ( 83.09507021368182222, 45.14153989563129699, 9.863572327592716960 ) ) ;
#64072 = CARTESIAN_POINT ( 'NONE',  ( 174.9671601572613326, 281.6994072225486434, -15.63500919100072473 ) ) ;
#64073 = CARTESIAN_POINT ( 'NONE',  ( -7.320788502016136512, 157.3923013555410080, 4.594050593750050204 ) ) ;
#64074 = CARTESIAN_POINT ( 'NONE',  ( 68.73183574854552091, 64.12522977685954118, -11.96507596856094402 ) ) ;
#64075 = FACE_OUTER_BOUND ( 'NONE', #96717, .T. ) ;
#64076 = AXIS2_PLACEMENT_3D ( 'NONE', #59038, #19099, #90007 ) ;
#64077 = CARTESIAN_POINT ( 'NONE',  ( -19.65312891409030271, 93.06504152958497400, 10.00000000000000000 ) ) ;
#64078 = CARTESIAN_POINT ( 'NONE',  ( 148.0826818691893152, 274.1602666119424043, -9.371267383421741926 ) ) ;
#64079 = CARTESIAN_POINT ( 'NONE',  ( 43.63646518856938172, 66.22046553916848666, 10.00000000000000000 ) ) ;
#64080 = CARTESIAN_POINT ( 'NONE',  ( 204.2133777088835700, 276.9390495533970693, 13.75768580338462144 ) ) ;
#64081 = CARTESIAN_POINT ( 'NONE',  ( 191.3413020738616410, 299.2341385521244774, -8.295023558158421295 ) ) ;
#64082 = CARTESIAN_POINT ( 'NONE',  ( 164.2672861321391053, 246.1277097281173667, -2.417001679502223777 ) ) ;
#64083 = EDGE_LOOP ( 'NONE', ( #25906, #63916, #9822, #82766 ) ) ;
#64084 =( BOUNDED_CURVE ( )  B_SPLINE_CURVE ( 2, ( #59065, #36286, #28189, #67691, #51995, #21117, #99602, #60563, #97623 ),
 .UNSPECIFIED., .F., .T. ) 
 B_SPLINE_CURVE_WITH_KNOTS ( ( 3, 2, 2, 2, 3 ),
 ( 0.3750000000000000000, 0.3763440860215053752, 0.3790322580645161255, 0.3817204301075268758, 0.3830645161290322509 ),
 .UNSPECIFIED. ) 
 CURVE ( )  GEOMETRIC_REPRESENTATION_ITEM ( )  RATIONAL_B_SPLINE_CURVE ( ( 0.9330127018922194093, 0.9330127018922194093, 1.000000000000000000, 0.8660254037844387076, 1.000000000000000000, 0.8660254037844387076, 1.000000000000000000, 0.9330127018922194093, 0.9330127018922194093 ) ) 
 REPRESENTATION_ITEM ( '' )  );
#64085 = CARTESIAN_POINT ( 'NONE',  ( 181.1902717559939617, 268.1300628243799338, 16.16177986835113600 ) ) ;
#64086 = CARTESIAN_POINT ( 'NONE',  ( 116.7102005222951817, 232.0643266524159856, -9.188101187500093303 ) ) ;
#64087 = CARTESIAN_POINT ( 'NONE',  ( 21.36958804686389612, 14.19860640527291906, 2.839279412974134775 ) ) ;
#64088 = CARTESIAN_POINT ( 'NONE',  ( 79.43862237908915347, 58.57025095756571176, -16.60657855749719758 ) ) ;
#64089 = CARTESIAN_POINT ( 'NONE',  ( 150.9690640482209574, 269.7773037333962520, 13.74186519101368020 ) ) ;
#64091 = CARTESIAN_POINT ( 'NONE',  ( -32.30932376655839988, 25.48519649537502119, -10.00000000000000000 ) ) ;
#64090 = CARTESIAN_POINT ( 'NONE',  ( 195.9359860111818250, 291.2759125279654882, 17.49638312768267312 ) ) ;
#64092 = CARTESIAN_POINT ( 'NONE',  ( 150.9724169730098424, 269.1550985917100434, -14.05609013274548857 ) ) ;
#64093 = ORIENTED_EDGE ( 'NONE', *, *, #99265, .T. ) ;
#64094 = CARTESIAN_POINT ( 'NONE',  ( 190.0093170351423169, 261.0487610539813659, -4.602376092151496678 ) ) ;
#64095 = CARTESIAN_POINT ( 'NONE',  ( 149.1429535397850827, 272.3238222086447990, -12.91457852089092384 ) ) ;
#64096 = CARTESIAN_POINT ( 'NONE',  ( 190.0435459140688295, 300.0465545779896388, 4.679742701079471878 ) ) ;
#64097 = CARTESIAN_POINT ( 'NONE',  ( 174.3263853019044802, 290.4440848627237983, -1.067528433193902115 ) ) ;
#64098 = CARTESIAN_POINT ( 'NONE',  ( 194.5504213170283094, 270.8435279203088157, -14.24376176104693137 ) ) ;
#64099 = ORIENTED_EDGE ( 'NONE', *, *, #61818, .T. ) ;
#64100 = LINE ( 'NONE', #40775, #44098 ) ;
#64101 = CARTESIAN_POINT ( 'NONE',  ( 175.6701573864172587, 278.5910633658755842, 15.45497855305149137 ) ) ;
#64102 = CARTESIAN_POINT ( 'NONE',  ( 165.5507010442709657, 269.3226483685077710, -16.52342293238164217 ) ) ;
#64103 = CARTESIAN_POINT ( 'NONE',  ( 200.2567476884168514, 272.3152526771139037, 12.76741103404060951 ) ) ;
#64104 = CARTESIAN_POINT ( 'NONE',  ( 155.9844261609601688, 261.1831564919472157, 17.17349893481298650 ) ) ;
#64105 = DIRECTION ( 'NONE',  ( 0.000000000000000000, -0.000000000000000000, 1.000000000000000000 ) ) ;
#64106 = CARTESIAN_POINT ( 'NONE',  ( 148.2541920228352126, 274.5676210274151003, 6.886971996321211265 ) ) ;
#64107 = ORIENTED_EDGE ( 'NONE', *, *, #5651, .T. ) ;
#64108 = CARTESIAN_POINT ( 'NONE',  ( 164.9054020227948740, 260.6345827824168282, 17.20773913071212391 ) ) ;
#64109 = CARTESIAN_POINT ( 'NONE',  ( 35.31444455405989657, 43.49540643055190969, 3.479690158560446702E-15 ) ) ;
#64110 = CARTESIAN_POINT ( 'NONE',  ( 192.6861190271732767, 288.4908837155273886, -15.91154857267342315 ) ) ;
#64111 = ORIENTED_EDGE ( 'NONE', *, *, #90976, .F. ) ;
#64112 = CARTESIAN_POINT ( 'NONE',  ( 167.8373819884664897, 280.7956131110225897, 12.19395811520589490 ) ) ;
#64113 = CARTESIAN_POINT ( 'NONE',  ( 148.0637215040603394, 274.1931069276759558, -7.795633835291665648 ) ) ;
#64114 = CARTESIAN_POINT ( 'NONE',  ( 165.5752708168755305, 245.8622137986321832, -1.085626278946311585 ) ) ;
#64116 = ADVANCED_FACE ( 'NONE', ( #81360 ), #35207, .T. ) ;
#64115 = ORIENTED_EDGE ( 'NONE', *, *, #28716, .F. ) ;
#64117 = CARTESIAN_POINT ( 'NONE',  ( 78.80495087215344086, 60.04985905707439997, 16.11149256888698389 ) ) ;
#64118 = DIRECTION ( 'NONE',  ( 0.4999999999999998890, -0.8660254037844385966, 0.000000000000000000 ) ) ;
#64119 = B_SPLINE_CURVE_WITH_KNOTS ( 'NONE', 3,
 ( #97337, #73525, #34512, #27905 ),
 .UNSPECIFIED., .F., .F.,
 ( 4, 4 ),
 ( 0.000000000000000000, 0.0009678251226235170916 ),
 .UNSPECIFIED. ) ;
#64120 = CARTESIAN_POINT ( 'NONE',  ( 88.43398120015881148, 44.08421024288151102, -2.684292198961160114 ) ) ;
#64121 = AXIS2_PLACEMENT_3D ( 'NONE', #46460, #68771, #100202 ) ;
#64122 = CARTESIAN_POINT ( 'NONE',  ( 81.74119788692269140, 59.14441083166271795, -0.5000000000000000000 ) ) ;
#64123 = CIRCLE ( 'NONE', #93291, 17.82106496071138935 ) ;
#64124 = CARTESIAN_POINT ( 'NONE',  ( 24.59328401069779702, 196.5530062829863311, -4.648177544792955347E-16 ) ) ;
#64125 = ORIENTED_EDGE ( 'NONE', *, *, #49809, .T. ) ;
#64126 = EDGE_CURVE ( 'NONE', #49525, #3243, #12934, .T. ) ;
#64127 = ORIENTED_EDGE ( 'NONE', *, *, #63866, .F. ) ;
#64129 = VECTOR ( 'NONE', #8460, 1000.000000000000114 ) ;
#64128 = CARTESIAN_POINT ( 'NONE',  ( 175.4420607406781585, 259.0809407130348632, 12.51945158449231776 ) ) ;
#64130 = ADVANCED_FACE ( 'NONE', ( #43794 ), #11930, .F. ) ;
#64131 = EDGE_LOOP ( 'NONE', ( #74395, #42740, #71614, #47932 ) ) ;
#64132 = CARTESIAN_POINT ( 'NONE',  ( 77.22537433491581282, 49.19994283889470665, -15.34347781851081116 ) ) ;
#64133 = ORIENTED_EDGE ( 'NONE', *, *, #92162, .T. ) ;
#64134 = CARTESIAN_POINT ( 'NONE',  ( 88.37406050535491886, 44.20074384979837845, 0.1102876639795926650 ) ) ;
#64135 = CARTESIAN_POINT ( 'NONE',  ( 78.07934852507207779, 48.52740830546968454, 14.36491527075813579 ) ) ;
#64136 = ORIENTED_EDGE ( 'NONE', *, *, #91820, .F. ) ;
#64137 = CARTESIAN_POINT ( 'NONE',  ( 164.9590787296926067, 244.9294898008548387, -2.278052160087662870 ) ) ;
#64138 = CARTESIAN_POINT ( 'NONE',  ( 147.2164090273763009, 275.6606951871798969, -7.081586236283015090 ) ) ;
#64139 = CARTESIAN_POINT ( 'NONE',  ( 161.2311971278517433, 276.6540853535840370, -12.65640296859774239 ) ) ;
#64140 = CARTESIAN_POINT ( 'NONE',  ( 193.1169444172380167, 296.1586357973259283, -13.13373377033755318 ) ) ;
#64141 = CARTESIAN_POINT ( 'NONE',  ( 201.0844796915553161, 282.3584598911111812, -16.59562674965125950 ) ) ;
#64142 = CARTESIAN_POINT ( 'NONE',  ( 23.64814127513160358, 118.0650415295850166, -40.00000000000000711 ) ) ;
#64143 = CARTESIAN_POINT ( 'NONE',  ( 183.4841190084916605, 284.4425740377230909, -16.26519031814292759 ) ) ;
#64144 = CARTESIAN_POINT ( 'NONE',  ( 125.2893514524760548, 233.9548013555409796, -4.594050593750042211 ) ) ;
#64145 = CARTESIAN_POINT ( 'NONE',  ( 70.68908763585848476, 61.42051710150978749, -14.81853427669291534 ) ) ;
#64146 = CARTESIAN_POINT ( 'NONE',  ( 36.01387044229257128, 42.83396525600393545, -2.839279412974133887 ) ) ;
#64147 = VERTEX_POINT ( 'NONE', #73230 ) ;
#64149 = ORIENTED_EDGE ( 'NONE', *, *, #45398, .F. ) ;
#64148 = CARTESIAN_POINT ( 'NONE',  ( 87.88600403731702215, 43.93895673462996143, -3.527816320842273257 ) ) ;
#64150 = AXIS2_PLACEMENT_3D ( 'NONE', #13090, #82528, #33902 ) ;
#64151 = CARTESIAN_POINT ( 'NONE',  ( 200.7003661377988522, 274.4207182511248106, 13.44867137911134414 ) ) ;
#64152 = CARTESIAN_POINT ( 'NONE',  ( 177.5731418194271498, 253.4711720865799975, 1.377694960479720176 ) ) ;
#64153 = CARTESIAN_POINT ( 'NONE',  ( 171.3124147562957944, 287.8937356591647472, -4.632457808386030607 ) ) ;
#64154 = LINE ( 'NONE', #25669, #22385 ) ;
#64155 = CARTESIAN_POINT ( 'NONE',  ( 156.7733467512841798, 279.4475125893658856, 7.423369370622811658 ) ) ;
#64156 = CARTESIAN_POINT ( 'NONE',  ( 152.6740002182599767, 266.2078699576288159, -17.16212636348624088 ) ) ;
#64157 = CARTESIAN_POINT ( 'NONE',  ( 173.3566611292251594, 287.3586671341846568, -9.788589206785145436 ) ) ;
#64158 = VECTOR ( 'NONE', #70376, 1000.000000000000114 ) ;
#64159 = CARTESIAN_POINT ( 'NONE',  ( 171.5128195627625018, 280.0544377941017160, 13.82747465963291589 ) ) ;
#64160 = CARTESIAN_POINT ( 'NONE',  ( 177.0796805162949568, 255.9639923578327512, -7.284429273897122137 ) ) ;
#64161 = ORIENTED_EDGE ( 'NONE', *, *, #67390, .T. ) ;
#64163 = EDGE_CURVE ( 'NONE', #43672, #85978, #83997, .T. ) ;
#64162 = DIRECTION ( 'NONE',  ( -0.8660254037844387076, -0.4999999999999998890, -0.000000000000000000 ) ) ;
#64164 = B_SPLINE_CURVE_WITH_KNOTS ( 'NONE', 3,
 ( #4022, #74447, #97738, #3546 ),
 .UNSPECIFIED., .F., .F.,
 ( 4, 4 ),
 ( 0.01475334623982018159, 0.02347991049736522506 ),
 .UNSPECIFIED. ) ;
#64165 = CARTESIAN_POINT ( 'NONE',  ( 65.99146032466613576, 68.67736554541691874, -0.3373263738352356711 ) ) ;
#64166 = ORIENTED_EDGE ( 'NONE', *, *, #40273, .F. ) ;
#64167 = CARTESIAN_POINT ( 'NONE',  ( 164.0279908745103796, 278.0166827825981954, 13.19491288999882350 ) ) ;
#64168 = ADVANCED_FACE ( 'NONE', ( #34704, #42786 ), #73720, .T. ) ;
#64169 = CARTESIAN_POINT ( 'NONE',  ( 203.2959387668414308, 268.8872303932580508, -2.890917808293821611 ) ) ;
#64170 = CARTESIAN_POINT ( 'NONE',  ( 191.4144919117340180, 299.1073700343318365, -9.990130103278371365 ) ) ;
#64171 = DIRECTION ( 'NONE',  ( -0.3535533905932763954, 0.6123724356958081261, 0.7071067811865344721 ) ) ;
#64172 = CARTESIAN_POINT ( 'NONE',  ( 162.6476498368881494, 248.9330020812748785, 10.75824100428386743 ) ) ;
#64174 = CARTESIAN_POINT ( 'NONE',  ( 154.7022681145324441, 277.6819014155639138, -9.051459774888167331 ) ) ;
#64173 = CARTESIAN_POINT ( 'NONE',  ( 164.6230904413119447, 284.1771003334332590, -6.922202500276794623 ) ) ;
#64175 = CARTESIAN_POINT ( 'NONE',  ( 153.2283961777204695, 265.2476279883323400, -17.66880461074566000 ) ) ;
#64176 = ORIENTED_EDGE ( 'NONE', *, *, #71134, .F. ) ;
#64177 = CARTESIAN_POINT ( 'NONE',  ( 72.32238060516027645, 62.28520104033361804, -14.34112121930858308 ) ) ;
#64178 = ADVANCED_FACE ( 'NONE', ( #29117 ), #58494, .T. ) ;
#64179 = CARTESIAN_POINT ( 'NONE',  ( 193.4969218094394989, 276.1359876676401086, -16.38138015012474824 ) ) ;
#64180 = CARTESIAN_POINT ( 'NONE',  ( 75.70957059507740894, 64.79295583396756797, -14.21030040932456728 ) ) ;
#64181 = CARTESIAN_POINT ( 'NONE',  ( 85.60311072857605552, 48.35646458700439609, 11.69947488989744677 ) ) ;
#64182 = CARTESIAN_POINT ( 'NONE',  ( 64.47116044126103418, 196.4824982072973683, 3.021315404115420679E-15 ) ) ;
#64183 = CARTESIAN_POINT ( 'NONE',  ( 41.49446470602975978, 58.46153712902343358, -10.00000000000000000 ) ) ;
#64184 = CARTESIAN_POINT ( 'NONE',  ( 168.2008345946905479, 248.1884056956802453, -5.064766917302788052 ) ) ;
#64185 = CARTESIAN_POINT ( 'NONE',  ( -7.673045192009834814, 172.5024278399160664, -9.188101187500093303 ) ) ;
#64186 = CARTESIAN_POINT ( 'NONE',  ( 96.27750042569734035, 217.2048013555409796, 4.594050593750051981 ) ) ;
#64187 = CARTESIAN_POINT ( 'NONE',  ( 88.03836335721405248, 44.60032456687661551, -4.083393883595300977 ) ) ;
#64188 = LINE ( 'NONE', #48497, #91654 ) ;
#64189 = CARTESIAN_POINT ( 'NONE',  ( -12.80041588338334790, 174.9637435831424739, 2.679491924311258266 ) ) ;
#64190 = VECTOR ( 'NONE', #51294, 999.9999999999998863 ) ;
#64191 = CARTESIAN_POINT ( 'NONE',  ( 78.32387762194203162, 56.55609178520109737, 16.20249635714992564 ) ) ;
#64192 = CARTESIAN_POINT ( 'NONE',  ( 160.9048106541811762, 281.6641488084669618, 5.546786390428459335 ) ) ;
#64194 = CARTESIAN_POINT ( 'NONE',  ( 162.7459776558209228, 248.7626933030860812, -9.895605163646791880 ) ) ;
#64193 = CARTESIAN_POINT ( 'NONE',  ( 67.53167658295855347, 67.09922345392760690, 8.942594108559751120 ) ) ;
#64195 = CARTESIAN_POINT ( 'NONE',  ( 161.6965001858482083, 250.5804416024775492, 12.67320179257150414 ) ) ;
#64196 = LINE ( 'NONE', #35289, #3869 ) ;
#64197 = CARTESIAN_POINT ( 'NONE',  ( 80.48174699225948814, 54.15325549600505184, -15.80187059250945047 ) ) ;
#64198 = VECTOR ( 'NONE', #26539, 1000.000000000000000 ) ;
#64199 = CARTESIAN_POINT ( 'NONE',  ( 147.7256246083515521, 244.5494855054051868, -2.679491924311248496 ) ) ;
#64200 = CARTESIAN_POINT ( 'NONE',  ( 86.10144160763246646, 220.5177522451418497, -10.00000000000009592 ) ) ;
#64201 = CARTESIAN_POINT ( 'NONE',  ( 73.59537120146498523, 69.79291368717997557, 9.952181187355030545 ) ) ;
#64202 = CARTESIAN_POINT ( 'NONE',  ( 40.22915850269944116, 194.0333772461660544, 9.188101187500095079 ) ) ;
#64203 = CARTESIAN_POINT ( 'NONE',  ( 76.71798530001490235, 63.32448642232582614, -15.43374014074777989 ) ) ;
#64204 = EDGE_CURVE ( 'NONE', #9798, #26753, #59466, .T. ) ;
#64205 = CARTESIAN_POINT ( 'NONE',  ( 65.93911412966747321, 215.0024278399160949, 9.188101187500095079 ) ) ;
#64206 = CARTESIAN_POINT ( 'NONE',  ( 161.8926315922002743, 250.2407320417157166, -13.77020595223768495 ) ) ;
#64207 = CARTESIAN_POINT ( 'NONE',  ( 107.3857722915638249, 221.2592609112380160, 2.679491924311254714 ) ) ;
#64209 = PLANE ( 'NONE',  #48980 ) ;
#64208 = CARTESIAN_POINT ( 'NONE',  ( 87.76955579613945702, 43.67712966683451725, -2.576982100675560439 ) ) ;
#64210 = CARTESIAN_POINT ( 'NONE',  ( 162.8931802014337791, 249.0911889412991229, -10.32038157250286048 ) ) ;
#64211 = CARTESIAN_POINT ( 'NONE',  ( 32.08968265630384309, 27.03085787977765264, 9.188101187500006262 ) ) ;
#64212 = CARTESIAN_POINT ( 'NONE',  ( 82.63458119455265205, 48.44224962061904449, -13.47290339139292925 ) ) ;
#64213 = CARTESIAN_POINT ( 'NONE',  ( 148.9285945872975390, 272.6951028054104427, -12.01265727652413240 ) ) ;
#64214 = EDGE_LOOP ( 'NONE', ( #23965, #18933, #88131, #60249 ) ) ;
#64215 = CARTESIAN_POINT ( 'NONE',  ( 19.96532700332172183, 20.03085787977762422, 9.188101187500006262 ) ) ;
#64216 = CARTESIAN_POINT ( 'NONE',  ( 75.92590343676303632, 205.4548013555409796, -4.594050593750042211 ) ) ;
#64217 = CARTESIAN_POINT ( 'NONE',  ( 76.69221233506321767, 63.60975152925200859, 15.32791472565302016 ) ) ;
#64218 = VECTOR ( 'NONE', #49324, 1000.000000000000000 ) ;
#64219 = CARTESIAN_POINT ( 'NONE',  ( -22.42236680055709641, 157.8615022471902591, 0.000000000000000000 ) ) ;
#64220 = FACE_OUTER_BOUND ( 'NONE', #62229, .T. ) ;
#64221 = DIRECTION ( 'NONE',  ( -0.000000000000000000, 0.000000000000000000, -1.000000000000000000 ) ) ;
#64222 = AXIS2_PLACEMENT_3D ( 'NONE', #27636, #36200, #58501 ) ;
#64223 = CARTESIAN_POINT ( 'NONE',  ( 31.47957939141361905, 85.21460096010893892, 59.99999999999999289 ) ) ;
#64224 = CARTESIAN_POINT ( 'NONE',  ( 87.60591442325252842, 44.91970625728536959, -6.572271063428638982 ) ) ;
#64225 = CARTESIAN_POINT ( 'NONE',  ( 133.0291931787496935, 237.6115022471901739, -5.000000000000041744 ) ) ;
#64226 = CARTESIAN_POINT ( 'NONE',  ( 200.8432122835317841, 282.7763473000181307, 17.15137370990203891 ) ) ;
#64227 = CARTESIAN_POINT ( 'NONE',  ( 75.37954934236186944, 53.16236703070756420, 16.48630273753103026 ) ) ;
#64228 = ORIENTED_EDGE ( 'NONE', *, *, #93462, .F. ) ;
#64229 = CARTESIAN_POINT ( 'NONE',  ( 82.29734961797254300, 53.60383310410944802, 15.81226994477781567 ) ) ;
#64230 = ORIENTED_EDGE ( 'NONE', *, *, #899, .F. ) ;
#64231 = CARTESIAN_POINT ( 'NONE',  ( 202.9972156839127990, 279.0455039708822937, 16.77197898838388213 ) ) ;
#64232 = CARTESIAN_POINT ( 'NONE',  ( 176.1478293119272109, 282.8961218008153651, 15.39372813948029339 ) ) ;
#64233 = CARTESIAN_POINT ( 'NONE',  ( 25.96864935082050252, 154.0458036431183189, -30.52142883766499892 ) ) ;
#64234 = ORIENTED_EDGE ( 'NONE', *, *, #1488, .T. ) ;
#64235 = CARTESIAN_POINT ( 'NONE',  ( 173.9559965888401507, 252.0681728601754799, -0.2505477230817378387 ) ) ;
#64237 = EDGE_CURVE ( 'NONE', #7544, #79399, #29577, .T. ) ;
#64236 = VERTEX_POINT ( 'NONE', #4826 ) ;
#64238 = DIRECTION ( 'NONE',  ( -0.8660254037844377084, -0.5000000000000014433, -0.000000000000000000 ) ) ;
#64239 = CARTESIAN_POINT ( 'NONE',  ( 194.3442947553755005, 294.0328026529847421, -15.97648891113594871 ) ) ;
#64240 = B_SPLINE_CURVE_WITH_KNOTS ( 'NONE', 3,
 ( #11983, #2902, #42839, #82425 ),
 .UNSPECIFIED., .F., .F.,
 ( 4, 4 ),
 ( 0.01015053972906150397, 0.01849756262824885783 ),
 .UNSPECIFIED. ) ;
#64241 = CARTESIAN_POINT ( 'NONE',  ( -14.83262083840142154, 124.7156766241961208, -37.49999999999995737 ) ) ;
#64242 = ORIENTED_EDGE ( 'NONE', *, *, #22731, .T. ) ;
#64243 = CARTESIAN_POINT ( 'NONE',  ( 35.22902474502244274, 28.84335787977765619, 9.188101187500006262 ) ) ;
#64244 = CARTESIAN_POINT ( 'NONE',  ( 79.88938969212057373, 44.69895041751207998, 11.22585976794914586 ) ) ;
#64245 = CARTESIAN_POINT ( 'NONE',  ( 84.81344185393595581, 50.36986395726449928, -13.44794441900970483 ) ) ;
#64246 = CARTESIAN_POINT ( 'NONE',  ( 80.78636346040434546, 48.92950834313149500, -13.82546426373123438 ) ) ;
#64248 = ADVANCED_FACE ( 'NONE', ( #97556 ), #96077, .T. ) ;
#64247 = FACE_OUTER_BOUND ( 'NONE', #94427, .T. ) ;
#64249 = DIRECTION ( 'NONE',  ( -0.8660254037844387076, -0.4999999999999998890, -0.000000000000000000 ) ) ;
#64250 = ADVANCED_FACE ( 'NONE', ( #80379 ), #33751, .T. ) ;
#64251 = ORIENTED_EDGE ( 'NONE', *, *, #26253, .T. ) ;
#64252 = ORIENTED_EDGE ( 'NONE', *, *, #55148, .T. ) ;
#64253 = DIRECTION ( 'NONE',  ( -0.5435407515102095299, 0.8393827800519358950, 0.000000000000000000 ) ) ;
#64255 = CARTESIAN_POINT ( 'NONE',  ( 148.4083960970861256, 273.5961130204771052, -8.574185186226726429 ) ) ;
#64254 = CARTESIAN_POINT ( 'NONE',  ( 204.8523313866422484, 275.8323493198358847, 14.65426965484541100 ) ) ;
#64256 = DIRECTION ( 'NONE',  ( -0.8143688203140631021, 0.5803476755362091399, 0.000000000000000000 ) ) ;
#64257 = CARTESIAN_POINT ( 'NONE',  ( 155.6126298223767890, 261.1180141786725244, 18.15400560664037855 ) ) ;
#64258 = CARTESIAN_POINT ( 'NONE',  ( 185.3642616951140383, 292.5731700952273968, -11.69566502907712469 ) ) ;
#64259 = LINE ( 'NONE', #89129, #58118 ) ;
#64260 = CARTESIAN_POINT ( 'NONE',  ( 207.3688238152966790, 271.4736565765441583, -4.151733834809656187 ) ) ;
#64261 = CARTESIAN_POINT ( 'NONE',  ( 206.4466068143230757, 270.6103183474565981, 2.450360801254404475 ) ) ;
#64262 = CARTESIAN_POINT ( 'NONE',  ( 79.55938800887707885, 59.45545654668635649, 16.55147640184673108 ) ) ;
#64263 = CARTESIAN_POINT ( 'NONE',  ( 85.88519558028406209, 211.2048013555409796, 4.594050593750051981 ) ) ;
#64264 = ORIENTED_EDGE ( 'NONE', *, *, #50491, .F. ) ;
#64265 = CARTESIAN_POINT ( 'NONE',  ( 48.16808589598787904, 104.3116767361652535, -10.00000000000000000 ) ) ;
#64266 = LINE ( 'NONE', #93708, #35032 ) ;
#64267 = VECTOR ( 'NONE', #99450, 1000.000000000000000 ) ;
#64268 = ORIENTED_EDGE ( 'NONE', *, *, #56543, .T. ) ;
#64269 = CARTESIAN_POINT ( 'NONE',  ( 167.7949682406799639, 266.8640267017669885, -17.72765487805554585 ) ) ;
#64270 = ORIENTED_EDGE ( 'NONE', *, *, #39398, .F. ) ;
#64271 = ORIENTED_EDGE ( 'NONE', *, *, #68585, .F. ) ;
#64272 = B_SPLINE_CURVE_WITH_KNOTS ( 'NONE', 3,
 ( #35923, #6027, #12654, #28322, #73944, #44006, #83067, #75442, #36416, #97753 ),
 .UNSPECIFIED., .F., .F.,
 ( 4, 2, 2, 2, 4 ),
 ( 0.000000000000000000, 0.2500000000000000000, 0.5000000000000000000, 0.7500000000000000000, 1.000000000000000000 ),
 .UNSPECIFIED. ) ;
#64273 = CARTESIAN_POINT ( 'NONE',  ( 80.19651160619561381, 44.67774917954261582, -11.72988265430777055 ) ) ;
#64274 = CARTESIAN_POINT ( 'NONE',  ( 67.05615745758373691, 67.62596409448416068, 6.666417839661090916 ) ) ;
#64276 = B_SPLINE_SURFACE_WITH_KNOTS ( 'NONE', 3, 1, ( 
 ( #96907, #58830 ),
 ( #66456, #97381 ),
 ( #27948, #20370 ),
 ( #51241, #82208 ),
 ( #43644, #66941 ),
 ( #97871, #28443 ),
 ( #99855, #60324 ),
 ( #45137, #91779 ),
 ( #52728, #82706 ),
 ( #51764, #91280 ),
 ( #52242, #61328 ),
 ( #38019, #46117 ),
 ( #21357, #68434 ),
 ( #28960, #98373 ),
 ( #21846, #22344 ),
 ( #13273, #44626 ),
 ( #53723, #77033 ),
 ( #83690, #75069 ),
 ( #6654, #53240 ),
 ( #83186, #22838 ),
 ( #14743, #13746 ),
 ( #14251, #84195 ),
 ( #45624, #37041 ),
 ( #76553, #6147 ),
 ( #75560, #67951 ),
 ( #29447, #90304 ),
 ( #98869, #67443 ),
 ( #76078, #84682 ),
 ( #68930, #30440 ),
 ( #60817, #37528 ),
 ( #44135, #99363 ),
 ( #7132, #92289 ),
 ( #15222, #7639 ),
 ( #36538, #38531 ) ),
 .UNSPECIFIED., .T., .F., .F.,
 ( 4, 2, 2, 2, 2, 2, 2, 2, 2, 2, 2, 2, 2, 2, 2, 2, 4 ),
 ( 2, 2 ),
 ( 0.000000000000000000, 0.06250000000000000000, 0.1250000000000000000, 0.1875000000000000000, 0.2500000000000000000, 0.3125000000000000000, 0.3750000000000000000, 0.4375000000000000000, 0.5000000000000000000, 0.5625000000000000000, 0.6250000000000000000, 0.6875000000000000000, 0.7500000000000000000, 0.8125000000000000000, 0.8750000000000000000, 0.9375000000000000000, 1.000000000000000000 ),
 ( 0.000000000000000000, 1.000000000000000000 ),
 .UNSPECIFIED. ) ;
#64275 = CARTESIAN_POINT ( 'NONE',  ( 73.62250635243424313, 69.55784274833359859, 10.23584637956792776 ) ) ;
#64277 = CARTESIAN_POINT ( 'NONE',  ( 82.97933013574042604, 41.49896216930607551, -2.766843078683310253 ) ) ;
#64278 = CARTESIAN_POINT ( 'NONE',  ( 85.04283770205356063, 47.23198909375206966, -10.98040028159587322 ) ) ;
#64279 = CARTESIAN_POINT ( 'NONE',  ( 162.4419666585835387, 249.2892557963607203, 10.75794555938079711 ) ) ;
#64280 = CARTESIAN_POINT ( 'NONE',  ( 100.7430306879021202, 216.7202760586659736, -5.415160957724236172E-17 ) ) ;
#64281 = VERTEX_POINT ( 'NONE', #41312 ) ;
#64282 = CIRCLE ( 'NONE', #41627, 1.449999999999993072 ) ;
#64283 = ORIENTED_EDGE ( 'NONE', *, *, #56931, .T. ) ;
#64284 = ADVANCED_FACE ( 'NONE', ( #89011 ), #57519, .T. ) ;
#64285 = CARTESIAN_POINT ( 'NONE',  ( 200.8245636081238104, 282.8086477533188940, -18.30100074294778523 ) ) ;
#64286 = ORIENTED_EDGE ( 'NONE', *, *, #81189, .T. ) ;
#64287 = FACE_OUTER_BOUND ( 'NONE', #16401, .T. ) ;
#64288 = CARTESIAN_POINT ( 'NONE',  ( 68.01423091693212086, 69.07147863764068063, -4.702031134324633044 ) ) ;
#64289 = CARTESIAN_POINT ( 'NONE',  ( 87.55613534105700069, 44.89236293052572790, -6.575074172489557611 ) ) ;
#64290 = CARTESIAN_POINT ( 'NONE',  ( -12.62545442379354554, 163.5177522451418781, -10.00000000000009592 ) ) ;
#64291 = CARTESIAN_POINT ( 'NONE',  ( 88.14062891587492743, 44.42319542341160599, 4.630203861778126928 ) ) ;
#64292 = ORIENTED_EDGE ( 'NONE', *, *, #92872, .T. ) ;
#64293 = AXIS2_PLACEMENT_3D ( 'NONE', #44971, #37367, #59665 ) ;
#64294 = CARTESIAN_POINT ( 'NONE',  ( 86.45475614751083526, 43.94238033638490748, -4.660792038277363325 ) ) ;
#64295 = CARTESIAN_POINT ( 'NONE',  ( 160.7563763136490991, 275.4827502265731027, 13.67813126869715745 ) ) ;
#64296 = CARTESIAN_POINT ( 'NONE',  ( 206.5081929095101998, 272.9643130319303737, -9.215516226794479238 ) ) ;
#64297 = CARTESIAN_POINT ( 'NONE',  ( 80.47957521310596007, 43.62501291645610024, 9.811056319678726823 ) ) ;
#64298 = CARTESIAN_POINT ( 'NONE',  ( 71.47272524832681029, 59.15296923211511171, -15.79140392200444332 ) ) ;
#64299 = CARTESIAN_POINT ( 'NONE',  ( 74.24029763082349120, 55.47955095029949746, -16.12046342301015756 ) ) ;
#64300 = CARTESIAN_POINT ( 'NONE',  ( 198.2505066714982149, 285.2670451491296149, 0.000000000000000000 ) ) ;
#64301 = ORIENTED_EDGE ( 'NONE', *, *, #67909, .T. ) ;
#64302 = CARTESIAN_POINT ( 'NONE',  ( 149.0237174825091415, 274.5263358477994871, 9.114370506038131481 ) ) ;
#64303 = CARTESIAN_POINT ( 'NONE',  ( 200.5810378487751393, 283.2304467414622877, 18.38516374632547112 ) ) ;
#64304 = CARTESIAN_POINT ( 'NONE',  ( 86.25587912986354411, 45.60430133017160870, 8.273538712114721250 ) ) ;
#64305 = CARTESIAN_POINT ( 'NONE',  ( 21.09856983598611535, 20.38052372038640669, 10.00000000000000533 ) ) ;
#64306 = CARTESIAN_POINT ( 'NONE',  ( 78.44203751522358914, 61.21016990572090322, 16.24725970467587999 ) ) ;
#64307 = CARTESIAN_POINT ( 'NONE',  ( 202.4027882010644248, 280.0750825725909863, -15.81779609180605739 ) ) ;
#64308 = ORIENTED_EDGE ( 'NONE', *, *, #51867, .F. ) ;
#64309 = CARTESIAN_POINT ( 'NONE',  ( 35.77580382318486585, 22.78380873178790011, -6.180339887498949025 ) ) ;
#64310 = B_SPLINE_CURVE_WITH_KNOTS ( 'NONE', 3,
 ( #26197, #33813, #41377, #88056 ),
 .UNSPECIFIED., .F., .F.,
 ( 4, 4 ),
 ( 0.02623590123331938015, 0.03547298285468161727 ),
 .UNSPECIFIED. ) ;
#64311 = EDGE_CURVE ( 'NONE', #80395, #67223, #31891, .T. ) ;
#64312 = CARTESIAN_POINT ( 'NONE',  ( 165.0532575723395041, 244.7663672603923715, -2.144843157699870773 ) ) ;
#64313 = CARTESIAN_POINT ( 'NONE',  ( 32.61785165683026122, 46.50599740114041225, 10.00000000000000000 ) ) ;
#64314 = CARTESIAN_POINT ( 'NONE',  ( 79.51440259700740398, 53.51398053849010950, 16.18861449462646007 ) ) ;
#64315 = CARTESIAN_POINT ( 'NONE',  ( 26.66754231763712824, 34.13478043621389446, 8.090169943749478065 ) ) ;
#64316 = CARTESIAN_POINT ( 'NONE',  ( 169.6737827488630330, 273.3960839505391505, 15.97819652875916496 ) ) ;
#64317 = LINE ( 'NONE', #11140, #54578 ) ;
#64318 = CARTESIAN_POINT ( 'NONE',  ( 161.1037873772034743, 273.3404041746127291, -15.20289387583265928 ) ) ;
#64319 = CARTESIAN_POINT ( 'NONE',  ( 85.85358028005475717, 43.51426421455354898, -4.436799439580211057 ) ) ;
#64320 = LINE ( 'NONE', #10126, #49726 ) ;
#64321 = CARTESIAN_POINT ( 'NONE',  ( 3.585285057187872493, 179.0024278399160949, 9.188101187500095079 ) ) ;
#64322 = DIRECTION ( 'NONE',  ( -0.000000000000000000, 0.000000000000000000, -1.000000000000000000 ) ) ;
#64323 = ORIENTED_EDGE ( 'NONE', *, *, #67351, .T. ) ;
#64324 = CARTESIAN_POINT ( 'NONE',  ( 160.2808189788048026, 253.4324493631022222, -14.69790056671751977 ) ) ;
#64325 = CARTESIAN_POINT ( 'NONE',  ( 26.07871176553302917, 38.55466486950701466, 7.012934429366973338E-14 ) ) ;
#64326 = CARTESIAN_POINT ( 'NONE',  ( 71.95199650962558735, 72.63932214931871556, -0.9219114722910072279 ) ) ;
#64327 = CARTESIAN_POINT ( 'NONE',  ( 27.69859311986958872, 195.9869531367911293, 4.594050593750046652 ) ) ;
#64328 = VECTOR ( 'NONE', #42605, 1000.000000000000000 ) ;
#64329 = CARTESIAN_POINT ( 'NONE',  ( -22.42236680055709641, 157.8615022471902591, 0.000000000000000000 ) ) ;
#64330 = CARTESIAN_POINT ( 'NONE',  ( 32.84085557565775559, 19.36477965099641452, 1.583844403245330712 ) ) ;
#64331 = CARTESIAN_POINT ( 'NONE',  ( 33.33147356615550194, 41.01751292744059185, 6.180339887498949913 ) ) ;
#64332 = CARTESIAN_POINT ( 'NONE',  ( 178.5672342955430736, 291.6450058653585415, 6.041949026109024956 ) ) ;
#64333 = CARTESIAN_POINT ( 'NONE',  ( 98.80083580102481733, 239.3967562850347122, -4.648177544792955347E-16 ) ) ;
#64334 = CARTESIAN_POINT ( 'NONE',  ( 196.4226663688725978, 290.4329574213987257, 16.56158086743572611 ) ) ;
#64335 = CARTESIAN_POINT ( 'NONE',  ( 178.9629750711524423, 278.2817214550511835, -16.74959616653973171 ) ) ;
#64336 = CARTESIAN_POINT ( 'NONE',  ( 7.019590965729775256, 22.79103043416547081, 8.090169943749478065 ) ) ;
#64337 = CARTESIAN_POINT ( 'NONE',  ( 190.1149742248946382, 298.7024877295776264, -8.095583997651624841 ) ) ;
#64338 = VECTOR ( 'NONE', #93375, 1000.000000000000000 ) ;
#64339 = CARTESIAN_POINT ( 'NONE',  ( 82.29453827371133912, 204.9865022471901170, 1.119607411625061291E-15 ) ) ;
#64340 = DIRECTION ( 'NONE',  ( -0.2359789242578327062, -0.9717581732643756354, 0.000000000000000000 ) ) ;
#64341 = CARTESIAN_POINT ( 'NONE',  ( -17.42236680055705023, 149.2012482093457777, 0.000000000000000000 ) ) ;
#64342 = CARTESIAN_POINT ( 'NONE',  ( 48.99766571601688270, 199.0958772461660544, -9.188101187500095079 ) ) ;
#64343 = CARTESIAN_POINT ( 'NONE',  ( 159.3767386493506137, 254.5983864451355032, 15.47015898230477760 ) ) ;
#64344 = EDGE_LOOP ( 'NONE', ( #37111, #35866, #33998, #16389 ) ) ;
#64345 = CARTESIAN_POINT ( 'NONE',  ( -9.255205446392002600, 85.17849077645132638, 14.12110100382514410 ) ) ;
#64346 = CARTESIAN_POINT ( 'NONE',  ( 150.9584389135710865, 269.1793093008492406, -15.82751450793727699 ) ) ;
#64347 = CARTESIAN_POINT ( 'NONE',  ( -106.6146531411566798, 123.6868197944956620, 37.50000000000002132 ) ) ;
#64348 = ORIENTED_EDGE ( 'NONE', *, *, #303, .T. ) ;
#64349 = CARTESIAN_POINT ( 'NONE',  ( 169.0845258451994084, 285.4515155598613774, 7.530877004957813980 ) ) ;
#64350 = LINE ( 'NONE', #68579, #32856 ) ;
#64351 = CARTESIAN_POINT ( 'NONE',  ( 71.66369827319218189, 72.02185750324218816, -1.551229696566573502 ) ) ;
#64352 = CARTESIAN_POINT ( 'NONE',  ( 93.96783902534114929, 218.3927522451417929, -10.00000000000009237 ) ) ;
#64353 = CARTESIAN_POINT ( 'NONE',  ( 21.83270445532239989, 34.64646525600390703, -2.839279412974133887 ) ) ;
#64354 = CARTESIAN_POINT ( 'NONE',  ( 202.8167949821795446, 279.3580017930215149, 15.61966256214195070 ) ) ;
#64355 = CARTESIAN_POINT ( 'NONE',  ( 197.0184425104562820, 289.4010428742387262, -16.90752553128928426 ) ) ;
#64356 = CARTESIAN_POINT ( 'NONE',  ( 204.5840280042472159, 276.2970644099866036, 14.65559382949596667 ) ) ;
#64357 = ORIENTED_EDGE ( 'NONE', *, *, #92741, .F. ) ;
#64358 = CIRCLE ( 'NONE', #90293, 14.99999999999968381 ) ;
#64359 = CARTESIAN_POINT ( 'NONE',  ( 12.93244592517074487, 8.262165230724926701, -2.296566073217252530E-15 ) ) ;
#64360 = CARTESIAN_POINT ( 'NONE',  ( 171.7156989675575289, 252.4012571563561949, 8.733959727973424236 ) ) ;
#64361 = CARTESIAN_POINT ( 'NONE',  ( 87.90770736294503251, 44.20194146633631505, 2.808464138919696484 ) ) ;
#64362 = ORIENTED_EDGE ( 'NONE', *, *, #40001, .F. ) ;
#64364 = EDGE_CURVE ( 'NONE', #82741, #71517, #57018, .T. ) ;
#64363 = CARTESIAN_POINT ( 'NONE',  ( 178.8612031755637020, 282.6164454953549807, 15.88195292133873160 ) ) ;
#64365 = CARTESIAN_POINT ( 'NONE',  ( 191.2056514706806070, 299.4690922889112699, 7.290007621276087590 ) ) ;
#64366 = CARTESIAN_POINT ( 'NONE',  ( 7.819191540449072164, 28.68125778831126382, -10.00000000000000000 ) ) ;
#64367 = CARTESIAN_POINT ( 'NONE',  ( 170.0730192398974339, 270.7478067695028017, 17.76568905885011418 ) ) ;
#64368 = ADVANCED_FACE ( 'NONE', ( #11460, #34234 ), #10950, .F. ) ;
#64369 = ORIENTED_EDGE ( 'NONE', *, *, #20805, .F. ) ;
#64370 = ORIENTED_EDGE ( 'NONE', *, *, #72996, .T. ) ;
#64371 = VECTOR ( 'NONE', #76314, 1000.000000000000227 ) ;
#64373 = CARTESIAN_POINT ( 'NONE',  ( 151.3542526322075901, 269.2885850756041464, -14.28695254860580199 ) ) ;
#64372 = FACE_OUTER_BOUND ( 'NONE', #33860, .T. ) ;
#64374 = CARTESIAN_POINT ( 'NONE',  ( 196.5475899070771675, 290.2165835061676944, -17.89382743182097002 ) ) ;
#64375 = ORIENTED_EDGE ( 'NONE', *, *, #30343, .T. ) ;
#64376 = CARTESIAN_POINT ( 'NONE',  ( 152.7375212135632125, 266.0978483664162582, -16.47968945089317572 ) ) ;
#64377 = EDGE_CURVE ( 'NONE', #85106, #72480, #42316, .T. ) ;
#64378 = CARTESIAN_POINT ( 'NONE',  ( 72.03933155393818311, 72.41131128147422658, -2.965003495713515402 ) ) ;
#64379 = CARTESIAN_POINT ( 'NONE',  ( 73.09905864054320546, 57.42323756090770814, -15.88034204403881589 ) ) ;
#64380 = CARTESIAN_POINT ( 'NONE',  ( 78.16855185334185308, 61.58847221756811052, -16.14202726422458767 ) ) ;
#64382 = EDGE_CURVE ( 'NONE', #70225, #8907, #74258, .T. ) ;
#64381 = DIRECTION ( 'NONE',  ( -0.5000000000000013323, 0.8660254037844378194, 0.000000000000000000 ) ) ;
#64383 = CARTESIAN_POINT ( 'NONE',  ( 119.3082767336485404, 233.5643266524159856, -9.188101187500093303 ) ) ;
#64384 = CARTESIAN_POINT ( 'NONE',  ( 183.9133946104620918, 288.6285713628617486, -13.17071474273308951 ) ) ;
#64385 = VERTEX_POINT ( 'NONE', #27144 ) ;
#64386 = CARTESIAN_POINT ( 'NONE',  ( 201.4968513823492060, 281.2160229052847171, 16.24425496473199004 ) ) ;
#64387 = VERTEX_POINT ( 'NONE', #72256 ) ;
#64388 = CARTESIAN_POINT ( 'NONE',  ( 30.11829213135327521, 40.49540643055189548, 3.479690158560446702E-15 ) ) ;
#64389 = CARTESIAN_POINT ( 'NONE',  ( 168.9579038699606315, 279.3139280689009070, 15.08363371378442608 ) ) ;
#64390 = CARTESIAN_POINT ( 'NONE',  ( 65.82437655349816907, 69.12761348810170148, -0.3171013769033947383 ) ) ;
#64391 = CARTESIAN_POINT ( 'NONE',  ( 67.34675250658217749, 203.5643266524159856, -9.188101187500093303 ) ) ;
#64392 = CARTESIAN_POINT ( 'NONE',  ( 74.40608543823466903, 68.34271654374390437, 11.35151599582641424 ) ) ;
#64393 =( BOUNDED_CURVE ( )  B_SPLINE_CURVE ( 2, ( #31037, #61925, #92876, #50233, #11267, #25440, #41123, #86805, #64446, #94877, #42619, #88807, #11755 ),
 .UNSPECIFIED., .F., .T. ) 
 B_SPLINE_CURVE_WITH_KNOTS ( ( 3, 2, 2, 2, 2, 2, 3 ),
 ( 0.3624999999999999889, 0.3649999999999999911, 0.3699999999999999956, 0.3750000000000000000, 0.3800000000000000044, 0.3850000000000000089, 0.3875000000000000111 ),
 .UNSPECIFIED. ) 
 CURVE ( )  GEOMETRIC_REPRESENTATION_ITEM ( )  RATIONAL_B_SPLINE_CURVE ( ( 0.9755282581475768211, 0.9755282581475768211, 1.000000000000000000, 0.9510565162951535312, 1.000000000000000000, 0.9510565162951535312, 1.000000000000000000, 0.9510565162951535312, 1.000000000000000000, 0.9510565162951535312, 1.000000000000000000, 0.9755282581475768211, 0.9755282581475768211 ) ) 
 REPRESENTATION_ITEM ( '' )  );
#64394 = CARTESIAN_POINT ( 'NONE',  ( 191.2645787786270262, 299.3670271975948367, 7.309947121636420242 ) ) ;
#64395 = CARTESIAN_POINT ( 'NONE',  ( 198.5386315514599858, 286.7679982181109608, 17.03868888912368718 ) ) ;
#64396 = CARTESIAN_POINT ( 'NONE',  ( 173.2942936627640620, 271.3368914396714331, 16.42383385673190332 ) ) ;
#64397 = ORIENTED_EDGE ( 'NONE', *, *, #63348, .T. ) ;
#64398 = CARTESIAN_POINT ( 'NONE',  ( 76.72068702196582990, 57.86501502775809058, -16.11583960702630591 ) ) ;
#64399 = CARTESIAN_POINT ( 'NONE',  ( 85.95981172767709211, 43.29180227630435951, -3.360722111609490526 ) ) ;
#64400 = CARTESIAN_POINT ( 'NONE',  ( 44.08135397534552169, 118.8355609772188188, -10.00000000000000000 ) ) ;
#64401 = DIRECTION ( 'NONE',  ( -0.000000000000000000, -0.000000000000000000, -1.000000000000000000 ) ) ;
#64402 = VECTOR ( 'NONE', #63466, 1000.000000000000114 ) ;
#64403 = ORIENTED_EDGE ( 'NONE', *, *, #42003, .F. ) ;
#64404 = CARTESIAN_POINT ( 'NONE',  ( 173.7340210619385914, 260.6390436719518675, -13.93636029417189093 ) ) ;
#64405 = CARTESIAN_POINT ( 'NONE',  ( 174.2364561098118259, 277.1437767697490813, -15.63526590635042446 ) ) ;
#64406 = CARTESIAN_POINT ( 'NONE',  ( 160.5819451565263023, 258.3323579126541745, -16.82900739823111991 ) ) ;
#64407 = CARTESIAN_POINT ( 'NONE',  ( 207.0171084425618346, 270.8969818057616408, 2.452340968668444532 ) ) ;
#64408 = CARTESIAN_POINT ( 'NONE',  ( 190.2389970918280540, 301.1433867864428748, 4.601241515604689525 ) ) ;
#64409 = CIRCLE ( 'NONE', #61201, 0.1418229129681591871 ) ;
#64410 = CARTESIAN_POINT ( 'NONE',  ( 180.7126655808842202, 271.3309753198433327, 16.61443135770589308 ) ) ;
#64411 = CARTESIAN_POINT ( 'NONE',  ( 164.7762319088960794, 245.2461897844768828, 2.994040459560653122 ) ) ;
#64412 = CARTESIAN_POINT ( 'NONE',  ( 164.1893796463498632, 253.9140536989919497, 14.56309422521135843 ) ) ;
#64413 = FACE_OUTER_BOUND ( 'NONE', #24545, .T. ) ;
#64414 = VECTOR ( 'NONE', #88270, 1000.000000000000000 ) ;
#64415 = CARTESIAN_POINT ( 'NONE',  ( 137.1160976468485444, 237.7202760586660020, -5.415160957724236172E-17 ) ) ;
#64416 = ORIENTED_EDGE ( 'NONE', *, *, #34279, .T. ) ;
#64417 = CARTESIAN_POINT ( 'NONE',  ( 87.51397647008028002, 44.34712510374425420, -4.234924872237962212 ) ) ;
#64418 = CARTESIAN_POINT ( 'NONE',  ( 82.57480368249606784, 41.04376301281222794, 1.111617510708536205 ) ) ;
#64419 = CARTESIAN_POINT ( 'NONE',  ( 46.89542285554266954, 70.53237680267110932, 10.00000000000000000 ) ) ;
#64420 = CARTESIAN_POINT ( 'NONE',  ( 182.7913689746213777, 285.6300500007765777, -15.59955371092600807 ) ) ;
#64421 = CARTESIAN_POINT ( 'NONE',  ( 74.72979125799862743, 60.84138562765400593, 15.40639291555719481 ) ) ;
#64422 = CARTESIAN_POINT ( 'NONE',  ( 175.2976070117660186, 253.4435804238109426, 4.989098000593277682 ) ) ;
#64423 = EDGE_LOOP ( 'NONE', ( #57653, #39594, #57675, #69768 ) ) ;
#64424 = CARTESIAN_POINT ( 'NONE',  ( 80.44351032975033888, 57.11231280812273781, -16.22991141722204134 ) ) ;
#64425 = VECTOR ( 'NONE', #49265, 1000.000000000000000 ) ;
#64426 = CARTESIAN_POINT ( 'NONE',  ( 71.88200430141152708, 72.22488123539891092, 0.5832661070486506727 ) ) ;
#64428 = CARTESIAN_POINT ( 'NONE',  ( 181.9401144352162021, 260.5691112182036591, 10.07005861877500763 ) ) ;
#64427 = CARTESIAN_POINT ( 'NONE',  ( 147.6346879868728479, 275.5076572718856482, 2.918840859857055658 ) ) ;
#64429 = CARTESIAN_POINT ( 'NONE',  ( 74.62796085038830540, 66.91441896689961766, 13.03852793085608397 ) ) ;
#64430 = CARTESIAN_POINT ( 'NONE',  ( 141.5001777056247931, 246.3768266524160140, 9.188101187500096856 ) ) ;
#64431 = EDGE_CURVE ( 'NONE', #70505, #39044, #48975, .T. ) ;
#64432 = CIRCLE ( 'NONE', #10856, 70.00000000000001421 ) ;
#64433 = FACE_OUTER_BOUND ( 'NONE', #21529, .T. ) ;
#64434 = CARTESIAN_POINT ( 'NONE',  ( 177.6699396433555762, 293.4499100638861364, -3.987850357589190153 ) ) ;
#64435 = CARTESIAN_POINT ( 'NONE',  ( 65.10058588945754821, 199.2048013555409796, 4.594050593750051981 ) ) ;
#64436 = EDGE_CURVE ( 'NONE', #89824, #20684, #9375, .T. ) ;
#64437 = CARTESIAN_POINT ( 'NONE',  ( 77.09656746912297365, 60.26159968811153078, -16.27885049838763720 ) ) ;
#64438 = CARTESIAN_POINT ( 'NONE',  ( 205.4103625296683617, 274.8658110279089897, -13.38953657917851814 ) ) ;
#64439 = CARTESIAN_POINT ( 'NONE',  ( 192.5260769942808281, 296.7927711323272888, 11.16196026814283471 ) ) ;
#64440 = CARTESIAN_POINT ( 'NONE',  ( 171.1373347109045824, 259.7557668617522495, 15.18341589746758480 ) ) ;
#64441 = CARTESIAN_POINT ( 'NONE',  ( 154.9517153487096550, 280.5398731376675414, -0.8905349252829396489 ) ) ;
#64442 = CARTESIAN_POINT ( 'NONE',  ( 172.6345960983117322, 287.6965781455015190, -8.272603404180184583 ) ) ;
#64443 = CARTESIAN_POINT ( 'NONE',  ( 155.0619429961492983, 262.0718317407570339, -17.08853361476647592 ) ) ;
#64444 = CARTESIAN_POINT ( 'NONE',  ( 157.2429883677972100, 271.5286301573580658, -14.65303208119756562 ) ) ;
#64445 = CARTESIAN_POINT ( 'NONE',  ( 112.1543725048142903, 248.8927522451419634, 2.944929066748280225E-16 ) ) ;
#64446 = CARTESIAN_POINT ( 'NONE',  ( 23.63615849558155446, 18.81029122506294726, 8.090169943749479842 ) ) ;
#64447 = EDGE_LOOP ( 'NONE', ( #66368, #45832, #54424, #48760 ) ) ;
#64448 = EDGE_CURVE ( 'NONE', #67853, #41536, #69409, .T. ) ;
#64449 = CARTESIAN_POINT ( 'NONE',  ( 159.2951220875037848, 257.7226857971661502, -17.27556336337253740 ) ) ;
#64450 = CARTESIAN_POINT ( 'NONE',  ( -4.533703103291246705, 174.3149278399161233, 9.188101187500093303 ) ) ;
#64451 = CARTESIAN_POINT ( 'NONE',  ( 37.63108229134613225, 192.5333772461660544, 9.188101187500095079 ) ) ;
#64452 = CARTESIAN_POINT ( 'NONE',  ( 14.27891468289787369, 30.01751292744055277, 6.180339887498949913 ) ) ;
#64453 = CARTESIAN_POINT ( 'NONE',  ( 88.10161777267849459, 43.64076697146427364, 0.1132407729617426612 ) ) ;
#64454 = CARTESIAN_POINT ( 'NONE',  ( 180.9701587135972431, 266.4289169444708705, -14.70082405781458945 ) ) ;
#64455 = CARTESIAN_POINT ( 'NONE',  ( 71.35865581505748878, 223.5530062829863027, -4.648177544792955347E-16 ) ) ;
#64456 = CARTESIAN_POINT ( 'NONE',  ( 190.7908437487391780, 300.1875603386860689, -4.317984972589949955 ) ) ;
#64457 = CARTESIAN_POINT ( 'NONE',  ( 72.23865006290039048, 71.95475215217994958, 3.607730569270007237 ) ) ;
#64459 = CARTESIAN_POINT ( 'NONE',  ( 61.41971759977600698, 196.2677522451418213, -5.000000000000041744 ) ) ;
#64458 = CARTESIAN_POINT ( 'NONE',  ( 11.77607482435655051, 8.927558733836240989, 6.180339887498953466 ) ) ;
#64460 = CARTESIAN_POINT ( 'NONE',  ( 3.562051267137642085, 25.55466486950697558, -1.111400068045478839E-16 ) ) ;
#64461 = CARTESIAN_POINT ( 'NONE',  ( 184.7298463175202698, 257.7777764843742148, 1.366536233435324821 ) ) ;
#64462 = CARTESIAN_POINT ( 'NONE',  ( 46.30674614090290220, 112.4688969640381231, 10.00000000000000000 ) ) ;
#64463 = CARTESIAN_POINT ( 'NONE',  ( 171.3171204526115616, 271.4791138034659070, -17.75561031716327420 ) ) ;
#64464 = CARTESIAN_POINT ( 'NONE',  ( 161.4023172760800833, 267.9375969907274566, 17.21476449095039030 ) ) ;
#64465 = CARTESIAN_POINT ( 'NONE',  ( 43.32339510341152788, 202.4865022471903160, -10.00000000000009415 ) ) ;
#64466 = B_SPLINE_CURVE_WITH_KNOTS ( 'NONE', 3,
 ( #94750, #96756, #26327, #81069, #72946, #33419, #17729, #3052, #87696, #56713, #64318, #4507, #3539, #25838, #42013, #57201, #65316, #25312, #49124, #19734, #80060, #72446, #33940, #27324, #96255, #26820, #64826, #95771, #57700, #88677, #50115, #11632, #58208, #50600, #12119, #42984, #35407, #59696, #74440, #28809, #22204, #75421, #97247, #74928, #67300, #27813, #5511, #83045 ),
 .UNSPECIFIED., .F., .F.,
 ( 4, 2, 2, 2, 2, 2, 2, 2, 2, 2, 2, 2, 2, 2, 2, 2, 2, 2, 2, 2, 2, 2, 2, 4 ),
 ( 0.002425426540219128169, 0.002845973489409292512, 0.003056246964004374900, 0.003161383701301915660, 0.003266520438599456854, 0.003371657175896998048, 0.003476793913194539242, 0.003687067387789621196, 0.004107614336979621174, 0.004948708235359621128, 0.005789802133739620216, 0.006630896032119620170, 0.007051442981309627087, 0.007471989930499632268, 0.007577126667797215095, 0.007629695036445971815, 0.007682263405094728534, 0.007734831773743485253, 0.007787400142392240238, 0.007892536879689727655, 0.008102810354284695551, 0.008313083828879661713, 0.008733630778069562811, 0.009154177727259465644 ),
 .UNSPECIFIED. ) ;
#64467 = CARTESIAN_POINT ( 'NONE',  ( -25.89332989531674301, 24.59406508915897760, -10.00000000000000000 ) ) ;
#64468 = CARTESIAN_POINT ( 'NONE',  ( 202.6070187115982719, 279.7213449518906145, 15.56322169823762280 ) ) ;
#64469 = VECTOR ( 'NONE', #76037, 1000.000000000000000 ) ;
#64470 = CARTESIAN_POINT ( 'NONE',  ( 8.727484440040480962, 175.8458772461660828, 9.188101187500095079 ) ) ;
#64471 = CARTESIAN_POINT ( 'NONE',  ( 32.17510246534131113, 41.68290643055190259, 3.479690158560446702E-15 ) ) ;
#64473 = CARTESIAN_POINT ( 'NONE',  ( 170.4606321698994407, 263.6007259650322680, 15.80273850856594997 ) ) ;
#64472 = CARTESIAN_POINT ( 'NONE',  ( 163.9905008462251317, 247.0786441245412561, 6.065918779697442531 ) ) ;
#64474 = CARTESIAN_POINT ( 'NONE',  ( 152.9920137376499838, 265.6570543845515431, 16.15798175643282164 ) ) ;
#64475 = CARTESIAN_POINT ( 'NONE',  ( 32.17510246534131113, 41.68290643055190259, 3.479690158560446702E-15 ) ) ;
#64477 = AXIS2_PLACEMENT_3D ( 'NONE', #38634, #53342, #84293 ) ;
#64476 = CARTESIAN_POINT ( 'NONE',  ( 184.0255633751473852, 258.2697744397484598, -2.304790711699857830 ) ) ;
#64478 = CARTESIAN_POINT ( 'NONE',  ( 66.54264984482914258, 68.81226801441182772, 2.258477026830885581 ) ) ;
#64479 = CARTESIAN_POINT ( 'NONE',  ( 196.2421909983451940, 290.7455499326673021, -17.31908925000307065 ) ) ;
#64480 = FACE_OUTER_BOUND ( 'NONE', #32874, .T. ) ;
#64481 = VECTOR ( 'NONE', #89253, 1000.000000000000000 ) ;
#64482 = CARTESIAN_POINT ( 'NONE',  ( 9.401013375279877238, 17.37878583063838889, 9.188101187500006262 ) ) ;
#64483 = CARTESIAN_POINT ( 'NONE',  ( 167.3422145247286039, 287.9343817845129934, 0.5404251914103093135 ) ) ;
#64484 = CARTESIAN_POINT ( 'NONE',  ( 15.60392711327956761, 29.98502408145592213, -5.678558825948271327 ) ) ;
#64485 = CARTESIAN_POINT ( 'NONE',  ( 206.9809521314431606, 272.1454700397959527, 9.518650961382352449 ) ) ;
#64486 = CARTESIAN_POINT ( 'NONE',  ( 152.9566069573676543, 278.2300974794858917, -4.664778606640360259 ) ) ;
#64487 = CARTESIAN_POINT ( 'NONE',  ( 76.55480823776410659, 226.5530062829863027, -4.648177544792955347E-16 ) ) ;
#64488 = CARTESIAN_POINT ( 'NONE',  ( 159.9788992190088948, 253.5554137441726255, -15.81862932303382330 ) ) ;
#64489 = ORIENTED_EDGE ( 'NONE', *, *, #43447, .T. ) ;
#64490 = CARTESIAN_POINT ( 'NONE',  ( 153.3616370783189211, 265.0168479788495688, 17.48287904751960653 ) ) ;
#64491 = CARTESIAN_POINT ( 'NONE',  ( 164.7694554770609159, 245.2579269087094076, -3.003635650077957742 ) ) ;
#64492 = CARTESIAN_POINT ( 'NONE',  ( 66.06021207013861840, 68.53184239669842270, 4.555218141334386850 ) ) ;
#64493 = CARTESIAN_POINT ( 'NONE',  ( 87.31810034388520592, 45.47295687595354252, 7.117869854781806005 ) ) ;
#64494 = DIRECTION ( 'NONE',  ( 4.336808689942034499E-16, 7.511572993685835585E-16, -1.000000000000000000 ) ) ;
#64495 = EDGE_LOOP ( 'NONE', ( #73244, #3767, #65365, #84284 ) ) ;
#64496 = AXIS2_PLACEMENT_3D ( 'NONE', #66095, #27611, #43276 ) ;
#64497 = ORIENTED_EDGE ( 'NONE', *, *, #20714, .F. ) ;
#64498 = CARTESIAN_POINT ( 'NONE',  ( 129.9777503372646095, 257.3967562850347122, -4.648177544792955347E-16 ) ) ;
#64499 = CARTESIAN_POINT ( 'NONE',  ( 86.70421956006907749, 47.09494090442339598, 10.43848816880117525 ) ) ;
#64500 = ORIENTED_EDGE ( 'NONE', *, *, #76532, .T. ) ;
#64501 = CARTESIAN_POINT ( 'NONE',  ( 77.94705490036190554, 58.67815114825116041, 16.13782593773457918 ) ) ;
#64502 = CARTESIAN_POINT ( 'NONE',  ( 188.9968840092409437, 297.1838958854766588, 7.940645936764939350 ) ) ;
#64503 = ORIENTED_EDGE ( 'NONE', *, *, #44455, .T. ) ;
#64505 = EDGE_CURVE ( 'NONE', #24764, #23591, #13445, .T. ) ;
#64504 = FACE_OUTER_BOUND ( 'NONE', #44518, .T. ) ;
#64506 = CARTESIAN_POINT ( 'NONE',  ( 84.22051715105205005, 48.65629006738927842, -12.53906321451517059 ) ) ;
#64507 = B_SPLINE_CURVE_WITH_KNOTS ( 'NONE', 3,
 ( #94347, #16305, #17304, #48208, #63904, #40590, #1115, #25926, #94842, #24901, #18323, #55777, #80153, #63408, #33003, #78122 ),
 .UNSPECIFIED., .F., .F.,
 ( 4, 1, 2, 2, 2, 1, 2, 2, 4 ),
 ( 0.000000000000000000, 0.1249999999999967804, 0.1874999999999966693, 0.2499999999999965583, 0.4999999999999932276, 0.6249999999999914513, 0.6874999999999918954, 0.7499999999999924505, 1.000000000000000000 ),
 .UNSPECIFIED. ) ;
#64508 = VECTOR ( 'NONE', #2791, 1000.000000000000000 ) ;
#64509 = CARTESIAN_POINT ( 'NONE',  ( 80.72348862661678481, 43.14103115498581076, 9.877424986543475782 ) ) ;
#64510 = ORIENTED_EDGE ( 'NONE', *, *, #41016, .F. ) ;
#64511 = CARTESIAN_POINT ( 'NONE',  ( 174.5422266480219662, 267.5925051635639420, 17.37569662752725463 ) ) ;
#64512 = CARTESIAN_POINT ( 'NONE',  ( 206.4943150373521803, 272.9883502116088039, 11.34100825923693101 ) ) ;
#64513 = CARTESIAN_POINT ( 'NONE',  ( 151.4015714417470519, 275.0754632453579802, -8.499728915061472989 ) ) ;
#64514 = B_SPLINE_SURFACE_WITH_KNOTS ( 'NONE', 3, 1, ( 
 ( #22988, #83849 ),
 ( #37201, #14415 ),
 ( #22503, #84839 ),
 ( #85344, #68103 ),
 ( #37686, #53396 ),
 ( #84346, #59990 ),
 ( #7296, #77721 ),
 ( #30105, #15377 ),
 ( #45780, #61974 ),
 ( #38176, #99521 ),
 ( #46275, #77198 ),
 ( #7805, #38691 ),
 ( #90960, #69596 ),
 ( #54371, #23480 ),
 ( #15889, #46801 ),
 ( #24497, #94436 ),
 ( #79748, #70086 ),
 ( #72118, #2219 ),
 ( #39668, #54890 ),
 ( #93943, #1206 ),
 ( #9824, #71118 ),
 ( #9303, #49307 ),
 ( #25501, #62999 ),
 ( #80245, #23992 ),
 ( #32085, #17395 ),
 ( #33100, #70592 ),
 ( #16891, #86865 ),
 ( #47781, #40685 ),
 ( #1719, #93439 ),
 ( #48307, #39171 ),
 ( #17917, #698 ) ),
 .UNSPECIFIED., .F., .F., .F.,
 ( 4, 3, 3, 3, 3, 3, 3, 3, 3, 3, 4 ),
 ( 2, 2 ),
 ( 0.000000000000000000, 0.1333490885032387052, 0.3007194338854507487, 0.4699862290245374608, 0.5844252810809412724, 0.6686540514502781196, 0.7354980260655558100, 0.8028463152565722405, 0.8633854507757224850, 0.9437142632667419040, 1.000000000000000000 ),
 ( 0.000000000000000000, 1.000000000000000000 ),
 .UNSPECIFIED. ) ;
#64515 = ORIENTED_EDGE ( 'NONE', *, *, #47988, .F. ) ;
#64516 = CARTESIAN_POINT ( 'NONE',  ( 171.4187126090420747, 256.0395575307684339, -11.60209380571112625 ) ) ;
#64517 = CARTESIAN_POINT ( 'NONE',  ( 203.0535368433499457, 278.9479528611958585, 16.46202213522710167 ) ) ;
#64518 = ORIENTED_EDGE ( 'NONE', *, *, #84564, .F. ) ;
#64519 = ORIENTED_EDGE ( 'NONE', *, *, #76556, .T. ) ;
#64520 = CARTESIAN_POINT ( 'NONE',  ( 156.7755893566837244, 266.6085710678392502, -16.22358508212092687 ) ) ;
#64521 = EDGE_LOOP ( 'NONE', ( #71369, #9103, #28942, #81123, #64370 ) ) ;
#64522 = CARTESIAN_POINT ( 'NONE',  ( 161.1235494854506953, 271.0628771894291731, 16.08318537909542556 ) ) ;
#64523 = ORIENTED_EDGE ( 'NONE', *, *, #87504, .F. ) ;
#64524 = CARTESIAN_POINT ( 'NONE',  ( 168.6046935506172417, 272.7627849129413562, 15.97842110015704264 ) ) ;
#64525 = CARTESIAN_POINT ( 'NONE',  ( 193.7351983448268129, 295.0877885827630962, 13.32537352665005059 ) ) ;
#64526 = CARTESIAN_POINT ( 'NONE',  ( 180.4994900830837992, 291.2687899966102236, -9.662810889139459292 ) ) ;
#64527 = CARTESIAN_POINT ( 'NONE',  ( 72.43095172406538040, 71.17131323670344045, 6.069991975535843132 ) ) ;
#64528 = CARTESIAN_POINT ( 'NONE',  ( 193.7987916076703243, 294.5354169763049867, 13.61361374954321768 ) ) ;
#64529 = CARTESIAN_POINT ( 'NONE',  ( 174.6180048270524594, 290.3475991095135100, 6.420941954033795973 ) ) ;
#64530 = CARTESIAN_POINT ( 'NONE',  ( 197.6885739199660463, 288.2403412252199928, -17.06545875591766759 ) ) ;
#64531 = ORIENTED_EDGE ( 'NONE', *, *, #50952, .F. ) ;
#64532 = CARTESIAN_POINT ( 'NONE',  ( 174.9358745049650565, 292.2217799751211942, 2.235529367806339263 ) ) ;
#64533 = CARTESIAN_POINT ( 'NONE',  ( 24.91850453858129910, 20.10170272979927475, -7.433330006724141015 ) ) ;
#64534 = CARTESIAN_POINT ( 'NONE',  ( 206.1215120922853146, 273.6340638536760821, 10.12238414215620885 ) ) ;
#64535 = CARTESIAN_POINT ( 'NONE',  ( 206.4943150373521803, 272.9883502116088039, 11.34100825923693101 ) ) ;
#64537 = VERTEX_POINT ( 'NONE', #44310 ) ;
#64536 = CARTESIAN_POINT ( 'NONE',  ( 198.2414483977475754, 287.2827345394944700, 16.94931984969033678 ) ) ;
#64538 = EDGE_LOOP ( 'NONE', ( #38299, #48823, #56245, #83809, #21738 ) ) ;
#64539 = CARTESIAN_POINT ( 'NONE',  ( 190.5800505906290141, 300.5526647984205511, 6.752949403983271814 ) ) ;
#64540 = CARTESIAN_POINT ( 'NONE',  ( 171.5607332741838036, 259.4587583041368930, -13.88734664787412321 ) ) ;
#64541 = CARTESIAN_POINT ( 'NONE',  ( 43.35468487962022266, 120.5828561944265687, -10.00000000000000000 ) ) ;
#64542 = CARTESIAN_POINT ( 'NONE',  ( 40.82928596147627331, 60.38352576601455723, -10.00000000000000000 ) ) ;
#64543 = CARTESIAN_POINT ( 'NONE',  ( 160.4869048512927918, 252.6755221785256822, -16.09843817406293809 ) ) ;
#64544 = CARTESIAN_POINT ( 'NONE',  ( 190.8232856196690079, 262.0104826008901568, -0.7083013378410631944 ) ) ;
#64545 = ORIENTED_EDGE ( 'NONE', *, *, #99485, .F. ) ;
#64547 = DIRECTION ( 'NONE',  ( 0.5000000000000013323, -0.8660254037844378194, 0.000000000000000000 ) ) ;
#64546 = B_SPLINE_CURVE_WITH_KNOTS ( 'NONE', 3,
 ( #24454, #47248, #63456, #31542 ),
 .UNSPECIFIED., .F., .F.,
 ( 4, 4 ),
 ( 0.01245835406871842466, 0.02099269020319429607 ),
 .UNSPECIFIED. ) ;
#64548 = CARTESIAN_POINT ( 'NONE',  ( 60.28305926085685229, 195.6115022471902023, -5.000000000000041744 ) ) ;
#64549 = AXIS2_PLACEMENT_3D ( 'NONE', #22045, #91998, #22548 ) ;
#64550 = CARTESIAN_POINT ( 'NONE',  ( -28.64605662510459183, 40.80936565889331291, 59.99999999999999289 ) ) ;
#64551 = CARTESIAN_POINT ( 'NONE',  ( 24.61363793893735874, 175.0177522451417929, 5.000000000000051514 ) ) ;
#64552 = CARTESIAN_POINT ( 'NONE',  ( 106.6698052711106186, 223.2048013555410080, 4.594050593750051981 ) ) ;
#64553 = CARTESIAN_POINT ( 'NONE',  ( 82.44400793032374963, 40.43910385561510878, -1.368357710041455011 ) ) ;
#64554 = AXIS2_PLACEMENT_3D ( 'NONE', #6874, #83421, #69667 ) ;
#64555 = CARTESIAN_POINT ( 'NONE',  ( 84.81057673196700364, 50.23847654986280276, 13.36435190918987459 ) ) ;
#64556 = CARTESIAN_POINT ( 'NONE',  ( 162.5082079047825800, 249.1745225923870919, 11.52567592363465465 ) ) ;
#64557 = VECTOR ( 'NONE', #66297, 1000.000000000000000 ) ;
#64558 = CARTESIAN_POINT ( 'NONE',  ( 11.67712314985746858, 186.7369531367911293, -4.594050593750048428 ) ) ;
#64559 = EDGE_CURVE ( 'NONE', #78822, #81724, #29623, .T. ) ;
#64560 = CARTESIAN_POINT ( 'NONE',  ( 200.8551880497955437, 282.7556046643899776, 18.00894873733387058 ) ) ;
#64561 = EDGE_LOOP ( 'NONE', ( #81725, #62138, #84223, #72812 ) ) ;
#64562 = AXIS2_PLACEMENT_3D ( 'NONE', #80674, #19834, #3640 ) ;
#64564 = ORIENTED_EDGE ( 'NONE', *, *, #59213, .F. ) ;
#64563 = UNCERTAINTY_MEASURE_WITH_UNIT (LENGTH_MEASURE( 1.000000000000000082E-05 ), #13615, 'distance_accuracy_value', 'NONE');
#64565 = CARTESIAN_POINT ( 'NONE',  ( 147.6130911253305271, 276.0666186809932015, -0.7644645089462269727 ) ) ;
#64566 = ADVANCED_FACE ( 'NONE', ( #76244 ), #75242, .T. ) ;
#64567 = CARTESIAN_POINT ( 'NONE',  ( 66.77752810875767864, 68.40544692769400115, 4.459354299965320401 ) ) ;
#64568 = CARTESIAN_POINT ( 'NONE',  ( 84.61167648532155283, 44.54557622999233502, 8.014713256522945528 ) ) ;
#64569 = CARTESIAN_POINT ( 'NONE',  ( 192.9940517273955720, 263.8598628230966483, -4.307169378521571446 ) ) ;
#64570 = CARTESIAN_POINT ( 'NONE',  ( -77.58047734835668052, 56.02942318228900120, 10.00000000000000000 ) ) ;
#64571 = VECTOR ( 'NONE', #25998, 1000.000000000000114 ) ;
#64572 = CARTESIAN_POINT ( 'NONE',  ( 69.04680748359113807, 64.17805710937504671, 12.06412625981762865 ) ) ;
#64573 = CARTESIAN_POINT ( 'NONE',  ( 168.0837743945575369, 251.4641930119366293, 10.72931100272645644 ) ) ;
#64574 = CARTESIAN_POINT ( 'NONE',  ( 47.67182463829572470, 189.1423013555410080, -4.594050593750043987 ) ) ;
#64575 = CARTESIAN_POINT ( 'NONE',  ( 79.60625107924921906, 206.7677522451417929, -5.000000000000041744 ) ) ;
#64576 = EDGE_LOOP ( 'NONE', ( #55022, #43068, #72995, #49130 ) ) ;
#64577 = EDGE_CURVE ( 'NONE', #37080, #65018, #52539, .T. ) ;
#64578 = CARTESIAN_POINT ( 'NONE',  ( 83.14942813903591912, 45.25422836440832697, 9.956978268961167444 ) ) ;
#64579 = B_SPLINE_CURVE_WITH_KNOTS ( 'NONE', 3,
 ( #214, #61986, #92939, #54382, #93451, #24005, #54903, #34125, #43185, #49319, #25517, #88885, #3242, #48829, #95963, #18430, #94953, #72131, #81255, #11343, #4202, #19925, #33623, #95477, #56900, #27022, #50303, #89370, #26526, #35099, #26030, #33113, #64520, #73619, #34607, #66010, #74126, #81747, #57905, #11830, #80772, #80258, #19446, #65019, #64013, #87884, #10824, #41703, #88380, #42199, #72646, #57400 ),
 .UNSPECIFIED., .F., .F.,
 ( 4, 2, 2, 2, 2, 2, 2, 2, 2, 2, 2, 2, 2, 2, 2, 2, 2, 2, 2, 2, 2, 2, 2, 2, 2, 4 ),
 ( 0.002899484069035259196, 0.003100245425264694290, 0.003301006781494129384, 0.003401387459608835873, 0.003501768137723542795, 0.003602148815838249283, 0.003702529493952955771, 0.003903290850182310201, 0.004104052206411664197, 0.004505574918870284586, 0.005308620343787543577, 0.006111665768704803436, 0.006914711193622062428, 0.007717756618539321420, 0.007818137296653968060, 0.007868327635711292248, 0.007918517974768614701, 0.007968708313825938888, 0.008018898652883261341, 0.008119279330997875022, 0.008320040687227098913, 0.008520802043456319336, 0.008721563399685543228, 0.008922324755914767119, 0.009123086112143989276, 0.009323847468373211433 ),
 .UNSPECIFIED. ) ;
#64580 = CARTESIAN_POINT ( 'NONE',  ( -22.42236680055709641, 157.8615022471902591, 0.000000000000000000 ) ) ;
#64581 = AXIS2_PLACEMENT_3D ( 'NONE', #48394, #1800, #54460 ) ;
#64582 = CARTESIAN_POINT ( 'NONE',  ( 4.126898030318161936, 167.0643266524160424, 9.188101187500095079 ) ) ;
#64583 = CARTESIAN_POINT ( 'NONE',  ( 68.55321753847707100, 64.55974346124446583, -12.18496927705354516 ) ) ;
#64584 = CARTESIAN_POINT ( 'NONE',  ( 199.0363797504450929, 285.9058730480928716, -17.12190301149298222 ) ) ;
#64585 = CARTESIAN_POINT ( 'NONE',  ( 186.5011568818524381, 282.7666149734188821, 16.16427038733343480 ) ) ;
#64586 = CARTESIAN_POINT ( 'NONE',  ( 193.1444937042664094, 296.1109190324805240, -12.15243020627156767 ) ) ;
#64587 = CARTESIAN_POINT ( 'NONE',  ( 43.24043327773039636, 120.8247932685368227, -10.00000000000000000 ) ) ;
#64588 = CARTESIAN_POINT ( 'NONE',  ( 163.9942050550062049, 246.6007000282974673, 5.791111691696777974 ) ) ;
#64589 = CARTESIAN_POINT ( 'NONE',  ( 147.2229325088103735, 275.6493961858936927, -0.4918294119671829390 ) ) ;
#64590 = CARTESIAN_POINT ( 'NONE',  ( 206.8968397926183229, 272.2911568841838061, 7.145103750817420440 ) ) ;
#64591 = EDGE_CURVE ( 'NONE', #49306, #49232, #67116, .T. ) ;
#64592 = ORIENTED_EDGE ( 'NONE', *, *, #28146, .T. ) ;
#64593 = CARTESIAN_POINT ( 'NONE',  ( -7.772103719870364635, 172.9865022471902876, 10.00000000000009237 ) ) ;
#64594 = CARTESIAN_POINT ( 'NONE',  ( 181.2112225862389323, 268.1041159954503996, 15.22766750904507660 ) ) ;
#64595 = CARTESIAN_POINT ( 'NONE',  ( 114.4365367415960293, 243.0024278399160949, -9.188101187500093303 ) ) ;
#64596 = CARTESIAN_POINT ( 'NONE',  ( 15.40246583222295129, 30.93396525600389424, 2.839279412974139660 ) ) ;
#64597 = CARTESIAN_POINT ( 'NONE',  ( 39.64431452495995245, 58.26521502737223557, 10.00000000000000000 ) ) ;
#64598 = DIRECTION ( 'NONE',  ( 0.4999999999999998890, -0.8660254037844385966, 0.000000000000000000 ) ) ;
#64600 = CARTESIAN_POINT ( 'NONE',  ( 149.3118911495987788, 247.0312136851381126, 5.028230608967417581 ) ) ;
#64599 = CARTESIAN_POINT ( 'NONE',  ( 196.1613785401733878, 290.8855212161054737, 15.98157687694135021 ) ) ;
#64601 = CARTESIAN_POINT ( 'NONE',  ( 150.4341052900205682, 270.0874817769553147, -15.18648472748443368 ) ) ;
#64602 = ORIENTED_EDGE ( 'NONE', *, *, #49871, .F. ) ;
#64603 = CARTESIAN_POINT ( 'NONE',  ( 189.7662698355838984, 261.5339742162131529, -4.454810789157368944 ) ) ;
#64604 = CARTESIAN_POINT ( 'NONE',  ( 196.7823306783968746, 289.8100005636337073, -17.85370042640856170 ) ) ;
#64605 = LINE ( 'NONE', #35186, #99247 ) ;
#64606 = CARTESIAN_POINT ( 'NONE',  ( -5.171971415982786979, 24.31384663199769491, 10.00000000000000000 ) ) ;
#64607 = CARTESIAN_POINT ( 'NONE',  ( 81.77341040013584461, 55.39003076602018183, -15.93424821120281010 ) ) ;
#64608 = CARTESIAN_POINT ( 'NONE',  ( 189.1592966827000737, 265.6623959474144954, 10.76674785942434909 ) ) ;
#64609 = CARTESIAN_POINT ( 'NONE',  ( 175.0739399029997116, 279.4198807484980307, 16.07690566252637510 ) ) ;
#64610 = CARTESIAN_POINT ( 'NONE',  ( 168.0272649302995092, 271.2940026294745053, -16.46671956731438158 ) ) ;
#64611 = EDGE_CURVE ( 'NONE', #10907, #1989, #35336, .T. ) ;
#64612 = EDGE_CURVE ( 'NONE', #15371, #41986, #5822, .T. ) ;
#64613 = CARTESIAN_POINT ( 'NONE',  ( 200.0499121993288441, 272.4670071845189909, 12.52220648084497512 ) ) ;
#64614 = LINE ( 'NONE', #95569, #26675 ) ;
#64615 = CARTESIAN_POINT ( 'NONE',  ( 25.96864935082050252, 154.0458036431183189, -21.50000000000001421 ) ) ;
#64616 = CARTESIAN_POINT ( 'NONE',  ( 148.1311260530199547, 274.4913500102855437, 6.529054274877645447 ) ) ;
#64617 = EDGE_CURVE ( 'NONE', #13423, #52319, #77859, .T. ) ;
#64618 = EDGE_LOOP ( 'NONE', ( #32704, #95946, #40792, #42559 ) ) ;
#64619 = CARTESIAN_POINT ( 'NONE',  ( 190.9966433480338139, 280.6469662536845817, 16.69273669211117550 ) ) ;
#64620 = CARTESIAN_POINT ( 'NONE',  ( 45.46674490716588224, 28.11110640527296312, -2.839279412974138328 ) ) ;
#64621 = CARTESIAN_POINT ( 'NONE',  ( 194.5455058173357372, 289.6927750867642999, -16.22697001666201189 ) ) ;
#64622 = ORIENTED_EDGE ( 'NONE', *, *, #232, .T. ) ;
#64623 = CARTESIAN_POINT ( 'NONE',  ( 165.3079345244091769, 279.7873310763220047, 11.79426121657854765 ) ) ;
#64625 = EDGE_CURVE ( 'NONE', #50553, #5374, #16302, .T. ) ;
#64624 = CARTESIAN_POINT ( 'NONE',  ( 194.8598199529639317, 293.1398868181796615, -15.91766051364927570 ) ) ;
#64626 = CARTESIAN_POINT ( 'NONE',  ( 82.73417970902306706, 44.01214333168216086, -9.530255576316653432 ) ) ;
#64627 = ORIENTED_EDGE ( 'NONE', *, *, #52083, .F. ) ;
#64628 = AXIS2_PLACEMENT_3D ( 'NONE', #31177, #93529, #61077 ) ;
#64630 = EDGE_CURVE ( 'NONE', #5467, #27174, #67663, .T. ) ;
#64629 = CARTESIAN_POINT ( 'NONE',  ( 79.01330593081745235, 59.80254073573071594, 16.49416071572547793 ) ) ;
#64631 = CARTESIAN_POINT ( 'NONE',  ( -22.42236680055709641, 157.8615022471902591, 0.000000000000000000 ) ) ;
#64632 = CARTESIAN_POINT ( 'NONE',  ( 190.8604783348975502, 300.0669496974951471, 7.597731640149610222 ) ) ;
#64633 = VECTOR ( 'NONE', #33959, 1000.000000000000000 ) ;
#64634 = CARTESIAN_POINT ( 'NONE',  ( 84.47860975560725194, 49.82577972120142817, -13.24615549146050952 ) ) ;
#64635 = CARTESIAN_POINT ( 'NONE',  ( 84.77891510154978505, 49.87095472550759467, -13.17003612441266469 ) ) ;
#64636 = CARTESIAN_POINT ( 'NONE',  ( 35.89232211637455094, 179.9824982072973683, 3.021315404115420679E-15 ) ) ;
#64637 = EDGE_CURVE ( 'NONE', #94303, #73115, #64579, .T. ) ;
#64638 = ORIENTED_EDGE ( 'NONE', *, *, #65791, .F. ) ;
#64639 = EDGE_CURVE ( 'NONE', #44339, #97853, #79762, .T. ) ;
#64640 = VERTEX_POINT ( 'NONE', #65506 ) ;
#64641 = CARTESIAN_POINT ( 'NONE',  ( 178.5336676047381843, 260.8667924985600166, 12.04724365429595068 ) ) ;
#64642 = VERTEX_POINT ( 'NONE', #12320 ) ;
#64643 = CARTESIAN_POINT ( 'NONE',  ( 77.53316523795550097, 49.65407854046259928, 14.92632681611246603 ) ) ;
#64644 = VERTEX_POINT ( 'NONE', #42688 ) ;
#64645 = LINE ( 'NONE', #55507, #45981 ) ;
#64647 = CARTESIAN_POINT ( 'NONE',  ( 86.35121876318000034, 43.08468197994678661, 0.3078304325362931637 ) ) ;
#64646 = CIRCLE ( 'NONE', #14453, 70.00000000000001421 ) ;
#64648 = ORIENTED_EDGE ( 'NONE', *, *, #26842, .F. ) ;
#64649 = DIRECTION ( 'NONE',  ( -0.4827766168686632997, -0.5834231310750495059, 0.6531035050674843800 ) ) ;
#64650 = CARTESIAN_POINT ( 'NONE',  ( 161.7900223312657033, 277.1148125758700189, -12.79293641940870785 ) ) ;
#64651 = CARTESIAN_POINT ( 'NONE',  ( 192.4259603496955719, 297.3554553095298729, -12.40738485318142814 ) ) ;
#64652 = CARTESIAN_POINT ( 'NONE',  ( 153.2583947049096764, 265.1956690150883560, -17.64103123457563882 ) ) ;
#64653 = CARTESIAN_POINT ( 'NONE',  ( 86.45815904198641988, 42.74312041874679124, -1.243629510017558948 ) ) ;
#64654 = CARTESIAN_POINT ( 'NONE',  ( 157.8859435148417560, 280.9531261477192743, 2.096246200910757196 ) ) ;
#64655 = CARTESIAN_POINT ( 'NONE',  ( 143.0428722300570143, 244.2048013555409511, 4.594050593750051981 ) ) ;
#64656 = ORIENTED_EDGE ( 'NONE', *, *, #33240, .F. ) ;
#64657 = CARTESIAN_POINT ( 'NONE',  ( 70.62475623734151498, 60.97173318496616190, -14.46351272653383369 ) ) ;
#64658 = CARTESIAN_POINT ( 'NONE',  ( 39.32338737416051089, 38.10171378149922106, 9.188101187500008038 ) ) ;
#64659 = ORIENTED_EDGE ( 'NONE', *, *, #25303, .F. ) ;
#64660 = VECTOR ( 'NONE', #24600, 1000.000000000000114 ) ;
#64662 = VERTEX_POINT ( 'NONE', #18934 ) ;
#64661 = CARTESIAN_POINT ( 'NONE',  ( 87.39605152047933245, 43.82633161050914339, -4.148852963258624627 ) ) ;
#64663 = CARTESIAN_POINT ( 'NONE',  ( 172.8210543149999978, 253.0650713199155177, -9.347212986753337560 ) ) ;
#64664 = DIRECTION ( 'NONE',  ( 0.8660254037844395958, 0.4999999999999985567, 0.000000000000000000 ) ) ;
#64665 = CARTESIAN_POINT ( 'NONE',  ( 44.98086946945897324, 119.9434018396067643, 177.5919119679930134 ) ) ;
#64666 = LINE ( 'NONE', #95615, #19174 ) ;
#64667 = CARTESIAN_POINT ( 'NONE',  ( 154.0294858510416418, 277.2251019646651571, 7.160722724867846445 ) ) ;
#64668 = CARTESIAN_POINT ( 'NONE',  ( 200.8147387322574957, 282.8256649374973790, -18.02438097732020239 ) ) ;
#64669 = CARTESIAN_POINT ( 'NONE',  ( 177.1701925416140000, 289.0260261616784874, -9.098077640916422126 ) ) ;
#64670 = CARTESIAN_POINT ( 'NONE',  ( 170.9473896922761185, 281.0006420345936817, 14.48361075345193605 ) ) ;
#64671 = CARTESIAN_POINT ( 'NONE',  ( 153.4281311866982946, 266.9016768047333130, 16.59090889036721350 ) ) ;
#64672 = CARTESIAN_POINT ( 'NONE',  ( 177.4410471705273835, 255.7678460362017177, -8.335468945180984690 ) ) ;
#64673 = ORIENTED_EDGE ( 'NONE', *, *, #21384, .F. ) ;
#64674 = CARTESIAN_POINT ( 'NONE',  ( 147.8505793332463725, 274.5622799967613332, -9.317516487097901035 ) ) ;
#64675 = CARTESIAN_POINT ( 'NONE',  ( 66.22087567261847596, 69.35898077670340456, 0.1737556617951544480 ) ) ;
#64676 = ORIENTED_EDGE ( 'NONE', *, *, #11475, .F. ) ;
#64677 = LINE ( 'NONE', #41859, #40288 ) ;
#64678 = CARTESIAN_POINT ( 'NONE',  ( 204.6061119446403040, 269.2277531849183561, -2.953647597350912424 ) ) ;
#64679 = CARTESIAN_POINT ( 'NONE',  ( 191.8032754232698380, 298.4339772392067403, -9.388979487922194167 ) ) ;
#64680 = DIRECTION ( 'NONE',  ( 0.000000000000000000, 0.000000000000000000, 1.000000000000000000 ) ) ;
#64681 = CARTESIAN_POINT ( 'NONE',  ( 202.7041331321765938, 279.5531378413010657, 17.14708438049711248 ) ) ;
#64683 = CARTESIAN_POINT ( 'NONE',  ( 151.4841312259729307, 274.9661650195698712, -8.701711564166631163 ) ) ;
#64682 = CYLINDRICAL_SURFACE ( 'NONE', #59774, 10.00000000000001066 ) ;
#64684 = CARTESIAN_POINT ( 'NONE',  ( 65.38900070045468738, 201.8927522451417929, -10.00000000000009237 ) ) ;
#64685 = EDGE_LOOP ( 'NONE', ( #86921, #17929, #30424, #14688 ) ) ;
#64686 = CARTESIAN_POINT ( 'NONE',  ( 71.39152386621661606, 62.51010730816707195, -13.96985413412476262 ) ) ;
#64687 = CARTESIAN_POINT ( 'NONE',  ( 193.3270472431910321, 276.0883453641457095, -16.25275238486911888 ) ) ;
#64688 = CARTESIAN_POINT ( 'NONE',  ( 69.70715393495058265, 66.25057049622556349, -10.63165605719265372 ) ) ;
#64689 = CARTESIAN_POINT ( 'NONE',  ( 152.7314557461996571, 266.1083540640618708, 17.39314074348802208 ) ) ;
#64690 =( BOUNDED_CURVE ( )  B_SPLINE_CURVE ( 2, ( #69942, #559, #1060, #78068, #39526, #31939, #95319, #40034, #25876 ),
 .UNSPECIFIED., .F., .T. ) 
 B_SPLINE_CURVE_WITH_KNOTS ( ( 3, 2, 2, 2, 3 ),
 ( 0.7298387096774193727, 0.7311827956989247479, 0.7338709677419354982, 0.7365591397849462485, 0.7379032258064516236 ),
 .UNSPECIFIED. ) 
 CURVE ( )  GEOMETRIC_REPRESENTATION_ITEM ( )  RATIONAL_B_SPLINE_CURVE ( ( 0.9330127018922194093, 0.9330127018922194093, 1.000000000000000000, 0.8660254037844387076, 1.000000000000000000, 0.8660254037844387076, 1.000000000000000000, 0.9330127018922194093, 0.9330127018922194093 ) ) 
 REPRESENTATION_ITEM ( '' )  );
#64691 = CARTESIAN_POINT ( 'NONE',  ( 80.80305022441423546, 43.21727299559393032, -9.912751086834814984 ) ) ;
#64692 = CARTESIAN_POINT ( 'NONE',  ( 66.76210968348311781, 68.73313199512115546, 3.352754309929160126 ) ) ;
#64693 = CARTESIAN_POINT ( 'NONE',  ( 198.7045056313791633, 284.4806958840320021, 17.79791830837532274 ) ) ;
#64694 = CARTESIAN_POINT ( 'NONE',  ( 87.80660267098954819, 215.3768266524160140, -9.188101187500091527 ) ) ;
#64695 = CARTESIAN_POINT ( 'NONE',  ( 88.07786909442063461, 44.67132779242000851, -4.228579230841192249 ) ) ;
#64696 = DIRECTION ( 'NONE',  ( -0.5000000000000002220, 0.8660254037844384856, 0.000000000000000000 ) ) ;
#64697 = ADVANCED_FACE ( 'NONE', ( #96960 ), #56407, .T. ) ;
#64699 = CARTESIAN_POINT ( 'NONE',  ( -1.733428585275474942, 158.2592609112379876, 2.679491924311254714 ) ) ;
#64698 = AXIS2_PLACEMENT_3D ( 'NONE', #39809, #56015, #93066 ) ;
#64700 = B_SPLINE_CURVE_WITH_KNOTS ( 'NONE', 3,
 ( #91563, #91078, #38314, #84472, #44918, #22134, #79256, #83980, #53024, #69223, #84963, #15507, #14545, #45419, #94441, #76354 ),
 .UNSPECIFIED., .F., .F.,
 ( 4, 1, 2, 2, 2, 1, 2, 2, 4 ),
 ( 0.000000000000000000, 0.1249999999999967526, 0.1874999999999966416, 0.2499999999999965583, 0.4999999999999960032, 0.6249999999999975575, 0.6874999999999977796, 0.7499999999999980016, 1.000000000000000000 ),
 .UNSPECIFIED. ) ;
#64701 = CARTESIAN_POINT ( 'NONE',  ( 75.31658791476552040, 55.15485285609985766, -16.13722419514472861 ) ) ;
#64702 = CARTESIAN_POINT ( 'NONE',  ( 160.8705110431349397, 281.6868185791299766, 5.475142679507278842 ) ) ;
#64704 = CARTESIAN_POINT ( 'NONE',  ( 207.6163508138795635, 271.0449272387537576, -1.385071889578343152 ) ) ;
#64703 = DIRECTION ( 'NONE',  ( -0.8660254037844379305, -0.5000000000000015543, -0.000000000000000000 ) ) ;
#64705 = CARTESIAN_POINT ( 'NONE',  ( 207.7395400852921341, 270.8315571617199566, 6.369933974605918259 ) ) ;
#64706 = EDGE_CURVE ( 'NONE', #19414, #91958, #74120, .T. ) ;
#64707 = DIRECTION ( 'NONE',  ( 1.000000000000000000, 0.000000000000000000, 0.000000000000000000 ) ) ;
#64708 = CARTESIAN_POINT ( 'NONE',  ( 74.60185817734695490, 56.26757446378344696, -16.11404827356958336 ) ) ;
#64709 = CARTESIAN_POINT ( 'NONE',  ( 81.20191240145091172, 53.29400499465850771, -15.90005951679047236 ) ) ;
#64710 = ADVANCED_FACE ( 'NONE', ( #96455 ), #2737, .F. ) ;
#64711 = LINE ( 'NONE', #72834, #31914 ) ;
#64712 = DIRECTION ( 'NONE',  ( 0.000000000000000000, 0.000000000000000000, 1.000000000000000000 ) ) ;
#64713 = AXIS2_PLACEMENT_3D ( 'NONE', #42362, #50968, #90017 ) ;
#64714 = CARTESIAN_POINT ( 'NONE',  ( 47.26526781268299260, 210.3464784336661637, 1.353441290958777327E-15 ) ) ;
#64715 = CARTESIAN_POINT ( 'NONE',  ( 77.07812270435945834, 63.66946605146480209, -15.38604565157081794 ) ) ;
#64716 = CARTESIAN_POINT ( 'NONE',  ( 74.76226857436894591, 201.7202760586659167, -5.415160957724236172E-17 ) ) ;
#64717 = CARTESIAN_POINT ( 'NONE',  ( 164.8489450237687493, 247.1202469751449939, -7.123750760659631531 ) ) ;
#64718 = CARTESIAN_POINT ( 'NONE',  ( 72.49386282319785835, 57.57572440859879492, 15.80166580940835885 ) ) ;
#64719 = DIRECTION ( 'NONE',  ( 0.000000000000000000, 1.000000000000000000, -1.090355031989287297E-16 ) ) ;
#64721 = CARTESIAN_POINT ( 'NONE',  ( 14.20097916528452942, 190.5530062829863311, -4.648177544792955347E-16 ) ) ;
#64720 = LINE ( 'NONE', #95669, #87330 ) ;
#64723 = AXIS2_PLACEMENT_3D ( 'NONE', #13987, #90539, #51482 ) ;
#64722 = CARTESIAN_POINT ( 'NONE',  ( 176.3506576600417191, 270.0042805746620616, -16.66995943565067861 ) ) ;
#64724 = CARTESIAN_POINT ( 'NONE',  ( 37.50591675755416077, 22.44966523072497111, -2.296566073217252530E-15 ) ) ;
#64725 = LINE ( 'NONE', #26221, #87200 ) ;
#64726 = CARTESIAN_POINT ( 'NONE',  ( -3.869528910404237632, 180.1199935810941781, 2.679491924311264039 ) ) ;
#64727 = ORIENTED_EDGE ( 'NONE', *, *, #86807, .F. ) ;
#64728 = CARTESIAN_POINT ( 'NONE',  ( 17.84595736030643920, 25.70171378149918340, -9.188101187500004485 ) ) ;
#64729 = CARTESIAN_POINT ( 'NONE',  ( 82.23173768200972233, 206.0327760586659451, 1.948934522072302763E-15 ) ) ;
#64730 = CARTESIAN_POINT ( 'NONE',  ( 38.52196584993465223, 56.41980893122115504, -10.00000000000000000 ) ) ;
#64731 = CYLINDRICAL_SURFACE ( 'NONE', #40980, 12.49999999999999645 ) ;
#64732 = CARTESIAN_POINT ( 'NONE',  ( -30.35047437581953034, 93.97944682170771102, 12.14429053135152792 ) ) ;
#64733 = DIRECTION ( 'NONE',  ( -0.000000000000000000, 0.000000000000000000, 1.000000000000000000 ) ) ;
#64734 = ORIENTED_EDGE ( 'NONE', *, *, #44332, .F. ) ;
#64735 = FACE_OUTER_BOUND ( 'NONE', #48155, .T. ) ;
#64736 = CARTESIAN_POINT ( 'NONE',  ( 192.8985195491038098, 288.1185855829259594, 16.03958602435291780 ) ) ;
#64737 = CARTESIAN_POINT ( 'NONE',  ( 72.50277233665612187, 71.58711300884623085, 5.243368462525016760 ) ) ;
#64738 = CARTESIAN_POINT ( 'NONE',  ( 120.4718248238752523, 250.3615022471903444, 5.000000000000046185 ) ) ;
#64739 = CARTESIAN_POINT ( 'NONE',  ( 42.14088959202413776, 24.73415679381825782, -6.890680421881970419E-14 ) ) ;
#64740 = ADVANCED_FACE ( 'NONE', ( #28000 ), #74633, .F. ) ;
#64741 = FACE_OUTER_BOUND ( 'NONE', #6105, .T. ) ;
#64742 = ORIENTED_EDGE ( 'NONE', *, *, #65508, .F. ) ;
#64743 = CARTESIAN_POINT ( 'NONE',  ( 165.6937111782763452, 246.6359652278159160, -1.301814763765337224 ) ) ;
#64744 = ORIENTED_EDGE ( 'NONE', *, *, #100085, .T. ) ;
#64745 = CARTESIAN_POINT ( 'NONE',  ( 202.3139361598622372, 280.2289788223093865, 15.93832709035092421 ) ) ;
#64746 = CARTESIAN_POINT ( 'NONE',  ( 207.4413961551520913, 270.9595189787718255, -0.9988337982141689553 ) ) ;
#64747 = CARTESIAN_POINT ( 'NONE',  ( 72.82541052025236183, 57.63392727407249083, -16.30571033187239749 ) ) ;
#64748 = ORIENTED_EDGE ( 'NONE', *, *, #26317, .F. ) ;
#64750 = EDGE_CURVE ( 'NONE', #83009, #46531, #26018, .T. ) ;
#64749 = DIRECTION ( 'NONE',  ( -0.9481851146622203297, -0.3177184104407421716, 0.000000000000000000 ) ) ;
#64751 = ORIENTED_EDGE ( 'NONE', *, *, #53947, .T. ) ;
#64753 = ADVANCED_FACE ( 'NONE', ( #45672 ), #66504, .T. ) ;
#64752 = CARTESIAN_POINT ( 'NONE',  ( 72.11862359525288468, 71.68643115293319568, 5.491312638656038025 ) ) ;
#64754 = CARTESIAN_POINT ( 'NONE',  ( 170.5847424161334800, 250.4031697645958729, 3.399405397972957488 ) ) ;
#64755 = CARTESIAN_POINT ( 'NONE',  ( 191.7451945007296956, 296.7399137238037952, -11.83242997637808713 ) ) ;
#64756 = ORIENTED_EDGE ( 'NONE', *, *, #41666, .F. ) ;
#64757 = EDGE_CURVE ( 'NONE', #50323, #34720, #59701, .T. ) ;
#64758 = CARTESIAN_POINT ( 'NONE',  ( 25.47001115121704373, 36.74646525600391556, 2.839279412974139660 ) ) ;
#64759 = FACE_OUTER_BOUND ( 'NONE', #13545, .T. ) ;
#64760 = LINE ( 'NONE', #96189, #72481 ) ;
#64761 = CARTESIAN_POINT ( 'NONE',  ( -0.8836234265189104597, 25.35879081310345029, -10.00000000000000000 ) ) ;
#64762 = ORIENTED_EDGE ( 'NONE', *, *, #89319, .T. ) ;
#64763 = ORIENTED_EDGE ( 'NONE', *, *, #92202, .F. ) ;
#64764 = CARTESIAN_POINT ( 'NONE',  ( 183.4383719652804530, 295.9431572655629452, 1.012549917523295040 ) ) ;
#64766 = CARTESIAN_POINT ( 'NONE',  ( 194.9455394410084921, 292.9914163096879065, -15.01116663483170655 ) ) ;
#64765 = CARTESIAN_POINT ( 'NONE',  ( 68.21627857846966947, 65.89183038565549566, 10.81150700775086371 ) ) ;
#64767 = CARTESIAN_POINT ( 'NONE',  ( 85.32371827457656366, 48.49939495466653483, 12.43282873216696593 ) ) ;
#64768 = CARTESIAN_POINT ( 'NONE',  ( 193.8365934467825298, 294.9121671145370556, 14.14845633038902584 ) ) ;
#64769 = CARTESIAN_POINT ( 'NONE',  ( 162.5148320529283126, 285.2034568178174254, 0.5437328601018158736 ) ) ;
#64770 = CARTESIAN_POINT ( 'NONE',  ( 169.6258775464486632, 274.3344629316208056, -17.15914146219304115 ) ) ;
#64771 = CARTESIAN_POINT ( 'NONE',  ( 164.3630144314164170, 245.9619034500468331, 5.823830253651713029 ) ) ;
#64772 = VECTOR ( 'NONE', #84895, 1000.000000000000000 ) ;
#64773 = CARTESIAN_POINT ( 'NONE',  ( 166.1457379652601105, 265.4834180535647761, 16.56432196572769300 ) ) ;
#64774 = CARTESIAN_POINT ( 'NONE',  ( 79.58936028502597537, 59.22294857574252802, 16.56770033466462166 ) ) ;
#64775 = CARTESIAN_POINT ( 'NONE',  ( 88.99704050542813150, 228.3149278399160664, 9.188101187500093303 ) ) ;
#64776 = ORIENTED_EDGE ( 'NONE', *, *, #8245, .F. ) ;
#64777 = CARTESIAN_POINT ( 'NONE',  ( 74.06977354252758516, 55.65288952014064705, -16.58740917872301068 ) ) ;
#64778 = DIRECTION ( 'NONE',  ( 0.000000000000000000, 0.000000000000000000, 1.000000000000000000 ) ) ;
#64779 = CARTESIAN_POINT ( 'NONE',  ( 166.2783657372584116, 279.3061210340277398, -13.84400717950042470 ) ) ;
#64780 = VERTEX_POINT ( 'NONE', #67492 ) ;
#64781 = B_SPLINE_CURVE_WITH_KNOTS ( 'NONE', 3,
 ( #75291, #20588, #85277, #46209 ),
 .UNSPECIFIED., .F., .F.,
 ( 4, 4 ),
 ( 0.004610365127728928078, 0.009594302975941142869 ),
 .UNSPECIFIED. ) ;
#64782 = ORIENTED_EDGE ( 'NONE', *, *, #39277, .F. ) ;
#64783 = CARTESIAN_POINT ( 'NONE',  ( 79.91676478670554218, 44.69584264316313948, -11.20854373491701139 ) ) ;
#64784 = CARTESIAN_POINT ( 'NONE',  ( 146.8637854207107409, 276.2714571898724216, 0.7988785540157756770 ) ) ;
#64785 = CARTESIAN_POINT ( 'NONE',  ( 155.8152618860606253, 260.7670451491295012, 0.000000000000000000 ) ) ;
#64786 = CARTESIAN_POINT ( 'NONE',  ( 159.9770824720811220, 253.5585604421560788, -16.42166711341322483 ) ) ;
#64787 = LINE ( 'NONE', #96215, #26918 ) ;
#64788 = CARTESIAN_POINT ( 'NONE',  ( 90.37718171876834106, 232.1744531367911293, 4.594050593750047540 ) ) ;
#64789 = VERTEX_POINT ( 'NONE', #97917 ) ;
#64790 = ORIENTED_EDGE ( 'NONE', *, *, #91401, .F. ) ;
#64791 = CARTESIAN_POINT ( 'NONE',  ( 45.11483101423404918, 69.99284853207299761, 10.00000000000000000 ) ) ;
#64792 = CARTESIAN_POINT ( 'NONE',  ( 162.6396274730868186, 248.9468972229755082, -10.26162218571527518 ) ) ;
#64793 = EDGE_LOOP ( 'NONE', ( #12832, #52288, #99751, #60874, #11058, #7822, #72126, #96066, #31819, #13543, #73034, #25278, #30620, #68213, #31591, #97550, #9281, #71627, #75883, #92918 ) ) ;
#64794 = ADVANCED_FACE ( 'NONE', ( #82754 ), #12831, .F. ) ;
#64795 = CARTESIAN_POINT ( 'NONE',  ( 22.57022264052298155, 36.52903772873359145, -1.583844403245329602 ) ) ;
#64796 = DIRECTION ( 'NONE',  ( -0.8660254037844387076, -0.4999999999999998890, -0.000000000000000000 ) ) ;
#64798 = DIRECTION ( 'NONE',  ( 0.000000000000000000, -0.000000000000000000, 1.000000000000000000 ) ) ;
#64797 = CARTESIAN_POINT ( 'NONE',  ( 134.2197177853555843, 257.4869531367911577, 4.594050593750046652 ) ) ;
#64799 = CARTESIAN_POINT ( 'NONE',  ( -2.305318362028928370, 156.1427522451417644, 1.119607411625061291E-15 ) ) ;
#64800 = CARTESIAN_POINT ( 'NONE',  ( 87.88540012852695327, 44.32205958948441094, 4.765779035299132715 ) ) ;
#64801 = VERTEX_POINT ( 'NONE', #83737 ) ;
#64802 = CARTESIAN_POINT ( 'NONE',  ( 156.7423333928520890, 259.1613101971172455, 17.21575223094429319 ) ) ;
#64803 = CARTESIAN_POINT ( 'NONE',  ( 81.06532563505241740, 46.71245566778327429, 12.32994159712216842 ) ) ;
#64804 = CARTESIAN_POINT ( 'NONE',  ( -12.95261720355844126, 24.63757726406876714, -10.00000000000000000 ) ) ;
#64805 = CARTESIAN_POINT ( 'NONE',  ( 149.7854447168632817, 277.1467554076948545, 4.663160563959508842 ) ) ;
#64806 = DIRECTION ( 'NONE',  ( -0.8660254037844387076, -0.4999999999999998890, -0.000000000000000000 ) ) ;
#64807 = DIRECTION ( 'NONE',  ( 1.000000000000000000, -4.068174368805037318E-13, 0.000000000000000000 ) ) ;
#64808 = LINE ( 'NONE', #55179, #93958 ) ;
#64809 = CARTESIAN_POINT ( 'NONE',  ( 66.16250339235085676, 220.5530062829863027, -4.648177544792955347E-16 ) ) ;
#64810 = CARTESIAN_POINT ( 'NONE',  ( 161.8289209813647176, 250.3510820566641257, 13.28523796267037937 ) ) ;
#64811 = CARTESIAN_POINT ( 'NONE',  ( 85.45558807839536541, 44.20360693575860012, 6.623748629729414361 ) ) ;
#64812 = CARTESIAN_POINT ( 'NONE',  ( 195.2495212664957194, 275.1290853193528392, -16.26662379558266380 ) ) ;
#64813 = CARTESIAN_POINT ( 'NONE',  ( 78.30955769916529619, 61.43963167811125459, 15.82323565659766018 ) ) ;
#64814 = DIRECTION ( 'NONE',  ( -0.8660254037844377084, -0.5000000000000014433, -0.000000000000000000 ) ) ;
#64815 = CARTESIAN_POINT ( 'NONE',  ( 202.2123796483002138, 280.4048798601741623, -15.85247869902013740 ) ) ;
#64816 = EDGE_CURVE ( 'NONE', #22997, #81391, #75122, .T. ) ;
#64817 = CARTESIAN_POINT ( 'NONE',  ( 75.94935831335567400, 63.33535154278327184, -14.87782447488597626 ) ) ;
#64819 = CARTESIAN_POINT ( 'NONE',  ( 185.3509297750883889, 266.4368487342368326, 13.13595510978240277 ) ) ;
#64818 = CARTESIAN_POINT ( 'NONE',  ( 180.4828997427432569, 266.7556949304461682, -14.76840115687851274 ) ) ;
#64820 = CARTESIAN_POINT ( 'NONE',  ( 79.86382474383562169, 55.95619954358613057, 16.50767179695137798 ) ) ;
#64821 = EDGE_CURVE ( 'NONE', #43030, #12312, #5697, .T. ) ;
#64822 = CARTESIAN_POINT ( 'NONE',  ( 36.87552185948406702, 26.45404122711136097, -8.090169943749478065 ) ) ;
#64823 = DIRECTION ( 'NONE',  ( 0.8660254037844390407, 0.4999999999999993339, 0.000000000000000000 ) ) ;
#64824 = CARTESIAN_POINT ( 'NONE',  ( -42.47074677134370546, 28.21475011077167849, -10.00000000000000000 ) ) ;
#64825 = CARTESIAN_POINT ( 'NONE',  ( 181.5682298158554602, 273.5681932549885573, 17.67500197916986693 ) ) ;
#64826 = CARTESIAN_POINT ( 'NONE',  ( 157.8797407370935559, 271.1684435876110228, -14.71067124673816018 ) ) ;
#64827 = CARTESIAN_POINT ( 'NONE',  ( 84.37266873162100467, 43.31764817757444064, -6.019247367396705961 ) ) ;
#64828 = EDGE_CURVE ( 'NONE', #49424, #51013, #29496, .T. ) ;
#64829 = CARTESIAN_POINT ( 'NONE',  ( 13.11156449881669595, 184.5024278399160949, -9.188101187500093303 ) ) ;
#64830 = FACE_OUTER_BOUND ( 'NONE', #96217, .T. ) ;
#64831 = ORIENTED_EDGE ( 'NONE', *, *, #5762, .F. ) ;
#64833 = CARTESIAN_POINT ( 'NONE',  ( 86.92045001522136261, 45.99340221249899940, 8.966174604352282529 ) ) ;
#64832 = B_SPLINE_CURVE_WITH_KNOTS ( 'NONE', 3,
 ( #86786, #95391, #40106, #31508, #47706, #24427, #70012, #78139, #85792, #628, #16819, #93359, #70518, #32010, #54815, #71545 ),
 .UNSPECIFIED., .F., .F.,
 ( 4, 2, 2, 2, 2, 2, 2, 4 ),
 ( 1.190910092370080074E-16, 0.0003787177898467455569, 0.0007574355796933719600, 0.001136153369539998634, 0.001514871159386624875, 0.001893588949233251332, 0.002272306739079878440, 0.003029742318773052424 ),
 .UNSPECIFIED. ) ;
#64834 = CARTESIAN_POINT ( 'NONE',  ( 204.3165321041017251, 270.7059293579960126, 8.545054412317711012 ) ) ;
#64835 = CARTESIAN_POINT ( 'NONE',  ( 71.91251904240313308, 72.63095699448832931, -0.6620033135626105514 ) ) ;
#64836 = CARTESIAN_POINT ( 'NONE',  ( 27.26558041797736465, 195.7369531367911293, -4.594050593750048428 ) ) ;
#64837 = CARTESIAN_POINT ( 'NONE',  ( 200.8769374536528858, 282.7179335918746688, 17.26928237494566787 ) ) ;
#64838 = CARTESIAN_POINT ( 'NONE',  ( 190.1635032421960148, 301.2741459696644029, -5.047660290019184259 ) ) ;
#64839 = CARTESIAN_POINT ( 'NONE',  ( 33.00035307926291495, 37.79103043416552055, 8.090169943749478065 ) ) ;
#64840 = CARTESIAN_POINT ( 'NONE',  ( 177.9038217119459091, 292.6972127826384735, 5.767030569036280419 ) ) ;
#64841 = CARTESIAN_POINT ( 'NONE',  ( 178.6854534826287022, 293.3287072856790587, 2.638351066326640737 ) ) ;
#64842 = CARTESIAN_POINT ( 'NONE',  ( 181.8955405286666860, 279.8176704957666630, -16.10530862137905928 ) ) ;
#64843 = CARTESIAN_POINT ( 'NONE',  ( 81.38228331512368641, 42.18052851754683275, 8.075145019496556387 ) ) ;
#64844 = CARTESIAN_POINT ( 'NONE',  ( 166.7371348775683941, 257.8943008475421834, -15.20426139718983194 ) ) ;
#64845 = LINE ( 'NONE', #32931, #85721 ) ;
#64846 = VECTOR ( 'NONE', #98401, 1000.000000000000000 ) ;
#64847 = LINE ( 'NONE', #16736, #28412 ) ;
#64848 = CARTESIAN_POINT ( 'NONE',  ( 90.23310447506868570, 216.2365022471902023, -10.00000000000009059 ) ) ;
#64849 = CARTESIAN_POINT ( 'NONE',  ( 18.28082717731156848, 171.3615022471901739, 5.000000000000051514 ) ) ;
#64850 = EDGE_CURVE ( 'NONE', #47527, #48040, #33937, .T. ) ;
#64851 = CARTESIAN_POINT ( 'NONE',  ( -54.35768244943842120, 45.75294371086302903, 59.99999999999999289 ) ) ;
#64852 = CARTESIAN_POINT ( 'NONE',  ( 46.56179571999062716, 203.8149278399160949, -9.188101187500095079 ) ) ;
#64853 = CARTESIAN_POINT ( 'NONE',  ( 198.0858447170796524, 287.5522480202560018, 18.44384186289807559 ) ) ;
#64854 = ORIENTED_EDGE ( 'NONE', *, *, #39768, .F. ) ;
#64855 = CARTESIAN_POINT ( 'NONE',  ( -17.48682250002296712, 81.73217073256289211, 14.51763226715314126 ) ) ;
#64856 = LINE ( 'NONE', #33450, #12580 ) ;
#64857 = CARTESIAN_POINT ( 'NONE',  ( 67.38972849331132409, 66.71699885800039453, -8.459198425301941882 ) ) ;
#64858 = ORIENTED_EDGE ( 'NONE', *, *, #66198, .T. ) ;
#64859 = CARTESIAN_POINT ( 'NONE',  ( 171.2389088083422166, 286.7460130492871713, 8.408771775780483182 ) ) ;
#64860 = CARTESIAN_POINT ( 'NONE',  ( 164.2600772519394923, 246.1401958748887182, -2.110785484364219311 ) ) ;
#64861 = LINE ( 'NONE', #3086, #68713 ) ;
#64862 = CARTESIAN_POINT ( 'NONE',  ( 85.33606590682254023, 45.99036976515365183, -10.09305720521511596 ) ) ;
#64863 = CARTESIAN_POINT ( 'NONE',  ( 23.73796034364816521, 35.74646525600390845, 2.839279412974139660 ) ) ;
#64864 = CARTESIAN_POINT ( 'NONE',  ( 162.7561251957091031, 248.7451172484279027, 11.07313294959361194 ) ) ;
#64865 = CARTESIAN_POINT ( 'NONE',  ( 148.9285945872975390, 272.6951028054104427, -12.01265727652413240 ) ) ;
#64866 = CARTESIAN_POINT ( 'NONE',  ( 156.9652392049574132, 258.7752260052484985, 18.40175728539550448 ) ) ;
#64867 = VERTEX_POINT ( 'NONE', #22393 ) ;
#64868 = CARTESIAN_POINT ( 'NONE',  ( 17.58072690530697813, 12.01110640527291373, 2.839279412974134775 ) ) ;
#64869 = DIRECTION ( 'NONE',  ( -0.000000000000000000, -1.000000000000000000, -0.000000000000000000 ) ) ;
#64870 = CARTESIAN_POINT ( 'NONE',  ( -56.29836151245349640, 34.88994676555962116, 10.00000000000000000 ) ) ;
#64871 = CARTESIAN_POINT ( 'NONE',  ( 71.67936538144843439, 72.44724869688445779, -1.358217801655851931 ) ) ;
#64872 = EDGE_CURVE ( 'NONE', #77711, #3380, #20324, .T. ) ;
#64873 = VERTEX_POINT ( 'NONE', #37091 ) ;
#64874 = CARTESIAN_POINT ( 'NONE',  ( 72.09555114463066161, 71.52603334931079360, -5.842164467371243397 ) ) ;
#64875 = CARTESIAN_POINT ( 'NONE',  ( 190.9907605556751093, 299.8412942717858414, 8.799173206188184437 ) ) ;
#64876 = FACE_OUTER_BOUND ( 'NONE', #84585, .T. ) ;
#64877 = FACE_OUTER_BOUND ( 'NONE', #28477, .T. ) ;
#64878 = ORIENTED_EDGE ( 'NONE', *, *, #57486, .T. ) ;
#64879 = ORIENTED_EDGE ( 'NONE', *, *, #75707, .T. ) ;
#64881 = CARTESIAN_POINT ( 'NONE',  ( 150.9309360722972428, 269.7956109838555108, -13.68607459661258297 ) ) ;
#64880 = CARTESIAN_POINT ( 'NONE',  ( 161.2488013048736377, 251.3558788108169040, -13.10044423494716170 ) ) ;
#64882 = CARTESIAN_POINT ( 'NONE',  ( 204.8523313866422484, 275.8323493198358847, 14.65426965484541100 ) ) ;
#64883 = EDGE_LOOP ( 'NONE', ( #25787, #96049, #87373, #82352 ) ) ;
#64884 = CARTESIAN_POINT ( 'NONE',  ( 37.05984716305037807, 40.13478043621391578, 8.090169943749478065 ) ) ;
#64885 = CARTESIAN_POINT ( 'NONE',  ( 159.7608930362198407, 253.9330115291272421, 15.38895778945778581 ) ) ;
#64886 = CARTESIAN_POINT ( 'NONE',  ( 72.72170611769777793, 57.01385831347377575, -15.91061902151446183 ) ) ;
#64887 = CARTESIAN_POINT ( 'NONE',  ( 78.33567785457334764, 61.58246172053951994, -15.80486485196054858 ) ) ;
#64888 = CARTESIAN_POINT ( 'NONE',  ( 204.8878784573704195, 275.7707799872745795, -14.13380496213581594 ) ) ;
#64889 = CARTESIAN_POINT ( 'NONE',  ( 120.4179585561885659, 231.1423013555409796, -4.594050593750043987 ) ) ;
#64890 = EDGE_CURVE ( 'NONE', #63648, #22887, #25581, .T. ) ;
#64891 = CARTESIAN_POINT ( 'NONE',  ( 79.60625107924913380, 226.7677522451419350, -5.000000000000047962 ) ) ;
#64892 = VERTEX_POINT ( 'NONE', #68982 ) ;
#64893 = CARTESIAN_POINT ( 'NONE',  ( 207.8302079587528794, 270.6745157982714431, 3.572475529330238153 ) ) ;
#64894 = VERTEX_POINT ( 'NONE', #39065 ) ;
#64895 = CARTESIAN_POINT ( 'NONE',  ( 30.49295849316677831, 39.64646525600392835, -2.839279412974133887 ) ) ;
#64896 = CARTESIAN_POINT ( 'NONE',  ( 157.4627203480516755, 258.4629190429250798, 16.86169483958236626 ) ) ;
#64897 = CARTESIAN_POINT ( 'NONE',  ( 78.45009037299155352, 47.91390430630379171, -14.50880498950433761 ) ) ;
#64898 = CARTESIAN_POINT ( 'NONE',  ( 61.77188751760235874, 194.2202760586659167, -5.415160957724236172E-17 ) ) ;
#64899 = CARTESIAN_POINT ( 'NONE',  ( 74.04232911944542650, 68.62205345152153768, 11.42009053252771800 ) ) ;
#64900 = CARTESIAN_POINT ( 'NONE',  ( 151.2648146047323507, 268.6486510375538614, 15.71323890031163550 ) ) ;
#64901 = CARTESIAN_POINT ( 'NONE',  ( 150.7471914551857708, 269.5452006317422047, 15.29409085476701691 ) ) ;
#64902 = CARTESIAN_POINT ( 'NONE',  ( 44.44706364856357084, 64.93738052781135650, -10.00000000000000000 ) ) ;
#64903 = ORIENTED_EDGE ( 'NONE', *, *, #35547, .T. ) ;
#64904 = DIRECTION ( 'NONE',  ( 0.9994538543569184696, -0.03304531753667278721, 0.000000000000000000 ) ) ;
#64905 = CARTESIAN_POINT ( 'NONE',  ( 83.75393680008980368, 42.85305525622027290, -5.701475753897882193 ) ) ;
#64906 = CARTESIAN_POINT ( 'NONE',  ( 174.3506819931331506, 286.9267872025895940, 11.76311152586403885 ) ) ;
#64907 = VERTEX_POINT ( 'NONE', #24394 ) ;
#64908 = CARTESIAN_POINT ( 'NONE',  ( 174.0105655393888355, 260.7770664459772547, -13.96503775365264133 ) ) ;
#64909 = CARTESIAN_POINT ( 'NONE',  ( 67.14771890113766517, 69.04852796021181405, -2.906451251998301011 ) ) ;
#64910 = ADVANCED_FACE ( 'NONE', ( #54780, #77086, #55760 ), #55268, .F. ) ;
#64911 = CARTESIAN_POINT ( 'NONE',  ( 161.5757715694810770, 250.7895496999525449, -14.51803553215175135 ) ) ;
#64912 = CARTESIAN_POINT ( 'NONE',  ( 78.57703514963246505, 53.48924796936273651, -16.27616477978846277 ) ) ;
#64913 = CARTESIAN_POINT ( 'NONE',  ( 190.6023073677431512, 300.5141149296460981, 3.174888932019753973 ) ) ;
#64914 = DIRECTION ( 'NONE',  ( 0.9979227057047517224, -0.06442261589618512863, 0.000000000000000000 ) ) ;
#64915 = CARTESIAN_POINT ( 'NONE',  ( 164.6869624841032191, 245.4008089637804346, 1.435659848726088317 ) ) ;
#64916 = FACE_OUTER_BOUND ( 'NONE', #75260, .T. ) ;
#64917 = CARTESIAN_POINT ( 'NONE',  ( 153.8464967062441815, 264.7140010578719398, -16.51288510356084061 ) ) ;
#64918 = CARTESIAN_POINT ( 'NONE',  ( 164.0854748117396582, 246.4426161724408928, -5.757837433625331514 ) ) ;
#64919 = B_SPLINE_CURVE_WITH_KNOTS ( 'NONE', 3,
 ( #6129, #14236, #76059, #37513, #7621, #92277, #29926, #22824, #15207, #46102, #78542, #48638, #10131, #71940, #79063, #63322, #77544, #62302, #62815, #79572, #2544, #39496, #85166, #24329, #94263, #86682, #47615, #55693, #33427, #71442, #40999, #40000, #46612, #2030, #94757, #23814, #24818, #55205, #93259, #15711, #70422, #86186, #25320, #40508, #56207, #48120, #8134, #54706, #16723, #39007 ),
 .UNSPECIFIED., .F., .F.,
 ( 4, 2, 2, 2, 2, 2, 2, 2, 2, 2, 2, 2, 2, 2, 2, 2, 2, 2, 2, 2, 2, 2, 2, 2, 4 ),
 ( 0.001230839774562330572, 0.001705398597812425978, 0.002179957421062521383, 0.002417236832687631645, 0.002535876538500167043, 0.002654516244312702007, 0.002773155950125237405, 0.002891795655937772803, 0.003129075067562843600, 0.003603633890813042005, 0.004078192714063240409, 0.005027310360563775130, 0.005976428007064311584, 0.006450986830314656140, 0.006925545653565000695, 0.007044185359377666197, 0.007103505212284000683, 0.007162825065190333435, 0.007281464771003024958, 0.007400104476815714746, 0.007637383888441099528, 0.007874663300066486044, 0.008111942711691870825, 0.008349222123317257341, 0.008823780946568158742 ),
 .UNSPECIFIED. ) ;
#64920 = CARTESIAN_POINT ( 'NONE',  ( 131.9199452241419124, 234.7202760586659736, -5.415160957724236172E-17 ) ) ;
#64921 = EDGE_LOOP ( 'NONE', ( #81491, #25498, #6174, #58742 ) ) ;
#64922 = CARTESIAN_POINT ( 'NONE',  ( 84.43795724362087185, 44.16455098980025440, -7.553542188705723248 ) ) ;
#64923 = CARTESIAN_POINT ( 'NONE',  ( -19.53260179278070652, 92.99029561550555911, 59.99999999999999289 ) ) ;
#64924 = CARTESIAN_POINT ( 'NONE',  ( 203.1044072055706806, 278.8598428092302584, -16.67109798570195878 ) ) ;
#64925 = CARTESIAN_POINT ( 'NONE',  ( 204.9004517216375518, 275.7490024547470853, 14.55104398969427670 ) ) ;
#64926 = CARTESIAN_POINT ( 'NONE',  ( -10.20233967203003544, 176.4637435831425023, 2.679491924311251605 ) ) ;
#64927 = VECTOR ( 'NONE', #54867, 1000.000000000000114 ) ;
#64928 = CARTESIAN_POINT ( 'NONE',  ( 76.29477762951383113, 51.62420456488434439, -15.67837010211920301 ) ) ;
#64929 = ORIENTED_EDGE ( 'NONE', *, *, #50443, .F. ) ;
#64930 = CARTESIAN_POINT ( 'NONE',  ( 80.51866135781378375, 57.13713896268047421, -16.22916027019209650 ) ) ;
#64931 = B_SPLINE_CURVE_WITH_KNOTS ( 'NONE', 3,
 ( #3244, #34127, #18432, #9319 ),
 .UNSPECIFIED., .F., .F.,
 ( 4, 4 ),
 ( 0.01260167760416553567, 0.01881583619385329004 ),
 .UNSPECIFIED. ) ;
#64932 = CARTESIAN_POINT ( 'NONE',  ( 158.0556171945634674, 275.8819595179413682, -12.51247609328395782 ) ) ;
#64934 = CARTESIAN_POINT ( 'NONE',  ( 185.7731237309448034, 262.0522970092281980, 9.834746716364003660 ) ) ;
#64933 = CARTESIAN_POINT ( 'NONE',  ( 147.7395812515338491, 275.4447818272566337, 3.760927250875937489 ) ) ;
#64935 = CARTESIAN_POINT ( 'NONE',  ( 157.8501323257721083, 280.8042112442767007, -7.123878780571343050 ) ) ;
#64936 = CARTESIAN_POINT ( 'NONE',  ( 135.7624123097878623, 255.3149278399160949, 9.188101187500093303 ) ) ;
#64937 = CARTESIAN_POINT ( 'NONE',  ( 23.90999230191038549, 184.6115022471902591, 10.00000000000009592 ) ) ;
#64938 = CARTESIAN_POINT ( 'NONE',  ( -29.41917662106829212, 23.74964416229700248, 10.00000000000000000 ) ) ;
#64939 = CARTESIAN_POINT ( 'NONE',  ( 71.35211999908521818, 205.8768266524160140, 9.188101187500098632 ) ) ;
#64940 = CARTESIAN_POINT ( 'NONE',  ( 174.5577213332984456, 251.6462513678240498, 3.602869039157936104 ) ) ;
#64941 = EDGE_CURVE ( 'NONE', #4560, #22737, #591, .T. ) ;
#64942 = CARTESIAN_POINT ( 'NONE',  ( 17.63446822084836896, 18.38052372038639959, 10.00000000000000533 ) ) ;
#64943 = CARTESIAN_POINT ( 'NONE',  ( 148.9694607950094394, 272.6243204573405592, 11.81236034532910573 ) ) ;
#64944 = CARTESIAN_POINT ( 'NONE',  ( 155.4130510163440988, 279.6938839982619811, -1.521710589521471535 ) ) ;
#64945 = CARTESIAN_POINT ( 'NONE',  ( 171.1527898587758045, 287.5703274966900835, -8.623511503197541117 ) ) ;
#64946 = CARTESIAN_POINT ( 'NONE',  ( 155.2193237801463113, 261.7992402267395846, -18.58295809893692407 ) ) ;
#64947 = EDGE_CURVE ( 'NONE', #30618, #76229, #13787, .T. ) ;
#64948 = CARTESIAN_POINT ( 'NONE',  ( 194.6028008291465881, 289.1389010384484664, 16.14037336114297361 ) ) ;
#64949 = CARTESIAN_POINT ( 'NONE',  ( 122.5466773502275544, 254.8927522451419634, 2.944929066748280225E-16 ) ) ;
#64950 = EDGE_CURVE ( 'NONE', #89630, #77668, #96102, .T. ) ;
#64951 = CARTESIAN_POINT ( 'NONE',  ( 81.07596274759146127, 51.75087684323265336, -15.00964593992177676 ) ) ;
#64952 = ORIENTED_EDGE ( 'NONE', *, *, #87124, .T. ) ;
#64953 = EDGE_CURVE ( 'NONE', #23257, #26637, #71513, .T. ) ;
#64954 = CARTESIAN_POINT ( 'NONE',  ( 66.74069431502459793, 67.35994133444863508, -6.833594717235060401 ) ) ;
#64955 = CARTESIAN_POINT ( 'NONE',  ( 147.6220714307702622, 274.9580672937808572, 8.392894244419288441 ) ) ;
#64956 = CARTESIAN_POINT ( 'NONE',  ( -4.614459115189767147, 158.9548013555409796, -4.594050593750042211 ) ) ;
#64957 = CARTESIAN_POINT ( 'NONE',  ( 34.76219959342768107, 197.0024278399161233, 9.188101187500095079 ) ) ;
#64958 = CARTESIAN_POINT ( 'NONE',  ( 175.6508819106952615, 256.4707162311754587, -10.98076396042754155 ) ) ;
#64959 = CARTESIAN_POINT ( 'NONE',  ( 13.51707852204697069, 30.73705186507753240, -3.090169943749475845 ) ) ;
#64960 = DIRECTION ( 'NONE',  ( -0.6623377501714527993, 0.7492053821868994712, 0.000000000000000000 ) ) ;
#64961 = CARTESIAN_POINT ( 'NONE',  ( 185.8492146212669240, 258.6745004276652935, -5.862532207920108540 ) ) ;
#64962 = CARTESIAN_POINT ( 'NONE',  ( 192.4867222293441387, 292.6075778101206879, -14.23530027676960863 ) ) ;
#64963 = CARTESIAN_POINT ( 'NONE',  ( 190.9441801652054096, 299.9219738747156043, -4.765040093794296716 ) ) ;
#64964 = CARTESIAN_POINT ( 'NONE',  ( 73.74547311384563386, 55.26076647750536353, -16.59506521500572518 ) ) ;
#64966 = CARTESIAN_POINT ( 'NONE',  ( 65.38900070045468738, 201.8927522451418213, -10.00000000000009059 ) ) ;
#64965 = CARTESIAN_POINT ( 'NONE',  ( 167.5258143496386367, 256.6353381695413987, 13.78324095373011104 ) ) ;
#64967 = CARTESIAN_POINT ( 'NONE',  ( 163.0331642552320659, 256.4053458108576251, -15.77289028494504031 ) ) ;
#64968 = CARTESIAN_POINT ( 'NONE',  ( 205.0716081116550527, 275.4525508911965517, -12.57761053684872188 ) ) ;
#64969 = CARTESIAN_POINT ( 'NONE',  ( 162.1559275291031099, 252.0210818530713652, -13.25156758742917518 ) ) ;
#64970 =( BOUNDED_CURVE ( )  B_SPLINE_CURVE ( 2, ( #83903, #52452, #68648, #36751, #23033, #29173, #14465, #30151, #38739 ),
 .UNSPECIFIED., .F., .T. ) 
 B_SPLINE_CURVE_WITH_KNOTS ( ( 3, 2, 2, 2, 3 ),
 ( 0.06854838709677418818, 0.06989247311827956333, 0.07258064516129032751, 0.07526881720430107781, 0.07661290322580645296 ),
 .UNSPECIFIED. ) 
 CURVE ( )  GEOMETRIC_REPRESENTATION_ITEM ( )  RATIONAL_B_SPLINE_CURVE ( ( 0.9330127018922194093, 0.9330127018922194093, 1.000000000000000000, 0.8660254037844387076, 1.000000000000000000, 0.8660254037844387076, 1.000000000000000000, 0.9330127018922194093, 0.9330127018922194093 ) ) 
 REPRESENTATION_ITEM ( '' )  );
#64971 = CARTESIAN_POINT ( 'NONE',  ( 31.70422093597028734, 199.1115022471903160, -5.000000000000047962 ) ) ;
#64972 = CARTESIAN_POINT ( 'NONE',  ( 169.9469112398214747, 250.9785751410766750, -8.718312767540300712 ) ) ;
#64973 = LINE ( 'NONE', #42151, #87102 ) ;
#64974 = CARTESIAN_POINT ( 'NONE',  ( 14.68175618682350780, 167.0327760586659451, 1.948934522072303157E-15 ) ) ;
#64975 = CARTESIAN_POINT ( 'NONE',  ( 35.16646543599519248, 35.70171378149922248, -9.188101187500004485 ) ) ;
#64976 = CARTESIAN_POINT ( 'NONE',  ( 164.1042149987925427, 252.5458357570947783, 13.30367259394180479 ) ) ;
#64977 = CARTESIAN_POINT ( 'NONE',  ( 192.1149248854976861, 297.8941845364767005, 12.26771790733441314 ) ) ;
#64978 = CARTESIAN_POINT ( 'NONE',  ( 30.58134869734400851, 35.84336893147758474, -7.433330006724137462 ) ) ;
#64979 = CARTESIAN_POINT ( 'NONE',  ( 206.5280879940269756, 272.9298537347264642, 11.21709153681466731 ) ) ;
#64980 = CARTESIAN_POINT ( 'NONE',  ( 164.9779129355220562, 244.8968679994381148, -1.771286574179712803 ) ) ;
#64981 = FACE_OUTER_BOUND ( 'NONE', #57624, .T. ) ;
#64982 = CARTESIAN_POINT ( 'NONE',  ( 34.30168821287347924, 42.73705186507756792, -3.090169943749475845 ) ) ;
#64983 = CARTESIAN_POINT ( 'NONE',  ( -17.42236680055705023, 149.2012482093457777, 0.000000000000000000 ) ) ;
#64984 = CARTESIAN_POINT ( 'NONE',  ( 10.98031343905817714, 14.84335787977761001, 9.188101187500006262 ) ) ;
#64985 = CARTESIAN_POINT ( 'NONE',  ( 168.7862764537476608, 288.1668982680979525, 0.5246234862430114720 ) ) ;
#64986 = CARTESIAN_POINT ( 'NONE',  ( 18.92609651878039756, 19.43085787977762635, -9.188101187500008038 ) ) ;
#64987 = CARTESIAN_POINT ( 'NONE',  ( 175.0387250457744983, 253.3993311541219953, -7.863511161993287146 ) ) ;
#64988 = FACE_OUTER_BOUND ( 'NONE', #49318, .T. ) ;
#64989 = CARTESIAN_POINT ( 'NONE',  ( 112.2445834879231796, 225.6115022471901739, -5.000000000000041744 ) ) ;
#64990 = CARTESIAN_POINT ( 'NONE',  ( 160.0081047537594543, 253.5048282741223602, -16.11956848123596941 ) ) ;
#64991 = CARTESIAN_POINT ( 'NONE',  ( 84.99999999999998579, 14.99999999999999467, 59.99999999999999289 ) ) ;
#64992 = ORIENTED_EDGE ( 'NONE', *, *, #19629, .T. ) ;
#64994 = CYLINDRICAL_SURFACE ( 'NONE', #71636, 10.00000000000010658 ) ;
#64993 =( BOUNDED_CURVE ( )  B_SPLINE_CURVE ( 2, ( #51784, #19893, #64989, #11312, #90322, #57872, #35575, #89341, #5179 ),
 .UNSPECIFIED., .F., .T. ) 
 B_SPLINE_CURVE_WITH_KNOTS ( ( 3, 2, 2, 2, 3 ),
 ( 0.7540322580645161255, 0.7553763440860215006, 0.7580645161290322509, 0.7607526881720430012, 0.7620967741935483764 ),
 .UNSPECIFIED. ) 
 CURVE ( )  GEOMETRIC_REPRESENTATION_ITEM ( )  RATIONAL_B_SPLINE_CURVE ( ( 0.9330127018922194093, 0.9330127018922194093, 1.000000000000000000, 0.8660254037844387076, 1.000000000000000000, 0.8660254037844387076, 1.000000000000000000, 0.9330127018922194093, 0.9330127018922194093 ) ) 
 REPRESENTATION_ITEM ( '' )  );
#64995 = CARTESIAN_POINT ( 'NONE',  ( 165.0509870607838252, 244.7702999017660375, -2.356357909806504392 ) ) ;
#64996 = CARTESIAN_POINT ( 'NONE',  ( 74.14312167556930433, 66.30466486950707861, 1.224646799147354045E-15 ) ) ;
#64997 = CARTESIAN_POINT ( 'NONE',  ( 87.49951909536234496, 45.04593868083597386, 6.937257679092502904 ) ) ;
#64998 = VECTOR ( 'NONE', #46643, 1000.000000000000114 ) ;
#64999 = ORIENTED_EDGE ( 'NONE', *, *, #38048, .T. ) ;
#65000 = ORIENTED_EDGE ( 'NONE', *, *, #99831, .F. ) ;
#65001 = LINE ( 'NONE', #88356, #37354 ) ;
#65002 = CARTESIAN_POINT ( 'NONE',  ( 86.20802731503823679, 47.17721747253784770, 10.82151197958144273 ) ) ;
#65003 = VERTEX_POINT ( 'NONE', #99907 ) ;
#65004 = CARTESIAN_POINT ( 'NONE',  ( 77.00607721352450596, 53.74328018355883074, 15.98262156706233306 ) ) ;
#65005 = CARTESIAN_POINT ( 'NONE',  ( 178.2293965766191661, 264.0593690949378356, 14.86337493992927605 ) ) ;
#65006 = VERTEX_POINT ( 'NONE', #1100 ) ;
#65007 = LINE ( 'NONE', #73607, #21585 ) ;
#65008 = CARTESIAN_POINT ( 'NONE',  ( 88.54549197286583251, 43.89854493182281203, -0.2370037879772138034 ) ) ;
#65009 = ADVANCED_FACE ( 'NONE', ( #69487 ), #46623, .F. ) ;
#65010 = CARTESIAN_POINT ( 'NONE',  ( 17.63446822084836896, 18.38052372038639959, 10.00000000000000533 ) ) ;
#65011 = VERTEX_POINT ( 'NONE', #73501 ) ;
#65012 = CARTESIAN_POINT ( 'NONE',  ( 200.6097954076514895, 283.1806371883870383, 16.82611162221071766 ) ) ;
#65013 = CARTESIAN_POINT ( 'NONE',  ( 169.3073612053613317, 276.1872213954042081, -15.55595306670203293 ) ) ;
#65014 = CARTESIAN_POINT ( 'NONE',  ( 81.89485588203808675, 55.22971306509116829, 16.24120679747551677 ) ) ;
#65015 = ORIENTED_EDGE ( 'NONE', *, *, #2043, .F. ) ;
#65016 = CARTESIAN_POINT ( 'NONE',  ( 170.6728735680048317, 255.5809563222128418, -11.58821030780939765 ) ) ;
#65017 = CARTESIAN_POINT ( 'NONE',  ( 203.0337691736598629, 278.9821914694464340, 16.08167820133810011 ) ) ;
#65018 = VERTEX_POINT ( 'NONE', #42568 ) ;
#65019 = CARTESIAN_POINT ( 'NONE',  ( 156.9771955771814476, 266.1637941048814469, -16.64471738717700688 ) ) ;
#65020 = ORIENTED_EDGE ( 'NONE', *, *, #76556, .F. ) ;
#65021 = DIRECTION ( 'NONE',  ( 1.000000000000000000, 0.000000000000000000, 0.000000000000000000 ) ) ;
#65022 = ORIENTED_EDGE ( 'NONE', *, *, #26832, .T. ) ;
#65023 = CARTESIAN_POINT ( 'NONE',  ( 193.2916431108056088, 295.8560487840508699, 14.28858925737053909 ) ) ;
#65024 = CARTESIAN_POINT ( 'NONE',  ( 177.8598173235638740, 289.1843520170486386, -9.332820079591703788 ) ) ;
#65026 = EDGE_CURVE ( 'NONE', #58073, #49297, #87768, .T. ) ;
#65025 = CARTESIAN_POINT ( 'NONE',  ( 71.69220090349242014, 69.88970279385412709, 7.579357904728459161 ) ) ;
#65027 = CARTESIAN_POINT ( 'NONE',  ( 183.7975612849717777, 256.6346208101135176, -2.981236333899912161 ) ) ;
#65028 = CARTESIAN_POINT ( 'NONE',  ( 25.88271472100439041, 39.90032630942972247, -10.00000000000000000 ) ) ;
#65029 = CARTESIAN_POINT ( 'NONE',  ( 191.2190380946134951, 260.9445496458436651, 3.106810577783889915 ) ) ;
#65030 = VERTEX_POINT ( 'NONE', #94825 ) ;
#65031 = CARTESIAN_POINT ( 'NONE',  ( 92.02724010209958294, 235.4860189848785410, -2.679491924311252493 ) ) ;
#65032 = CARTESIAN_POINT ( 'NONE',  ( 20.82173017108080515, 32.99752408145591431, 5.678558825948277544 ) ) ;
#65033 = DIRECTION ( 'NONE',  ( -0.6116140086401625764, 0.7911563084720434347, 0.000000000000000000 ) ) ;
#65035 = ORIENTED_EDGE ( 'NONE', *, *, #58498, .T. ) ;
#65034 = CARTESIAN_POINT ( 'NONE',  ( 159.7953104873542145, 253.8733987550956783, 15.41928249285404107 ) ) ;
#65036 = ORIENTED_EDGE ( 'NONE', *, *, #50987, .F. ) ;
#65037 = CARTESIAN_POINT ( 'NONE',  ( 190.9260630086136530, 299.9533537104214247, 6.698530349890277513 ) ) ;
#65038 = CARTESIAN_POINT ( 'NONE',  ( 171.5198295675851057, 259.4245737330473389, -13.88290939651866829 ) ) ;
#65039 = CARTESIAN_POINT ( 'NONE',  ( 189.3423859142968695, 300.6963629005612120, 0.4146017780601669589 ) ) ;
#65040 = DIRECTION ( 'NONE',  ( -0.000000000000000000, 0.000000000000000000, -1.000000000000000000 ) ) ;
#65041 = CARTESIAN_POINT ( 'NONE',  ( 46.06580888206229929, 190.7365022471901739, -10.00000000000009237 ) ) ;
#65042 = CARTESIAN_POINT ( 'NONE',  ( 148.6603736319484597, 273.1596751277295425, -9.224525803417190417 ) ) ;
#65043 = ORIENTED_EDGE ( 'NONE', *, *, #19363, .T. ) ;
#65044 = CARTESIAN_POINT ( 'NONE',  ( 175.7882114856885210, 291.4026636951798537, -6.622811550496607857 ) ) ;
#65045 = LINE ( 'NONE', #55911, #33843 ) ;
#65046 = LINE ( 'NONE', #66537, #54398 ) ;
#65047 = CARTESIAN_POINT ( 'NONE',  ( 164.9335952247126045, 244.9736285262353306, -1.661461410667423255 ) ) ;
#65048 = CARTESIAN_POINT ( 'NONE',  ( 31.46967238556418422, 175.6427522451417644, 1.119607411625061291E-15 ) ) ;
#65049 = CARTESIAN_POINT ( 'NONE',  ( 102.2582280487598609, 229.8458772461660544, 9.188101187500095079 ) ) ;
#65050 = CARTESIAN_POINT ( 'NONE',  ( 166.8965953329662568, 259.4083194189263963, 16.50658842888446642 ) ) ;
#65051 = CARTESIAN_POINT ( 'NONE',  ( 168.6156890688689884, 286.4116463664167895, -8.226575548882113509 ) ) ;
#65052 = CARTESIAN_POINT ( 'NONE',  ( 162.6419541827858950, 248.9428672435623184, 10.30167521348375459 ) ) ;
#65053 = CARTESIAN_POINT ( 'NONE',  ( 31.75860784375665702, 179.9548013555409796, -4.594050593750042211 ) ) ;
#65054 = CARTESIAN_POINT ( 'NONE',  ( 172.0630936339023265, 254.4764114392720273, 11.54978638049990103 ) ) ;
#65055 = ORIENTED_EDGE ( 'NONE', *, *, #3337, .T. ) ;
#65056 = ORIENTED_EDGE ( 'NONE', *, *, #79289, .F. ) ;
#65057 = CARTESIAN_POINT ( 'NONE',  ( 185.1598287763772532, 259.9719152823935815, -5.764292841724723893 ) ) ;
#65058 = CARTESIAN_POINT ( 'NONE',  ( 67.41639658691251213, 69.05313671411084897, 3.556105138604360061 ) ) ;
#65059 = CARTESIAN_POINT ( 'NONE',  ( 82.67950799182933963, 41.89762085301913430, 4.838269528849628465 ) ) ;
#65060 = CARTESIAN_POINT ( 'NONE',  ( 193.5605340833295998, 262.7645764782593005, -3.913255771308810971 ) ) ;
#65061 = DIRECTION ( 'NONE',  ( 0.1783728972749306640, 0.9839629614562466209, 0.000000000000000000 ) ) ;
#65062 = CARTESIAN_POINT ( 'NONE',  ( 182.7015270599942767, 284.3474866054488643, 14.96321108283051515 ) ) ;
#65063 = FACE_OUTER_BOUND ( 'NONE', #42947, .T. ) ;
#65064 = CARTESIAN_POINT ( 'NONE',  ( 48.02338713675939630, 198.5333772461660828, 9.188101187500095079 ) ) ;
#65065 = CARTESIAN_POINT ( 'NONE',  ( 91.22542524669046315, 210.1427522451417360, 1.119607411625061291E-15 ) ) ;
#65066 = ORIENTED_EDGE ( 'NONE', *, *, #69955, .T. ) ;
#65067 = CARTESIAN_POINT ( 'NONE',  ( 83.95052478757145309, 47.16512906835476571, 11.42333699328953145 ) ) ;
#65068 = ADVANCED_FACE ( 'NONE', ( #18306 ), #80138, .F. ) ;
#65069 = B_SPLINE_CURVE_WITH_KNOTS ( 'NONE', 3,
 ( #21542, #45320, #76255, #52425 ),
 .UNSPECIFIED., .F., .F.,
 ( 4, 4 ),
 ( 0.03623143502817663397, 0.04492301886968718544 ),
 .UNSPECIFIED. ) ;
#65070 = CARTESIAN_POINT ( 'NONE',  ( 158.5653840560831043, 282.4927873443422754, -1.666044833076710585 ) ) ;
#65071 = CARTESIAN_POINT ( 'NONE',  ( 5.155129649429669669, 173.7833772461660828, -9.188101187500095079 ) ) ;
#65072 = CARTESIAN_POINT ( 'NONE',  ( 68.51023738315195999, 64.28149084335623797, -12.38465469846545730 ) ) ;
#65073 = CARTESIAN_POINT ( 'NONE',  ( 151.0426280674448378, 269.0334894088936153, -15.84467774422408581 ) ) ;
#65074 = PLANE ( 'NONE',  #59681 ) ;
#65075 = CARTESIAN_POINT ( 'NONE',  ( 147.1034852426517148, 275.8562849197056153, -3.648177088342072327 ) ) ;
#65076 = CARTESIAN_POINT ( 'NONE',  ( 69.54491560247440418, 68.33319813537798382, -8.868170946166037183 ) ) ;
#65077 = CARTESIAN_POINT ( 'NONE',  ( 164.3853877993040840, 245.9231516401292197, 5.995325337583643943 ) ) ;
#65078 = CARTESIAN_POINT ( 'NONE',  ( 67.62392126478502519, 221.3967562850346837, -4.648177544792955347E-16 ) ) ;
#65079 = FACE_OUTER_BOUND ( 'NONE', #18776, .T. ) ;
#65080 = EDGE_LOOP ( 'NONE', ( #20825, #68571, #97658, #60265 ) ) ;
#65081 = CARTESIAN_POINT ( 'NONE',  ( -8.493791556357424000, 179.2365022471903160, 2.944929066748280225E-16 ) ) ;
#65082 = CARTESIAN_POINT ( 'NONE',  ( 85.09877614057847950, 47.61067639237452909, 11.82617649972324259 ) ) ;
#65083 = CARTESIAN_POINT ( 'NONE',  ( 128.5637496887121927, 245.0333772461660544, 9.188101187500095079 ) ) ;
#65084 = CARTESIAN_POINT ( 'NONE',  ( 21.69737781089059681, 21.03085787977762777, 9.188101187500006262 ) ) ;
#65085 = CARTESIAN_POINT ( 'NONE',  ( 74.92881689719639837, 67.14644430943499742, 12.99852016367277052 ) ) ;
#65086 = LINE ( 'NONE', #3799, #1530 ) ;
#65088 = CARTESIAN_POINT ( 'NONE',  ( 185.5460614991013983, 288.0617137868250666, 14.93142655311823397 ) ) ;
#65087 = CARTESIAN_POINT ( 'NONE',  ( 157.8092552871339365, 257.3133472685137235, 17.04082256169242626 ) ) ;
#65089 = CARTESIAN_POINT ( 'NONE',  ( 11.95823279523498073, 29.83705186507753027, 3.090169943749475401 ) ) ;
#65090 = VERTEX_POINT ( 'NONE', #12708 ) ;
#65091 = CARTESIAN_POINT ( 'NONE',  ( 191.5694459269389824, 298.8389818071599962, 7.944420692511652504 ) ) ;
#65092 = CARTESIAN_POINT ( 'NONE',  ( 196.3507576896697344, 290.5575069072837664, -17.68249398312240928 ) ) ;
#65093 = LINE ( 'NONE', #2315, #28073 ) ;
#65094 = CARTESIAN_POINT ( 'NONE',  ( 174.5937358169846902, 290.6289298292567764, -1.069262448657138043 ) ) ;
#65095 = CARTESIAN_POINT ( 'NONE',  ( 81.39533252797791363, 55.41833949407015325, -16.32393128051840137 ) ) ;
#65096 = ORIENTED_EDGE ( 'NONE', *, *, #19842, .T. ) ;
#65097 = CARTESIAN_POINT ( 'NONE',  ( 69.93689855390263688, 65.90667941659796725, -11.72867282680260281 ) ) ;
#65098 = VECTOR ( 'NONE', #72988, 1000.000000000000000 ) ;
#65100 = CARTESIAN_POINT ( 'NONE',  ( 175.8408436088426186, 278.6720592842420956, 15.46214555605372531 ) ) ;
#65099 = B_SPLINE_CURVE_WITH_KNOTS ( 'NONE', 3,
 ( #93265, #23319, #53232, #69430, #76545, #70429, #54207, #68921, #77550, #61814, #99847, #53714, #62821, #23820, #93777, #86194 ),
 .UNSPECIFIED., .F., .F.,
 ( 4, 1, 2, 2, 2, 1, 2, 2, 4 ),
 ( 0.000000000000000000, 0.1250000000000020539, 0.1875000000000021927, 0.2500000000000023315, 0.5000000000000027756, 0.6250000000000039968, 0.6875000000000046629, 0.7500000000000052180, 1.000000000000000000 ),
 .UNSPECIFIED. ) ;
#65101 = CARTESIAN_POINT ( 'NONE',  ( 166.8389619083949924, 270.5748136803991883, -16.31214114901503720 ) ) ;
#65102 = CARTESIAN_POINT ( 'NONE',  ( 72.13526286807632459, 72.32911410822552511, 1.080822308860484027 ) ) ;
#65103 = B_SPLINE_SURFACE_WITH_KNOTS ( 'NONE', 3, 1, ( 
 ( #5323, #28604 ),
 ( #21038, #52899 ),
 ( #13912, #90961 ),
 ( #36199, #83851 ),
 ( #52402, #74743 ),
 ( #67104, #67605 ),
 ( #30106, #44299 ),
 ( #68599, #29612 ),
 ( #51920, #6311 ),
 ( #22504, #75727 ),
 ( #44791, #90468 ),
 ( #59487, #82860 ),
 ( #98534, #99522 ),
 ( #12942, #91442 ),
 ( #5810, #36696 ),
 ( #13432, #60988 ),
 ( #98029, #75228 ),
 ( #4833, #37202 ),
 ( #29125, #60484 ),
 ( #20529, #97542 ),
 ( #14416, #83346 ),
 ( #51409, #45299 ),
 ( #76232, #82371 ),
 ( #12431, #68104 ),
 ( #59991, #6807 ),
 ( #21518, #74247 ),
 ( #37689, #66613 ),
 ( #99025, #91955 ),
 ( #81855, #43300 ),
 ( #35714, #58983 ),
 ( #28109, #89952 ),
 ( #32087, #85872 ),
 ( #54372, #100022 ),
 ( #64882, #203 ) ),
 .UNSPECIFIED., .T., .F., .F.,
 ( 4, 2, 2, 2, 2, 2, 2, 2, 2, 2, 2, 2, 2, 2, 2, 2, 4 ),
 ( 2, 2 ),
 ( 0.000000000000000000, 0.06250000000000000000, 0.1250000000000000000, 0.1875000000000000000, 0.2500000000000000000, 0.3125000000000000000, 0.3750000000000000000, 0.4375000000000000000, 0.5000000000000000000, 0.5625000000000000000, 0.6250000000000000000, 0.6875000000000000000, 0.7500000000000000000, 0.8125000000000000000, 0.8750000000000000000, 0.9375000000000000000, 1.000000000000000000 ),
 ( 0.000000000000000000, 1.000000000000000000 ),
 .UNSPECIFIED. ) ;
#65104 = B_SPLINE_CURVE_WITH_KNOTS ( 'NONE', 3,
 ( #54368, #92924, #31083, #14411, #68100, #5806, #99518, #6803, #45777, #61971, #36691, #22985, #85341, #99021, #53391, #7802, #59987, #69091, #76699, #77195, #98530, #68595, #22500, #100017, #30602, #38687, #75722, #21999, #46272, #23477, #7292, #15886, #38173, #29607, #61488, #67600, #92438, #46798, #69591, #30102, #91949, #52398, #90957, #29120, #21513, #37683 ),
 .UNSPECIFIED., .F., .F.,
 ( 4, 1, 2, 2, 1, 2, 2, 1, 1, 2, 2, 1, 1, 2, 2, 1, 1, 2, 2, 1, 1, 1, 2, 2, 1, 1, 1, 2, 2, 4 ),
 ( 0.000000000000000000, 0.06249999999999931999, 0.09374999999999898692, 0.1249999999999986677, 0.1875000000000011935, 0.2187500000000009437, 0.2500000000000007216, 0.3125000000000002776, 0.3437500000000017208, 0.3593750000000022204, 0.3750000000000026645, 0.4375000000000003886, 0.4687499999999992784, 0.4843749999999972244, 0.4999999999999951150, 0.5624999999999961142, 0.5937499999999952260, 0.6093749999999964473, 0.6249999999999977796, 0.6874999999999930056, 0.7187499999999892308, 0.7343749999999890088, 0.7421874999999888978, 0.7499999999999888978, 0.8124999999999964473, 0.8437499999999985567, 0.8593749999999996669, 0.8671874999999986677, 0.8749999999999976685, 1.000000000000000000 ),
 .UNSPECIFIED. ) ;
#65105 = CARTESIAN_POINT ( 'NONE',  ( 80.48032370448046890, 56.76188079953907106, 16.17739337235778052 ) ) ;
#65106 = CARTESIAN_POINT ( 'NONE',  ( 155.6661834545002989, 261.4322516281303592, 17.01228065901951325 ) ) ;
#65107 = LINE ( 'NONE', #34212, #90593 ) ;
#65108 = CARTESIAN_POINT ( 'NONE',  ( 153.4389798490260262, 264.8828863703868137, 16.68923469758090761 ) ) ;
#65109 = ORIENTED_EDGE ( 'NONE', *, *, #93047, .F. ) ;
#65110 = DIRECTION ( 'NONE',  ( 0.5000000000000048850, -0.8660254037844358210, 0.000000000000000000 ) ) ;
#65111 = CARTESIAN_POINT ( 'NONE',  ( 5.036790953515181357, 27.00034080476288523, -1.878358725466461243E-16 ) ) ;
#65112 = CARTESIAN_POINT ( 'NONE',  ( 191.8248132796572918, 287.9113088684474064, -15.87179701694280176 ) ) ;
#65113 = VERTEX_POINT ( 'NONE', #29878 ) ;
#65114 = CARTESIAN_POINT ( 'NONE',  ( 77.80736617348490824, 61.72758938687779562, 16.06622420362089798 ) ) ;
#65115 = CARTESIAN_POINT ( 'NONE',  ( 148.0826818691893152, 274.1602666119424043, -9.371267383421741926 ) ) ;
#65116 = CARTESIAN_POINT ( 'NONE',  ( 156.0874977470830345, 262.0026131717037856, -16.96117934707180552 ) ) ;
#65117 = VERTEX_POINT ( 'NONE', #67376 ) ;
#65118 = CARTESIAN_POINT ( 'NONE',  ( 78.73521911786851035, 59.96578626319077188, 16.11589682977616533 ) ) ;
#65119 = LINE ( 'NONE', #32213, #24898 ) ;
#65120 = AXIS2_PLACEMENT_3D ( 'NONE', #56430, #71157, #64036 ) ;
#65121 = EDGE_CURVE ( 'NONE', #734, #43672, #66890, .T. ) ;
#65122 = ORIENTED_EDGE ( 'NONE', *, *, #28684, .F. ) ;
#65123 = CARTESIAN_POINT ( 'NONE',  ( 79.14797540978585744, 51.65882171989947125, -15.32139210428527321 ) ) ;
#65124 = CARTESIAN_POINT ( 'NONE',  ( 81.40142225033505952, 41.96015433569891684, -7.703957233619936673 ) ) ;
#65125 = ORIENTED_EDGE ( 'NONE', *, *, #69452, .F. ) ;
#65126 = ORIENTED_EDGE ( 'NONE', *, *, #34437, .T. ) ;
#65127 = CARTESIAN_POINT ( 'NONE',  ( -28.63239376340754561, 61.06670042544809007, -10.00000000000000000 ) ) ;
#65128 = ORIENTED_EDGE ( 'NONE', *, *, #84190, .T. ) ;
#65129 = CARTESIAN_POINT ( 'NONE',  ( 171.7383634674231416, 249.5738785302591509, -2.481706805167441576 ) ) ;
#65131 = EDGE_CURVE ( 'NONE', #69843, #4429, #7785, .T. ) ;
#65130 = VERTEX_POINT ( 'NONE', #90737 ) ;
#65132 = CARTESIAN_POINT ( 'NONE',  ( 74.67627071976463071, 57.26912010096364725, 16.03321057786944692 ) ) ;
#65133 = CARTESIAN_POINT ( 'NONE',  ( 155.3513572141771704, 261.5705516107003064, -17.00592413546589299 ) ) ;
#65134 = ORIENTED_EDGE ( 'NONE', *, *, #79460, .T. ) ;
#65135 = CARTESIAN_POINT ( 'NONE',  ( 183.0440910913980872, 280.4743473074019562, -16.11601913062221669 ) ) ;
#65136 = CARTESIAN_POINT ( 'NONE',  ( 32.14254330279432992, 120.6340272870843364, 59.99999999999999289 ) ) ;
#65137 = CARTESIAN_POINT ( 'NONE',  ( 151.3884156280674063, 268.8244654414531283, 14.32026866203507076 ) ) ;
#65138 = CARTESIAN_POINT ( 'NONE',  ( 161.8067806907298518, 277.5376414676186982, -13.20325758529581961 ) ) ;
#65139 = CARTESIAN_POINT ( 'NONE',  ( 147.2089949622447875, 275.6735367246781720, -3.633014386235353221 ) ) ;
#65141 = EDGE_CURVE ( 'NONE', #88888, #87622, #61710, .T. ) ;
#65140 = CARTESIAN_POINT ( 'NONE',  ( 200.7134601498536028, 283.0010845879393742, -16.98649239173277792 ) ) ;
#65142 = DIRECTION ( 'NONE',  ( -0.3213938048432640748, 0.5566703992264119272, -0.7660444431189857850 ) ) ;
#65143 = CARTESIAN_POINT ( 'NONE',  ( 10.48659854325162222, 166.8615022471902023, 5.000000000000051514 ) ) ;
#65144 = CARTESIAN_POINT ( 'NONE',  ( 138.2797325092426490, 241.4548013555409796, -4.594050593750042211 ) ) ;
#65145 = CARTESIAN_POINT ( 'NONE',  ( 196.2953682204578456, 263.5854184417236752, 0.8810977108677261471 ) ) ;
#65146 = CARTESIAN_POINT ( 'NONE',  ( 40.90268743793880901, 35.56628583063844218, 9.188101187500006262 ) ) ;
#65147 = ORIENTED_EDGE ( 'NONE', *, *, #60251, .F. ) ;
#65149 = ORIENTED_EDGE ( 'NONE', *, *, #92424, .F. ) ;
#65148 = CARTESIAN_POINT ( 'NONE',  ( 204.0395441575055031, 271.6647427339178762, 9.749783370949133499 ) ) ;
#65150 = B_SPLINE_CURVE_WITH_KNOTS ( 'NONE', 3,
 ( #18845, #88793, #57814, #96368 ),
 .UNSPECIFIED., .F., .F.,
 ( 4, 4 ),
 ( 0.003259762943304704563, 0.01121638692189557036 ),
 .UNSPECIFIED. ) ;
#65151 = CARTESIAN_POINT ( 'NONE',  ( 78.28406713961415164, 47.42774444821681357, -13.76474501704126929 ) ) ;
#65152 = CARTESIAN_POINT ( 'NONE',  ( 76.28172291344246503, 65.04177861043513076, -14.25052431483989324 ) ) ;
#65153 = CARTESIAN_POINT ( 'NONE',  ( 157.6339405821837829, 280.6012083038259561, -7.094479895829409521 ) ) ;
#65154 = CARTESIAN_POINT ( 'NONE',  ( 70.91684448083535131, 60.93905801807242995, 14.54788300031792936 ) ) ;
#65155 = CARTESIAN_POINT ( 'NONE',  ( -31.49356256989596758, 94.88921800892812541, 36.50000000000000000 ) ) ;
#65156 = DIRECTION ( 'NONE',  ( -1.000000000000000000, 0.000000000000000000, 0.000000000000000000 ) ) ;
#65157 = CARTESIAN_POINT ( 'NONE',  ( 88.22170401875577284, 44.22125859644826562, -1.816381297913363779 ) ) ;
#65158 = ORIENTED_EDGE ( 'NONE', *, *, #48377, .T. ) ;
#65159 = CARTESIAN_POINT ( 'NONE',  ( 194.2389208611690492, 294.2153155915419802, -15.75132567904764791 ) ) ;
#65160 = CARTESIAN_POINT ( 'NONE',  ( 66.01181605970899113, 68.68997318219119563, -0.06151385425865887879 ) ) ;
#65161 = ORIENTED_EDGE ( 'NONE', *, *, #82176, .F. ) ;
#65162 = CARTESIAN_POINT ( 'NONE',  ( 163.2575071667584723, 277.3374444033298118, 12.94744084712231569 ) ) ;
#65163 = CARTESIAN_POINT ( 'NONE',  ( 201.1240395725599228, 267.4342541147308339, -2.284400240072811172 ) ) ;
#65164 = CARTESIAN_POINT ( 'NONE',  ( 50.15574305400770072, 101.0118721476823964, 10.00000000000000000 ) ) ;
#65165 = CARTESIAN_POINT ( 'NONE',  ( 149.0359194785865498, 272.5092106407810206, 12.76357969772040590 ) ) ;
#65167 = VECTOR ( 'NONE', #1300, 999.9999999999998863 ) ;
#65166 = CARTESIAN_POINT ( 'NONE',  ( 162.6220573360242270, 248.9773295930640131, 10.49878733418918486 ) ) ;
#65169 = CARTESIAN_POINT ( 'NONE',  ( 151.3150518705357683, 275.2366200239924297, -9.722076783269896438 ) ) ;
#65168 = CARTESIAN_POINT ( 'NONE',  ( -19.65312891409030271, 93.06504152958497400, 10.00000000000000888 ) ) ;
#65170 = VECTOR ( 'NONE', #28459, 1000.000000000000227 ) ;
#65171 = CARTESIAN_POINT ( 'NONE',  ( 203.4543820542745891, 269.9310094597221337, 5.750300676160139624 ) ) ;
#65172 = ORIENTED_EDGE ( 'NONE', *, *, #45944, .F. ) ;
#65173 = ADVANCED_FACE ( 'NONE', ( #36472 ), #75496, .F. ) ;
#65174 = CARTESIAN_POINT ( 'NONE',  ( 73.45240594507248488, 61.98306700939508573, -14.75352172543200524 ) ) ;
#65175 = DIRECTION ( 'NONE',  ( 0.7696402260561062691, 0.6384778167143364547, 0.000000000000000000 ) ) ;
#65176 = ADVANCED_FACE ( 'NONE', ( #27883 ), #14245, .T. ) ;
#65177 = VECTOR ( 'NONE', #70458, 1000.000000000000000 ) ;
#65178 = CARTESIAN_POINT ( 'NONE',  ( 74.69145432289207065, 65.16111103690977302, -13.69219638301821185 ) ) ;
#65179 = CARTESIAN_POINT ( 'NONE',  ( 192.8323852661406761, 296.6515067047851062, 11.86505947732313615 ) ) ;
#65180 = CARTESIAN_POINT ( 'NONE',  ( 80.78722682204974603, 43.18815817188708195, -9.889478511952381368 ) ) ;
#65181 = CARTESIAN_POINT ( 'NONE',  ( -17.42236680055705023, 149.2012482093457777, 0.000000000000000000 ) ) ;
#65182 = CARTESIAN_POINT ( 'NONE',  ( 202.6070187115982719, 279.7213449518906145, 15.56322169823762280 ) ) ;
#65183 = CARTESIAN_POINT ( 'NONE',  ( 13.46382118881039602, 169.3923013555410080, 4.594050593750050204 ) ) ;
#65184 = CARTESIAN_POINT ( 'NONE',  ( 106.6698052711106186, 223.2048013555410080, 4.594050593750051981 ) ) ;
#65185 = CARTESIAN_POINT ( 'NONE',  ( 154.9528145190857344, 262.2608478075840708, -17.26679351315302213 ) ) ;
#65186 = CARTESIAN_POINT ( 'NONE',  ( 88.05624235485146301, 44.55787864911080476, -5.145732200269209855 ) ) ;
#65187 = CARTESIAN_POINT ( 'NONE',  ( 183.9260584196478874, 294.3655144402644055, -7.753805750097078509 ) ) ;
#65188 = CARTESIAN_POINT ( 'NONE',  ( -19.63199130574582796, 93.20528039779287610, 59.99999999999999289 ) ) ;
#65189 = ADVANCED_FACE ( 'NONE', ( #46054 ), #53179, .F. ) ;
#65190 = VECTOR ( 'NONE', #54615, 1000.000000000000227 ) ;
#65191 = CARTESIAN_POINT ( 'NONE',  ( 75.84856439504059722, 51.76521084193598909, 15.76359423700355755 ) ) ;
#65192 = CARTESIAN_POINT ( 'NONE',  ( 161.6289632141471486, 282.0538248220675541, 5.604263265739757749 ) ) ;
#65193 = CARTESIAN_POINT ( 'NONE',  ( 194.2223991963907963, 294.2439319543634610, -14.97294938100067441 ) ) ;
#65194 = EDGE_CURVE ( 'NONE', #30353, #41966, #41762, .T. ) ;
#65195 = CARTESIAN_POINT ( 'NONE',  ( 181.7974296340893261, 291.5457255195387916, 9.383524427102701182 ) ) ;
#65196 = EDGE_CURVE ( 'NONE', #98414, #28497, #77493, .T. ) ;
#65197 = CARTESIAN_POINT ( 'NONE',  ( -19.65312891409030271, 93.06504152958497400, 10.00000000000000888 ) ) ;
#65198 = FACE_OUTER_BOUND ( 'NONE', #89743, .T. ) ;
#65199 = CARTESIAN_POINT ( 'NONE',  ( 6.860117161356369841, 164.7677522451418213, -5.000000000000041744 ) ) ;
#65200 = CARTESIAN_POINT ( 'NONE',  ( 80.10468490011123777, 54.30569091379602753, -15.86741517739214125 ) ) ;
#65201 = CARTESIAN_POINT ( 'NONE',  ( 79.40524497836292994, 46.23731968723249253, -13.25138998636449372 ) ) ;
#65202 = CARTESIAN_POINT ( 'NONE',  ( 81.63493525668631889, 229.4860189848785410, -2.679491924311252493 ) ) ;
#65203 = LINE ( 'NONE', #85172, #69386 ) ;
#65204 = CARTESIAN_POINT ( 'NONE',  ( 90.35072584248885619, 210.7202760586659736, -5.415160957724236172E-17 ) ) ;
#65205 = CARTESIAN_POINT ( 'NONE',  ( 161.7412967960748915, 250.5028515975580774, -14.36228887024421041 ) ) ;
#65206 = CARTESIAN_POINT ( 'NONE',  ( 72.57191691350548979, 57.24899938748259132, 15.86174820108270112 ) ) ;
#65207 = CARTESIAN_POINT ( 'NONE',  ( -16.14732403980535835, 103.0408369278337801, 12.67348291615926215 ) ) ;
#65209 = CARTESIAN_POINT ( 'NONE',  ( 151.7785311547446270, 267.7588678722433428, 16.64796787849914850 ) ) ;
#65208 = CARTESIAN_POINT ( 'NONE',  ( 197.5862184977020490, 286.6310308989096711, -17.64960021936426671 ) ) ;
#65210 = CARTESIAN_POINT ( 'NONE',  ( 173.2447795235415811, 268.2516447256268179, -16.29229155239807980 ) ) ;
#65211 = CARTESIAN_POINT ( 'NONE',  ( 35.02453322635827249, 23.14754757982092315, -5.678558825948275768 ) ) ;
#65212 = CARTESIAN_POINT ( 'NONE',  ( 80.75896084256157792, 48.90990202073309945, -14.35679662723407368 ) ) ;
#65213 = CARTESIAN_POINT ( 'NONE',  ( 84.99894282664955369, 46.71838944095585333, -10.45175089821682413 ) ) ;
#65214 = ORIENTED_EDGE ( 'NONE', *, *, #80679, .T. ) ;
#65215 = CARTESIAN_POINT ( 'NONE',  ( 15.95033727479334651, 30.18502408145591787, 5.678558825948277544 ) ) ;
#65216 = CARTESIAN_POINT ( 'NONE',  ( 74.97842782955004282, 214.0958772461660544, -9.188101187500095079 ) ) ;
#65217 = CARTESIAN_POINT ( 'NONE',  ( 169.3398175065472344, 288.7630245530638717, -1.132601341623118874 ) ) ;
#65218 = CARTESIAN_POINT ( 'NONE',  ( -32.49964441091157141, 93.83990077386336282, 10.47370245339621420 ) ) ;
#65219 = CARTESIAN_POINT ( 'NONE',  ( 191.7460210811677541, 287.9459192371517133, -15.84374680109877609 ) ) ;
#65220 = EDGE_LOOP ( 'NONE', ( #55342, #80363, #64264 ) ) ;
#65221 = CARTESIAN_POINT ( 'NONE',  ( 86.10128179547638183, 47.01522930412664181, 10.71950609365847384 ) ) ;
#65222 = CARTESIAN_POINT ( 'NONE',  ( 190.3592232750935409, 286.7364522702076215, 16.27178271100322249 ) ) ;
#65223 = LINE ( 'NONE', #27233, #79308 ) ;
#65224 = CARTESIAN_POINT ( 'NONE',  ( 125.6679772465819127, 253.3615022471903444, 5.000000000000046185 ) ) ;
#65225 = CARTESIAN_POINT ( 'NONE',  ( 157.1458804504438831, 258.4623461901232417, -17.08829597948888335 ) ) ;
#65226 = CARTESIAN_POINT ( 'NONE',  ( 74.85635044626891954, 53.33667049677163874, 16.05360532518207606 ) ) ;
#65227 = ORIENTED_EDGE ( 'NONE', *, *, #28717, .T. ) ;
#65228 = CARTESIAN_POINT ( 'NONE',  ( 165.5469766331900985, 246.9197538857407608, -1.831016119632084438 ) ) ;
#65229 = ORIENTED_EDGE ( 'NONE', *, *, #28974, .F. ) ;
#65230 = CARTESIAN_POINT ( 'NONE',  ( 163.2437751800324293, 247.9004826992694461, 9.806027032984305336 ) ) ;
#65231 = CARTESIAN_POINT ( 'NONE',  ( 207.2447263765708954, 270.1464842563735829, -0.1082122603863571730 ) ) ;
#65232 = DIRECTION ( 'NONE',  ( 0.8660254037844384856, 0.5000000000000002220, -5.782411586589354927E-17 ) ) ;
#65233 = CARTESIAN_POINT ( 'NONE',  ( 77.23930090163744921, 62.99565350650583895, -15.27869716933193445 ) ) ;
#65234 = ORIENTED_EDGE ( 'NONE', *, *, #12227, .F. ) ;
#65235 = CARTESIAN_POINT ( 'NONE',  ( 72.24104924332462474, 71.74196171561413848, 5.528620549063430367 ) ) ;
#65236 = CARTESIAN_POINT ( 'NONE',  ( 167.4483379500863407, 247.4779818019835034, 3.613496412595774920 ) ) ;
#65237 = CARTESIAN_POINT ( 'NONE',  ( 194.0917849768643748, 280.7715605316444680, -17.25264104449663449 ) ) ;
#65238 = CARTESIAN_POINT ( 'NONE',  ( 201.3053657339852691, 274.7141922394133076, -14.27644254562359372 ) ) ;
#65239 = ORIENTED_EDGE ( 'NONE', *, *, #42377, .F. ) ;
#65240 = EDGE_CURVE ( 'NONE', #35732, #90334, #30877, .T. ) ;
#65241 = CARTESIAN_POINT ( 'NONE',  ( 30.18562306610639112, 29.37878583063842441, 9.188101187500006262 ) ) ;
#65242 = LINE ( 'NONE', #71363, #57567 ) ;
#65243 = AXIS2_PLACEMENT_3D ( 'NONE', #40373, #56066, #86552 ) ;
#65244 = EDGE_CURVE ( 'NONE', #21644, #67514, #46558, .T. ) ;
#65245 = CARTESIAN_POINT ( 'NONE',  ( 162.8751945631634612, 272.8900720096677333, -16.40198242748087054 ) ) ;
#65246 = ORIENTED_EDGE ( 'NONE', *, *, #29271, .T. ) ;
#65247 = ORIENTED_EDGE ( 'NONE', *, *, #95333, .T. ) ;
#65248 = CARTESIAN_POINT ( 'NONE',  ( 186.1378587046176847, 298.7759093635723389, 1.082710523946170733 ) ) ;
#65250 = CARTESIAN_POINT ( 'NONE',  ( 148.2352135776142177, 273.8960739431854563, -9.245976304249309052 ) ) ;
#65249 = CARTESIAN_POINT ( 'NONE',  ( 163.9704062730716032, 246.6419207277664327, 7.317582738093436845 ) ) ;
#65251 = CARTESIAN_POINT ( 'NONE',  ( 85.76586952047404111, 48.61475482067446308, -11.85709152719317139 ) ) ;
#65252 = DIRECTION ( 'NONE',  ( 0.5000000000000002220, -0.8660254037844385966, 9.251858538542986372E-17 ) ) ;
#65253 = AXIS2_PLACEMENT_3D ( 'NONE', #69689, #23081, #24586 ) ;
#65254 = CARTESIAN_POINT ( 'NONE',  ( -19.57831724403558837, 92.94455521224399774, 59.99999999999999289 ) ) ;
#65255 = DIRECTION ( 'NONE',  ( 0.5000000000000014433, -0.8660254037844378194, 0.000000000000000000 ) ) ;
#65257 = EDGE_CURVE ( 'NONE', #28901, #85997, #62760, .T. ) ;
#65256 = CARTESIAN_POINT ( 'NONE',  ( 164.7586010964001844, 245.2767272474987408, 5.149004892315893755 ) ) ;
#65258 = CARTESIAN_POINT ( 'NONE',  ( 47.05668214639808156, 76.45164061169337799, -10.00000000000000000 ) ) ;
#65259 = FACE_OUTER_BOUND ( 'NONE', #42017, .T. ) ;
#65260 = CARTESIAN_POINT ( 'NONE',  ( 103.7194723697636221, 236.8149278399160949, -9.188101187500095079 ) ) ;
#65261 = ORIENTED_EDGE ( 'NONE', *, *, #33829, .F. ) ;
#65262 = CARTESIAN_POINT ( 'NONE',  ( 73.83780735420440067, 55.05980088889993596, -16.60220836681794054 ) ) ;
#65263 = DIRECTION ( 'NONE',  ( -0.9862134920484688649, -0.1654779384134468789, 0.000000000000000000 ) ) ;
#65264 = CARTESIAN_POINT ( 'NONE',  ( 166.3892922564430705, 279.1128815750697640, -13.41989996223110282 ) ) ;
#65265 = ORIENTED_EDGE ( 'NONE', *, *, #59265, .T. ) ;
#65266 = EDGE_LOOP ( 'NONE', ( #24982, #65147 ) ) ;
#65267 = CARTESIAN_POINT ( 'NONE',  ( 87.17617632782311432, 45.93339551703158463, -8.679440343565334004 ) ) ;
#65268 = ADVANCED_FACE ( 'NONE', ( #23261 ), #47566, .T. ) ;
#65269 = CARTESIAN_POINT ( 'NONE',  ( 180.0871239489544848, 293.6764218470086689, -2.637204768131844013 ) ) ;
#65270 = CARTESIAN_POINT ( 'NONE',  ( 84.83489698312170901, 42.27858766766668452, -0.5892840222501907199 ) ) ;
#65271 = DIRECTION ( 'NONE',  ( 0.4552093898365224267, -0.8903844177683372108, 0.000000000000000000 ) ) ;
#65272 = LINE ( 'NONE', #19204, #94918 ) ;
#65273 = EDGE_CURVE ( 'NONE', #69721, #63278, #80660, .T. ) ;
#65274 = CARTESIAN_POINT ( 'NONE',  ( 98.68587325814904432, 227.7833772461660544, -9.188101187500095079 ) ) ;
#65275 = ORIENTED_EDGE ( 'NONE', *, *, #5997, .F. ) ;
#65276 =( BOUNDED_CURVE ( )  B_SPLINE_CURVE ( 2, ( #550, #31431, #55713, #59, #48143, #9670, #62324, #79087, #92778 ),
 .UNSPECIFIED., .F., .T. ) 
 B_SPLINE_CURVE_WITH_KNOTS ( ( 3, 2, 2, 2, 3 ),
 ( 0.5120967741935483764, 0.5134408602150537515, 0.5161290322580645018, 0.5188172043010752521, 0.5201612903225806273 ),
 .UNSPECIFIED. ) 
 CURVE ( )  GEOMETRIC_REPRESENTATION_ITEM ( )  RATIONAL_B_SPLINE_CURVE ( ( 0.9330127018922194093, 0.9330127018922194093, 1.000000000000000000, 0.8660254037844387076, 1.000000000000000000, 0.8660254037844387076, 1.000000000000000000, 0.9330127018922194093, 0.9330127018922194093 ) ) 
 REPRESENTATION_ITEM ( '' )  );
#65277 = ORIENTED_EDGE ( 'NONE', *, *, #47881, .F. ) ;
#65278 = CARTESIAN_POINT ( 'NONE',  ( 169.7005567072155259, 288.7155782076579271, 4.430715832634252394 ) ) ;
#65279 = CARTESIAN_POINT ( 'NONE',  ( 207.6523394534040392, 270.9825930866021508, -2.115019688068903392 ) ) ;
#65280 = VERTEX_POINT ( 'NONE', #979 ) ;
#65281 = CARTESIAN_POINT ( 'NONE',  ( 23.18815102787819171, 35.16126292948896293, -6.180339887498951690 ) ) ;
#65282 = PLANE ( 'NONE',  #23538 ) ;
#65283 = CARTESIAN_POINT ( 'NONE',  ( 68.87368469670209947, 69.23618240007901647, -5.598517026418342368 ) ) ;
#65285 = CARTESIAN_POINT ( 'NONE',  ( 69.66171794495750191, 62.30057999729555718, -13.54004527842230488 ) ) ;
#65284 = CARTESIAN_POINT ( 'NONE',  ( 139.9303331133829715, 251.5958772461660544, -9.188101187500095079 ) ) ;
#65286 = CARTESIAN_POINT ( 'NONE',  ( -9.233521592304517966, 172.1427522451419065, 10.00000000000009237 ) ) ;
#65287 = FACE_OUTER_BOUND ( 'NONE', #74217, .T. ) ;
#65288 = EDGE_LOOP ( 'NONE', ( #86492, #14394, #50346, #3365 ) ) ;
#65289 = B_SPLINE_CURVE_WITH_KNOTS ( 'NONE', 3,
 ( #13074, #36341, #99159, #53532, #76365, #21653, #20661, #90604, #30244, #15025, #60619, #6937, #6455, #29747, #68735, #83486, #75877, #37333, #14052, #45917, #61125, #98173, #13566, #67243, #44437, #5950, #98676, #21170, #82989, #68236, #91574, #51550, #76835, #22146, #7433, #22647, #38326, #69233, #100163, #30749, #82512, #74874, #5457, #48443, #93062, #55026 ),
 .UNSPECIFIED., .F., .F.,
 ( 4, 1, 2, 2, 1, 2, 2, 1, 1, 2, 2, 1, 1, 2, 2, 1, 1, 2, 2, 1, 1, 1, 2, 2, 1, 1, 1, 2, 2, 4 ),
 ( 0.000000000000000000, 0.06249999999999364397, 0.09374999999999052147, 0.1249999999999873990, 0.1874999999999764910, 0.2187499999999706346, 0.2499999999999647504, 0.3124999999999538147, 0.3437499999999505951, 0.3593749999999505396, 0.3749999999999504285, 0.4374999999999527600, 0.4687499999999538702, 0.4843749999999560352, 0.4999999999999581446, 0.5624999999999705791, 0.5937499999999786837, 0.6093749999999810152, 0.6249999999999832356, 0.6874999999999926725, 0.7187499999999995559, 0.7343750000000008882, 0.7421875000000018874, 0.7500000000000028866, 0.8125000000000117684, 0.8437500000000146549, 0.8593750000000178746, 0.8671875000000195399, 0.8750000000000210942, 1.000000000000000000 ),
 .UNSPECIFIED. ) ;
#65290 = CARTESIAN_POINT ( 'NONE',  ( 157.1184542243154567, 258.5098498072379698, 16.84490127433854667 ) ) ;
#65291 = CARTESIAN_POINT ( 'NONE',  ( 160.3188448450098065, 275.5225805274294544, 12.83265129500923685 ) ) ;
#65292 = EDGE_CURVE ( 'NONE', #49291, #63028, #81474, .T. ) ;
#65293 = CARTESIAN_POINT ( 'NONE',  ( 82.75024023773026727, 40.61788017064008471, -1.390363622740588223 ) ) ;
#65294 = CARTESIAN_POINT ( 'NONE',  ( 188.9450937826650545, 269.5268139213692962, 14.88809917091533741 ) ) ;
#65295 = CARTESIAN_POINT ( 'NONE',  ( 45.03194321908421927, 185.2592609112380160, 2.679491924311254714 ) ) ;
#65296 = DIRECTION ( 'NONE',  ( -0.000000000000000000, -0.000000000000000000, -1.000000000000000000 ) ) ;
#65297 = DIRECTION ( 'NONE',  ( -0.8099771808667527440, -0.5864613938488599798, 0.000000000000000000 ) ) ;
#65298 = DIRECTION ( 'NONE',  ( -0.000000000000000000, 0.000000000000000000, -1.000000000000000000 ) ) ;
#65299 = EDGE_CURVE ( 'NONE', #44213, #66291, #37164, .T. ) ;
#65300 = CARTESIAN_POINT ( 'NONE',  ( 80.89006754182553038, 55.13283443129127193, 15.96266433881070945 ) ) ;
#65301 = CARTESIAN_POINT ( 'NONE',  ( 66.59659379507385779, 69.02878726636450324, -0.1500247100265385269 ) ) ;
#65302 = CARTESIAN_POINT ( 'NONE',  ( 160.0061168334508750, 253.5082714530983026, -16.02306982074888708 ) ) ;
#65303 = CARTESIAN_POINT ( 'NONE',  ( 83.38047668388445288, 51.78471284047383705, 14.96842148903410497 ) ) ;
#65304 = CARTESIAN_POINT ( 'NONE',  ( 163.1096928939807924, 248.1327200311062882, -9.690381021358412283 ) ) ;
#65305 = DIRECTION ( 'NONE',  ( -0.8660254037844387076, -0.4999999999999998890, -0.000000000000000000 ) ) ;
#65306 = EDGE_CURVE ( 'NONE', #50951, #17891, #1601, .T. ) ;
#65307 = CARTESIAN_POINT ( 'NONE',  ( 71.28050843997250752, 64.71893044897940683, -12.66255568095732897 ) ) ;
#65309 = CARTESIAN_POINT ( 'NONE',  ( 190.9474291326297930, 266.7645650087163745, -12.82661358031884546 ) ) ;
#65308 = CARTESIAN_POINT ( 'NONE',  ( 177.7502759686835816, 264.9915612121205299, -15.08494360417384961 ) ) ;
#65310 = ADVANCED_FACE ( 'NONE', ( #50071 ), #80519, .F. ) ;
#65311 = CARTESIAN_POINT ( 'NONE',  ( 182.4009855739953991, 264.2690820246323256, -14.57423425229302438 ) ) ;
#65312 = CARTESIAN_POINT ( 'NONE',  ( 35.64779661956466583, 28.78052372038643369, -10.00000000000000355 ) ) ;
#65313 = B_SPLINE_CURVE_WITH_KNOTS ( 'NONE', 3,
 ( #5535, #91165, #22735, #36419 ),
 .UNSPECIFIED., .F., .F.,
 ( 4, 4 ),
 ( 0.007625806130884848696, 0.01343629536117592511 ),
 .UNSPECIFIED. ) ;
#65314 = CARTESIAN_POINT ( 'NONE',  ( 99.70756906128829655, 216.8262482093457493, 3.021315404115420679E-15 ) ) ;
#65315 = LINE ( 'NONE', #96254, #70221 ) ;
#65316 = CARTESIAN_POINT ( 'NONE',  ( 160.7004439013812487, 272.9463992000354438, -14.94530573250521144 ) ) ;
#65317 = CARTESIAN_POINT ( 'NONE',  ( 86.28849223104248267, 43.59502242935581506, -3.924905614730060499 ) ) ;
#65318 = CARTESIAN_POINT ( 'NONE',  ( 14.24839638916628459, 179.0333772461660544, 9.188101187500095079 ) ) ;
#65319 = AXIS2_PLACEMENT_3D ( 'NONE', #9516, #26699, #73799 ) ;
#65320 = CARTESIAN_POINT ( 'NONE',  ( 83.11190622883978563, 51.97173441866404886, 14.72729092114622063 ) ) ;
#65321 = ORIENTED_EDGE ( 'NONE', *, *, #87184, .F. ) ;
#65323 = CARTESIAN_POINT ( 'NONE',  ( 86.63801457440831655, 46.38311672867401114, 9.077114030922938781 ) ) ;
#65322 = VECTOR ( 'NONE', #6919, 1000.000000000000227 ) ;
#65324 = CARTESIAN_POINT ( 'NONE',  ( 186.0400780920065529, 271.7087950812899066, 16.90619359840448510 ) ) ;
#65325 = FACE_OUTER_BOUND ( 'NONE', #11639, .T. ) ;
#65326 = CARTESIAN_POINT ( 'NONE',  ( 39.55283647781661216, 184.4548013555409796, -4.594050593750042211 ) ) ;
#65327 = CARTESIAN_POINT ( 'NONE',  ( 87.01945182987638816, 46.04471723482853918, 8.958281803387862396 ) ) ;
#65328 = CARTESIAN_POINT ( 'NONE',  ( 147.5634954182374372, 275.0595239235922236, 4.682022975662822439 ) ) ;
#65329 = CARTESIAN_POINT ( 'NONE',  ( 37.17256469204938440, 37.16454794089044356, -10.00000000000000355 ) ) ;
#65330 = CARTESIAN_POINT ( 'NONE',  ( 180.5087874685112581, 292.9443678237462336, 6.144088910392417446 ) ) ;
#65331 = CARTESIAN_POINT ( 'NONE',  ( 146.6138605399200117, 276.7043397814778132, -0.5394499176159462950 ) ) ;
#65332 = DIRECTION ( 'NONE',  ( 0.9954067278227226589, -0.09573633691164461224, 0.000000000000000000 ) ) ;
#65333 = CARTESIAN_POINT ( 'NONE',  ( 81.34546223144695887, 42.12293715088343760, 8.018599761840913942 ) ) ;
#65334 = PRODUCT ( 'Middle Movable Base', 'Middle Movable Base', '', ( #60334 ) ) ;
#65335 = CARTESIAN_POINT ( 'NONE',  ( 87.11953417171658032, 46.01840446382728800, -8.187078523733017477 ) ) ;
#65336 = CARTESIAN_POINT ( 'NONE',  ( 46.22371820283660782, 112.7232458147606451, 10.00000000000000000 ) ) ;
#65337 = CARTESIAN_POINT ( 'NONE',  ( 87.63003801413758254, 45.43815880539863628, -6.688036734344514400 ) ) ;
#65338 = CARTESIAN_POINT ( 'NONE',  ( 74.50030963965132003, 220.4865022471902876, -10.00000000000009415 ) ) ;
#65339 = CARTESIAN_POINT ( 'NONE',  ( 74.90746300446748762, 65.80853403655308398, -13.37832520640001910 ) ) ;
#65340 = CARTESIAN_POINT ( 'NONE',  ( 162.2378898886269951, 268.0060074806465309, -16.71809273753259717 ) ) ;
#65341 = CARTESIAN_POINT ( 'NONE',  ( 51.59574192737019160, 200.5958772461660544, -9.188101187500095079 ) ) ;
#65342 = ORIENTED_EDGE ( 'NONE', *, *, #97782, .T. ) ;
#65343 = CARTESIAN_POINT ( 'NONE',  ( 179.0484917649878298, 259.9789987921100192, 12.89662402083353854 ) ) ;
#65344 = CARTESIAN_POINT ( 'NONE',  ( 147.0670278774466908, 275.9194309285509235, 3.666898409139099257 ) ) ;
#65345 = CARTESIAN_POINT ( 'NONE',  ( 67.25058181848319805, 66.49012357423811181, -8.666073719759312510 ) ) ;
#65346 = ORIENTED_EDGE ( 'NONE', *, *, #91412, .T. ) ;
#65347 = CARTESIAN_POINT ( 'NONE',  ( 170.8335652545856362, 286.3135742921572273, 7.469445898408281437 ) ) ;
#65348 = CARTESIAN_POINT ( 'NONE',  ( 207.5338226493333025, 271.1878702128032614, 6.432541580693135863 ) ) ;
#65349 = CYLINDRICAL_SURFACE ( 'NONE', #50928, 7.273499999999997634 ) ;
#65350 = CARTESIAN_POINT ( 'NONE',  ( 25.85549604718420014, 26.87878583063842797, -9.188101187500006262 ) ) ;
#65351 = CARTESIAN_POINT ( 'NONE',  ( 186.8024928136323695, 263.1790814610873213, 11.56963523927125337 ) ) ;
#65352 = CARTESIAN_POINT ( 'NONE',  ( 86.53352045429423356, 47.35036163402705967, -10.26701049652133513 ) ) ;
#65353 = CARTESIAN_POINT ( 'NONE',  ( -64.94778771796556782, 41.33875607593969193, -10.00000000000000000 ) ) ;
#65354 = ORIENTED_EDGE ( 'NONE', *, *, #69079, .F. ) ;
#65355 = CARTESIAN_POINT ( 'NONE',  ( 13.17245041747802148, 29.64646525600389637, -2.839279412974133887 ) ) ;
#65356 = DIRECTION ( 'NONE',  ( 0.5000000000000001110, -0.8660254037844384856, -0.000000000000000000 ) ) ;
#65357 = DIRECTION ( 'NONE',  ( -1.000000000000000000, 4.892646582057456999E-14, 0.000000000000000000 ) ) ;
#65358 = DIRECTION ( 'NONE',  ( -0.09274582908234026146, -0.9956898167541081701, 0.000000000000000000 ) ) ;
#65359 = ORIENTED_EDGE ( 'NONE', *, *, #82586, .T. ) ;
#65360 = DIRECTION ( 'NONE',  ( 0.4999999999999998890, -0.8660254037844385966, 0.000000000000000000 ) ) ;
#65361 = CARTESIAN_POINT ( 'NONE',  ( 151.2648146047323507, 268.6486510375538614, 15.71323890031163550 ) ) ;
#65362 = CARTESIAN_POINT ( 'NONE',  ( 177.3160476213384982, 256.0269507273385443, -7.165014414593925629 ) ) ;
#65363 = DIRECTION ( 'NONE',  ( -0.9981117208278907915, 0.06142469166374903145, 0.000000000000000000 ) ) ;
#65364 = ORIENTED_EDGE ( 'NONE', *, *, #79642, .F. ) ;
#65365 = ORIENTED_EDGE ( 'NONE', *, *, #54147, .F. ) ;
#65367 = CARTESIAN_POINT ( 'NONE',  ( 151.3023505463322067, 269.2715888188440090, -14.21498388727478535 ) ) ;
#65366 = CARTESIAN_POINT ( 'NONE',  ( 207.8575108622103755, 270.6272257822888037, -6.381720258959569847 ) ) ;
#65368 = CARTESIAN_POINT ( 'NONE',  ( 184.3388797322841981, 264.0495600577374375, -13.68812008961389282 ) ) ;
#65369 = ORIENTED_EDGE ( 'NONE', *, *, #58243, .F. ) ;
#65370 = DIRECTION ( 'NONE',  ( -0.000000000000000000, -0.000000000000000000, -1.000000000000000000 ) ) ;
#65371 = CARTESIAN_POINT ( 'NONE',  ( 159.4230536986738400, 254.5181664265525683, 16.83068086755798376 ) ) ;
#65372 = CARTESIAN_POINT ( 'NONE',  ( 156.6812872898450735, 261.2670451491295012, 0.000000000000000000 ) ) ;
#65373 = CARTESIAN_POINT ( 'NONE',  ( 78.08206365161463225, 61.83366292688850052, -15.70979438352861379 ) ) ;
#65374 = CARTESIAN_POINT ( 'NONE',  ( 204.6075833744878878, 276.2562653119390461, -13.34672481898815910 ) ) ;
#65376 = ADVANCED_FACE ( 'NONE', ( #11094 ), #72401, .T. ) ;
#65375 = CARTESIAN_POINT ( 'NONE',  ( 115.2218061334819623, 228.1423013555409796, -4.594050593750043987 ) ) ;
#65377 = CARTESIAN_POINT ( 'NONE',  ( -73.83803415018344651, 50.74234351129840093, -10.00000000000000000 ) ) ;
#65378 = EDGE_LOOP ( 'NONE', ( #93723, #72515, #96016, #53988 ) ) ;
#65379 = CARTESIAN_POINT ( 'NONE',  ( 163.8455942243524248, 246.8581015375447691, -7.178103170949780676 ) ) ;
#65380 = ORIENTED_EDGE ( 'NONE', *, *, #28700, .F. ) ;
#65381 = CARTESIAN_POINT ( 'NONE',  ( 32.39821438149254362, 40.74646525600392977, 2.839279412974139660 ) ) ;
#65382 = CARTESIAN_POINT ( 'NONE',  ( 159.4889735931715222, 254.4039898200529706, 16.88104032092801887 ) ) ;
#65383 = CARTESIAN_POINT ( 'NONE',  ( 78.19930204122441353, 47.67057537844316784, -14.46097917792036647 ) ) ;
#65384 = CARTESIAN_POINT ( 'NONE',  ( 70.26924114858965709, 217.5024278399160664, -9.188101187500093303 ) ) ;
#65385 = ADVANCED_FACE ( 'NONE', ( #95228 ), #85500, .T. ) ;
#65386 = CARTESIAN_POINT ( 'NONE',  ( -30.41973204483513982, 95.86956414332775012, 12.73750267444827422 ) ) ;
#65387 = CARTESIAN_POINT ( 'NONE',  ( 151.0036289208911171, 269.1010379121764799, 14.24595189915657478 ) ) ;
#65388 = CARTESIAN_POINT ( 'NONE',  ( 201.7511365947159163, 271.6656860447648114, 11.60973541740156101 ) ) ;
#65389 = CARTESIAN_POINT ( 'NONE',  ( 175.6541281476291090, 278.4009151887023563, 16.88439838973073037 ) ) ;
#65390 = EDGE_CURVE ( 'NONE', #19593, #78035, #69245, .T. ) ;
#65391 = ORIENTED_EDGE ( 'NONE', *, *, #98351, .F. ) ;
#65392 = AXIS2_PLACEMENT_3D ( 'NONE', #409, #17097, #47995 ) ;
#65393 = CARTESIAN_POINT ( 'NONE',  ( 33.63407072503001416, 49.62913085183823370, -10.00000000000000000 ) ) ;
#65394 = CARTESIAN_POINT ( 'NONE',  ( 87.42296356251033274, 43.77044090453171776, -1.503769482561249538 ) ) ;
#65395 = CARTESIAN_POINT ( 'NONE',  ( 155.5587153255869453, 261.2113968263770971, -18.30500480654006878 ) ) ;
#65396 = ORIENTED_EDGE ( 'NONE', *, *, #41544, .F. ) ;
#65397 = CARTESIAN_POINT ( 'NONE',  ( 194.9643996604583833, 292.9587494513586989, 15.17976699960614440 ) ) ;
#65398 = FACE_OUTER_BOUND ( 'NONE', #44458, .T. ) ;
#65399 = DIRECTION ( 'NONE',  ( 0.5000000000000013323, -0.8660254037844378194, 0.000000000000000000 ) ) ;
#65400 = CARTESIAN_POINT ( 'NONE',  ( 70.10597207235390727, 222.8297689869269220, -2.679491924311252493 ) ) ;
#65401 = VECTOR ( 'NONE', #42318, 1000.000000000000114 ) ;
#65402 = CARTESIAN_POINT ( 'NONE',  ( 190.1519139143167081, 301.2942192743771557, 4.481136594690903863 ) ) ;
#65403 = CARTESIAN_POINT ( 'NONE',  ( 177.1262862392189845, 269.6057104283654553, 17.56656865388298172 ) ) ;
#65404 = CARTESIAN_POINT ( 'NONE',  ( 164.7462163020046262, 245.2981783406326599, 1.451255823150352064 ) ) ;
#65405 = DIRECTION ( 'NONE',  ( 0.5000000000000002220, -0.8660254037844385966, 9.251858538542986372E-17 ) ) ;
#65406 = CARTESIAN_POINT ( 'NONE',  ( 167.3995633324949210, 256.4415895850399352, 13.70966202949693091 ) ) ;
#65407 = CARTESIAN_POINT ( 'NONE',  ( 1.210598108517954463, 183.0530062829863596, 2.649461200531984646E-14 ) ) ;
#65408 = CARTESIAN_POINT ( 'NONE',  ( 129.3218690127885964, 233.2202760586659736, -5.415160957724236172E-17 ) ) ;
#65409 = ORIENTED_EDGE ( 'NONE', *, *, #32108, .T. ) ;
#65410 = CARTESIAN_POINT ( 'NONE',  ( 86.75859043018910199, 44.26021819578813421, -5.163563606523318583 ) ) ;
#65411 = CARTESIAN_POINT ( 'NONE',  ( -53.68831936616819434, 31.89637462494507147, 10.00000000000000000 ) ) ;
#65412 = APPLICATION_CONTEXT ( 'automotive_design' ) ;
#65413 = DIRECTION ( 'NONE',  ( -1.000000000000000000, 0.000000000000000000, 0.000000000000000000 ) ) ;
#65414 = CARTESIAN_POINT ( 'NONE',  ( 164.3853877993040840, 245.9231516401292197, 5.995325337583643943 ) ) ;
#65415 = CARTESIAN_POINT ( 'NONE',  ( 75.37392722170159232, 64.45239491791643616, 14.26364343640139332 ) ) ;
#65416 = DIRECTION ( 'NONE',  ( 0.000000000000000000, 0.000000000000000000, 1.000000000000000000 ) ) ;
#65417 = ORIENTED_EDGE ( 'NONE', *, *, #53760, .F. ) ;
#65418 = CARTESIAN_POINT ( 'NONE',  ( 48.53010236944520273, 101.9116055364396090, -10.00000000000000000 ) ) ;
#65419 = EDGE_CURVE ( 'NONE', #18680, #21764, #2874, .T. ) ;
#65420 = CARTESIAN_POINT ( 'NONE',  ( 183.8037341582430884, 275.4624792557407318, 17.77592483611231700 ) ) ;
#65421 = CYLINDRICAL_SURFACE ( 'NONE', #95339, 10.00000000000001066 ) ;
#65422 = CARTESIAN_POINT ( 'NONE',  ( 164.2960764465929060, 246.0778434407177713, -1.520364048796653877 ) ) ;
#65423 = CARTESIAN_POINT ( 'NONE',  ( 148.6720373546558847, 247.4548013555409796, -4.594050593750042211 ) ) ;
#65424 = CARTESIAN_POINT ( 'NONE',  ( 20.80673460501611771, 189.4865022471903160, 10.00000000000009415 ) ) ;
#65425 = ADVANCED_FACE ( 'NONE', ( #27774 ), #24000, .F. ) ;
#65426 = DIRECTION ( 'NONE',  ( 0.04218457335174655848, 0.9991098346884246251, 0.000000000000000000 ) ) ;
#65427 = CARTESIAN_POINT ( 'NONE',  ( 174.6584545799940145, 251.8359307791901927, 3.578998500653847614 ) ) ;
#65428 = EDGE_CURVE ( 'NONE', #73620, #66637, #51465, .T. ) ;
#65429 = CARTESIAN_POINT ( 'NONE',  ( 22.49950015666239622, 18.15404122711133539, 8.090169943749479842 ) ) ;
#65430 = CARTESIAN_POINT ( 'NONE',  ( 149.1903793729515257, 272.2416782560088677, 12.95958987445043675 ) ) ;
#65431 = CARTESIAN_POINT ( 'NONE',  ( 155.2991919149069133, 279.6252298253222079, -1.573765988037651553 ) ) ;
#65432 = CARTESIAN_POINT ( 'NONE',  ( 169.8115178593924099, 285.4166933214704045, -7.965421809193424352 ) ) ;
#65433 = CARTESIAN_POINT ( 'NONE',  ( 7.225231395932167899, 28.43104314603600358, 10.00000000000000000 ) ) ;
#65434 = CARTESIAN_POINT ( 'NONE',  ( 157.4774070382625837, 270.9583249496453163, -14.71635891169374943 ) ) ;
#65435 = CARTESIAN_POINT ( 'NONE',  ( 133.6606700321278822, 254.6427522451419065, 10.00000000000009237 ) ) ;
#65436 = CARTESIAN_POINT ( 'NONE',  ( 173.1778226176500084, 284.7536295044762369, -13.02365280795374858 ) ) ;
#65437 = VERTEX_POINT ( 'NONE', #23633 ) ;
#65438 = CARTESIAN_POINT ( 'NONE',  ( 196.4390255720217908, 290.4046224503736653, 16.34739044515864848 ) ) ;
#65439 = CARTESIAN_POINT ( 'NONE',  ( 148.2159754900428936, 273.9293952882992471, 9.267836332806297150 ) ) ;
#65440 = CARTESIAN_POINT ( 'NONE',  ( 0.1486806056246424423, 161.7048013555410080, 4.594050593750051981 ) ) ;
#65441 = CARTESIAN_POINT ( 'NONE',  ( 39.95835201613431309, 200.0024278399160949, 9.188101187500095079 ) ) ;
#65442 = CARTESIAN_POINT ( 'NONE',  ( 178.8711053662235599, 258.8915962790593994, -11.54485168611661194 ) ) ;
#65443 = CARTESIAN_POINT ( 'NONE',  ( 15.67984500357415278, 27.79103043416548502, 8.090169943749478065 ) ) ;
#65444 = CARTESIAN_POINT ( 'NONE',  ( 88.19107160583139660, 43.69314304319705400, 0.1842422985582093387 ) ) ;
#65445 = DIRECTION ( 'NONE',  ( 0.9659258262890740854, -0.2588190451024993677, 8.659560562354725782E-17 ) ) ;
#65446 = CARTESIAN_POINT ( 'NONE',  ( 72.23440922827423094, 71.91206544914358290, -3.821601542290089970 ) ) ;
#65447 = CARTESIAN_POINT ( 'NONE',  ( 190.1696443193688708, 301.2635093119881162, -4.804312979389741223 ) ) ;
#65448 = CARTESIAN_POINT ( 'NONE',  ( 73.77371296639375942, 55.45649524975051037, -16.58834881926898674 ) ) ;
#65450 = CARTESIAN_POINT ( 'NONE',  ( 69.64695893572810803, 221.0177522451419065, 5.000000000000046185 ) ) ;
#65449 = CARTESIAN_POINT ( 'NONE',  ( 71.81202244518924260, 212.2677522451418497, 10.00000000000009592 ) ) ;
#65451 = CARTESIAN_POINT ( 'NONE',  ( 76.30616544034060666, 50.97262258187969763, -15.53540872755634439 ) ) ;
#65452 = CARTESIAN_POINT ( 'NONE',  ( 29.18428119120667574, 28.80066082961423390, 10.00000000000000533 ) ) ;
#65453 = CARTESIAN_POINT ( 'NONE',  ( 175.8939073520130592, 252.7054158260212375, 5.280091837693253964 ) ) ;
#65454 = VECTOR ( 'NONE', #83881, 1000.000000000000000 ) ;
#65455 = EDGE_CURVE ( 'NONE', #6076, #55290, #17368, .T. ) ;
#65456 = CARTESIAN_POINT ( 'NONE',  ( 181.6779078793408075, 294.9161590443458749, 1.016312488909408618 ) ) ;
#65457 = CARTESIAN_POINT ( 'NONE',  ( 52.05581792490468729, 190.8615022471902023, 5.000000000000051514 ) ) ;
#65458 = CARTESIAN_POINT ( 'NONE',  ( 184.8842770087186125, 293.8891543674287732, 9.635832499575185395 ) ) ;
#65459 = CARTESIAN_POINT ( 'NONE',  ( 163.1484656051875106, 248.0655637253488806, 9.714247672444804138 ) ) ;
#65460 = CARTESIAN_POINT ( 'NONE',  ( 6.400214715252306341, 168.3768266524160140, 9.188101187500098632 ) ) ;
#65461 = CARTESIAN_POINT ( 'NONE',  ( 36.24660459446916150, 29.43085787977765833, -9.188101187500008038 ) ) ;
#65463 = EDGE_CURVE ( 'NONE', #12604, #25883, #40322, .T. ) ;
#65462 = CARTESIAN_POINT ( 'NONE',  ( 163.8910887309009468, 247.2502849824839473, 6.562832656486317973 ) ) ;
#65464 = CARTESIAN_POINT ( 'NONE',  ( 4.102725850843912170, 28.55253618238880620, 10.00000000000000000 ) ) ;
#65465 = CARTESIAN_POINT ( 'NONE',  ( 29.46033357383057449, 37.98502408145594700, -5.678558825948271327 ) ) ;
#65466 = CARTESIAN_POINT ( 'NONE',  ( 156.2207618296380360, 261.2732867776778107, -17.42379591280306883 ) ) ;
#65467 = VECTOR ( 'NONE', #23495, 1000.000000000000000 ) ;
#65468 = CARTESIAN_POINT ( 'NONE',  ( 179.7401746537150871, 276.9590119395865031, 16.29634411216163414 ) ) ;
#65469 = CARTESIAN_POINT ( 'NONE',  ( 149.0203866098534888, 272.5361143586139860, -12.73049804737905255 ) ) ;
#65470 = CARTESIAN_POINT ( 'NONE',  ( 179.7646569558871192, 262.8383775195224530, -12.87982295168864866 ) ) ;
#65471 =( NAMED_UNIT ( * ) SI_UNIT ( $, .STERADIAN. ) SOLID_ANGLE_UNIT ( ) );
#65472 = CARTESIAN_POINT ( 'NONE',  ( 5.869580825389008716, 26.49540643055185996, 3.479690158560446702E-15 ) ) ;
#65473 = CARTESIAN_POINT ( 'NONE',  ( 165.6219050428149728, 285.3937648927450255, 0.4054896356418120629 ) ) ;
#65474 = CARTESIAN_POINT ( 'NONE',  ( 13.87187630571069086, 28.98502408145591502, -5.678558825948271327 ) ) ;
#65475 = CARTESIAN_POINT ( 'NONE',  ( 159.1821849787265535, 259.3862596468384254, 16.68185694244520079 ) ) ;
#65476 = CARTESIAN_POINT ( 'NONE',  ( 67.86860378221429357, 65.58690806574966814, -10.91583492536020294 ) ) ;
#65477 = VERTEX_POINT ( 'NONE', #62633 ) ;
#65478 = CARTESIAN_POINT ( 'NONE',  ( 159.8597520197352537, 253.7617827468940277, -16.74905990210778839 ) ) ;
#65479 = EDGE_LOOP ( 'NONE', ( #73638, #11964, #60850, #66129 ) ) ;
#65480 = CARTESIAN_POINT ( 'NONE',  ( 152.4260784792123218, 267.7455040185449775, 15.55703180322229429 ) ) ;
#65481 = CARTESIAN_POINT ( 'NONE',  ( 207.6007741873543750, 271.0719067473055475, 7.587922723682903658 ) ) ;
#65482 = CARTESIAN_POINT ( 'NONE',  ( 29.26302659224649361, 17.86426979415090699, -3.090169943749474069 ) ) ;
#65483 = CARTESIAN_POINT ( 'NONE',  ( 87.64408659938918333, 45.45982483689996911, 6.724836266884324232 ) ) ;
#65484 = ORIENTED_EDGE ( 'NONE', *, *, #56105, .F. ) ;
#65485 = ORIENTED_EDGE ( 'NONE', *, *, #13400, .F. ) ;
#65487 = FACE_OUTER_BOUND ( 'NONE', #1622, .T. ) ;
#65486 = CARTESIAN_POINT ( 'NONE',  ( 159.1467459328969483, 279.6928109942932110, -9.939058806323174622 ) ) ;
#65488 = CARTESIAN_POINT ( 'NONE',  ( 152.7153488183568300, 266.1362520814392951, 17.33540622643059237 ) ) ;
#65489 = ORIENTED_EDGE ( 'NONE', *, *, #60060, .F. ) ;
#65490 = CARTESIAN_POINT ( 'NONE',  ( 76.79044849124564109, 52.81680254209042857, 15.85812468158750654 ) ) ;
#65491 = CARTESIAN_POINT ( 'NONE',  ( -105.0000000000000000, 0.000000000000000000, 59.99999999999999289 ) ) ;
#65492 = VERTEX_POINT ( 'NONE', #84012 ) ;
#65493 = DIRECTION ( 'NONE',  ( -1.850371707708595795E-16, -7.401486830834383181E-16, 1.000000000000000000 ) ) ;
#65494 = CARTESIAN_POINT ( 'NONE',  ( 76.30616544034060666, 50.97262258187969763, -15.53540872755634439 ) ) ;
#65495 = CARTESIAN_POINT ( 'NONE',  ( 35.43895548624276159, 201.2677522451419350, -5.000000000000047962 ) ) ;
#65496 = VECTOR ( 'NONE', #35817, 1000.000000000000000 ) ;
#65497 = VERTEX_POINT ( 'NONE', #357 ) ;
#65498 = CARTESIAN_POINT ( 'NONE',  ( 200.7523954295751594, 282.9336467052548869, 18.23634913067694185 ) ) ;
#65499 = CARTESIAN_POINT ( 'NONE',  ( 168.7291386885503641, 276.2063200971475112, -16.27615330769202728 ) ) ;
#65500 = CARTESIAN_POINT ( 'NONE',  ( 73.26674808670287575, 57.93223743048974939, 15.81806325431525373 ) ) ;
#65501 = ORIENTED_EDGE ( 'NONE', *, *, #53579, .T. ) ;
#65502 = FACE_OUTER_BOUND ( 'NONE', #94704, .T. ) ;
#65503 = DIRECTION ( 'NONE',  ( -1.000000000000000000, 0.000000000000000000, 0.000000000000000000 ) ) ;
#65504 = ORIENTED_EDGE ( 'NONE', *, *, #61885, .F. ) ;
#65505 = ADVANCED_FACE ( 'NONE', ( #6955 ), #99195, .F. ) ;
#65506 = CARTESIAN_POINT ( 'NONE',  ( 46.74164954608104239, 27.39040679176987325, -6.890680421881970419E-14 ) ) ;
#65507 = ORIENTED_EDGE ( 'NONE', *, *, #82257, .F. ) ;
#65508 = EDGE_CURVE ( 'NONE', #79283, #93301, #64154, .T. ) ;
#65509 = DIRECTION ( 'NONE',  ( 0.4999999999999998890, -0.8660254037844385966, 0.000000000000000000 ) ) ;
#65510 = EDGE_LOOP ( 'NONE', ( #46566, #59271, #39414, #95685 ) ) ;
#65511 = CARTESIAN_POINT ( 'NONE',  ( 168.8236688076963787, 272.7617961321510620, 16.01230988885185624 ) ) ;
#65512 = CARTESIAN_POINT ( 'NONE',  ( 147.5457841970795414, 275.0902006585022264, 5.820375447813823655 ) ) ;
#65513 = CARTESIAN_POINT ( 'NONE',  ( 180.1740792144395016, 291.5944223663697699, -9.968613414868679357 ) ) ;
#65514 = CARTESIAN_POINT ( 'NONE',  ( 69.93400769858298816, 66.24381931584940730, 10.75078203157522161 ) ) ;
#65515 = FACE_OUTER_BOUND ( 'NONE', #46927, .T. ) ;
#65516 = CARTESIAN_POINT ( 'NONE',  ( 86.41859815849130655, 43.12384784049413611, 0.4076689040990972845 ) ) ;
#65517 = CARTESIAN_POINT ( 'NONE',  ( 158.8485397013565148, 255.5132538595654808, -17.60067122166952913 ) ) ;
#65518 = EDGE_LOOP ( 'NONE', ( #98143, #89968 ) ) ;
#65519 = CARTESIAN_POINT ( 'NONE',  ( 13.52134341065866430, 31.30466486950697558, 0.000000000000000000 ) ) ;
#65520 = CARTESIAN_POINT ( 'NONE',  ( 20.10065364775352847, 33.64646525600390703, -2.839279412974133887 ) ) ;
#65521 = CARTESIAN_POINT ( 'NONE',  ( 164.3090168944849836, 246.0554299274959931, 2.641760039552302430 ) ) ;
#65522 = CARTESIAN_POINT ( 'NONE',  ( 206.5479446040613141, 272.8954610772809133, 10.74757481123993230 ) ) ;
#65524 = ORIENTED_EDGE ( 'NONE', *, *, #29297, .T. ) ;
#65523 = DIRECTION ( 'NONE',  ( -0.8660254037844387076, -0.4999999999999998890, -0.000000000000000000 ) ) ;
#65525 = VERTEX_POINT ( 'NONE', #56550 ) ;
#65526 = CARTESIAN_POINT ( 'NONE',  ( 146.6728205609862528, 276.6022180293756492, -3.499970163110023513 ) ) ;
#65527 = CYLINDRICAL_SURFACE ( 'NONE', #56170, 60.00000000000002132 ) ;
#65528 = CARTESIAN_POINT ( 'NONE',  ( 37.67689025969888661, 40.49103043416553049, -8.090169943749479842 ) ) ;
#65529 = DIRECTION ( 'NONE',  ( 0.000000000000000000, 0.000000000000000000, 1.000000000000000000 ) ) ;
#65530 = VECTOR ( 'NONE', #20806, 1000.000000000000000 ) ;
#65531 = CARTESIAN_POINT ( 'NONE',  ( 198.8804936074056400, 286.1758757680331087, -18.57050748239813487 ) ) ;
#65532 = CARTESIAN_POINT ( 'NONE',  ( 93.55286852290896604, 231.4865022471903444, 10.00000000000009415 ) ) ;
#65533 = EDGE_LOOP ( 'NONE', ( #12491, #47715, #67494, #73840 ) ) ;
#65534 = CARTESIAN_POINT ( 'NONE',  ( 167.6146168596400514, 252.8497314824998909, -12.44459218179994231 ) ) ;
#65535 = EDGE_CURVE ( 'NONE', #7154, #55615, #9464, .T. ) ;
#65536 = CARTESIAN_POINT ( 'NONE',  ( 60.85245129477298320, 194.3932355074535678, -2.679491924311248496 ) ) ;
#65537 = CARTESIAN_POINT ( 'NONE',  ( 164.4858674010174298, 245.7491158648375347, -2.958464974013825355 ) ) ;
#65538 = CARTESIAN_POINT ( 'NONE',  ( 32.84087927488953085, 179.7677522451417929, -5.000000000000041744 ) ) ;
#65539 = CARTESIAN_POINT ( 'NONE',  ( 103.0428032491157779, 239.4869531367911293, 4.594050593750046652 ) ) ;
#65540 = VECTOR ( 'NONE', #96288, 1000.000000000000000 ) ;
#65541 = CARTESIAN_POINT ( 'NONE',  ( 184.0050395437343980, 296.7880006952361214, -2.759016181532926382 ) ) ;
#65542 = CARTESIAN_POINT ( 'NONE',  ( 164.1364888002910618, 280.6458552486410554, -11.61947351137251516 ) ) ;
#65543 = CARTESIAN_POINT ( 'NONE',  ( 50.33662733789741139, 94.26254718190894266, 10.00000000000000000 ) ) ;
#65544 =( REPRESENTATION_RELATIONSHIP ('NONE','NONE', #67038, #88422 ) REPRESENTATION_RELATIONSHIP_WITH_TRANSFORMATION ( #30451 )SHAPE_REPRESENTATION_RELATIONSHIP( ) );
#65545 = CARTESIAN_POINT ( 'NONE',  ( 162.4198556707359842, 249.3275531507180460, 11.06129461055015106 ) ) ;
#65546 = CARTESIAN_POINT ( 'NONE',  ( 20.25662117580333188, 176.3768266524159856, -9.188101187500091527 ) ) ;
#65547 = CARTESIAN_POINT ( 'NONE',  ( 170.0754848107476960, 276.6018564280034866, -16.56579670670192073 ) ) ;
#65548 = ORIENTED_EDGE ( 'NONE', *, *, #64953, .T. ) ;
#65549 = EDGE_LOOP ( 'NONE', ( #32964, #29736, #5351, #60754 ) ) ;
#65550 = CARTESIAN_POINT ( 'NONE',  ( 185.8492146212669240, 258.6745004276652935, -5.862532207920108540 ) ) ;
#65551 = CARTESIAN_POINT ( 'NONE',  ( 87.91539880103944427, 43.93416759974002872, 0.4624922486833659696 ) ) ;
#65552 = CARTESIAN_POINT ( 'NONE',  ( 76.05733463510750880, 51.21219284135379013, 16.11160009721543318 ) ) ;
#65553 = CARTESIAN_POINT ( 'NONE',  ( 193.3495834857956481, 263.1287464498848294, -3.752072735475438847 ) ) ;
#65554 = CARTESIAN_POINT ( 'NONE',  ( 3.562051267137642085, 25.55466486950697558, -1.111400068045478839E-16 ) ) ;
#65555 =( BOUNDED_CURVE ( )  B_SPLINE_CURVE ( 2, ( #48390, #86447, #72208, #48894, #8882, #95029, #79333, #55460, #9903 ),
 .UNSPECIFIED., .F., .T. ) 
 B_SPLINE_CURVE_WITH_KNOTS ( ( 3, 2, 2, 2, 3 ),
 ( 0.9475806451612903691, 0.9489247311827957443, 0.9516129032258064946, 0.9543010752688172449, 0.9556451612903226200 ),
 .UNSPECIFIED. ) 
 CURVE ( )  GEOMETRIC_REPRESENTATION_ITEM ( )  RATIONAL_B_SPLINE_CURVE ( ( 0.9330127018922194093, 0.9330127018922194093, 1.000000000000000000, 0.8660254037844387076, 1.000000000000000000, 0.8660254037844387076, 1.000000000000000000, 0.9330127018922194093, 0.9330127018922194093 ) ) 
 REPRESENTATION_ITEM ( '' )  );
#65556 = CARTESIAN_POINT ( 'NONE',  ( 181.8556362198626175, 285.1488821084953429, 15.75693339034319251 ) ) ;
#65557 = CARTESIAN_POINT ( 'NONE',  ( 73.92441827737660276, 68.29833774401778612, -11.64939612493447996 ) ) ;
#65558 = CARTESIAN_POINT ( 'NONE',  ( 43.96406660440233338, 190.0643266524159856, -9.188101187500093303 ) ) ;
#65559 = CARTESIAN_POINT ( 'NONE',  ( 88.77168660263443201, 235.3927522451419634, 2.944929066748280225E-16 ) ) ;
#65560 = ORIENTED_EDGE ( 'NONE', *, *, #16226, .F. ) ;
#65561 = CARTESIAN_POINT ( 'NONE',  ( 79.09474592215634914, 60.19097512726884958, -16.45688605998253706 ) ) ;
#65562 = B_SPLINE_CURVE_WITH_KNOTS ( 'NONE', 3,
 ( #33632, #349, #48836, #25525 ),
 .UNSPECIFIED., .F., .F.,
 ( 4, 4 ),
 ( 0.01050920366396543466, 0.01592988117231719167 ),
 .UNSPECIFIED. ) ;
#65563 = CARTESIAN_POINT ( 'NONE',  ( 179.2174706742607952, 259.4863410742793235, -10.30736484160015465 ) ) ;
#65564 = EDGE_CURVE ( 'NONE', #73010, #3544, #20439, .T. ) ;
#65565 = VECTOR ( 'NONE', #16558, 1000.000000000000000 ) ;
#65566 = CARTESIAN_POINT ( 'NONE',  ( 2.394847222749281190, 166.0643266524160140, -9.188101187500093303 ) ) ;
#65567 = CARTESIAN_POINT ( 'NONE',  ( 68.71080560055042952, 64.06082602079280264, -12.00658928456073227 ) ) ;
#65568 = CARTESIAN_POINT ( 'NONE',  ( 73.49832466283049826, 68.39562707634591732, -11.34410690473859873 ) ) ;
#65569 = CARTESIAN_POINT ( 'NONE',  ( 181.5558742819051474, 255.2544784655372894, -2.503599602330015994 ) ) ;
#65570 = CARTESIAN_POINT ( 'NONE',  ( 193.1649355862271591, 296.0755126543221536, -12.21556774862162698 ) ) ;
#65571 = DIRECTION ( 'NONE',  ( -0.9182972510888884887, 0.3958915996110436430, 0.000000000000000000 ) ) ;
#65572 = CARTESIAN_POINT ( 'NONE',  ( 204.9608076533459950, 275.6444629144898499, 14.31488288944633069 ) ) ;
#65573 = CARTESIAN_POINT ( 'NONE',  ( 71.85869513609316073, 58.67586711399008692, -15.48493562761569287 ) ) ;
#65574 = CARTESIAN_POINT ( 'NONE',  ( 147.6088797830324779, 274.9809158978982850, 8.531536684623960198 ) ) ;
#65575 = ORIENTED_EDGE ( 'NONE', *, *, #96063, .T. ) ;
#65576 = CARTESIAN_POINT ( 'NONE',  ( 164.3602934812760452, 245.9666162739349318, -7.171958108566009571 ) ) ;
#65577 = CARTESIAN_POINT ( 'NONE',  ( 8.321535033790526725, 165.6115022471902023, -5.000000000000041744 ) ) ;
#65578 = CARTESIAN_POINT ( 'NONE',  ( 42.87900647455834502, 24.75620593066997444, 8.404119662683931360E-14 ) ) ;
#65579 = CARTESIAN_POINT ( 'NONE',  ( 119.6326891643026471, 246.0024278399160949, -9.188101187500093303 ) ) ;
#65580 = CARTESIAN_POINT ( 'NONE',  ( 14.99289142922413021, 26.84336893147755276, -7.433330006724137462 ) ) ;
#65581 = CARTESIAN_POINT ( 'NONE',  ( 74.78994931159289195, 67.11760897871008069, 12.96302903502454029 ) ) ;
#65582 = DIRECTION ( 'NONE',  ( 0.000000000000000000, 0.000000000000000000, 1.000000000000000000 ) ) ;
#65584 = CARTESIAN_POINT ( 'NONE',  ( 187.7402798015425844, 292.1894069392869824, 13.83160755710144052 ) ) ;
#65583 = DIRECTION ( 'NONE',  ( -0.000000000000000000, -0.000000000000000000, 1.000000000000000000 ) ) ;
#65585 = DIRECTION ( 'NONE',  ( -0.8660254037844379305, -0.5000000000000014433, -0.000000000000000000 ) ) ;
#65586 = ORIENTED_EDGE ( 'NONE', *, *, #35325, .F. ) ;
#65587 = CARTESIAN_POINT ( 'NONE',  ( 191.3375250863502970, 299.2406804863936145, 8.828791580707859410 ) ) ;
#65588 = CARTESIAN_POINT ( 'NONE',  ( 163.7818144303927284, 246.9685713811793164, 8.963733003589158699 ) ) ;
#65589 = CARTESIAN_POINT ( 'NONE',  ( 190.0601721553029222, 300.2863949309033842, 3.228815124723532382 ) ) ;
#65590 = CARTESIAN_POINT ( 'NONE',  ( 173.5762231131973010, 289.9594224631762813, -1.068267067776312196 ) ) ;
#65591 = CARTESIAN_POINT ( 'NONE',  ( 81.49556199178041993, 55.44509743070403118, -16.31886845347543513 ) ) ;
#65592 = EDGE_LOOP ( 'NONE', ( #73474, #12561, #26009, #65246 ) ) ;
#65593 = CARTESIAN_POINT ( 'NONE',  ( 73.95900928047775835, 65.06227567762803687, -13.94751918840041505 ) ) ;
#65594 = CARTESIAN_POINT ( 'NONE',  ( 165.4786559991963202, 269.4527545339830681, -16.40171962000061967 ) ) ;
#65595 = CARTESIAN_POINT ( 'NONE',  ( 82.99478726538977469, 41.85582147743899384, 4.139490622842754597 ) ) ;
#65596 = CARTESIAN_POINT ( 'NONE',  ( 80.41751025656814988, 56.26485224411339203, 16.12594336028984543 ) ) ;
#65597 = VECTOR ( 'NONE', #56098, 1000.000000000000000 ) ;
#65598 = CARTESIAN_POINT ( 'NONE',  ( 30.67581576542834654, 198.5177522451419350, 5.000000000000046185 ) ) ;
#65599 = CARTESIAN_POINT ( 'NONE',  ( 72.35257617177605027, 71.70739429922333841, -5.765621772327581773 ) ) ;
#65600 = CARTESIAN_POINT ( 'NONE',  ( 150.6217852516201106, 277.7502518432382885, -5.874856709598950559E-05 ) ) ;
#65601 = CARTESIAN_POINT ( 'NONE',  ( 194.5273606940714330, 283.0013335026653181, 17.66207452344210438 ) ) ;
#65602 = CARTESIAN_POINT ( 'NONE',  ( 12.53791098520745173, 8.208019796199266693, -3.090169943749474069 ) ) ;
#65603 = CARTESIAN_POINT ( 'NONE',  ( 186.1370921618058674, 283.3846817430978149, 17.26256540491417368 ) ) ;
#65604 = ORIENTED_EDGE ( 'NONE', *, *, #46516, .F. ) ;
#65605 = CARTESIAN_POINT ( 'NONE',  ( 167.7082397602646324, 281.0209505053426824, 12.79449922633788894 ) ) ;
#65606 = CARTESIAN_POINT ( 'NONE',  ( 194.4666154385731431, 293.8209370148700827, -14.56896502715340702 ) ) ;
#65607 = DIRECTION ( 'NONE',  ( -0.5888918169447132644, 0.8082118706970061739, 0.000000000000000000 ) ) ;
#65609 = ORIENTED_EDGE ( 'NONE', *, *, #68513, .F. ) ;
#65608 = AXIS2_PLACEMENT_3D ( 'NONE', #33712, #28086, #50387 ) ;
#65610 = CARTESIAN_POINT ( 'NONE',  ( 78.70340902619774681, 59.85553566278375115, 16.12483691164164412 ) ) ;
#65611 = CARTESIAN_POINT ( 'NONE',  ( 185.5891282490076435, 291.1072362729600513, 12.16301403431581818 ) ) ;
#65612 = DIRECTION ( 'NONE',  ( -0.5000000000000003331, 0.8660254037844383745, 0.000000000000000000 ) ) ;
#65613 = VERTEX_POINT ( 'NONE', #33781 ) ;
#65614 = CARTESIAN_POINT ( 'NONE',  ( 93.48972083544241229, 224.7833772461660260, -9.188101187500095079 ) ) ;
#65615 = CARTESIAN_POINT ( 'NONE',  ( 81.10660686981061929, 51.01353853940796768, -14.74231750527668261 ) ) ;
#65616 = CARTESIAN_POINT ( 'NONE',  ( 84.60739412327551179, 49.90025452092439906, -13.66407646797534703 ) ) ;
#65617 = CARTESIAN_POINT ( 'NONE',  ( 183.8303768749067899, 259.1719814329002816, -5.825300294667353995 ) ) ;
#65618 = ORIENTED_EDGE ( 'NONE', *, *, #62571, .T. ) ;
#65619 = EDGE_CURVE ( 'NONE', #37182, #19430, #64666, .T. ) ;
#65620 = CARTESIAN_POINT ( 'NONE',  ( 105.1540004908901693, 221.5177522451418213, 5.000000000000051514 ) ) ;
#65621 = ORIENTED_EDGE ( 'NONE', *, *, #58813, .T. ) ;
#65622 = CARTESIAN_POINT ( 'NONE',  ( 176.1640045926653499, 252.3529155287689321, -3.563159428949892682 ) ) ;
#65623 = VERTEX_POINT ( 'NONE', #18571 ) ;
#65624 = EDGE_CURVE ( 'NONE', #62997, #40327, #3384, .T. ) ;
#65625 = LINE ( 'NONE', #89013, #55680 ) ;
#65626 = CARTESIAN_POINT ( 'NONE',  ( 203.2187760522547819, 278.6617501559703101, -15.08675642319914978 ) ) ;
#65627 = VERTEX_POINT ( 'NONE', #10974 ) ;
#65628 = CARTESIAN_POINT ( 'NONE',  ( 206.8044235653369185, 272.4512264852788235, -7.311027623652901042 ) ) ;
#65629 = CARTESIAN_POINT ( 'NONE',  ( 151.3601338604896682, 268.8932253746694983, 14.28446672321297939 ) ) ;
#65630 = CARTESIAN_POINT ( 'NONE',  ( 158.6259107095311833, 274.9228465685866354, -12.63726120636060379 ) ) ;
#65631 = EDGE_CURVE ( 'NONE', #61239, #11450, #28132, .T. ) ;
#65632 = CARTESIAN_POINT ( 'NONE',  ( 200.6680263064462792, 283.0797783131037022, -17.21821073473145347 ) ) ;
#65633 = ADVANCED_FACE ( 'NONE', ( #37108 ), #21423, .F. ) ;
#65634 = CARTESIAN_POINT ( 'NONE',  ( 87.34642337659644795, 43.20430561321286689, -4.696387144280492735E-07 ) ) ;
#65635 = LINE ( 'NONE', #73747, #7857 ) ;
#65636 = CARTESIAN_POINT ( 'NONE',  ( 134.2197177853555843, 257.4869531367911577, 4.594050593750046652 ) ) ;
#65637 = EDGE_LOOP ( 'NONE', ( #53173, #9160 ) ) ;
#65638 = CARTESIAN_POINT ( 'NONE',  ( 75.67231652922859553, 54.75346391114741351, 16.12193936410828599 ) ) ;
#65639 = CARTESIAN_POINT ( 'NONE',  ( 9.471979480098337234, 23.65586893147754566, -7.433330006724137462 ) ) ;
#65640 = ORIENTED_EDGE ( 'NONE', *, *, #56188, .F. ) ;
#65641 = VECTOR ( 'NONE', #39607, 1000.000000000000114 ) ;
#65643 = VERTEX_POINT ( 'NONE', #68012 ) ;
#65642 = CARTESIAN_POINT ( 'NONE',  ( 204.0134405048271447, 271.6787652324207443, 9.733109749488880524 ) ) ;
#65644 = CARTESIAN_POINT ( 'NONE',  ( -46.35039662390601478, 28.35603213498495023, -10.00000000000000000 ) ) ;
#65645 = CARTESIAN_POINT ( 'NONE',  ( 170.7750159713022811, 288.2613212839527250, -5.614454501361259453 ) ) ;
#65646 = CARTESIAN_POINT ( 'NONE',  ( 153.3013304660010760, 276.9256174101875558, 7.023167453551987904 ) ) ;
#65647 = DIRECTION ( 'NONE',  ( 0.4999999999999992784, -0.8660254037844390407, 0.000000000000000000 ) ) ;
#65648 = VECTOR ( 'NONE', #73282, 1000.000000000000000 ) ;
#65649 = CARTESIAN_POINT ( 'NONE',  ( 192.6560709476634372, 292.3755120997685140, -14.35773016799012680 ) ) ;
#65650 = CARTESIAN_POINT ( 'NONE',  ( 87.63119364650854948, 45.29408460765224476, 6.394950601605615681 ) ) ;
#65651 = CARTESIAN_POINT ( 'NONE',  ( 194.2605386096435893, 292.8896166215183143, 15.20382020497128472 ) ) ;
#65652 = VERTEX_POINT ( 'NONE', #43710 ) ;
#65653 = PLANE ( 'NONE',  #94741 ) ;
#65654 = ORIENTED_EDGE ( 'NONE', *, *, #92042, .F. ) ;
#65655 = CARTESIAN_POINT ( 'NONE',  ( -8.406493707509316238, 25.24382671950690948, -10.00000000000000000 ) ) ;
#65656 = CARTESIAN_POINT ( 'NONE',  ( 204.8652996567902278, 269.2354455564837963, -2.974687384846896876 ) ) ;
#65657 = CARTESIAN_POINT ( 'NONE',  ( 163.9582657378243766, 246.6629487516456720, -7.496770747748987773 ) ) ;
#65658 = DIRECTION ( 'NONE',  ( 1.000000000000000000, 0.000000000000000000, 0.000000000000000000 ) ) ;
#65659 = CARTESIAN_POINT ( 'NONE',  ( 202.8499463704053198, 279.3005819042728604, 17.04674939340617001 ) ) ;
#65661 = CARTESIAN_POINT ( 'NONE',  ( 88.48118267945454818, 44.00993189541001271, 2.076335272536708576 ) ) ;
#65660 = DIRECTION ( 'NONE',  ( -0.000000000000000000, -0.000000000000000000, -1.000000000000000000 ) ) ;
#65662 = CARTESIAN_POINT ( 'NONE',  ( 166.1325645896313006, 247.4337816087006559, 6.210353822890861686 ) ) ;
#65663 = ORIENTED_EDGE ( 'NONE', *, *, #12845, .T. ) ;
#65664 = CIRCLE ( 'NONE', #4195, 70.00000000000001421 ) ;
#65665 = AXIS2_PLACEMENT_3D ( 'NONE', #51093, #29804, #83547 ) ;
#65666 = CARTESIAN_POINT ( 'NONE',  ( 74.23294069390520633, 67.58675612407668609, 12.40011470933238158 ) ) ;
#65667 = CARTESIAN_POINT ( 'NONE',  ( 190.2629546459234859, 273.4080951500121159, -16.67925241984795903 ) ) ;
#65668 = CARTESIAN_POINT ( 'NONE',  ( 71.88039266631933799, 65.91489085601192244, -12.06854722625687337 ) ) ;
#65669 = AXIS2_PLACEMENT_3D ( 'NONE', #7114, #37998, #77012 ) ;
#65670 = CARTESIAN_POINT ( 'NONE',  ( 192.1640094933931096, 297.8091675017319062, 12.36911124822534447 ) ) ;
#65671 = CARTESIAN_POINT ( 'NONE',  ( 80.87585157758311993, 42.95980323379527732, -9.554274543293205468 ) ) ;
#65672 = CARTESIAN_POINT ( 'NONE',  ( 41.64315915125185086, 206.3967562850347122, -4.648177544792955347E-16 ) ) ;
#65673 = CARTESIAN_POINT ( 'NONE',  ( 16.06189740016370848, 170.8923013555409796, 4.594050593750050204 ) ) ;
#65674 = CARTESIAN_POINT ( 'NONE',  ( 104.0981849360367875, 243.1589784336661921, -6.496448406907675876E-16 ) ) ;
#65675 = CARTESIAN_POINT ( 'NONE',  ( 202.8151641853381477, 279.3608264160075692, -16.28741359973609448 ) ) ;
#65676 = CARTESIAN_POINT ( 'NONE',  ( 87.96405694255219032, 44.24133552746449283, -4.384643187820149279 ) ) ;
#65677 = CARTESIAN_POINT ( 'NONE',  ( 180.9300408734833923, 255.0300470106541297, -2.486323749695340091 ) ) ;
#65678 = CARTESIAN_POINT ( 'NONE',  ( 77.55626133878482165, 49.73613333205595666, 14.95107568548285037 ) ) ;
#65679 = EDGE_CURVE ( 'NONE', #51044, #33408, #55915, .T. ) ;
#65680 = CARTESIAN_POINT ( 'NONE',  ( 77.25846549316018752, 51.17059816455404331, 15.45812498229560639 ) ) ;
#65681 = CARTESIAN_POINT ( 'NONE',  ( 164.0096516886412701, 284.3946043071177883, 5.908419196777021654 ) ) ;
#65682 = CARTESIAN_POINT ( 'NONE',  ( 148.2352135776142177, 273.8960739431854563, -9.245976304249309052 ) ) ;
#65683 = DIRECTION ( 'NONE',  ( -0.2500151307524235422, 0.9682419296822714072, 0.000000000000000000 ) ) ;
#65684 = CARTESIAN_POINT ( 'NONE',  ( 84.37450382530433046, 50.67865889666357759, 13.77848111769147366 ) ) ;
#65685 = CARTESIAN_POINT ( 'NONE',  ( -19.74615283476394367, 92.95798879106189361, 59.99999999999999289 ) ) ;
#65686 = CARTESIAN_POINT ( 'NONE',  ( 140.5888732624033821, 258.6427522451418781, -10.00000000000009592 ) ) ;
#65687 = EDGE_CURVE ( 'NONE', #88229, #39565, #97938, .T. ) ;
#65688 = CARTESIAN_POINT ( 'NONE',  ( 89.99855592466249732, 212.7677522451417929, -5.000000000000041744 ) ) ;
#65689 = LINE ( 'NONE', #35294, #98332 ) ;
#65690 = EDGE_CURVE ( 'NONE', #13530, #86376, #74079, .T. ) ;
#65691 = CARTESIAN_POINT ( 'NONE',  ( 78.44218234892278474, 228.3464784336661353, 1.353441290958777327E-15 ) ) ;
#65692 = CARTESIAN_POINT ( 'NONE',  ( 161.0974665087481981, 251.6179983666593216, -13.69252715295363210 ) ) ;
#65693 = CARTESIAN_POINT ( 'NONE',  ( 78.61816319214723592, 52.61787231995300829, -16.10833693956800161 ) ) ;
#65694 = CARTESIAN_POINT ( 'NONE',  ( -19.65312891409030271, 93.06504152958497400, 10.00000000000000888 ) ) ;
#65696 = CARTESIAN_POINT ( 'NONE',  ( 199.8196579795990715, 284.5491953587354601, 17.07111731403734822 ) ) ;
#65695 = CARTESIAN_POINT ( 'NONE',  ( 157.1837449796689725, 258.3967629017010381, 16.97243084443542216 ) ) ;
#65697 = CARTESIAN_POINT ( 'NONE',  ( 198.8157103782086210, 286.2880836124806478, -18.60729372713428020 ) ) ;
#65698 = CARTESIAN_POINT ( 'NONE',  ( 173.1711317957924052, 268.1345242171204859, -16.28840157703276859 ) ) ;
#65699 = CARTESIAN_POINT ( 'NONE',  ( 33.90351810284484202, 25.28920272979928896, -7.433330006724141015 ) ) ;
#65700 = CARTESIAN_POINT ( 'NONE',  ( 86.32721218574307898, 47.55264674982593931, -11.12316258729871699 ) ) ;
#65701 = CARTESIAN_POINT ( 'NONE',  ( 75.51649238510275097, 60.77114109127464303, 15.98312560776951230 ) ) ;
#65702 = VERTEX_POINT ( 'NONE', #85778 ) ;
#65703 = CARTESIAN_POINT ( 'NONE',  ( 16.11390655273756778, 24.70171378149918340, -9.188101187500004485 ) ) ;
#65704 = CARTESIAN_POINT ( 'NONE',  ( 5.294102074706517058, 26.55466486950697558, -1.111400068045478839E-16 ) ) ;
#65705 = DIRECTION ( 'NONE',  ( 0.5000000000000048850, -0.8660254037844358210, 0.000000000000000000 ) ) ;
#65706 = CARTESIAN_POINT ( 'NONE',  ( 48.43557798863805886, 76.81918075477977936, 177.5919119679930134 ) ) ;
#65707 = VECTOR ( 'NONE', #85244, 1000.000000000000000 ) ;
#65708 = CARTESIAN_POINT ( 'NONE',  ( 86.20802731503823679, 47.17721747253784770, 10.82151197958144273 ) ) ;
#65709 = CARTESIAN_POINT ( 'NONE',  ( 193.5969836369176562, 288.4623895989528251, 16.08576061698174797 ) ) ;
#65710 = CARTESIAN_POINT ( 'NONE',  ( 50.33662733789742560, 94.26254718190892845, 177.5919119679930134 ) ) ;
#65711 = CARTESIAN_POINT ( 'NONE',  ( 131.8023238567217277, 240.2365022471901739, -10.00000000000009059 ) ) ;
#65712 = CARTESIAN_POINT ( 'NONE',  ( 157.8811243250769110, 257.1888664433053009, -17.39256699147873064 ) ) ;
#65713 = CARTESIAN_POINT ( 'NONE',  ( 74.75954543159157595, 53.46422244337664864, 16.07001580372355320 ) ) ;
#65714 = VERTEX_POINT ( 'NONE', #62904 ) ;
#65715 = CARTESIAN_POINT ( 'NONE',  ( 169.5987612212706210, 248.4539404957666591, -1.946464333004839675 ) ) ;
#65716 = ORIENTED_EDGE ( 'NONE', *, *, #84540, .F. ) ;
#65717 = CARTESIAN_POINT ( 'NONE',  ( 163.4004183463084416, 247.6291687766210146, 10.19167732382099345 ) ) ;
#65718 = CARTESIAN_POINT ( 'NONE',  ( 173.2798715285074991, 281.8114527337138497, 15.08241540710736750 ) ) ;
#65719 = ORIENTED_EDGE ( 'NONE', *, *, #57949, .F. ) ;
#65720 = CARTESIAN_POINT ( 'NONE',  ( 49.60098510475376088, 81.22027839155747131, 10.00000000000000000 ) ) ;
#65721 = ORIENTED_EDGE ( 'NONE', *, *, #9051, .F. ) ;
#65722 = CARTESIAN_POINT ( 'NONE',  ( 71.95473880081605955, 71.54457537667215661, 5.606738443688809248 ) ) ;
#65723 = CARTESIAN_POINT ( 'NONE',  ( 205.8720179146364160, 274.0662004455563761, 12.32128734042425933 ) ) ;
#65724 = CARTESIAN_POINT ( 'NONE',  ( 142.3387059458346755, 262.1744531367911009, 4.594050593750047540 ) ) ;
#65725 = CARTESIAN_POINT ( 'NONE',  ( 87.91725590613566510, 44.21674671100767284, -4.392329086374231473 ) ) ;
#65726 = CARTESIAN_POINT ( 'NONE',  ( 202.0271362839079643, 275.0056074051718724, -14.19488698628315326 ) ) ;
#65727 = CARTESIAN_POINT ( 'NONE',  ( 46.41032958717836010, 27.76426979415094110, 3.090169943749476733 ) ) ;
#65728 = CARTESIAN_POINT ( 'NONE',  ( 30.33837380989695731, 32.91421378149920685, 9.188101187500008038 ) ) ;
#65729 = VECTOR ( 'NONE', #6701, 999.9999999999998863 ) ;
#65730 = CARTESIAN_POINT ( 'NONE',  ( 79.06023636259786258, 58.49762800437630972, -16.20933576862745440 ) ) ;
#65731 = EDGE_CURVE ( 'NONE', #4325, #90496, #70924, .T. ) ;
#65732 = CARTESIAN_POINT ( 'NONE',  ( 156.6812872898450735, 261.2670451491295012, 0.000000000000000000 ) ) ;
#65733 = FACE_OUTER_BOUND ( 'NONE', #1261, .T. ) ;
#65734 = AXIS2_PLACEMENT_3D ( 'NONE', #50565, #12084, #35368 ) ;
#65735 = VERTEX_POINT ( 'NONE', #118 ) ;
#65736 = ORIENTED_EDGE ( 'NONE', *, *, #44686, .F. ) ;
#65737 = CARTESIAN_POINT ( 'NONE',  ( 184.8890758847559823, 296.9636581320273763, 1.025268066086537644 ) ) ;
#65739 = CARTESIAN_POINT ( 'NONE',  ( 147.9791529310278122, 274.3395839928920168, -7.789432462804474433 ) ) ;
#65738 = CARTESIAN_POINT ( 'NONE',  ( 204.3371846825755824, 276.7246095846310823, 14.72513001683937262 ) ) ;
#65740 = CARTESIAN_POINT ( 'NONE',  ( 85.91498916281075537, 48.46192805135255099, 12.13455285288522667 ) ) ;
#65741 = CARTESIAN_POINT ( 'NONE',  ( 66.54075137518580618, 68.81555626029071959, -2.231460399992863497 ) ) ;
#65742 = CARTESIAN_POINT ( 'NONE',  ( 157.3834985187485529, 282.2511498796980050, -0.4876292292492137581 ) ) ;
#65743 = LINE ( 'NONE', #95210, #45166 ) ;
#65744 = EDGE_CURVE ( 'NONE', #46006, #1717, #25828, .T. ) ;
#65745 = CARTESIAN_POINT ( 'NONE',  ( 208.1381420012782542, 270.1411583912371270, -4.612438132219912390 ) ) ;
#65746 = EDGE_CURVE ( 'NONE', #14010, #32823, #49222, .T. ) ;
#65747 = CARTESIAN_POINT ( 'NONE',  ( -97.59541525468981149, 48.06504152958505216, -36.50000000000000000 ) ) ;
#65748 = CARTESIAN_POINT ( 'NONE',  ( 78.88256717313477395, 59.65579592159198086, 16.50129574805685806 ) ) ;
#65749 = CARTESIAN_POINT ( 'NONE',  ( 109.2678814824639204, 224.7048013555410080, 4.594050593750051981 ) ) ;
#65750 = VERTEX_POINT ( 'NONE', #96852 ) ;
#65751 = CARTESIAN_POINT ( 'NONE',  ( 73.82455155085514775, 55.55241100957154288, -16.58550341923981719 ) ) ;
#65752 = PLANE ( 'NONE',  #70653 ) ;
#65753 = CARTESIAN_POINT ( 'NONE',  ( 163.0140611511896793, 276.5848272863240709, -14.06802711415683760 ) ) ;
#65754 = ORIENTED_EDGE ( 'NONE', *, *, #8290, .T. ) ;
#65755 = ORIENTED_EDGE ( 'NONE', *, *, #70780, .F. ) ;
#65756 = CARTESIAN_POINT ( 'NONE',  ( 87.22262286821016630, 46.01322853962243897, -8.753954545221112937 ) ) ;
#65757 = CARTESIAN_POINT ( 'NONE',  ( 177.0163663914809433, 292.4487994013190928, -2.715256582491245130 ) ) ;
#65758 = CARTESIAN_POINT ( 'NONE',  ( 157.6335212189247557, 257.6177276032722716, 16.76495363836117036 ) ) ;
#65759 = CARTESIAN_POINT ( 'NONE',  ( 14.17036660571061368, 16.38052372038639604, 10.00000000000000533 ) ) ;
#65760 = CARTESIAN_POINT ( 'NONE',  ( 208.2018443082727970, 270.0308227589636090, 1.727811837614598556 ) ) ;
#65761 = CARTESIAN_POINT ( 'NONE',  ( 97.11602866590727956, 233.0024278399160664, 9.188101187500095079 ) ) ;
#65762 = EDGE_LOOP ( 'NONE', ( #35927, #18654, #40189, #29981 ) ) ;
#65763 = VERTEX_POINT ( 'NONE', #10720 ) ;
#65764 = CARTESIAN_POINT ( 'NONE',  ( -0.2492734796364602656, 27.10516647459198225, -10.00000000000000000 ) ) ;
#65765 = ORIENTED_EDGE ( 'NONE', *, *, #78809, .T. ) ;
#65766 = CARTESIAN_POINT ( 'NONE',  ( 194.2751985042537513, 266.1072248296521252, -7.746649050517742552 ) ) ;
#65767 = CARTESIAN_POINT ( 'NONE',  ( 29.68521398013932711, 18.10801979619930080, 3.090169943749476733 ) ) ;
#65768 = AXIS2_PLACEMENT_3D ( 'NONE', #16695, #63791, #86655 ) ;
#65769 = CARTESIAN_POINT ( 'NONE',  ( 165.5604721375479755, 285.4306498218772390, 0.8607609473838128133 ) ) ;
#65771 = CARTESIAN_POINT ( 'NONE',  ( 69.59872347107847190, 62.52290715608992144, -13.38904497502296920 ) ) ;
#65770 = CARTESIAN_POINT ( 'NONE',  ( 136.7913381204293728, 237.5327760586659736, 1.948934522072303157E-15 ) ) ;
#65772 = CARTESIAN_POINT ( 'NONE',  ( 72.26191451101281871, 71.91445694603925176, -5.118044210176695863 ) ) ;
#65773 = FACE_OUTER_BOUND ( 'NONE', #36214, .T. ) ;
#65774 = ORIENTED_EDGE ( 'NONE', *, *, #15929, .F. ) ;
#65776 = CARTESIAN_POINT ( 'NONE',  ( 205.0608432903593155, 275.4711961086152883, 13.55071766891341412 ) ) ;
#65775 = VECTOR ( 'NONE', #16445, 1000.000000000000114 ) ;
#65777 = CARTESIAN_POINT ( 'NONE',  ( 81.60462840567272735, 48.29055636627209225, 13.20316565662312236 ) ) ;
#65778 = CARTESIAN_POINT ( 'NONE',  ( 82.17911912404201757, 40.65326309479461742, -3.506590647633029523 ) ) ;
#65779 = LINE ( 'NONE', #50580, #15727 ) ;
#65780 = CARTESIAN_POINT ( 'NONE',  ( 174.0424481033923314, 287.4814580433055653, 10.99910921803667208 ) ) ;
#65781 = AXIS2_PLACEMENT_3D ( 'NONE', #28759, #74393, #30251 ) ;
#65782 = DIRECTION ( 'NONE',  ( 0.000000000000000000, -1.000000000000000000, 1.060575238724906175E-16 ) ) ;
#65783 = CARTESIAN_POINT ( 'NONE',  ( 197.1048653879311132, 280.7190563205994067, -16.61298024664429107 ) ) ;
#65784 = CARTESIAN_POINT ( 'NONE',  ( 129.2042476453684117, 238.7365022471901739, -10.00000000000009237 ) ) ;
#65785 = CARTESIAN_POINT ( 'NONE',  ( 80.78458207904813548, 54.24769972901211190, 15.79515950411193259 ) ) ;
#65786 = CARTESIAN_POINT ( 'NONE',  ( 67.13575020204197585, 69.32447942518001582, -0.8057866954429201423 ) ) ;
#65787 = CARTESIAN_POINT ( 'NONE',  ( 206.7923762329701276, 272.4720930770340033, -9.496103119940368487 ) ) ;
#65788 = CARTESIAN_POINT ( 'NONE',  ( 78.31539865234907438, 61.49392785109991166, 15.81390201164141196 ) ) ;
#65789 = CARTESIAN_POINT ( 'NONE',  ( 178.1281481821618797, 292.9991590599575488, -6.064681374715556572 ) ) ;
#65790 = CARTESIAN_POINT ( 'NONE',  ( 163.2015365837845309, 247.9736420940113248, -10.76959291176343747 ) ) ;
#65791 = EDGE_CURVE ( 'NONE', #47928, #39924, #32970, .T. ) ;
#65792 = CIRCLE ( 'NONE', #94997, 4.999999999999993783 ) ;
#65793 = CARTESIAN_POINT ( 'NONE',  ( 74.17947873915457535, 55.31082063550417161, 16.12337822475624094 ) ) ;
#65794 = CARTESIAN_POINT ( 'NONE',  ( 78.38478726132005647, 48.59772224786558326, 14.85394671703156178 ) ) ;
#65795 = ADVANCED_FACE ( 'NONE', ( #33338 ), #40912, .T. ) ;
#65796 = CARTESIAN_POINT ( 'NONE',  ( 34.30385554556135475, 35.50829794293883168, -10.00000000000000355 ) ) ;
#65797 = DIRECTION ( 'NONE',  ( -0.7061384650677096086, -0.7080737730998225565, 0.000000000000000000 ) ) ;
#65798 = CARTESIAN_POINT ( 'NONE',  ( 71.60534465744318311, 58.98582914060868632, -15.35957662280589275 ) ) ;
#65799 = VECTOR ( 'NONE', #59149, 1000.000000000000000 ) ;
#65800 = CARTESIAN_POINT ( 'NONE',  ( 81.50613923611670941, 43.19572371951541356, -8.552294727196889212 ) ) ;
#65801 = CARTESIAN_POINT ( 'NONE',  ( 14.51920287573142510, 173.0643266524160140, 9.188101187500095079 ) ) ;
#65802 = CARTESIAN_POINT ( 'NONE',  ( -22.42236680055709641, 157.8615022471902591, 0.000000000000000000 ) ) ;
#65803 = EDGE_LOOP ( 'NONE', ( #75887, #75098, #18078, #87268 ) ) ;
#65804 = EDGE_CURVE ( 'NONE', #83079, #25248, #100003, .T. ) ;
#65805 = CARTESIAN_POINT ( 'NONE',  ( 87.01945182987638816, 46.04471723482853918, 8.958281803387862396 ) ) ;
#65806 = DIRECTION ( 'NONE',  ( 0.4999999999999992784, -0.8660254037844390407, 0.000000000000000000 ) ) ;
#65807 = CARTESIAN_POINT ( 'NONE',  ( 82.03128457439912324, 41.77525573450511587, 5.434104432741746926 ) ) ;
#65808 = CARTESIAN_POINT ( 'NONE',  ( 44.74898890052324418, 187.4548013555409796, -4.594050593750042211 ) ) ;
#65809 = CARTESIAN_POINT ( 'NONE',  ( 161.8811854682448939, 250.2605573099562264, 13.51112293479948789 ) ) ;
#65810 = CARTESIAN_POINT ( 'NONE',  ( 190.7908437487391780, 300.1875603386860689, -4.317984972589949955 ) ) ;
#65811 = CARTESIAN_POINT ( 'NONE',  ( 33.88626221353634804, 43.65659080271453973, -1.878358725466461243E-16 ) ) ;
#65812 = CARTESIAN_POINT ( 'NONE',  ( 202.9528762288709061, 270.0503579255801014, -6.478656441495562746 ) ) ;
#65813 = CARTESIAN_POINT ( 'NONE',  ( 191.6823192895500370, 298.6434794082964572, -8.424208857102787107 ) ) ;
#65814 = CARTESIAN_POINT ( 'NONE',  ( 44.95821123098110661, 116.5722627105190270, -10.00000000000000000 ) ) ;
#65815 = CARTESIAN_POINT ( 'NONE',  ( 71.96486598315394190, 67.72978614143600851, -10.50385197199905285 ) ) ;
#65816 = CARTESIAN_POINT ( 'NONE',  ( 84.80240350195578003, 229.7677522451419350, -5.000000000000047962 ) ) ;
#65817 = DIRECTION ( 'NONE',  ( -0.2805612043866616556, -0.9598361373656993933, 0.000000000000000000 ) ) ;
#65818 = ADVANCED_FACE ( 'NONE', ( #78971 ), #62216, .F. ) ;
#65819 = CARTESIAN_POINT ( 'NONE',  ( 192.5112645657038684, 295.4124808762264252, -13.34516070875820759 ) ) ;
#65820 = CARTESIAN_POINT ( 'NONE',  ( 77.96441125478908418, 222.4865022471903160, 10.00000000000009237 ) ) ;
#65821 = DIRECTION ( 'NONE',  ( 0.000000000000000000, 0.000000000000000000, 1.000000000000000000 ) ) ;
#65822 = CARTESIAN_POINT ( 'NONE',  ( 31.26830227169403997, 36.79103043416551344, 8.090169943749478065 ) ) ;
#65823 = ORIENTED_EDGE ( 'NONE', *, *, #77420, .T. ) ;
#65824 = CARTESIAN_POINT ( 'NONE',  ( 43.80151329331025067, 196.0958772461660544, -9.188101187500095079 ) ) ;
#65825 = VERTEX_POINT ( 'NONE', #48027 ) ;
#65826 = CARTESIAN_POINT ( 'NONE',  ( 162.5761427237234784, 263.2594962941460608, 17.31260787709388538 ) ) ;
#65827 = CARTESIAN_POINT ( 'NONE',  ( 198.7136873185829984, 286.4647927352960437, -18.57144721070432070 ) ) ;
#65828 = CARTESIAN_POINT ( 'NONE',  ( 67.54350597765656516, 66.80466261606197520, -8.460816904384278914 ) ) ;
#65829 = ORIENTED_EDGE ( 'NONE', *, *, #27330, .T. ) ;
#65830 = CARTESIAN_POINT ( 'NONE',  ( 171.3312619405691066, 286.5464919449711374, 7.566358419436266303 ) ) ;
#65831 = CARTESIAN_POINT ( 'NONE',  ( 164.2723164851102808, 246.1189969011916503, -1.993789335506892302 ) ) ;
#65832 = CARTESIAN_POINT ( 'NONE',  ( -19.65312891409030271, 93.06504152958497400, 10.00000000000000888 ) ) ;
#65833 = CARTESIAN_POINT ( 'NONE',  ( 27.91350267930052809, 31.51421378149921182, -9.188101187500004485 ) ) ;
#65834 = CARTESIAN_POINT ( 'NONE',  ( 189.6437701857260549, 264.6299060724186347, 10.65328101858895771 ) ) ;
#65835 = CARTESIAN_POINT ( 'NONE',  ( 86.53753835918318771, 47.29678250252424476, -10.20988859552574013 ) ) ;
#65836 = VECTOR ( 'NONE', #54957, 1000.000000000000114 ) ;
#65837 = CARTESIAN_POINT ( 'NONE',  ( 171.2977123844769949, 255.8120995149402859, 11.88195947517418283 ) ) ;
#65838 = ORIENTED_EDGE ( 'NONE', *, *, #89036, .T. ) ;
#65839 = VECTOR ( 'NONE', #94810, 1000.000000000000114 ) ;
#65840 = CARTESIAN_POINT ( 'NONE',  ( 16.86928618479235809, 18.24335787977762280, -9.188101187500008038 ) ) ;
#65841 = CARTESIAN_POINT ( 'NONE',  ( 76.46509270602138031, 63.14577049208008930, 15.06850016415780935 ) ) ;
#65842 = CARTESIAN_POINT ( 'NONE',  ( 174.7964402711189393, 255.1616715225093515, 8.226461705621156639 ) ) ;
#65843 = LINE ( 'NONE', #21749, #21341 ) ;
#65844 = EDGE_CURVE ( 'NONE', #18147, #34226, #11299, .T. ) ;
#65845 = ORIENTED_EDGE ( 'NONE', *, *, #68247, .F. ) ;
#65846 = CARTESIAN_POINT ( 'NONE',  ( 182.6345022024692355, 283.7833407587357897, 15.47623830145432855 ) ) ;
#65847 = LINE ( 'NONE', #12170, #79190 ) ;
#65848 = CARTESIAN_POINT ( 'NONE',  ( 169.1311965936330353, 247.8770103324328034, 7.134965090537657859E-13 ) ) ;
#65849 = ORIENTED_EDGE ( 'NONE', *, *, #23090, .T. ) ;
#65850 = VERTEX_POINT ( 'NONE', #11057 ) ;
#65851 = EDGE_CURVE ( 'NONE', #86376, #57995, #98316, .T. ) ;
#65852 = VECTOR ( 'NONE', #28642, 1000.000000000000000 ) ;
#65853 =( BOUNDED_CURVE ( )  B_SPLINE_CURVE ( 2, ( #9271, #41650, #87351, #71085, #24955, #93404, #32047, #17358, #93910 ),
 .UNSPECIFIED., .F., .T. ) 
 B_SPLINE_CURVE_WITH_KNOTS ( ( 3, 2, 2, 2, 3 ),
 ( 0.3024193548387096864, 0.3037634408602150615, 0.3064516129032258118, 0.3091397849462365621, 0.3104838709677419373 ),
 .UNSPECIFIED. ) 
 CURVE ( )  GEOMETRIC_REPRESENTATION_ITEM ( )  RATIONAL_B_SPLINE_CURVE ( ( 0.9330127018922194093, 0.9330127018922194093, 1.000000000000000000, 0.8660254037844387076, 1.000000000000000000, 0.8660254037844387076, 1.000000000000000000, 0.9330127018922194093, 0.9330127018922194093 ) ) 
 REPRESENTATION_ITEM ( '' )  );
#65855 = DIRECTION ( 'NONE',  ( -0.000000000000000000, 0.000000000000000000, 1.000000000000000000 ) ) ;
#65854 = CARTESIAN_POINT ( 'NONE',  ( 161.5083988044524119, 250.9062427520286178, -14.53522982831775856 ) ) ;
#65856 = CARTESIAN_POINT ( 'NONE',  ( 149.0598351764325002, 272.4677874370131576, -11.59078276432863674 ) ) ;
#65857 = EDGE_LOOP ( 'NONE', ( #75512, #46727, #3148, #27092 ) ) ;
#65858 = CARTESIAN_POINT ( 'NONE',  ( 66.25519791831798955, 69.22521726602100500, -2.104850759282526962 ) ) ;
#65859 = CARTESIAN_POINT ( 'NONE',  ( 159.3169041484411537, 254.7020228407560580, 16.67170756419672628 ) ) ;
#65860 = CARTESIAN_POINT ( 'NONE',  ( 180.9962514683335257, 255.6518059654043782, 5.281628127585873855 ) ) ;
#65861 = FACE_OUTER_BOUND ( 'NONE', #37211, .T. ) ;
#65862 = DIRECTION ( 'NONE',  ( 1.000000000000000000, 0.000000000000000000, 0.000000000000000000 ) ) ;
#65863 = CARTESIAN_POINT ( 'NONE',  ( 114.2743305262689404, 236.7833772461660544, -9.188101187500095079 ) ) ;
#65864 = ADVANCED_FACE ( 'NONE', ( #3459 ), #56634, .T. ) ;
#65865 = CARTESIAN_POINT ( 'NONE',  ( 190.3167824967908643, 299.0086585129598689, -8.112609889089975823 ) ) ;
#65866 = CARTESIAN_POINT ( 'NONE',  ( 149.2923684163597784, 272.0650280510108701, -12.99082738998495756 ) ) ;
#65867 = CARTESIAN_POINT ( 'NONE',  ( 35.89232211637455094, 179.9824982072973683, 3.021315404115420679E-15 ) ) ;
#65868 = ORIENTED_EDGE ( 'NONE', *, *, #97604, .T. ) ;
#65869 = AXIS2_PLACEMENT_3D ( 'NONE', #34035, #10726, #41094 ) ;
#65870 = CARTESIAN_POINT ( 'NONE',  ( 201.3965252030675686, 280.5319479810296457, 16.51675258086747533 ) ) ;
#65871 = VERTEX_POINT ( 'NONE', #27244 ) ;
#65872 = EDGE_CURVE ( 'NONE', #72912, #8322, #81473, .T. ) ;
#65873 = CARTESIAN_POINT ( 'NONE',  ( 31.91767387367526609, 30.37878583063843152, 9.188101187500006262 ) ) ;
#65874 = CARTESIAN_POINT ( 'NONE',  ( 159.9307118030769175, 253.6388767968520881, 16.60600887889890487 ) ) ;
#65875 = CARTESIAN_POINT ( 'NONE',  ( 75.27358033784481961, 66.49579001460178063, -13.13245767378105811 ) ) ;
#65876 = EDGE_CURVE ( 'NONE', #83731, #1098, #35327, .T. ) ;
#65877 = CARTESIAN_POINT ( 'NONE',  ( 69.15955932604958889, 219.9244531367911293, -4.594050593750046652 ) ) ;
#65878 = EDGE_LOOP ( 'NONE', ( #38216, #3563, #20021, #94975 ) ) ;
#65879 = CARTESIAN_POINT ( 'NONE',  ( -30.05470439949217365, 95.09793926796578489, 12.69393916137930667 ) ) ;
#65880 = CARTESIAN_POINT ( 'NONE',  ( 190.9501423151522772, 299.9116471280854626, 8.746938802470586083 ) ) ;
#65881 = LINE ( 'NONE', #90234, #69324 ) ;
#65882 = CARTESIAN_POINT ( 'NONE',  ( 172.2733305175966620, 277.0538235811624759, 16.56964073552936867 ) ) ;
#65883 = ORIENTED_EDGE ( 'NONE', *, *, #52238, .F. ) ;
#65884 = CARTESIAN_POINT ( 'NONE',  ( 179.5196496019146650, 266.1175816663657656, 16.29367087753972498 ) ) ;
#65885 = CARTESIAN_POINT ( 'NONE',  ( 86.51620552470654957, 43.45092470964799247, -2.691706072484096879 ) ) ;
#65886 = CARTESIAN_POINT ( 'NONE',  ( 203.1705638993064156, 278.7452560544191442, -15.08126533799095093 ) ) ;
#65887 = ORIENTED_EDGE ( 'NONE', *, *, #85646, .F. ) ;
#65888 = CARTESIAN_POINT ( 'NONE',  ( 194.7178830804197673, 293.3857286928936219, 15.96025387054093869 ) ) ;
#65889 = DIRECTION ( 'NONE',  ( 0.7884491381006394350, -0.6150999566154746745, 0.000000000000000000 ) ) ;
#65890 = CARTESIAN_POINT ( 'NONE',  ( 163.8562647933944731, 260.4330591941297826, -16.17453866336511581 ) ) ;
#65891 = DIRECTION ( 'NONE',  ( -0.000000000000000000, -0.000000000000000000, -1.000000000000000000 ) ) ;
#65892 = CARTESIAN_POINT ( 'NONE',  ( 11.23059542939759581, 30.24628978557580083, 177.5919119679930134 ) ) ;
#65893 = CARTESIAN_POINT ( 'NONE',  ( 206.4943150373521803, 272.9883502116088039, 11.34100825923693101 ) ) ;
#65894 = CARTESIAN_POINT ( 'NONE',  ( 206.3106310032756596, 273.3065002911688453, 10.17860425536756175 ) ) ;
#65895 = CARTESIAN_POINT ( 'NONE',  ( 134.1658515176688411, 238.2677522451417929, -5.000000000000041744 ) ) ;
#65896 = CARTESIAN_POINT ( 'NONE',  ( 167.6280379227422941, 256.4154598753431742, 13.62701025628873097 ) ) ;
#65897 = ORIENTED_EDGE ( 'NONE', *, *, #53495, .T. ) ;
#65898 = CARTESIAN_POINT ( 'NONE',  ( 208.3152833949211526, 269.8343404973242059, 2.763633873278860342 ) ) ;
#65899 = CARTESIAN_POINT ( 'NONE',  ( 128.8345561752773278, 239.0643266524160140, 9.188101187500095079 ) ) ;
#65900 = ORIENTED_EDGE ( 'NONE', *, *, #64625, .F. ) ;
#65901 = CARTESIAN_POINT ( 'NONE',  ( 83.59145317797239727, 44.17686507203912782, -8.297778310668469715 ) ) ;
#65902 = CARTESIAN_POINT ( 'NONE',  ( 83.25069437720389942, 41.52116721019276468, 1.986236189183263390 ) ) ;
#65903 = CARTESIAN_POINT ( 'NONE',  ( 168.6768854746088664, 281.1804913396564984, -13.82603935691987296 ) ) ;
#65904 = CARTESIAN_POINT ( 'NONE',  ( 164.3330377059402849, 246.0138246616164110, 7.208046019122525294 ) ) ;
#65905 = CARTESIAN_POINT ( 'NONE',  ( 75.16962353025014920, 63.22591803360379004, 14.72285336180162396 ) ) ;
#65906 = DIRECTION ( 'NONE',  ( -1.000000000000000000, 0.000000000000000000, 0.000000000000000000 ) ) ;
#65907 = VERTEX_POINT ( 'NONE', #4950 ) ;
#65908 = CARTESIAN_POINT ( 'NONE',  ( 77.14591628819390223, 58.19862468565533931, 16.13876800688947810 ) ) ;
#65909 = B_SPLINE_CURVE_WITH_KNOTS ( 'NONE', 3,
 ( #21448, #21937, #75167, #7228, #69026, #60919, #36135, #52829, #45233, #99457, #76642, #67538, #30033, #22926, #98467, #22438, #53331, #76169, #99956, #53813, #38112, #75655, #29061, #97963, #52334, #20975, #61426, #84777, #28538, #6240, #59420, #83783, #90400, #84286, #14830, #37134, #59928, #29545, #68040, #14345, #90898, #51856, #60418, #37623, #68534, #82797, #13363, #16829 ),
 .UNSPECIFIED., .F., .F.,
 ( 4, 2, 2, 2, 2, 2, 2, 2, 2, 2, 2, 2, 2, 2, 2, 2, 2, 2, 2, 2, 2, 2, 2, 4 ),
 ( 0.0001718391672230527530, 0.001192457371175957440, 0.001702766473152372839, 0.001830343748646495608, 0.001957921024140618811, 0.002085498299634741797, 0.002213075575128864783, 0.002468230126117043101, 0.002723384677105221852, 0.003233693779081678234, 0.004254311983034685975, 0.005274930186987694149, 0.005785239288964233798, 0.006040393839952425993, 0.006295548390940617321, 0.006359337028687664720, 0.006423125666434712118, 0.006550702941928721046, 0.006805857492916878547, 0.007316166594893006199, 0.007571321145881069158, 0.007826475696869132984, 0.008081630247857197677, 0.008336784798845260636 ),
 .UNSPECIFIED. ) ;
#65910 = DIRECTION ( 'NONE',  ( -0.8660254037844387076, -0.4999999999999998890, -0.000000000000000000 ) ) ;
#65911 = CARTESIAN_POINT ( 'NONE',  ( 164.9133935349224203, 245.0086188793504505, -2.355115420316610919 ) ) ;
#65912 = CARTESIAN_POINT ( 'NONE',  ( -38.63165894407827494, 162.9368197944959036, 2.598076211353396392 ) ) ;
#65913 = CARTESIAN_POINT ( 'NONE',  ( 195.5576243985897236, 263.4396298511827013, 0.8694183353164576245 ) ) ;
#65914 = CARTESIAN_POINT ( 'NONE',  ( 190.3791419447713906, 300.9006487807255326, -5.688668718458480988 ) ) ;
#65915 = CARTESIAN_POINT ( 'NONE',  ( 69.48133079272756163, 70.40394783201412565, 3.079148351843276288 ) ) ;
#65916 = CIRCLE ( 'NONE', #57815, 49.99999999999999289 ) ;
#65917 = VECTOR ( 'NONE', #18158, 1000.000000000000114 ) ;
#65918 = CARTESIAN_POINT ( 'NONE',  ( 170.7113395477583424, 250.4904927623917104, 3.433421072208380220 ) ) ;
#65919 = B_SPLINE_SURFACE_WITH_KNOTS ( 'NONE', 3, 1, ( 
 ( #81574, #36417 ),
 ( #4531, #81089 ),
 ( #19754, #50622 ),
 ( #20750, #65337 ),
 ( #67324, #73945 ),
 ( #29827, #91660 ),
 ( #61216, #75960 ),
 ( #21728, #83068 ),
 ( #22733, #53611 ),
 ( #7516, #29338 ),
 ( #52612, #100245 ),
 ( #75443, #23212 ),
 ( #54102, #15607 ),
 ( #77443, #38911 ),
 ( #69817, #9025 ),
 ( #77940, #94165 ),
 ( #63223, #18134 ),
 ( #16620, #63726 ),
 ( #70316, #87096 ),
 ( #64224, #32322 ),
 ( #86584, #17635 ),
 ( #17119, #78958 ),
 ( #49035, #72356 ),
 ( #93156, #85584 ),
 ( #9547, #74355 ),
 ( #49521, #73830 ),
 ( #27731, #20137 ),
 ( #51517, #72858 ),
 ( #34809, #26235 ),
 ( #43907, #96664 ),
 ( #43408, #33854 ) ),
 .UNSPECIFIED., .F., .F., .F.,
 ( 4, 3, 3, 3, 3, 3, 3, 3, 3, 3, 4 ),
 ( 2, 2 ),
 ( 0.000000000000000000, 0.1333490885032282969, 0.3007194338854215498, 0.4699862290245004903, 0.5844252810809279497, 0.6686540514502673505, 0.7354980260655414881, 0.8028463152565613603, 0.8633854507757170449, 0.9437142632667081532, 1.000000000000000000 ),
 ( 0.000000000000000000, 1.000000000000000000 ),
 .UNSPECIFIED. ) ;
#65920 = CARTESIAN_POINT ( 'NONE',  ( 24.24684063885245422, 16.12755873383626337, -6.180339887498949025 ) ) ;
#65921 = CARTESIAN_POINT ( 'NONE',  ( 190.8153366230912411, 300.1451374358846920, 3.771947273125533684 ) ) ;
#65922 = CARTESIAN_POINT ( 'NONE',  ( 188.4688990864094080, 295.3997683978527675, -11.43812978727723717 ) ) ;
#65923 = CARTESIAN_POINT ( 'NONE',  ( 169.2909702781398664, 285.2592091808388659, -8.894609513033637782 ) ) ;
#65924 = B_SPLINE_CURVE_WITH_KNOTS ( 'NONE', 3,
 ( #55903, #86897, #1237, #94977, #31117, #32120, #63030, #69626, #79286, #24527, #55406, #9859, #40718, #71663, #92958, #33132, #64034, #25541, #56428, #46307, #77232, #7839, #38720, #56920, #80281, #48850, #50325, #19469, #65038, #19944, #64540, #80792, #10348, #49833, #43208, #2761, #10847, #81277, #41724, #87909, #57926, #42708, #88906, #11367, #33651, #18956, #95985, #26049, #26548, #3750 ),
 .UNSPECIFIED., .F., .F.,
 ( 4, 2, 2, 2, 2, 2, 2, 2, 2, 2, 2, 2, 2, 2, 2, 2, 2, 2, 2, 2, 2, 2, 2, 2, 4 ),
 ( 0.0006375827441053666606, 0.001063963319884116175, 0.001277153607773526441, 0.001383748751718216069, 0.001490343895662905697, 0.001703534183552284954, 0.001916724471441664211, 0.002343105047220586656, 0.003195866198778431980, 0.004048627350336277304, 0.004901388501894122195, 0.005327769077673054181, 0.005540959365562520174, 0.005647554509507253170, 0.005700852081479585408, 0.005754149653451917645, 0.005807447225424249883, 0.005860744797396582120, 0.005967339941341270881, 0.006180530229230528708, 0.006606910805009000125, 0.006820101092898229328, 0.007033291380787459399, 0.007246481668676688602, 0.007459671956565918673 ),
 .UNSPECIFIED. ) ;
#65925 = CARTESIAN_POINT ( 'NONE',  ( 155.3716771045260714, 261.5353565282119348, -18.54934131471355840 ) ) ;
#65926 = CARTESIAN_POINT ( 'NONE',  ( 193.9750484533059591, 288.7567388352306352, 16.08761660616773170 ) ) ;
#65927 = VECTOR ( 'NONE', #8498, 1000.000000000000114 ) ;
#65928 = CARTESIAN_POINT ( 'NONE',  ( 141.5270674498366077, 242.5177522451417929, 5.000000000000051514 ) ) ;
#65929 = CARTESIAN_POINT ( 'NONE',  ( 87.86298961015023679, 44.89260222163543546, 6.207647304897661478 ) ) ;
#65930 = EDGE_LOOP ( 'NONE', ( #77366, #8132, #83591, #61236 ) ) ;
#65931 = ADVANCED_FACE ( 'NONE', ( #11557 ), #12047, .T. ) ;
#65932 = CARTESIAN_POINT ( 'NONE',  ( 195.9920715006079490, 291.1787696107118677, 15.99608784761372071 ) ) ;
#65933 = B_SPLINE_CURVE_WITH_KNOTS ( 'NONE', 3,
 ( #68039, #29544, #98960, #14829, #43734, #84285, #66548, #97477, #83782, #67036, #28043, #52333, #58919, #91372 ),
 .UNSPECIFIED., .F., .F.,
 ( 4, 2, 2, 2, 2, 2, 4 ),
 ( 0.001016148850039182410, 0.001267816211751153889, 0.001519483573463125368, 0.001771150935175097065, 0.002022818296887068327, 0.002526153020311010418, 0.003029487743734952075 ),
 .UNSPECIFIED. ) ;
#65934 = CARTESIAN_POINT ( 'NONE',  ( 148.3519871123208986, 273.6938162480936398, 8.180046468253793890 ) ) ;
#65935 = CARTESIAN_POINT ( 'NONE',  ( -7.131779314644562717, 172.8149278399161233, 9.188101187500093303 ) ) ;
#65936 = B_SPLINE_CURVE_WITH_KNOTS ( 'NONE', 3,
 ( #93179, #23732, #46024, #54627 ),
 .UNSPECIFIED., .F., .F.,
 ( 4, 4 ),
 ( 0.04193484224020654905, 0.04887066958154938356 ),
 .UNSPECIFIED. ) ;
#65937 = CARTESIAN_POINT ( 'NONE',  ( 36.87296296726972855, 204.3464784336661637, 1.353441290958777327E-15 ) ) ;
#65938 = CARTESIAN_POINT ( 'NONE',  ( 179.0286630115520552, 258.6160276279643995, -11.58942154470568120 ) ) ;
#65939 = CARTESIAN_POINT ( 'NONE',  ( 24.06687416953986514, 14.86426979415089633, -3.090169943749474069 ) ) ;
#65940 = DIRECTION ( 'NONE',  ( 0.4999999999999998890, -0.8660254037844385966, 0.000000000000000000 ) ) ;
#65941 = AXIS2_PLACEMENT_3D ( 'NONE', #4084, #97315, #5091 ) ;
#65942 = CARTESIAN_POINT ( 'NONE',  ( 157.8696211474012330, 257.2087905314882619, -17.27527248276125604 ) ) ;
#65943 = CARTESIAN_POINT ( 'NONE',  ( 72.01443008256866563, 72.40752555085421704, -2.913864408233449943 ) ) ;
#65944 = FACE_OUTER_BOUND ( 'NONE', #46027, .T. ) ;
#65945 = CARTESIAN_POINT ( 'NONE',  ( 149.7049461522049398, 276.2981810546235693, 3.707541583551217546 ) ) ;
#65946 = CARTESIAN_POINT ( 'NONE',  ( 77.46154149802761424, 203.9824982072973967, 3.021315404115420679E-15 ) ) ;
#65947 = CARTESIAN_POINT ( 'NONE',  ( 77.32817876982272765, 63.13942984521013813, 15.61058464551962111 ) ) ;
#65948 = EDGE_CURVE ( 'NONE', #38684, #80425, #45092, .T. ) ;
#65949 = CARTESIAN_POINT ( 'NONE',  ( 157.5487431480040925, 257.7645675294749594, -18.29554785922338311 ) ) ;
#65950 = CARTESIAN_POINT ( 'NONE',  ( 198.0355408163131585, 287.6393769322024241, 18.20720360189982756 ) ) ;
#65951 = EDGE_CURVE ( 'NONE', #74392, #95597, #3936, .T. ) ;
#65952 = CARTESIAN_POINT ( 'NONE',  ( 179.0941012263468224, 294.2742093295549921, 1.060795132963676446 ) ) ;
#65953 = CARTESIAN_POINT ( 'NONE',  ( 38.12724268070488876, 199.4865022471903160, -10.00000000000009415 ) ) ;
#65954 = CARTESIAN_POINT ( 'NONE',  ( 181.7815335863513155, 291.6605149460361304, 9.238327825430930673 ) ) ;
#65955 = MECHANICAL_DESIGN_GEOMETRIC_PRESENTATION_REPRESENTATION (  '', ( #44901 ), #23932 ) ;
#65956 = DIRECTION ( 'NONE',  ( -0.9778746070300391446, 0.2091919045418505763, 0.000000000000000000 ) ) ;
#65957 = CARTESIAN_POINT ( 'NONE',  ( 6.129408228687162286, 174.3458772461660828, 9.188101187500095079 ) ) ;
#65958 = CARTESIAN_POINT ( 'NONE',  ( 164.8661019620574564, 285.8049561880657734, 4.405979315412141162 ) ) ;
#65959 = CARTESIAN_POINT ( 'NONE',  ( 80.49432606691982528, 57.82183276640385117, -16.24662948867364420 ) ) ;
#65960 = CARTESIAN_POINT ( 'NONE',  ( 192.8010417052266234, 296.7057953447782097, 12.10593424093686643 ) ) ;
#65961 = CARTESIAN_POINT ( 'NONE',  ( 31.53879454291322659, 39.18502408145594984, 5.678558825948277544 ) ) ;
#65962 = CARTESIAN_POINT ( 'NONE',  ( 22.25607796093117230, 24.80066082961421969, 10.00000000000000533 ) ) ;
#65963 = CARTESIAN_POINT ( 'NONE',  ( 207.5686001603237116, 271.1276337968068333, 7.659944433763431704 ) ) ;
#65964 = CARTESIAN_POINT ( 'NONE',  ( 154.8596847415876994, 262.4221533139083817, 17.65401077761399762 ) ) ;
#65965 = CARTESIAN_POINT ( 'NONE',  ( 149.1004267900891307, 272.3974806997987343, -12.86882154300063341 ) ) ;
#65966 = CARTESIAN_POINT ( 'NONE',  ( 177.9552638626009298, 260.7378092407702184, -13.94576028113082877 ) ) ;
#65967 = PRODUCT_CONTEXT ( 'NONE', #29179, 'mechanical' ) ;
#65968 = CARTESIAN_POINT ( 'NONE',  ( 6.527493107231251201, 21.95586893147753216, 7.433330006724141015 ) ) ;
#65969 = CARTESIAN_POINT ( 'NONE',  ( 165.5860183037962088, 285.4175239968740243, 0.2436608606880265870 ) ) ;
#65970 = CARTESIAN_POINT ( 'NONE',  ( 22.90017757337614768, 16.14754757982090183, -5.678558825948275768 ) ) ;
#65971 = CARTESIAN_POINT ( 'NONE',  ( 185.5826357821268289, 271.8226265777869912, -17.01680751177637063 ) ) ;
#65972 = CARTESIAN_POINT ( 'NONE',  ( 152.6547697591180111, 278.7515079535921814, -4.825746761778547445 ) ) ;
#65973 = EDGE_LOOP ( 'NONE', ( #24272, #70747, #66252, #52045 ) ) ;
#65974 = CYLINDRICAL_SURFACE ( 'NONE', #19520, 4.999999999999993783 ) ;
#65975 = CARTESIAN_POINT ( 'NONE',  ( 74.98386055540046868, 53.36045814093387207, -16.04777311236104609 ) ) ;
#65976 = CARTESIAN_POINT ( 'NONE',  ( 159.7692415128758228, 253.9185515433934768, -16.85856106119654285 ) ) ;
#65977 = DIRECTION ( 'NONE',  ( -1.000000000000000000, -1.110223024625156343E-15, 0.000000000000000000 ) ) ;
#65978 = ORIENTED_EDGE ( 'NONE', *, *, #66888, .F. ) ;
#65979 = CARTESIAN_POINT ( 'NONE',  ( 152.3689561497722025, 267.5166801192429489, 15.45798366088414433 ) ) ;
#65980 = CARTESIAN_POINT ( 'NONE',  ( 206.9026071836525205, 272.2811674698855313, 7.240992997279449561 ) ) ;
#65981 = CARTESIAN_POINT ( 'NONE',  ( 66.76556300634629793, 68.39317378885236565, 4.474931876891666604 ) ) ;
#65982 = CARTESIAN_POINT ( 'NONE',  ( 87.16381268512610347, 45.36703396835236646, 7.086030772169831238 ) ) ;
#65983 = ORIENTED_EDGE ( 'NONE', *, *, #87317, .T. ) ;
#65984 = VERTEX_POINT ( 'NONE', #33865 ) ;
#65985 = EDGE_CURVE ( 'NONE', #9430, #53961, #10548, .T. ) ;
#65987 = CARTESIAN_POINT ( 'NONE',  ( 204.2457645315488719, 276.8829539310449945, 14.53406579917280261 ) ) ;
#65986 = CARTESIAN_POINT ( 'NONE',  ( 159.7094009514765673, 278.7085482198767181, -9.578478531124655859 ) ) ;
#65988 = CARTESIAN_POINT ( 'NONE',  ( 192.0332533962074706, 298.0356437054567778, 11.70630383928353346 ) ) ;
#65989 = ORIENTED_EDGE ( 'NONE', *, *, #25121, .F. ) ;
#65990 = CARTESIAN_POINT ( 'NONE',  ( 76.77247148145950462, 52.74177840875945122, 15.84678155200985472 ) ) ;
#65991 = CARTESIAN_POINT ( 'NONE',  ( 178.0177195456097934, 264.0150987585001303, 14.74376966487514728 ) ) ;
#65992 = VERTEX_POINT ( 'NONE', #96677 ) ;
#65993 = CARTESIAN_POINT ( 'NONE',  ( 69.05014585453179166, 64.34709911403272997, -11.93475642575615758 ) ) ;
#65994 = CARTESIAN_POINT ( 'NONE',  ( 88.54812304393657030, 43.90120638611161752, -0.3063217976418578514 ) ) ;
#65995 = EDGE_CURVE ( 'NONE', #17891, #65871, #47500, .T. ) ;
#65996 = EDGE_CURVE ( 'NONE', #70505, #45420, #83793, .T. ) ;
#65997 = AXIS2_PLACEMENT_3D ( 'NONE', #39204, #55405, #47811 ) ;
#65998 = CARTESIAN_POINT ( 'NONE',  ( 181.8559320684326224, 273.7276056269956257, 17.73031764801637067 ) ) ;
#65999 = ORIENTED_EDGE ( 'NONE', *, *, #89791, .T. ) ;
#66000 = CARTESIAN_POINT ( 'NONE',  ( 159.7174048142719300, 254.4296914360206188, -15.32135016668171268 ) ) ;
#66001 = CARTESIAN_POINT ( 'NONE',  ( 166.2676906195303843, 273.7285489158338123, -15.68808713425968726 ) ) ;
#66002 = AXIS2_PLACEMENT_3D ( 'NONE', #48940, #73737, #66127 ) ;
#66003 = CARTESIAN_POINT ( 'NONE',  ( 73.39892793531787163, 58.47633737766673079, 15.73411582304112422 ) ) ;
#66004 = ORIENTED_EDGE ( 'NONE', *, *, #37950, .F. ) ;
#66005 = ADVANCED_FACE ( 'NONE', ( #61103 ), #13056, .T. ) ;
#66006 = CARTESIAN_POINT ( 'NONE',  ( 177.8451913026518696, 279.4803919955936635, -16.40387529202023487 ) ) ;
#66007 = CARTESIAN_POINT ( 'NONE',  ( 169.2792358738191467, 261.7039271258366853, -15.92131019875227871 ) ) ;
#66008 = EDGE_CURVE ( 'NONE', #93223, #75236, #33773, .T. ) ;
#66009 = ORIENTED_EDGE ( 'NONE', *, *, #69063, .T. ) ;
#66010 = CARTESIAN_POINT ( 'NONE',  ( 156.7768383517496886, 266.5326515087351140, -16.24880001600576662 ) ) ;
#66011 = ORIENTED_EDGE ( 'NONE', *, *, #40283, .F. ) ;
#66012 = DIRECTION ( 'NONE',  ( -1.000000000000000000, 0.000000000000000000, 0.000000000000000000 ) ) ;
#66013 = VERTEX_POINT ( 'NONE', #77323 ) ;
#66014 = VECTOR ( 'NONE', #15370, 1000.000000000000114 ) ;
#66015 = LINE ( 'NONE', #87405, #14037 ) ;
#66016 = CARTESIAN_POINT ( 'NONE',  ( 193.3179319617974556, 295.8105151584606460, 14.44946628013603984 ) ) ;
#66017 = CARTESIAN_POINT ( 'NONE',  ( 189.5844812082644921, 299.2301777039353397, -4.284560523659924236 ) ) ;
#66018 = CARTESIAN_POINT ( 'NONE',  ( 13.51924585473484974, 23.50829794293879615, -10.00000000000000355 ) ) ;
#66019 = CARTESIAN_POINT ( 'NONE',  ( 152.6992418905140028, 266.1641500988167763, 17.27767170937316621 ) ) ;
#66020 = CARTESIAN_POINT ( 'NONE',  ( -19.65312891409030271, 93.06504152958497400, 177.5919119679930134 ) ) ;
#66021 = CARTESIAN_POINT ( 'NONE',  ( 159.0721002551609615, 255.1260356218077447, -16.41935828481064163 ) ) ;
#66022 = AXIS2_PLACEMENT_3D ( 'NONE', #16278, #31968, #16776 ) ;
#66023 = ORIENTED_EDGE ( 'NONE', *, *, #57162, .T. ) ;
#66024 = CARTESIAN_POINT ( 'NONE',  ( 76.32033379547380036, 57.26470140725930236, -16.14692908151009831 ) ) ;
#66025 = CARTESIAN_POINT ( 'NONE',  ( -56.29836151245349640, 34.88994676555962116, 10.00000000000000000 ) ) ;
#66027 = CARTESIAN_POINT ( 'NONE',  ( -13.79761285583127872, 128.9229902121449811, 8.559299291603829198E-14 ) ) ;
#66026 = CARTESIAN_POINT ( 'NONE',  ( 165.6020508749395219, 253.3981458705029013, 13.80445833791507404 ) ) ;
#66029 = VERTEX_POINT ( 'NONE', #93551 ) ;
#66028 = CARTESIAN_POINT ( 'NONE',  ( 46.54103524584390783, 115.8319611975524595, -10.00000000000000000 ) ) ;
#66030 = ORIENTED_EDGE ( 'NONE', *, *, #94579, .T. ) ;
#66031 = B_SPLINE_CURVE_WITH_KNOTS ( 'NONE', 3,
 ( #50699, #66412, #27906, #58786, #28400, #49229, #80163, #10730, #34037, #44584, #67908, #14700, #91235, #61289, #36499, #46078, #22802, #83139, #21801, #61785, #67402, #84154, #20829, #36998 ),
 .UNSPECIFIED., .F., .F.,
 ( 4, 2, 2, 2, 2, 2, 2, 2, 2, 2, 2, 4 ),
 ( 0.000000000000000000, 0.1250000000000071332, 0.2500000000000142664, 0.3750000000000214273, 0.4375000000000193179, 0.5000000000000172085, 0.5625000000000150990, 0.6250000000000129896, 0.6875000000000108802, 0.7500000000000087708, 0.8750000000000044409, 1.000000000000000000 ),
 .UNSPECIFIED. ) ;
#66032 = CARTESIAN_POINT ( 'NONE',  ( 186.7717813178919641, 276.6902415280541732, 16.68087175089405250 ) ) ;
#66033 = CARTESIAN_POINT ( 'NONE',  ( 83.34286953481752391, 51.57169424047764750, -14.50199425999806735 ) ) ;
#66034 = CARTESIAN_POINT ( 'NONE',  ( 163.7042615485562749, 247.9028158862528244, 8.306869792309049316 ) ) ;
#66035 = DIRECTION ( 'NONE',  ( 0.000000000000000000, 0.000000000000000000, 1.000000000000000000 ) ) ;
#66036 = CARTESIAN_POINT ( 'NONE',  ( 199.3060188183595471, 285.4388444827598050, -18.38090059002489696 ) ) ;
#66037 = CARTESIAN_POINT ( 'NONE',  ( 190.1033615149403033, 301.3783144969264640, 0.1109884230970359376 ) ) ;
#66038 = VERTEX_POINT ( 'NONE', #55986 ) ;
#66039 = CARTESIAN_POINT ( 'NONE',  ( -22.42236680055709641, 157.8615022471902591, 0.000000000000000000 ) ) ;
#66040 = CARTESIAN_POINT ( 'NONE',  ( 185.0338664617105735, 285.2265299937916438, -16.56857016979445874 ) ) ;
#66041 = AXIS2_PLACEMENT_3D ( 'NONE', #12372, #95007, #88426 ) ;
#66042 = DIRECTION ( 'NONE',  ( -0.7905172007421662483, 0.000000000000000000, -0.6124398381316892293 ) ) ;
#66044 = EDGE_CURVE ( 'NONE', #74402, #50322, #92556, .T. ) ;
#66043 = FACE_OUTER_BOUND ( 'NONE', #51669, .T. ) ;
#66045 = CARTESIAN_POINT ( 'NONE',  ( 35.43895548624280423, 191.2677522451418781, 10.00000000000009592 ) ) ;
#66046 = CARTESIAN_POINT ( 'NONE',  ( 112.2989703957094605, 226.4548013555409796, -4.594050593750042211 ) ) ;
#66047 = CARTESIAN_POINT ( 'NONE',  ( 181.0435294081004827, 294.2478791158599165, -2.647642130805165195 ) ) ;
#66048 = CARTESIAN_POINT ( 'NONE',  ( 167.2900023830132170, 283.1360949131732809, -11.47530909209802275 ) ) ;
#66049 = DIRECTION ( 'NONE',  ( 0.000000000000000000, 0.000000000000000000, 1.000000000000000000 ) ) ;
#66050 = CARTESIAN_POINT ( 'NONE',  ( 208.3210024379012282, 269.8244348243121635, 2.045688540111487264 ) ) ;
#66051 = CARTESIAN_POINT ( 'NONE',  ( 22.47598482088346117, 171.5327760586659451, 1.948934522072303157E-15 ) ) ;
#66052 = DIRECTION ( 'NONE',  ( 0.4999999999999992784, -0.8660254037844390407, 0.000000000000000000 ) ) ;
#66053 = ORIENTED_EDGE ( 'NONE', *, *, #40780, .F. ) ;
#66054 = ORIENTED_EDGE ( 'NONE', *, *, #41807, .F. ) ;
#66055 = FACE_OUTER_BOUND ( 'NONE', #3967, .T. ) ;
#66056 = CARTESIAN_POINT ( 'NONE',  ( 185.7739710534217181, 258.8015903883575675, -5.557864263316704800 ) ) ;
#66057 = CARTESIAN_POINT ( 'NONE',  ( 70.11469351433765951, 71.12949179974985725, -0.2432596123983654379 ) ) ;
#66058 = CARTESIAN_POINT ( 'NONE',  ( 193.6400864899449914, 264.2141502298499631, -4.346378420391690867 ) ) ;
#66059 = LINE ( 'NONE', #50352, #43006 ) ;
#66060 = CARTESIAN_POINT ( 'NONE',  ( 185.5250016208995874, 286.2042338949377722, 15.39722344320556680 ) ) ;
#66061 = CARTESIAN_POINT ( 'NONE',  ( 73.95565718806818722, 68.30423517461105121, -11.66005733018688773 ) ) ;
#66062 = CARTESIAN_POINT ( 'NONE',  ( 46.88655524640979166, 204.0024278399160949, -9.188101187500093303 ) ) ;
#66063 = CARTESIAN_POINT ( 'NONE',  ( 85.23541620384800410, 230.0177522451419350, 5.000000000000046185 ) ) ;
#66064 = CIRCLE ( 'NONE', #22375, 17.82106496071138224 ) ;
#66065 = VERTEX_POINT ( 'NONE', #23102 ) ;
#66066 = LINE ( 'NONE', #97973, #91764 ) ;
#66067 = ADVANCED_FACE ( 'NONE', ( #16014 ), #47894, .T. ) ;
#66068 = CARTESIAN_POINT ( 'NONE',  ( -5.174027508517049512, 174.4865022471903160, 10.00000000000009415 ) ) ;
#66069 = VECTOR ( 'NONE', #12705, 1000.000000000000114 ) ;
#66070 = CARTESIAN_POINT ( 'NONE',  ( -1.340060878953613477, 170.0333772461660828, 9.188101187500095079 ) ) ;
#66071 = VECTOR ( 'NONE', #69374, 1000.000000000000000 ) ;
#66072 = CARTESIAN_POINT ( 'NONE',  ( 68.84812201532827203, 64.26021157803218387, -11.91067767038833480 ) ) ;
#66073 = CARTESIAN_POINT ( 'NONE',  ( 198.9590707264871412, 286.0397762054715827, -17.05306195936250191 ) ) ;
#66074 = CARTESIAN_POINT ( 'NONE',  ( 79.38214399233697804, 46.87024971659150907, 13.67178478057998525 ) ) ;
#66075 = CARTESIAN_POINT ( 'NONE',  ( 146.8153075009282134, 276.3554234099810287, -4.113808735271278216 ) ) ;
#66076 = CARTESIAN_POINT ( 'NONE',  ( -3.153128914090298274, 64.48620320469859735, 0.000000000000000000 ) ) ;
#66077 = LINE ( 'NONE', #36653, #54700 ) ;
#66078 = EDGE_CURVE ( 'NONE', #14428, #13682, #15497, .T. ) ;
#66079 = CARTESIAN_POINT ( 'NONE',  ( 70.43502381298807791, 70.21998739243254306, 5.513655153572781131 ) ) ;
#66080 = CARTESIAN_POINT ( 'NONE',  ( 164.4858674010174298, 245.7491158648375347, -2.958464974013825355 ) ) ;
#66081 = VERTEX_POINT ( 'NONE', #70712 ) ;
#66082 = EDGE_CURVE ( 'NONE', #91721, #71865, #78836, .T. ) ;
#66083 = CARTESIAN_POINT ( 'NONE',  ( -4.668846022976141263, 178.1115022471903160, -5.000000000000047962 ) ) ;
#66084 = DIRECTION ( 'NONE',  ( 0.7005979833698788850, 0.7135562106085679979, 0.000000000000000000 ) ) ;
#66085 = CARTESIAN_POINT ( 'NONE',  ( 125.1810982770029881, 233.8923013555409796, 4.594050593750050204 ) ) ;
#66086 = CARTESIAN_POINT ( 'NONE',  ( 22.44070990177030112, 31.14336893147756413, 7.433330006724141015 ) ) ;
#66087 = CARTESIAN_POINT ( 'NONE',  ( 74.70353909524752112, 67.05423462026553239, 12.97237599094835936 ) ) ;
#66088 = LINE ( 'NONE', #87958, #54871 ) ;
#66090 = CARTESIAN_POINT ( 'NONE',  ( 74.63372323989780455, 66.93453420673688470, 13.02704161780705761 ) ) ;
#66089 = CARTESIAN_POINT ( 'NONE',  ( 82.10523990517461357, 41.85707133252695655, -5.529865280922476423 ) ) ;
#66091 = ORIENTED_EDGE ( 'NONE', *, *, #36457, .T. ) ;
#66092 = CARTESIAN_POINT ( 'NONE',  ( 151.4361976351029000, 268.3518069213970421, 15.15218985681980612 ) ) ;
#66093 = CARTESIAN_POINT ( 'NONE',  ( 207.6125545502318346, 271.0515025602701940, -0.9531936345505281905 ) ) ;
#66094 = CARTESIAN_POINT ( 'NONE',  ( 190.6291740046558232, 300.0075276777452586, 3.996728472176227509 ) ) ;
#66095 = CARTESIAN_POINT ( 'NONE',  ( 41.82599275875796252, 62.29945068332010294, -10.00000000000000000 ) ) ;
#66096 = CARTESIAN_POINT ( 'NONE',  ( 81.44589832458051148, 55.42546683620729908, -16.32034488869437894 ) ) ;
#66097 = ORIENTED_EDGE ( 'NONE', *, *, #36360, .F. ) ;
#66098 = CARTESIAN_POINT ( 'NONE',  ( 68.55578159652473857, 66.09187073463988327, 10.06848484671900756 ) ) ;
#66099 = DIRECTION ( 'NONE',  ( 0.000000000000000000, -0.000000000000000000, 1.000000000000000000 ) ) ;
#66100 = CARTESIAN_POINT ( 'NONE',  ( 71.73821799984662562, 72.51259063078050815, 0.9720659048468541785 ) ) ;
#66101 = CARTESIAN_POINT ( 'NONE',  ( 82.70906748317777613, 41.57766049848077472, 3.737552679734466032 ) ) ;
#66102 = CARTESIAN_POINT ( 'NONE',  ( 198.9271290976750208, 272.1319763448123581, 12.23897718048457151 ) ) ;
#66103 = DIRECTION ( 'NONE',  ( 0.8660254037844395958, 0.4999999999999985567, 0.000000000000000000 ) ) ;
#66104 = LINE ( 'NONE', #97528, #82557 ) ;
#66105 = CARTESIAN_POINT ( 'NONE',  ( 148.5064712399015718, 274.2256579647487342, -7.884393238739946241 ) ) ;
#66106 = EDGE_CURVE ( 'NONE', #90058, #44657, #27079, .T. ) ;
#66107 = CARTESIAN_POINT ( 'NONE',  ( 8.995063969029878592, 17.14441083166259006, 10.00000000000000533 ) ) ;
#66108 = CARTESIAN_POINT ( 'NONE',  ( 83.51785737385900177, 46.57979345909983238, 11.73479753357512401 ) ) ;
#66109 = EDGE_LOOP ( 'NONE', ( #13181, #66381, #19041, #2517 ) ) ;
#66110 = CARTESIAN_POINT ( 'NONE',  ( 73.67824366217406862, 55.52431661998091528, 16.58293631993679540 ) ) ;
#66111 = CARTESIAN_POINT ( 'NONE',  ( 148.3874010092782498, 273.6324775792697892, -8.328854486678444857 ) ) ;
#66112 = CARTESIAN_POINT ( 'NONE',  ( 159.5557817863224557, 264.0312905115982289, -17.30914965676515038 ) ) ;
#66113 = ORIENTED_EDGE ( 'NONE', *, *, #19029, .F. ) ;
#66114 = CARTESIAN_POINT ( 'NONE',  ( 78.87940645753282354, 60.08920343663678665, 16.11186154035030782 ) ) ;
#66115 = DIRECTION ( 'NONE',  ( -1.000000000000000000, 0.000000000000000000, 0.000000000000000000 ) ) ;
#66116 = VECTOR ( 'NONE', #35783, 1000.000000000000227 ) ;
#66117 = CARTESIAN_POINT ( 'NONE',  ( 189.5650719070094112, 268.9827374331138685, -14.62586421207108955 ) ) ;
#66118 = VERTEX_POINT ( 'NONE', #46913 ) ;
#66119 = CARTESIAN_POINT ( 'NONE',  ( 83.63833477162943097, 231.3464784336661637, 1.353441290958777525E-15 ) ) ;
#66120 = CARTESIAN_POINT ( 'NONE',  ( 84.31620464638353951, 49.88582837545166626, -13.33668689155092757 ) ) ;
#66121 = CARTESIAN_POINT ( 'NONE',  ( 84.68407782013028395, 49.81677542588726482, -13.17038101989053622 ) ) ;
#66122 = CARTESIAN_POINT ( 'NONE',  ( 81.30093862219625578, 42.22353087488599499, -7.211150227892720643 ) ) ;
#66123 = ORIENTED_EDGE ( 'NONE', *, *, #90907, .F. ) ;
#66124 = EDGE_CURVE ( 'NONE', #19199, #88235, #84953, .T. ) ;
#66125 = CARTESIAN_POINT ( 'NONE',  ( 198.2505066714982149, 285.2670451491296149, 0.000000000000000000 ) ) ;
#66126 = ORIENTED_EDGE ( 'NONE', *, *, #30590, .F. ) ;
#66127 = DIRECTION ( 'NONE',  ( -0.5000000000000002220, 0.8660254037844384856, 0.000000000000000000 ) ) ;
#66129 = ORIENTED_EDGE ( 'NONE', *, *, #29455, .F. ) ;
#66128 = B_SPLINE_CURVE_WITH_KNOTS ( 'NONE', 3,
 ( #80018, #85633, #31862, #62762 ),
 .UNSPECIFIED., .F., .F.,
 ( 4, 4 ),
 ( 0.009429426956353095107, 0.01478986007845733280 ),
 .UNSPECIFIED. ) ;
#66130 = CARTESIAN_POINT ( 'NONE',  ( 171.5402001534711189, 272.6215992900089873, -17.66257148859359560 ) ) ;
#66131 = CARTESIAN_POINT ( 'NONE',  ( 203.0862352702880003, 278.8913175244117610, -15.09542727681365015 ) ) ;
#66132 = ORIENTED_EDGE ( 'NONE', *, *, #19988, .T. ) ;
#66133 = CARTESIAN_POINT ( 'NONE',  ( 192.3926678149021825, 295.4131196713046847, -13.42882169270698256 ) ) ;
#66134 = CARTESIAN_POINT ( 'NONE',  ( 82.21410988463139802, 40.73976263607374193, 3.762362152811430160 ) ) ;
#66135 = CARTESIAN_POINT ( 'NONE',  ( 151.4587940952941381, 268.7129208180788851, 14.41012130913438050 ) ) ;
#66136 = VECTOR ( 'NONE', #80288, 1000.000000000000000 ) ;
#66137 = PLANE ( 'NONE',  #51094 ) ;
#66138 = CARTESIAN_POINT ( 'NONE',  ( 172.6505904036989136, 280.8448313155626579, -15.39888677054324440 ) ) ;
#66140 = CARTESIAN_POINT ( 'NONE',  ( 18.55511606660780899, 34.21091486745861232, -1.111400068045478839E-16 ) ) ;
#66139 = VECTOR ( 'NONE', #95183, 1000.000000000000227 ) ;
#66141 = CARTESIAN_POINT ( 'NONE',  ( 141.2293712190596011, 252.3458772461660260, 9.188101187500095079 ) ) ;
#66142 = DIRECTION ( 'NONE',  ( -0.8660254037844387076, -0.4999999999999998890, -0.000000000000000000 ) ) ;
#66143 = CARTESIAN_POINT ( 'NONE',  ( 75.88266154223501303, 55.68909319084332310, 16.14856353405036771 ) ) ;
#66144 = B_SPLINE_CURVE_WITH_KNOTS ( 'NONE', 3,
 ( #47756, #85848, #17893, #8777, #9800, #56862 ),
 .UNSPECIFIED., .F., .F.,
 ( 4, 2, 4 ),
 ( 0.000000000000000000, 0.0004889391310944574218, 0.0009778782621889148437 ),
 .UNSPECIFIED. ) ;
#66145 = CARTESIAN_POINT ( 'NONE',  ( 16.39654754030849659, 10.26216523072493203, -2.296566073217252530E-15 ) ) ;
#66147 = EDGE_CURVE ( 'NONE', #96097, #90241, #94057, .T. ) ;
#66146 = AXIS2_PLACEMENT_3D ( 'NONE', #71262, #18560, #79888 ) ;
#66148 = ORIENTED_EDGE ( 'NONE', *, *, #70720, .T. ) ;
#66149 = CARTESIAN_POINT ( 'NONE',  ( 163.9835549846052913, 281.8964108386193743, 8.550639651353808546 ) ) ;
#66150 = CIRCLE ( 'NONE', #83977, 9.212605237762131694 ) ;
#66152 = ORIENTED_EDGE ( 'NONE', *, *, #53077, .T. ) ;
#66151 = CARTESIAN_POINT ( 'NONE',  ( 85.35583701238070375, 48.33319239702164083, -12.28927654967824701 ) ) ;
#66153 = DIRECTION ( 'NONE',  ( -0.8660254037844387076, -0.4999999999999998890, -0.000000000000000000 ) ) ;
#66154 = CARTESIAN_POINT ( 'NONE',  ( 170.5277015564773535, 288.6887139008781560, -5.574706778066785162 ) ) ;
#66155 = CARTESIAN_POINT ( 'NONE',  ( 154.7406134505728232, 277.6489013670466193, 7.166873607358588139 ) ) ;
#66156 = CARTESIAN_POINT ( 'NONE',  ( 165.4256356872135427, 246.8481156136332970, -1.873358472144460274 ) ) ;
#66157 = CARTESIAN_POINT ( 'NONE',  ( 174.8559098654806689, 282.1809755462382441, 14.33990550510826090 ) ) ;
#66158 = CARTESIAN_POINT ( 'NONE',  ( 85.04454326977196388, 42.52624631695034907, 2.010354791463878410 ) ) ;
#66159 = CARTESIAN_POINT ( 'NONE',  ( 87.99802445900249381, 44.07685147378857238, -1.716111015435727527 ) ) ;
#66160 = VECTOR ( 'NONE', #79745, 1000.000000000000227 ) ;
#66161 =( BOUNDED_CURVE ( )  B_SPLINE_CURVE ( 2, ( #75273, #5366, #97586, #21560, #36743, #98582, #75771, #66166, #28158 ),
 .UNSPECIFIED., .F., .T. ) 
 B_SPLINE_CURVE_WITH_KNOTS ( ( 3, 2, 2, 2, 3 ),
 ( 0.1250000000000000000, 0.1263440860215053752, 0.1290322580645161255, 0.1317204301075268758, 0.1330645161290322509 ),
 .UNSPECIFIED. ) 
 CURVE ( )  GEOMETRIC_REPRESENTATION_ITEM ( )  RATIONAL_B_SPLINE_CURVE ( ( 0.9330127018922194093, 0.9330127018922194093, 1.000000000000000000, 0.8660254037844387076, 1.000000000000000000, 0.8660254037844387076, 1.000000000000000000, 0.9330127018922194093, 0.9330127018922194093 ) ) 
 REPRESENTATION_ITEM ( '' )  );
#66162 = ORIENTED_EDGE ( 'NONE', *, *, #15644, .F. ) ;
#66163 = CARTESIAN_POINT ( 'NONE',  ( 184.9083320494203235, 273.0902778310993426, -16.51607607619348528 ) ) ;
#66164 = CARTESIAN_POINT ( 'NONE',  ( 65.86576390661227265, 69.15346480495860249, 0.2105079060664491741 ) ) ;
#66165 = VERTEX_POINT ( 'NONE', #30723 ) ;
#66166 = CARTESIAN_POINT ( 'NONE',  ( 2.555990577167667421, 183.8297689869268936, -2.679491924311252493 ) ) ;
#66167 = CARTESIAN_POINT ( 'NONE',  ( 202.8161320915185968, 268.6936331435907732, -2.878963594486870115 ) ) ;
#66168 = DIRECTION ( 'NONE',  ( -0.8218955677251095215, -0.5696381972391070247, 0.000000000000000000 ) ) ;
#66169 = CARTESIAN_POINT ( 'NONE',  ( 190.0707697440390689, 301.4347651000360884, 4.271360729158901748 ) ) ;
#66170 = PLANE ( 'NONE',  #77511 ) ;
#66172 = CARTESIAN_POINT ( 'NONE',  ( 88.13962338646859962, 43.88173199026377347, 2.505344897735772847 ) ) ;
#66171 = CARTESIAN_POINT ( 'NONE',  ( 71.47791206682282450, 72.34364865201938244, -1.216664393387148380 ) ) ;
#66173 = VECTOR ( 'NONE', #74599, 1000.000000000000000 ) ;
#66174 = DIRECTION ( 'NONE',  ( -0.000000000000000000, -0.000000000000000000, -1.000000000000000000 ) ) ;
#66175 = ORIENTED_EDGE ( 'NONE', *, *, #7828, .T. ) ;
#66176 = B_SPLINE_SURFACE_WITH_KNOTS ( 'NONE', 3, 1, ( 
 ( #58104, #89086 ),
 ( #65697, #80966 ),
 ( #5901, #21127 ),
 ( #43393, #67198 ),
 ( #74832, #75323 ),
 ( #13030, #81943 ),
 ( #43892, #89560 ),
 ( #27221, #59581 ),
 ( #5412, #36792 ),
 ( #82947, #66698 ),
 ( #73324, #67704 ),
 ( #20121, #19635 ),
 ( #50495, #36295 ),
 ( #52004, #13520 ),
 ( #50993, #81449 ),
 ( #12521, #11531 ),
 ( #4405, #42391 ),
 ( #3913, #12021 ),
 ( #73811, #35301 ),
 ( #74336, #44883 ),
 ( #75823, #46891 ),
 ( #30194, #15992 ),
 ( #45868, #62070 ),
 ( #37782, #6410 ),
 ( #77815, #83438 ),
 ( #91532, #29212 ),
 ( #61080, #69187 ),
 ( #60080, #23573 ),
 ( #92051, #92532 ),
 ( #14004, #23079 ),
 ( #53971, #6892 ),
 ( #76793, #15474 ),
 ( #99616, #84437 ),
 ( #69687, #85443 ) ),
 .UNSPECIFIED., .T., .F., .F.,
 ( 4, 2, 2, 2, 2, 2, 2, 2, 2, 2, 2, 2, 2, 2, 2, 2, 4 ),
 ( 2, 2 ),
 ( 0.000000000000000000, 0.06250000000000000000, 0.1250000000000000000, 0.1875000000000000000, 0.2500000000000000000, 0.3125000000000000000, 0.3750000000000000000, 0.4375000000000000000, 0.5000000000000000000, 0.5625000000000000000, 0.6250000000000000000, 0.6875000000000000000, 0.7500000000000000000, 0.8125000000000000000, 0.8750000000000000000, 0.9375000000000000000, 1.000000000000000000 ),
 ( 0.000000000000000000, 1.000000000000000000 ),
 .UNSPECIFIED. ) ;
#66177 = ORIENTED_EDGE ( 'NONE', *, *, #78036, .T. ) ;
#66178 = CARTESIAN_POINT ( 'NONE',  ( 72.03258563326085095, 62.35762028613417840, -14.22870005908225544 ) ) ;
#66179 = CARTESIAN_POINT ( 'NONE',  ( 80.44411425790228520, 57.92825487739349200, 16.25450948704126830 ) ) ;
#66180 = B_SPLINE_CURVE_WITH_KNOTS ( 'NONE', 3,
 ( #61844, #47644, #8659, #15745 ),
 .UNSPECIFIED., .F., .F.,
 ( 4, 4 ),
 ( 0.01054893006521931756, 0.01602403026634139499 ),
 .UNSPECIFIED. ) ;
#66181 = CARTESIAN_POINT ( 'NONE',  ( 70.66815415073801887, 66.12807013279959278, -11.28611302301944441 ) ) ;
#66182 = CARTESIAN_POINT ( 'NONE',  ( 174.9101025265537999, 290.5686053034625047, 2.562613730387248712 ) ) ;
#66183 = CARTESIAN_POINT ( 'NONE',  ( 192.8325075361489382, 296.6512949269187516, 11.74553025762331515 ) ) ;
#66184 = CARTESIAN_POINT ( 'NONE',  ( 81.00087151702695110, 43.68496140122994120, -9.524658774912921899 ) ) ;
#66185 = CARTESIAN_POINT ( 'NONE',  ( -15.10528209597770299, 24.46087392797018722, 10.00000000000000000 ) ) ;
#66186 = CARTESIAN_POINT ( 'NONE',  ( 12.40843950188935629, 165.7202760586659736, -5.415160957724236172E-17 ) ) ;
#66187 = CARTESIAN_POINT ( 'NONE',  ( 98.36111373172988692, 227.5958772461660260, -9.188101187500095079 ) ) ;
#66188 = CARTESIAN_POINT ( 'NONE',  ( 203.5555343017997529, 278.0784677578903370, -15.71723084798551362 ) ) ;
#66189 = CARTESIAN_POINT ( 'NONE',  ( 38.12724268070488876, 199.4865022471903160, -10.00000000000009592 ) ) ;
#66190 = CARTESIAN_POINT ( 'NONE',  ( 186.7244937263979523, 295.9831862837335734, -7.509257591937855913 ) ) ;
#66191 = CARTESIAN_POINT ( 'NONE',  ( 21.20245638554208867, 36.22472881207376361, 177.5919119679930134 ) ) ;
#66192 = CARTESIAN_POINT ( 'NONE',  ( 195.2221546850906009, 283.6286238037334897, 17.82163192674956420 ) ) ;
#66193 = CARTESIAN_POINT ( 'NONE',  ( 150.8555837531579868, 276.0290483310748755, -8.437460036063264113 ) ) ;
#66194 = FACE_OUTER_BOUND ( 'NONE', #61267, .T. ) ;
#66195 = LINE ( 'NONE', #96639, #16792 ) ;
#66196 = B_SPLINE_CURVE_WITH_KNOTS ( 'NONE', 3,
 ( #55123, #32834, #70335, #23723, #17651, #87115, #93681, #2460, #47532, #48033, #17135, #78460, #18150, #9044, #78975, #9562, #40425, #71358 ),
 .UNSPECIFIED., .F., .F.,
 ( 4, 2, 2, 2, 2, 2, 2, 2, 4 ),
 ( 0.000000000000000000, 0.0003132019396418706447, 0.0006264038792837412894, 0.0009396058189256119341, 0.001252807758567482579, 0.001566009698209353332, 0.001879211637851223868, 0.002192413577493094404, 0.002505615517134965158 ),
 .UNSPECIFIED. ) ;
#66197 = CARTESIAN_POINT ( 'NONE',  ( 84.62070576355738183, 50.25222463068733703, 13.86530520652494758 ) ) ;
#66198 = EDGE_CURVE ( 'NONE', #29349, #2126, #85983, .T. ) ;
#66199 = CARTESIAN_POINT ( 'NONE',  ( 207.3589495855971450, 271.0586446502292119, 2.456771036675355457 ) ) ;
#66200 = CARTESIAN_POINT ( 'NONE',  ( 138.7926119064592569, 262.4860189848785694, -2.679491924311252493 ) ) ;
#66201 = EDGE_CURVE ( 'NONE', #34850, #59964, #39781, .T. ) ;
#66203 = EDGE_CURVE ( 'NONE', #73362, #60492, #23597, .T. ) ;
#66202 = DIRECTION ( 'NONE',  ( 0.9053220668578600971, 0.4247257412262792631, 0.000000000000000000 ) ) ;
#66204 = VECTOR ( 'NONE', #34949, 1000.000000000000000 ) ;
#66205 = ADVANCED_FACE ( 'NONE', ( #86477 ), #1327, .T. ) ;
#66206 = CARTESIAN_POINT ( 'NONE',  ( 72.19064823929512897, 221.6744531367911293, 4.594050593750047540 ) ) ;
#66207 = CARTESIAN_POINT ( 'NONE',  ( 207.2707369601997982, 271.6435479931266173, -5.381413637561199614 ) ) ;
#66208 = DIRECTION ( 'NONE',  ( 0.4999999999999992784, -0.8660254037844390407, 0.000000000000000000 ) ) ;
#66209 = VECTOR ( 'NONE', #37034, 1000.000000000000114 ) ;
#66210 = CARTESIAN_POINT ( 'NONE',  ( -15.30390832730448913, 102.7700744756162692, 12.27820281893983356 ) ) ;
#66212 = CARTESIAN_POINT ( 'NONE',  ( 85.68213310926148552, 42.83582516110543992, -1.677889640976326868 ) ) ;
#66211 = CARTESIAN_POINT ( 'NONE',  ( 196.0395593785976018, 291.0965181932902510, 15.97855489120023087 ) ) ;
#66213 = CARTESIAN_POINT ( 'NONE',  ( 75.71688963635942571, 65.45405155058689672, 14.28099675560567228 ) ) ;
#66214 = CARTESIAN_POINT ( 'NONE',  ( 80.31380282231825163, 44.31269810431638945, 11.34184801982937429 ) ) ;
#66215 = CARTESIAN_POINT ( 'NONE',  ( 29.36891313204580456, 35.14336893147757479, 7.433330006724141015 ) ) ;
#66216 = DIRECTION ( 'NONE',  ( -0.9172102815912978047, -0.3984034379159046568, 0.000000000000000000 ) ) ;
#66217 = CARTESIAN_POINT ( 'NONE',  ( 135.6272693901030379, 239.1115022471902023, -5.000000000000041744 ) ) ;
#66218 = ORIENTED_EDGE ( 'NONE', *, *, #90808, .F. ) ;
#66219 = CARTESIAN_POINT ( 'NONE',  ( 16.96131155903493593, 31.83396525600390348, -2.839279412974133887 ) ) ;
#66220 = VECTOR ( 'NONE', #67163, 1000.000000000000000 ) ;
#66221 = CARTESIAN_POINT ( 'NONE',  ( 17.25239830753785952, 10.36477965099639498, 1.583844403245364907 ) ) ;
#66222 = CARTESIAN_POINT ( 'NONE',  ( -31.05641173554239032, 93.49636139580346139, 11.47754913427577783 ) ) ;
#66223 = CARTESIAN_POINT ( 'NONE',  ( 191.4139643784075702, 288.5963964191323612, -15.97086743186968150 ) ) ;
#66224 = ORIENTED_EDGE ( 'NONE', *, *, #56597, .F. ) ;
#66225 = CARTESIAN_POINT ( 'NONE',  ( 86.15223587325151300, 47.11913640227773925, 10.79538652562921541 ) ) ;
#66226 = CARTESIAN_POINT ( 'NONE',  ( 153.7445562035061073, 266.9407863685345319, 16.39162974861245559 ) ) ;
#66227 = LINE ( 'NONE', #26727, #38740 ) ;
#66228 = AXIS2_PLACEMENT_3D ( 'NONE', #86113, #30846, #92681 ) ;
#66229 = CARTESIAN_POINT ( 'NONE',  ( 137.7201641159153098, 256.9865022471903444, 10.00000000000009237 ) ) ;
#66230 = CYLINDRICAL_SURFACE ( 'NONE', #27852, 12.50000000000000000 ) ;
#66231 = CARTESIAN_POINT ( 'NONE',  ( 74.89001754810668388, 53.31247712445269826, 16.04945090674765851 ) ) ;
#66232 = ORIENTED_EDGE ( 'NONE', *, *, #53447, .F. ) ;
#66233 = CARTESIAN_POINT ( 'NONE',  ( 85.61210927225859280, 46.71934343149948887, 10.13913704453490539 ) ) ;
#66234 = ORIENTED_EDGE ( 'NONE', *, *, #427, .T. ) ;
#66235 = CARTESIAN_POINT ( 'NONE',  ( 38.65784837781280459, 56.65029301956751340, 10.00000000000000000 ) ) ;
#66236 = CARTESIAN_POINT ( 'NONE',  ( 86.86805282215009072, 44.88340327883143743, 6.465678163750347984 ) ) ;
#66237 = ORIENTED_EDGE ( 'NONE', *, *, #51252, .F. ) ;
#66238 = DIRECTION ( 'NONE',  ( -0.5906904945688911113, 0.000000000000000000, -0.8068982213550597304 ) ) ;
#66239 = VERTEX_POINT ( 'NONE', #7930 ) ;
#66240 = CARTESIAN_POINT ( 'NONE',  ( 71.97624815057693581, 71.57072644777218784, 5.573434703584684513 ) ) ;
#66241 = DIRECTION ( 'NONE',  ( -0.8660254037844387076, -0.4999999999999998890, -0.000000000000000000 ) ) ;
#66242 = CARTESIAN_POINT ( 'NONE',  ( 194.1641048280396262, 280.7869678786154282, -17.47222775142457962 ) ) ;
#66243 = CARTESIAN_POINT ( 'NONE',  ( 87.87366831029828518, 44.19753277059973584, -4.411077605820552527 ) ) ;
#66244 = CARTESIAN_POINT ( 'NONE',  ( 201.1060504099706350, 282.3210983108598384, -18.18000168485860257 ) ) ;
#66245 = CIRCLE ( 'NONE', #22557, 70.00000000000001421 ) ;
#66246 = CYLINDRICAL_SURFACE ( 'NONE', #25168, 17.82106496071139645 ) ;
#66247 = CARTESIAN_POINT ( 'NONE',  ( 34.35336353842534152, 22.76004757982091675, 5.678558825948272215 ) ) ;
#66248 = CARTESIAN_POINT ( 'NONE',  ( -15.31269525828471068, 104.2312461070085021, 45.19948692389422717 ) ) ;
#66249 = CARTESIAN_POINT ( 'NONE',  ( 166.9861783932322226, 275.8614021614311014, 14.86566658955477216 ) ) ;
#66250 = CARTESIAN_POINT ( 'NONE',  ( 189.9696409261737529, 300.5309180763717904, 0.2178362128448007862 ) ) ;
#66251 = ORIENTED_EDGE ( 'NONE', *, *, #30407, .T. ) ;
#66252 = ORIENTED_EDGE ( 'NONE', *, *, #81130, .F. ) ;
#66253 = CARTESIAN_POINT ( 'NONE',  ( 182.6529124911135114, 296.5506374232393227, 0.2862361614567174861 ) ) ;
#66254 = CARTESIAN_POINT ( 'NONE',  ( 84.43973019491031096, 50.14528805649905507, 13.86389828189430062 ) ) ;
#66256 = CARTESIAN_POINT ( 'NONE',  ( 194.2389208611690492, 294.2153155915419802, -15.75132567904764791 ) ) ;
#66255 = CARTESIAN_POINT ( 'NONE',  ( 68.26472058833583390, 65.55548226720446792, 10.44615040622151803 ) ) ;
#66257 = CARTESIAN_POINT ( 'NONE',  ( 85.93470712620026575, 48.23248545518190866, 11.93606436224419376 ) ) ;
#66258 = CARTESIAN_POINT ( 'NONE',  ( 66.08029938247301516, 68.49631965208827467, -2.562324766759315420 ) ) ;
#66259 = CARTESIAN_POINT ( 'NONE',  ( 131.1347626044233152, 236.5177522451417929, 5.000000000000051514 ) ) ;
#66260 = CARTESIAN_POINT ( 'NONE',  ( 205.1793861064249711, 275.2658739283173759, -14.08953480709093675 ) ) ;
#66261 = CARTESIAN_POINT ( 'NONE',  ( 183.4954143574004206, 273.2329798171908237, -17.56828100048216257 ) ) ;
#66262 = DIRECTION ( 'NONE',  ( 0.000000000000000000, 0.000000000000000000, 1.000000000000000000 ) ) ;
#66263 = EDGE_CURVE ( 'NONE', #95838, #68986, #100076, .T. ) ;
#66264 = CARTESIAN_POINT ( 'NONE',  ( 43.83595887736690599, 122.5461495720015677, 177.5919119679930134 ) ) ;
#66265 = CARTESIAN_POINT ( 'NONE',  ( 94.46399941469991290, 225.3458772461660544, 9.188101187500095079 ) ) ;
#66266 = VERTEX_POINT ( 'NONE', #100138 ) ;
#66267 = CYLINDRICAL_SURFACE ( 'NONE', #90059, 70.00000000000002842 ) ;
#66268 = CARTESIAN_POINT ( 'NONE',  ( 166.8004966849435959, 278.2115916653574459, -13.35053495303439952 ) ) ;
#66269 = ADVANCED_FACE ( 'NONE', ( #62094 ), #40294, .T. ) ;
#66270 = ORIENTED_EDGE ( 'NONE', *, *, #16537, .T. ) ;
#66271 = EDGE_LOOP ( 'NONE', ( #47100, #22057, #49787, #32347 ) ) ;
#66272 = CARTESIAN_POINT ( 'NONE',  ( 87.23690874686347740, 46.15778144619924461, -8.941654336830676897 ) ) ;
#66273 = FACE_OUTER_BOUND ( 'NONE', #25904, .T. ) ;
#66274 = CARTESIAN_POINT ( 'NONE',  ( 157.8092552871339365, 257.3133472685137235, 17.04082256169242626 ) ) ;
#66275 = CARTESIAN_POINT ( 'NONE',  ( 206.4484807199597753, 273.0677375780628608, -9.220527398138528952 ) ) ;
#66276 = CARTESIAN_POINT ( 'NONE',  ( 163.1394982460384995, 248.0810956470044175, 11.48951572717839298 ) ) ;
#66277 = ORIENTED_EDGE ( 'NONE', *, *, #54298, .T. ) ;
#66278 = ORIENTED_EDGE ( 'NONE', *, *, #98872, .T. ) ;
#66279 = FACE_OUTER_BOUND ( 'NONE', #97081, .T. ) ;
#66280 = FACE_OUTER_BOUND ( 'NONE', #81789, .T. ) ;
#66281 = ORIENTED_EDGE ( 'NONE', *, *, #96234, .T. ) ;
#66282 = ADVANCED_FACE ( 'NONE', ( #24610 ), #94444, .F. ) ;
#66283 = VECTOR ( 'NONE', #26765, 1000.000000000000000 ) ;
#66284 = CARTESIAN_POINT ( 'NONE',  ( 194.6771686668232917, 266.3497618079242670, -7.776454509335324339 ) ) ;
#66285 = CARTESIAN_POINT ( 'NONE',  ( 153.3729367728608679, 265.3919680633787834, 16.19611827385041281 ) ) ;
#66286 = CARTESIAN_POINT ( 'NONE',  ( 82.30283500558374499, 44.69232536722564930, 9.873559656175117993 ) ) ;
#66288 = CARTESIAN_POINT ( 'NONE',  ( 69.51817709403496792, 62.60037355296611850, -13.88906238228599577 ) ) ;
#66287 = CARTESIAN_POINT ( 'NONE',  ( 125.9924764494033980, 252.7369531367911293, -4.594050593750048428 ) ) ;
#66289 = FACE_OUTER_BOUND ( 'NONE', #13172, .T. ) ;
#66290 = VECTOR ( 'NONE', #37769, 1000.000000000000000 ) ;
#66291 = VERTEX_POINT ( 'NONE', #42298 ) ;
#66292 = CARTESIAN_POINT ( 'NONE',  ( 204.2956748066270620, 276.7965067987898919, 13.85972809245231119 ) ) ;
#66293 = CARTESIAN_POINT ( 'NONE',  ( 71.30005785884924308, 62.11168698697181156, 14.13435735937659388 ) ) ;
#66294 = CARTESIAN_POINT ( 'NONE',  ( 82.23170604078318036, 40.61139441586372101, -3.203312919990458418 ) ) ;
#66295 = CARTESIAN_POINT ( 'NONE',  ( 80.95862166114621061, 43.54618974350823635, 9.386765060990684972 ) ) ;
#66296 = CARTESIAN_POINT ( 'NONE',  ( 178.5955509887552353, 285.1658660899858546, 13.49892897318265561 ) ) ;
#66297 = DIRECTION ( 'NONE',  ( -0.000000000000000000, -0.000000000000000000, -1.000000000000000000 ) ) ;
#66298 = DIRECTION ( 'NONE',  ( -1.000000000000000000, 0.000000000000000000, 0.000000000000000000 ) ) ;
#66299 = CARTESIAN_POINT ( 'NONE',  ( 29.13110022456613635, 42.86445400964587549, 10.00000000000000000 ) ) ;
#66300 = VECTOR ( 'NONE', #49984, 1000.000000000000227 ) ;
#66301 = CARTESIAN_POINT ( 'NONE',  ( 80.54656262287409163, 52.70628843406199593, 15.42795475958373252 ) ) ;
#66302 = CARTESIAN_POINT ( 'NONE',  ( 16.16012747849099540, 9.734156793818206310, 1.333680081654574804E-15 ) ) ;
#66303 = CARTESIAN_POINT ( 'NONE',  ( 191.9281725887558991, 273.9750938816710004, -16.55071879691933390 ) ) ;
#66304 = CARTESIAN_POINT ( 'NONE',  ( -6.813555604197667037, 155.3262482093457777, -6.972266317189433020E-16 ) ) ;
#66305 = CARTESIAN_POINT ( 'NONE',  ( 162.7007457333762090, 248.8410372908842021, -10.94671474643812914 ) ) ;
#66306 = VECTOR ( 'NONE', #60095, 1000.000000000000114 ) ;
#66307 = SURFACE_STYLE_USAGE ( .BOTH. , #2652 ) ;
#66309 = LINE ( 'NONE', #29800, #41495 ) ;
#66308 = DIRECTION ( 'NONE',  ( -0.1860369090531061032, -0.9825427565607341984, 0.000000000000000000 ) ) ;
#66310 = CARTESIAN_POINT ( 'NONE',  ( 175.8027662909930484, 284.8719843250962072, 14.11304877541382119 ) ) ;
#66311 = VECTOR ( 'NONE', #89185, 1000.000000000000114 ) ;
#66312 = CARTESIAN_POINT ( 'NONE',  ( 37.57390229391633341, 33.64441083166263979, -10.00000000000000533 ) ) ;
#66313 = LINE ( 'NONE', #21705, #4530 ) ;
#66314 = FACE_OUTER_BOUND ( 'NONE', #42727, .T. ) ;
#66315 = CARTESIAN_POINT ( 'NONE',  ( 86.09177458334599464, 43.55638514111210213, -4.160762740161195516 ) ) ;
#66316 = CARTESIAN_POINT ( 'NONE',  ( 5.696048431029936410, 186.3464784336661637, 1.353441290958777327E-15 ) ) ;
#66317 = CARTESIAN_POINT ( 'NONE',  ( 80.99988074727858134, 44.69027685233859870, 10.63760621275858576 ) ) ;
#66318 = ORIENTED_EDGE ( 'NONE', *, *, #52325, .F. ) ;
#66319 = B_SPLINE_CURVE_WITH_KNOTS ( 'NONE', 3,
 ( #69434, #46627, #10650, #17752, #25333, #2047, #34438, #81087, #10149, #18750, #79079, #49147, #41525, #57720, #94771, #11653, #2557, #33440, #9661, #40521, #80081, #42514, #73451, #55704, #18252, #72468, #17226, #11164, #19269, #3557, #3074 ),
 .UNSPECIFIED., .F., .F.,
 ( 4, 3, 3, 3, 3, 3, 3, 3, 3, 3, 4 ),
 ( 0.000000000000000000, 0.1333490885032338480, 0.3007194338854361493, 0.4699862290245140906, 0.5844252810809331677, 0.6686540514502653521, 0.7354980260655413771, 0.8028463152565569194, 0.8633854507757173780, 0.9437142632667304687, 1.000000000000000000 ),
 .UNSPECIFIED. ) ;
#66320 = EDGE_CURVE ( 'NONE', #19447, #26502, #58267, .T. ) ;
#66321 = CARTESIAN_POINT ( 'NONE',  ( 87.13698410836482822, 46.33067510313777859, 8.599260793297284877 ) ) ;
#66322 = CARTESIAN_POINT ( 'NONE',  ( 32.07315653955450330, 47.77038272570916888, -10.00000000000000000 ) ) ;
#66323 = CARTESIAN_POINT ( 'NONE',  ( 71.89024115076192345, 72.14005084039141025, -1.691652508062526650 ) ) ;
#66324 = CARTESIAN_POINT ( 'NONE',  ( 39.63359248971512727, 199.8149278399161233, 9.188101187500093303 ) ) ;
#66325 = CARTESIAN_POINT ( 'NONE',  ( 86.92045001522136261, 45.99340221249899940, 8.966174604352282529 ) ) ;
#66326 = CARTESIAN_POINT ( 'NONE',  ( 170.5993847053230468, 287.8722104901659691, 7.679145147933459370 ) ) ;
#66327 = CARTESIAN_POINT ( 'NONE',  ( 190.5541309856500050, 300.5975588711562523, -4.167177996129430184 ) ) ;
#66328 = CARTESIAN_POINT ( 'NONE',  ( 37.86538501507695287, 37.56454794089044213, 10.00000000000000355 ) ) ;
#66329 = CARTESIAN_POINT ( 'NONE',  ( 170.8463542321686077, 287.4393069310528972, -8.645854640182026429 ) ) ;
#66330 = CARTESIAN_POINT ( 'NONE',  ( 191.0862225170008628, 299.6759493045793192, -9.402218231374108726 ) ) ;
#66331 = CARTESIAN_POINT ( 'NONE',  ( 180.0904441998713992, 279.0932581032296298, -17.39800262650857832 ) ) ;
#66332 = CARTESIAN_POINT ( 'NONE',  ( 68.22205435738101187, 65.90345407221148832, 10.80313017757570471 ) ) ;
#66333 = CARTESIAN_POINT ( 'NONE',  ( 87.05121076158607707, 45.95104493586815408, -8.147482009912135226 ) ) ;
#66334 = CARTESIAN_POINT ( 'NONE',  ( 183.8210692855788864, 257.9504670327482927, 6.873620218444065344 ) ) ;
#66335 = CARTESIAN_POINT ( 'NONE',  ( 94.56323149399085537, 218.7365022471902023, 10.00000000000009592 ) ) ;
#66336 = CARTESIAN_POINT ( 'NONE',  ( 75.33387806111561247, 65.67578613345442307, -13.61108734441214807 ) ) ;
#66337 = CARTESIAN_POINT ( 'NONE',  ( 161.5955478064990416, 267.7463613786376868, -17.24529233156741981 ) ) ;
#66338 = ORIENTED_EDGE ( 'NONE', *, *, #69723, .T. ) ;
#66339 = CARTESIAN_POINT ( 'NONE',  ( 66.64328041388984047, 197.0327760586659736, 1.948934522072303157E-15 ) ) ;
#66340 = ORIENTED_EDGE ( 'NONE', *, *, #55327, .F. ) ;
#66341 = CARTESIAN_POINT ( 'NONE',  ( 162.5527276353931825, 263.2273425849169257, 17.54043303782436425 ) ) ;
#66342 = CARTESIAN_POINT ( 'NONE',  ( 186.8003541658358984, 299.2222177555264011, -0.6103433986344138917 ) ) ;
#66343 = CARTESIAN_POINT ( 'NONE',  ( 67.67908650673803095, 66.83328552386096533, -8.531651213308034443 ) ) ;
#66344 = ORIENTED_EDGE ( 'NONE', *, *, #30523, .T. ) ;
#66345 = CARTESIAN_POINT ( 'NONE',  ( -36.52772323645827868, 26.41323893245353105, -10.00000000000000000 ) ) ;
#66346 = CARTESIAN_POINT ( 'NONE',  ( 164.3774690880109119, 245.9368672504194819, -2.805681983503304000 ) ) ;
#66347 = CARTESIAN_POINT ( 'NONE',  ( -19.65312891409030271, 93.06504152958497400, 177.5919119679930134 ) ) ;
#66348 = CARTESIAN_POINT ( 'NONE',  ( 31.37760429443829224, 33.51421378149921537, -9.188101187500004485 ) ) ;
#66349 = CARTESIAN_POINT ( 'NONE',  ( 189.0372613391137975, 265.5483559667888471, 10.71995464741518767 ) ) ;
#66350 = CARTESIAN_POINT ( 'NONE',  ( 86.50792306782743424, 47.43283652443698628, -10.36525212966502174 ) ) ;
#66351 = CARTESIAN_POINT ( 'NONE',  ( 34.61729389309891758, 20.39040679176985549, -6.890680421881970419E-14 ) ) ;
#66352 = ORIENTED_EDGE ( 'NONE', *, *, #19842, .F. ) ;
#66353 = B_SPLINE_CURVE_WITH_KNOTS ( 'NONE', 3,
 ( #67114, #60002, #12442, #50420, #21048, #82870, #74752, #20044, #13443, #50915 ),
 .UNSPECIFIED., .F., .F.,
 ( 4, 2, 2, 2, 4 ),
 ( 1.148183921853115802E-16, 0.0004091266720098301062, 0.0008182533440195453953, 0.001227380016029260956, 0.001636506688038975432 ),
 .UNSPECIFIED. ) ;
#66354 = CARTESIAN_POINT ( 'NONE',  ( 13.45569633750675465, 25.95586893147754282, 7.433330006724141015 ) ) ;
#66355 = CARTESIAN_POINT ( 'NONE',  ( 76.31365291358306990, 61.99157619597451685, 15.38880639136091233 ) ) ;
#66356 = DIRECTION ( 'NONE',  ( -0.4999999999999997780, -0.8660254037844387076, 0.000000000000000000 ) ) ;
#66357 = DIRECTION ( 'NONE',  ( 1.000000000000000000, 0.000000000000000000, 0.000000000000000000 ) ) ;
#66358 = ORIENTED_EDGE ( 'NONE', *, *, #85698, .T. ) ;
#66359 = CARTESIAN_POINT ( 'NONE',  ( 77.21042888011766081, 57.50458007534377458, 16.59863515784280352 ) ) ;
#66360 = CARTESIAN_POINT ( 'NONE',  ( 190.8623743139412454, 300.0636657654615647, 8.577953960666059530 ) ) ;
#66361 = FACE_OUTER_BOUND ( 'NONE', #53267, .T. ) ;
#66362 = ORIENTED_EDGE ( 'NONE', *, *, #45370, .T. ) ;
#66363 = AXIS2_PLACEMENT_3D ( 'NONE', #59413, #5735, #44713 ) ;
#66364 = ORIENTED_EDGE ( 'NONE', *, *, #93065, .T. ) ;
#66366 = CARTESIAN_POINT ( 'NONE',  ( 85.49318370521093868, 48.99722645306705715, -12.73116331006621493 ) ) ;
#66365 = CARTESIAN_POINT ( 'NONE',  ( 207.1572261440131797, 271.8401544939704877, -5.633070628900782140 ) ) ;
#66367 = CARTESIAN_POINT ( 'NONE',  ( 196.4783028304046013, 290.3365922432724346, -16.37291435488387492 ) ) ;
#66368 = ORIENTED_EDGE ( 'NONE', *, *, #58382, .T. ) ;
#66369 = CARTESIAN_POINT ( 'NONE',  ( 66.52541744028246740, 68.80911811048743232, -2.215339755367858210 ) ) ;
#66370 = CARTESIAN_POINT ( 'NONE',  ( 198.1300353965528984, 287.4757075181870505, 18.48278456664528946 ) ) ;
#66371 = DIRECTION ( 'NONE',  ( -1.000000000000000000, 0.000000000000000000, 0.000000000000000000 ) ) ;
#66372 = DIRECTION ( 'NONE',  ( 0.5000000000000013323, -0.8660254037844378194, 0.000000000000000000 ) ) ;
#66373 = CARTESIAN_POINT ( 'NONE',  ( 117.3868696429430258, 229.3923013555409796, 4.594050593750050204 ) ) ;
#66374 = CARTESIAN_POINT ( 'NONE',  ( 117.4407359106297406, 238.6115022471902307, 10.00000000000009592 ) ) ;
#66375 = CARTESIAN_POINT ( 'NONE',  ( 206.3023480738090996, 271.3208467458289874, 7.632938913807082670 ) ) ;
#66376 = CARTESIAN_POINT ( 'NONE',  ( 117.7780771369770463, 227.2592609112379876, 2.679491924311254714 ) ) ;
#66377 = EDGE_CURVE ( 'NONE', #81256, #24137, #73231, .T. ) ;
#66378 = VERTEX_POINT ( 'NONE', #21512 ) ;
#66379 = CARTESIAN_POINT ( 'NONE',  ( 164.4414259850711915, 245.8260906552167171, -6.983224448873608381 ) ) ;
#66380 = ORIENTED_EDGE ( 'NONE', *, *, #44800, .T. ) ;
#66381 = ORIENTED_EDGE ( 'NONE', *, *, #89652, .T. ) ;
#66382 = CARTESIAN_POINT ( 'NONE',  ( 198.6562788533279615, 286.5642271139020636, 17.47134757795404525 ) ) ;
#66383 = CARTESIAN_POINT ( 'NONE',  ( -30.18034446749236821, 25.12100238203590763, -10.00000000000000000 ) ) ;
#66384 = CARTESIAN_POINT ( 'NONE',  ( 66.56148311469628709, 218.4244531367911293, -4.594050593750046652 ) ) ;
#66385 = VERTEX_POINT ( 'NONE', #5805 ) ;
#66386 = CYLINDRICAL_SURFACE ( 'NONE', #46551, 10.00000000000010658 ) ;
#66387 = CARTESIAN_POINT ( 'NONE',  ( 81.63113279203287220, 55.88178493786749357, 16.01941705845313280 ) ) ;
#66388 = CARTESIAN_POINT ( 'NONE',  ( 198.0542955016221924, 287.6068928643675804, 18.26164672886581997 ) ) ;
#66389 = CARTESIAN_POINT ( 'NONE',  ( -18.11259370987442452, 171.8967562850347690, 9.296355089585912665E-16 ) ) ;
#66390 = ORIENTED_EDGE ( 'NONE', *, *, #74241, .F. ) ;
#66391 = CARTESIAN_POINT ( 'NONE',  ( 112.9278751967105450, 247.5530062829863311, -4.648177544792955347E-16 ) ) ;
#66392 = DIRECTION ( 'NONE',  ( -0.8660254037844387076, -0.4999999999999998890, -0.000000000000000000 ) ) ;
#66393 = ORIENTED_EDGE ( 'NONE', *, *, #53103, .F. ) ;
#66394 = CYLINDRICAL_SURFACE ( 'NONE', #86900, 16.60714546451156792 ) ;
#66395 = FACE_OUTER_BOUND ( 'NONE', #19197, .T. ) ;
#66396 = EDGE_CURVE ( 'NONE', #48842, #19318, #23270, .T. ) ;
#66397 = CARTESIAN_POINT ( 'NONE',  ( -0.4668637173180778532, 25.74574839753308808, 177.5919119679930134 ) ) ;
#66398 = CARTESIAN_POINT ( 'NONE',  ( 206.4767272400630134, 270.6244814104205716, 2.441409265890493785 ) ) ;
#66399 = CARTESIAN_POINT ( 'NONE',  ( 180.1168005803277481, 295.2192856762299016, -2.191971455912026467 ) ) ;
#66400 = FACE_OUTER_BOUND ( 'NONE', #82188, .T. ) ;
#66401 = CARTESIAN_POINT ( 'NONE',  ( 206.5479446040613141, 272.8954610772809133, 10.74757481123993230 ) ) ;
#66402 = CARTESIAN_POINT ( 'NONE',  ( 153.2593913506692616, 267.1939427739956727, -16.45456985337825984 ) ) ;
#66403 = VERTEX_POINT ( 'NONE', #35709 ) ;
#66404 = FACE_OUTER_BOUND ( 'NONE', #94930, .T. ) ;
#66405 = CARTESIAN_POINT ( 'NONE',  ( 127.1025053677084742, 238.0643266524160424, -9.188101187500093303 ) ) ;
#66406 = ORIENTED_EDGE ( 'NONE', *, *, #91951, .F. ) ;
#66407 = CARTESIAN_POINT ( 'NONE',  ( 83.13178773832562740, 44.19191255805648666, -8.679323957351682495 ) ) ;
#66408 = B_SPLINE_CURVE_WITH_KNOTS ( 'NONE', 3,
 ( #60866, #46682, #93836, #62878 ),
 .UNSPECIFIED., .F., .F.,
 ( 4, 4 ),
 ( 0.002563918088655046078, 0.005315235947567602259 ),
 .UNSPECIFIED. ) ;
#66409 = CARTESIAN_POINT ( 'NONE',  ( 184.0019883067494675, 259.5089881467251303, 6.346366111470802096 ) ) ;
#66410 = CARTESIAN_POINT ( 'NONE',  ( 205.3095662483215733, 273.2405008374320801, -10.93512342935413884 ) ) ;
#66411 = ADVANCED_FACE ( 'NONE', ( #91437 ), #6305, .F. ) ;
#66412 = CARTESIAN_POINT ( 'NONE',  ( 79.24143198459856308, 59.88451820689867588, -16.14143938394746414 ) ) ;
#66413 = CARTESIAN_POINT ( 'NONE',  ( 74.97830149814869571, 62.15334231524035147, 15.06231098758508402 ) ) ;
#66414 = CARTESIAN_POINT ( 'NONE',  ( -22.42236680055709641, 157.8615022471902591, 0.000000000000000000 ) ) ;
#66415 = ORIENTED_EDGE ( 'NONE', *, *, #50360, .T. ) ;
#66416 = CARTESIAN_POINT ( 'NONE',  ( 77.44539015164885143, 60.39115425616281385, 15.91752098216395162 ) ) ;
#66417 = CARTESIAN_POINT ( 'NONE',  ( 182.3798495899531247, 275.9165375621991529, -16.43942715639238017 ) ) ;
#66418 = LINE ( 'NONE', #35515, #93228 ) ;
#66419 = DIRECTION ( 'NONE',  ( -0.000000000000000000, 0.000000000000000000, -1.000000000000000000 ) ) ;
#66420 = LINE ( 'NONE', #37006, #7834 ) ;
#66421 = FACE_OUTER_BOUND ( 'NONE', #91542, .T. ) ;
#66422 = CARTESIAN_POINT ( 'NONE',  ( 69.53218774831623250, 70.45193905447369787, 3.001416003324469450 ) ) ;
#66423 = CARTESIAN_POINT ( 'NONE',  ( 204.6075833744878878, 276.2562653119390461, -13.34672481898815910 ) ) ;
#66424 = CARTESIAN_POINT ( 'NONE',  ( 170.8556692713231655, 250.1274861400973464, 4.270813221915627622 ) ) ;
#66425 = EDGE_CURVE ( 'NONE', #34863, #83781, #90463, .T. ) ;
#66426 = ADVANCED_FACE ( 'NONE', ( #21032, #99517 ), #51404, .T. ) ;
#66427 = CARTESIAN_POINT ( 'NONE',  ( 20.05933935144479463, 19.78052372038640527, -10.00000000000000355 ) ) ;
#66428 = CARTESIAN_POINT ( 'NONE',  ( 149.5593209768671841, 271.6026526530012575, 11.55487339793564949 ) ) ;
#66429 = DIRECTION ( 'NONE',  ( 0.000000000000000000, 0.000000000000000000, 1.000000000000000000 ) ) ;
#66430 = CARTESIAN_POINT ( 'NONE',  ( 172.1473514959812690, 287.0828204173988638, -8.113061055153803380 ) ) ;
#66431 = CARTESIAN_POINT ( 'NONE',  ( 159.2303255284352304, 254.8519814094557603, 16.39103317446447150 ) ) ;
#66432 = AXIS2_PLACEMENT_3D ( 'NONE', #54418, #8843, #94483 ) ;
#66433 = CARTESIAN_POINT ( 'NONE',  ( 188.7055302822745944, 298.7144859465759623, -6.936194914715221316 ) ) ;
#66434 = ADVANCED_FACE ( 'NONE', ( #44785 ), #99020, .T. ) ;
#66435 = CARTESIAN_POINT ( 'NONE',  ( 139.3620039403755015, 241.2677522451417929, -5.000000000000041744 ) ) ;
#66436 = CARTESIAN_POINT ( 'NONE',  ( 47.57035326562169075, 72.63383583914733777, 10.00000000000000000 ) ) ;
#66437 = ORIENTED_EDGE ( 'NONE', *, *, #61527, .T. ) ;
#66438 = ADVANCED_FACE ( 'NONE', ( #52893 ), #83845, .F. ) ;
#66439 = FACE_OUTER_BOUND ( 'NONE', #2717, .T. ) ;
#66440 = CARTESIAN_POINT ( 'NONE',  ( 151.3898985249405200, 268.4319993325432847, -14.65018536945715510 ) ) ;
#66441 = CARTESIAN_POINT ( 'NONE',  ( -3.911334118262431936, 177.7369531367911293, -4.594050593750048428 ) ) ;
#66442 = CARTESIAN_POINT ( 'NONE',  ( 62.15060008387555257, 200.5643266524159856, -9.188101187500093303 ) ) ;
#66443 = CARTESIAN_POINT ( 'NONE',  ( 176.1391974210675357, 257.4512529022192666, -10.49415748218208932 ) ) ;
#66444 = CARTESIAN_POINT ( 'NONE',  ( 85.08976737157280468, 48.95938582862681443, 12.42920128896121668 ) ) ;
#66445 = CARTESIAN_POINT ( 'NONE',  ( 204.6235849755581455, 276.2285497258825444, -13.59355699282649432 ) ) ;
#66446 = CARTESIAN_POINT ( 'NONE',  ( 72.30409372968703963, 72.02947187496847903, -3.500239827782243296 ) ) ;
#66447 = CARTESIAN_POINT ( 'NONE',  ( 73.74733062278515661, 55.38161606902450984, -16.59075967854369438 ) ) ;
#66448 = EDGE_CURVE ( 'NONE', #26733, #40804, #93278, .T. ) ;
#66449 = CARTESIAN_POINT ( 'NONE',  ( 171.0430343787876382, 258.3364600833120903, 13.98411771018495386 ) ) ;
#66450 = EDGE_CURVE ( 'NONE', #75103, #17277, #8302, .T. ) ;
#66451 = CARTESIAN_POINT ( 'NONE',  ( 179.3339753375761347, 254.6678550771822529, -4.099179283769126769 ) ) ;
#66452 = CARTESIAN_POINT ( 'NONE',  ( 150.3470217762446737, 270.2383148473169854, 15.04338213197856078 ) ) ;
#66453 =( BOUNDED_CURVE ( )  B_SPLINE_CURVE ( 2, ( #14244, #45130, #99356, #75061, #22336, #53235, #14735, #45618, #9658 ),
 .UNSPECIFIED., .F., .T. ) 
 B_SPLINE_CURVE_WITH_KNOTS ( ( 3, 2, 2, 2, 3 ),
 ( 0.8750000000000000000, 0.8763440860215053752, 0.8790322580645161255, 0.8817204301075268758, 0.8830645161290322509 ),
 .UNSPECIFIED. ) 
 CURVE ( )  GEOMETRIC_REPRESENTATION_ITEM ( )  RATIONAL_B_SPLINE_CURVE ( ( 0.9330127018922194093, 0.9330127018922194093, 1.000000000000000000, 0.8660254037844387076, 1.000000000000000000, 0.8660254037844387076, 1.000000000000000000, 0.9330127018922194093, 0.9330127018922194093 ) ) 
 REPRESENTATION_ITEM ( '' )  );
#66454 = CARTESIAN_POINT ( 'NONE',  ( 43.46773267070898328, 189.2365022471902023, -10.00000000000009059 ) ) ;
#66455 = CARTESIAN_POINT ( 'NONE',  ( 184.3432414080211288, 293.3642184156927897, 9.509896531551312648 ) ) ;
#66456 = CARTESIAN_POINT ( 'NONE',  ( 189.8123550829396891, 301.8823524224806647, -0.5679054518196169354 ) ) ;
#66457 = CARTESIAN_POINT ( 'NONE',  ( -0.5279885150232012103, 164.3768266524160140, -9.188101187500091527 ) ) ;
#66458 = CARTESIAN_POINT ( 'NONE',  ( 72.73269248836918166, 71.16345857084105830, -7.307540741686431751 ) ) ;
#66459 = CARTESIAN_POINT ( 'NONE',  ( 79.31104985338477320, 59.89077999431003008, 16.15264230762560516 ) ) ;
#66460 = CARTESIAN_POINT ( 'NONE',  ( 34.51455378690028652, 28.43085787977765477, -9.188101187500008038 ) ) ;
#66461 = CARTESIAN_POINT ( 'NONE',  ( 164.9171241593586217, 245.0021572482830550, 1.622680932994367220 ) ) ;
#66462 = CARTESIAN_POINT ( 'NONE',  ( 164.3274319858398087, 246.0235340536434592, -1.770631424362269168 ) ) ;
#66463 = FACE_OUTER_BOUND ( 'NONE', #12077, .T. ) ;
#66464 = CARTESIAN_POINT ( 'NONE',  ( 153.3038478579095170, 266.0895745828713075, -16.28333902283113588 ) ) ;
#66465 = CARTESIAN_POINT ( 'NONE',  ( 176.5163929983920355, 260.4762631834057061, -13.32580715195663146 ) ) ;
#66466 = DIRECTION ( 'NONE',  ( 0.000000000000000000, 0.000000000000000000, 1.000000000000000000 ) ) ;
#66467 = CARTESIAN_POINT ( 'NONE',  ( 15.78914702631840328, 24.51421378149918695, -9.188101187500004485 ) ) ;
#66468 = CARTESIAN_POINT ( 'NONE',  ( 165.6535135722015184, 285.4045712548459051, 0.4591178296265144287 ) ) ;
#66469 = CARTESIAN_POINT ( 'NONE',  ( 82.48148221723897677, 54.22512503293472719, 15.59203162474583415 ) ) ;
#66470 = DIRECTION ( 'NONE',  ( -0.4829524219151362097, 0.8756465943326133816, 0.000000000000000000 ) ) ;
#66471 = CARTESIAN_POINT ( 'NONE',  ( -27.42236680055714260, 166.5217562850347406, 1.224646799147364892E-15 ) ) ;
#66472 = ORIENTED_EDGE ( 'NONE', *, *, #24734, .F. ) ;
#66473 = CARTESIAN_POINT ( 'NONE',  ( 156.8792359301817214, 276.4852139478325626, 11.15229350607063274 ) ) ;
#66474 = PLANE ( 'NONE',  #48911 ) ;
#66475 = ORIENTED_EDGE ( 'NONE', *, *, #355, .F. ) ;
#66476 = CARTESIAN_POINT ( 'NONE',  ( 192.8325075361489382, 296.6512949269187516, 11.74553025762331515 ) ) ;
#66477 = CARTESIAN_POINT ( 'NONE',  ( 72.76825883208245216, 219.4865022471902876, 10.00000000000009415 ) ) ;
#66478 = CARTESIAN_POINT ( 'NONE',  ( 66.24598407424289803, 68.55598904622115697, 4.800278518307799835 ) ) ;
#66479 = CARTESIAN_POINT ( 'NONE',  ( 154.9067123643522734, 262.3406990819208886, -18.18534662427576265 ) ) ;
#66480 = ORIENTED_EDGE ( 'NONE', *, *, #51836, .F. ) ;
#66481 = VERTEX_POINT ( 'NONE', #39167 ) ;
#66483 = DIRECTION ( 'NONE',  ( -0.8660254037844387076, -0.4999999999999998890, -0.000000000000000000 ) ) ;
#66482 = CARTESIAN_POINT ( 'NONE',  ( 164.2858849336956268, 246.6305630168277503, -4.528670904437447575 ) ) ;
#66484 = CARTESIAN_POINT ( 'NONE',  ( 192.4454213697443095, 297.3217478340386606, 12.58566886711101596 ) ) ;
#66485 = EDGE_LOOP ( 'NONE', ( #18859, #42037, #88223, #1595 ) ) ;
#66486 = CARTESIAN_POINT ( 'NONE',  ( 88.44819812734249354, 44.06706281553302773, -2.545729839345954204 ) ) ;
#66487 = CARTESIAN_POINT ( 'NONE',  ( 80.24292271875241056, 58.10242382007938744, 16.26432532982812518 ) ) ;
#66488 = CARTESIAN_POINT ( 'NONE',  ( -19.65312891409030271, 93.06504152958497400, 59.99999999999999289 ) ) ;
#66489 = ORIENTED_EDGE ( 'NONE', *, *, #82884, .T. ) ;
#66490 = CARTESIAN_POINT ( 'NONE',  ( 78.25048285508148638, 61.03959493798094371, -15.91191902859591778 ) ) ;
#66491 = CARTESIAN_POINT ( 'NONE',  ( 85.37179553587198200, 208.5494855054051584, -2.679491924311248496 ) ) ;
#66492 = CARTESIAN_POINT ( 'NONE',  ( 149.7109319212262051, 271.3400547943878109, -12.38605961032017433 ) ) ;
#66493 = CARTESIAN_POINT ( 'NONE',  ( 80.91343449481020400, 43.02608183091172123, 9.608889258680049394 ) ) ;
#66494 = EDGE_CURVE ( 'NONE', #12428, #20062, #198, .T. ) ;
#66495 = ORIENTED_EDGE ( 'NONE', *, *, #36089, .F. ) ;
#66496 = CARTESIAN_POINT ( 'NONE',  ( 159.9381800915330416, 254.2419649056765820, -15.29477132317076915 ) ) ;
#66497 = CARTESIAN_POINT ( 'NONE',  ( 206.5280879940269756, 272.9298537347264642, 11.21709153681466731 ) ) ;
#66498 = CARTESIAN_POINT ( 'NONE',  ( 73.72813317336040484, 59.85036616854785763, 15.47704302871372839 ) ) ;
#66499 = VERTEX_POINT ( 'NONE', #62994 ) ;
#66500 = CARTESIAN_POINT ( 'NONE',  ( 149.0323968763055689, 272.5153119669064949, 11.64231532207353403 ) ) ;
#66501 = CARTESIAN_POINT ( 'NONE',  ( 171.8887382467565317, 263.4056550183183276, -15.47577216865978400 ) ) ;
#66502 = ADVANCED_FACE ( 'NONE', ( #93435 ), #31577, .F. ) ;
#66503 = ORIENTED_EDGE ( 'NONE', *, *, #20226, .F. ) ;
#66504 = PLANE ( 'NONE',  #27253 ) ;
#66505 = VERTEX_POINT ( 'NONE', #54367 ) ;
#66506 = CARTESIAN_POINT ( 'NONE',  ( -13.11024591527734628, 27.99999999999999645, 32.50000000000000000 ) ) ;
#66507 = ORIENTED_EDGE ( 'NONE', *, *, #97588, .T. ) ;
#66508 = CARTESIAN_POINT ( 'NONE',  ( 156.6663764169331898, 266.5808990040749222, -16.21966367912098050 ) ) ;
#66509 = CARTESIAN_POINT ( 'NONE',  ( 87.62257652462700719, 43.83610729166736064, 1.029400949057958314 ) ) ;
#66510 = DIRECTION ( 'NONE',  ( -0.000000000000000000, 0.000000000000000000, -1.000000000000000000 ) ) ;
#66511 = DIRECTION ( 'NONE',  ( 0.000000000000000000, 1.000000000000000000, 0.000000000000000000 ) ) ;
#66512 = CARTESIAN_POINT ( 'NONE',  ( 132.6918519524023736, 258.9637435831425023, 2.679491924311251605 ) ) ;
#66513 = CARTESIAN_POINT ( 'NONE',  ( 157.2021838295288489, 258.7528274272191311, -16.83974058492033166 ) ) ;
#66514 = EDGE_CURVE ( 'NONE', #57272, #74992, #26818, .T. ) ;
#66515 = CARTESIAN_POINT ( 'NONE',  ( 178.4260950018880294, 291.5365620954837027, 6.089707329432893168 ) ) ;
#66516 = CARTESIAN_POINT ( 'NONE',  ( 158.5494479970505779, 256.0312958875455820, -16.13101935219385297 ) ) ;
#66517 = VERTEX_POINT ( 'NONE', #30601 ) ;
#66518 = CARTESIAN_POINT ( 'NONE',  ( 79.83679441914436836, 55.88931611243568653, -16.12940057729960230 ) ) ;
#66519 = CARTESIAN_POINT ( 'NONE',  ( 206.5508451493652444, 272.8904371854448527, 11.05407534521577695 ) ) ;
#66520 = CARTESIAN_POINT ( 'NONE',  ( 205.8030308266901898, 274.1856895869457844, 10.55961490432110317 ) ) ;
#66522 = ORIENTED_EDGE ( 'NONE', *, *, #57294, .T. ) ;
#66521 = CARTESIAN_POINT ( 'NONE',  ( -19.65312891409030271, 93.06504152958497400, 10.00000000000000888 ) ) ;
#66523 = CARTESIAN_POINT ( 'NONE',  ( 192.6316891401646387, 296.9991225918579403, 12.51992576083217301 ) ) ;
#66524 = LINE ( 'NONE', #49453, #44666 ) ;
#66525 = ORIENTED_EDGE ( 'NONE', *, *, #15983, .T. ) ;
#66526 = CARTESIAN_POINT ( 'NONE',  ( 147.2752695334602322, 275.5587458000830452, -2.690728879113632566 ) ) ;
#66527 = CARTESIAN_POINT ( 'NONE',  ( 82.64744444949904789, 51.85429353291556254, -14.77163707229560963 ) ) ;
#66528 = FACE_OUTER_BOUND ( 'NONE', #42317, .T. ) ;
#66529 = ADVANCED_FACE ( 'NONE', ( #39664 ), #78209, .F. ) ;
#66530 = CARTESIAN_POINT ( 'NONE',  ( 10.46840290624634306, 27.81751292744054993, -6.180339887498951690 ) ) ;
#66531 = EDGE_CURVE ( 'NONE', #74702, #1108, #318, .T. ) ;
#66532 = CARTESIAN_POINT ( 'NONE',  ( 159.8699404666255930, 253.7441358392297843, -15.37844326134346673 ) ) ;
#66533 = CARTESIAN_POINT ( 'NONE',  ( 190.6082082143898617, 300.5038943634461361, -0.5472910358126498176 ) ) ;
#66534 = VERTEX_POINT ( 'NONE', #70588 ) ;
#66535 = CARTESIAN_POINT ( 'NONE',  ( 163.3723087697842971, 247.6778559913402091, -10.08585062664141319 ) ) ;
#66536 = CARTESIAN_POINT ( 'NONE',  ( 190.9103068040902258, 266.1559691903721045, 12.32197154148064655 ) ) ;
#66537 = CARTESIAN_POINT ( 'NONE',  ( 89.82826426823238819, 45.13720097505219542, 0.2499999999999960032 ) ) ;
#66538 = CARTESIAN_POINT ( 'NONE',  ( -22.42236680055709641, 157.8615022471902591, 0.000000000000000000 ) ) ;
#66539 = CARTESIAN_POINT ( 'NONE',  ( 23.67544375150414737, 191.1427522451419634, -10.00000000000009415 ) ) ;
#66540 = CARTESIAN_POINT ( 'NONE',  ( 101.5001087246834857, 241.6589784336661637, -6.496448406907676862E-16 ) ) ;
#66541 = CARTESIAN_POINT ( 'NONE',  ( 181.2763874864546949, 294.3971386994905401, -2.647043256306043979 ) ) ;
#66542 = CARTESIAN_POINT ( 'NONE',  ( 162.8931802014337791, 249.0911889412991229, -10.32038157250286048 ) ) ;
#66543 = CARTESIAN_POINT ( 'NONE',  ( 157.0935036675524827, 258.5530654392286465, 17.32636058289560665 ) ) ;
#66544 = CARTESIAN_POINT ( 'NONE',  ( 93.96857342517718337, 15.00000000000000000, -9.212605237762131694 ) ) ;
#66545 = CARTESIAN_POINT ( 'NONE',  ( 40.66251830035667325, 182.0327760586659451, 1.948934522072303157E-15 ) ) ;
#66546 = CARTESIAN_POINT ( 'NONE',  ( 43.27754793094329244, 25.39040679176986970, -6.890680421881970419E-14 ) ) ;
#66547 = EDGE_LOOP ( 'NONE', ( #29500, #95966, #75124, #42050 ) ) ;
#66548 = CARTESIAN_POINT ( 'NONE',  ( 191.3401838285315080, 298.8338641635404542, 7.654257991345104095 ) ) ;
#66549 = CARTESIAN_POINT ( 'NONE',  ( 74.46971312594514814, 68.19886894342141659, -11.52194869617921569 ) ) ;
#66550 = EDGE_CURVE ( 'NONE', #3978, #55003, #50768, .T. ) ;
#66551 = CARTESIAN_POINT ( 'NONE',  ( 119.5854454918513170, 251.3967562850347122, -4.648177544792955347E-16 ) ) ;
#66552 = CARTESIAN_POINT ( 'NONE',  ( 190.1752790837055045, 301.2537496138681945, -5.177773110520776711 ) ) ;
#66553 = CARTESIAN_POINT ( 'NONE',  ( 81.78771499908393139, 41.70666495146470254, -5.605238045589925555 ) ) ;
#66554 = CARTESIAN_POINT ( 'NONE',  ( 7.283862947486896999, 19.90829794293878408, 10.00000000000000355 ) ) ;
#66555 = CARTESIAN_POINT ( 'NONE',  ( 68.53065452504849020, 198.8262482093457777, 3.021315404115420679E-15 ) ) ;
#66556 = CARTESIAN_POINT ( 'NONE',  ( 102.9889369814290347, 230.2677522451418497, 10.00000000000009592 ) ) ;
#66557 = EDGE_CURVE ( 'NONE', #91721, #44730, #48303, .T. ) ;
#66558 = CARTESIAN_POINT ( 'NONE',  ( 48.37494963522306080, 207.9244531367911293, -4.594050593750046652 ) ) ;
#66559 = CARTESIAN_POINT ( 'NONE',  ( 90.43156862655462191, 233.0177522451419350, 5.000000000000046185 ) ) ;
#66560 = VERTEX_POINT ( 'NONE', #86859 ) ;
#66561 = CARTESIAN_POINT ( 'NONE',  ( 194.7965532219227498, 266.2737535417827530, -7.589310887033829722 ) ) ;
#66562 = EDGE_CURVE ( 'NONE', #55017, #48579, #3227, .T. ) ;
#66563 = CARTESIAN_POINT ( 'NONE',  ( 178.8342571948529951, 258.9790443764770203, -10.10065873795960023 ) ) ;
#66564 = CARTESIAN_POINT ( 'NONE',  ( 207.6050568035884680, 271.0644890383991310, -1.456818755242089702 ) ) ;
#66565 = CARTESIAN_POINT ( 'NONE',  ( 10.51348828746337638, 183.0024278399160949, -9.188101187500093303 ) ) ;
#66566 = EDGE_CURVE ( 'NONE', #33367, #8285, #99368, .T. ) ;
#66567 = CARTESIAN_POINT ( 'NONE',  ( 199.2205425252482200, 285.5868937652708155, -18.05012564782189344 ) ) ;
#66568 = CARTESIAN_POINT ( 'NONE',  ( -19.73169950930824967, 92.94697205762078340, 59.99999999999999289 ) ) ;
#66569 = CARTESIAN_POINT ( 'NONE',  ( 66.33611483106668061, 68.05323429769379118, -4.754337940927038098 ) ) ;
#66570 = CARTESIAN_POINT ( 'NONE',  ( 42.06911538997637479, 207.3464784336661353, 1.353441290958777327E-15 ) ) ;
#66571 = CARTESIAN_POINT ( 'NONE',  ( 164.4698008747318738, 245.7769439046653019, -6.272955660526681854 ) ) ;
#66572 = CARTESIAN_POINT ( 'NONE',  ( 72.53559621566675730, 57.32287681765896536, 16.32930890408951541 ) ) ;
#66573 = CARTESIAN_POINT ( 'NONE',  ( 69.43155330386302637, 68.70253108992608304, 7.308829108440537681 ) ) ;
#66575 = B_SPLINE_CURVE_WITH_KNOTS ( 'NONE', 3,
 ( #19622, #50480, #3419, #73796, #18607, #66192, #97137, #2923, #66681, #57078 ),
 .UNSPECIFIED., .F., .F.,
 ( 4, 3, 3, 4 ),
 ( 5.849685106239000612E-15, 0.001498044977023057535, 0.004494154408229840761, 0.004642971226047358860 ),
 .UNSPECIFIED. ) ;
#66574 = CARTESIAN_POINT ( 'NONE',  ( 207.6826438088389750, 270.9301044032979462, 7.252082088659585146 ) ) ;
#66576 = EDGE_LOOP ( 'NONE', ( #2979, #45393, #71146, #15130 ) ) ;
#66577 = VECTOR ( 'NONE', #20133, 1000.000000000000000 ) ;
#66578 = CARTESIAN_POINT ( 'NONE',  ( 4.496589500409242213, 166.7365022471902023, -10.00000000000009059 ) ) ;
#66579 = LINE ( 'NONE', #34676, #48197 ) ;
#66580 = CARTESIAN_POINT ( 'NONE',  ( 131.9199452241419124, 234.7202760586659736, -5.415160957724236172E-17 ) ) ;
#66581 = CARTESIAN_POINT ( 'NONE',  ( 20.42541317417268942, 33.83396525600390703, -2.839279412974133887 ) ) ;
#66583 = CARTESIAN_POINT ( 'NONE',  ( 165.0842110975921742, 244.7127541819816372, 1.670879517523061075 ) ) ;
#66582 = B_SPLINE_CURVE_WITH_KNOTS ( 'NONE', 3,
 ( #5670, #77054, #7662, #69459 ),
 .UNSPECIFIED., .F., .F.,
 ( 4, 4 ),
 ( 0.002667466630201718782, 0.003029344800501278766 ),
 .UNSPECIFIED. ) ;
#66584 = CARTESIAN_POINT ( 'NONE',  ( 83.80447776121599190, 52.10292630681441040, -14.99896445683751622 ) ) ;
#66585 = CARTESIAN_POINT ( 'NONE',  ( 76.62413771374467331, 63.45693921867285070, 15.36854489724363759 ) ) ;
#66587 = CARTESIAN_POINT ( 'NONE',  ( 189.5521783559119342, 289.6378612515180748, 14.85317001376669843 ) ) ;
#66586 = CARTESIAN_POINT ( 'NONE',  ( 76.28872632190457637, 51.00282802105010660, -16.03419075268625349 ) ) ;
#66588 = CARTESIAN_POINT ( 'NONE',  ( 150.3767742445782289, 270.1867820605125416, -15.10420222983148442 ) ) ;
#66589 = ORIENTED_EDGE ( 'NONE', *, *, #37319, .T. ) ;
#66590 = CARTESIAN_POINT ( 'NONE',  ( 190.8094645593471341, 300.1553081486349015, 8.399847186519689757 ) ) ;
#66591 = CARTESIAN_POINT ( 'NONE',  ( 164.1233341003454314, 246.3770419610369800, 7.970621798363497490 ) ) ;
#66592 = CARTESIAN_POINT ( 'NONE',  ( 190.9904595088351584, 263.1162866600020038, -8.709768327411630651 ) ) ;
#66593 = CARTESIAN_POINT ( 'NONE',  ( 169.5763875261042415, 266.0051543528422826, -17.23840913299506283 ) ) ;
#66594 = CARTESIAN_POINT ( 'NONE',  ( 13.25720545158990937, 8.449665230724928477, -2.296566073217252530E-15 ) ) ;
#66595 = ORIENTED_EDGE ( 'NONE', *, *, #6025, .F. ) ;
#66596 = CARTESIAN_POINT ( 'NONE',  ( 68.81099849051250317, 66.60367167969251057, 9.666683708442542766 ) ) ;
#66597 = CARTESIAN_POINT ( 'NONE',  ( 171.2449227966682770, 284.2896847597517649, -11.26649335755497283 ) ) ;
#66598 = CARTESIAN_POINT ( 'NONE',  ( 77.54947637239327207, 49.71488793443786136, 14.94482653940103134 ) ) ;
#66599 = CARTESIAN_POINT ( 'NONE',  ( 196.1582417222007848, 271.0076856177163904, 12.85313896011626333 ) ) ;
#66600 = CARTESIAN_POINT ( 'NONE',  ( 182.1059484044376688, 295.6613757171786574, 4.943108598893879879 ) ) ;
#66601 = CARTESIAN_POINT ( 'NONE',  ( 69.67981129362297565, 70.80532903890349417, 1.547790508053775937 ) ) ;
#66602 = CARTESIAN_POINT ( 'NONE',  ( 74.08065690531797998, 54.82731643721707826, -16.13522336645905142 ) ) ;
#66603 = CARTESIAN_POINT ( 'NONE',  ( 192.7251185966330240, 281.9663580653335089, 16.81651591906913978 ) ) ;
#66604 = CARTESIAN_POINT ( 'NONE',  ( 12.36470590445056317, 8.108019796199268825, 3.090169943749476733 ) ) ;
#66605 = CARTESIAN_POINT ( 'NONE',  ( 94.76169564547690527, 215.5177522451417929, 5.000000000000051514 ) ) ;
#66606 = ORIENTED_EDGE ( 'NONE', *, *, #62159, .F. ) ;
#66607 = CARTESIAN_POINT ( 'NONE',  ( 169.5007657120409874, 248.2156828994837099, -1.963647642838588503 ) ) ;
#66608 = DIRECTION ( 'NONE',  ( -0.8660254037844387076, -0.4999999999999998890, -0.000000000000000000 ) ) ;
#66609 = CARTESIAN_POINT ( 'NONE',  ( 156.2535903939119635, 261.5009266245895674, -17.19818558915508433 ) ) ;
#66610 = ORIENTED_EDGE ( 'NONE', *, *, #99511, .F. ) ;
#66611 = CARTESIAN_POINT ( 'NONE',  ( 147.2592533090473239, 275.5864867145116932, -0.3770461397900867762 ) ) ;
#66612 = CARTESIAN_POINT ( 'NONE',  ( 205.0815341406070615, 273.1773411830968712, -9.768730833708779926 ) ) ;
#66613 = CARTESIAN_POINT ( 'NONE',  ( 164.4990934228277411, 245.7262077230798809, 6.470820838822735510 ) ) ;
#66614 = CARTESIAN_POINT ( 'NONE',  ( 189.5534384022301424, 269.0062095459838929, -14.92796778812864922 ) ) ;
#66615 = ORIENTED_EDGE ( 'NONE', *, *, #14490, .T. ) ;
#66616 = CARTESIAN_POINT ( 'NONE',  ( 78.92949518643405327, 222.5024278399160949, 9.188101187500095079 ) ) ;
#66617 = CARTESIAN_POINT ( 'NONE',  ( 155.5793834749241853, 261.1755985416265275, 17.09727664165891525 ) ) ;
#66618 = CARTESIAN_POINT ( 'NONE',  ( 84.42663183290281381, 49.91580812419739033, -13.73522929182741947 ) ) ;
#66619 = CARTESIAN_POINT ( 'NONE',  ( 185.0654652685402368, 260.0011547607978741, -6.087314472554996136 ) ) ;
#66620 = EDGE_LOOP ( 'NONE', ( #4567, #2487, #27160, #9472 ) ) ;
#66621 = ORIENTED_EDGE ( 'NONE', *, *, #4795, .F. ) ;
#66622 = FACE_OUTER_BOUND ( 'NONE', #73263, .T. ) ;
#66623 = B_SPLINE_CURVE_WITH_KNOTS ( 'NONE', 3,
 ( #86735, #48689, #25372, #2088 ),
 .UNSPECIFIED., .F., .F.,
 ( 4, 4 ),
 ( 0.005006823703232672271, 0.01302678491365392814 ),
 .UNSPECIFIED. ) ;
#66624 = ORIENTED_EDGE ( 'NONE', *, *, #75974, .F. ) ;
#66625 = CARTESIAN_POINT ( 'NONE',  ( 192.7503840695331121, 293.9944895470539450, 14.24544604289089555 ) ) ;
#66626 = VERTEX_POINT ( 'NONE', #42671 ) ;
#66627 = CARTESIAN_POINT ( 'NONE',  ( 159.6023402823087451, 258.6676503891110883, 17.43025742997651761 ) ) ;
#66628 = CARTESIAN_POINT ( 'NONE',  ( 155.1865148098964937, 261.8560670301561686, -16.99758927948949605 ) ) ;
#66629 = ORIENTED_EDGE ( 'NONE', *, *, #67141, .F. ) ;
#66630 = CARTESIAN_POINT ( 'NONE',  ( 207.0720832995076250, 271.9876262265548235, -6.798746899112098951 ) ) ;
#66631 = CARTESIAN_POINT ( 'NONE',  ( 82.49834280522868823, 40.76233756830425392, 3.189866935900057765 ) ) ;
#66632 = DIRECTION ( 'NONE',  ( 0.000000000000000000, 0.000000000000000000, 1.000000000000000000 ) ) ;
#66633 = CARTESIAN_POINT ( 'NONE',  ( 147.9500839974939197, 274.3899328626944225, -9.375093207164509224 ) ) ;
#66634 = EDGE_CURVE ( 'NONE', #54109, #44579, #30445, .T. ) ;
#66635 = CARTESIAN_POINT ( 'NONE',  ( 157.5377142495414944, 281.7650987280287609, 2.959616700945237433 ) ) ;
#66636 = CARTESIAN_POINT ( 'NONE',  ( 168.0409292894617295, 267.0411674002936024, -16.96956704154970907 ) ) ;
#66637 = VERTEX_POINT ( 'NONE', #34112 ) ;
#66638 = CARTESIAN_POINT ( 'NONE',  ( 76.45176290624858950, 58.46688331479428058, 16.04654028584893055 ) ) ;
#66639 = CARTESIAN_POINT ( 'NONE',  ( 13.40518456965460281, 16.24335787977761925, -9.188101187500008038 ) ) ;
#66640 = EDGE_LOOP ( 'NONE', ( #3766, #19559, #67115 ) ) ;
#66641 = CARTESIAN_POINT ( 'NONE',  ( 167.4774516927647880, 284.1243695549201789, 9.174491941972370057 ) ) ;
#66643 = ORIENTED_EDGE ( 'NONE', *, *, #67651, .T. ) ;
#66642 = CARTESIAN_POINT ( 'NONE',  ( 203.9281103364544379, 271.7020019549630661, 9.691553030514192812 ) ) ;
#66644 = CARTESIAN_POINT ( 'NONE',  ( 3.694774645000036273, 161.3932355074535678, -2.679491924311248496 ) ) ;
#66645 = DIRECTION ( 'NONE',  ( -0.8660254037844384856, -0.5000000000000002220, 0.000000000000000000 ) ) ;
#66646 = CARTESIAN_POINT ( 'NONE',  ( 76.12311946169329246, 64.72429642162367713, -14.36203512785002090 ) ) ;
#66647 = CARTESIAN_POINT ( 'NONE',  ( 161.1791855798394408, 281.3418815567459319, -6.591164736166998495 ) ) ;
#66648 = EDGE_CURVE ( 'NONE', #76155, #22001, #11326, .T. ) ;
#66649 = FACE_OUTER_BOUND ( 'NONE', #56762, .T. ) ;
#66650 = LINE ( 'NONE', #60520, #85207 ) ;
#66651 = EDGE_CURVE ( 'NONE', #69830, #77062, #61829, .T. ) ;
#66652 = CARTESIAN_POINT ( 'NONE',  ( 169.1311965936330353, 247.8770103324328034, 7.134965090537657859E-13 ) ) ;
#66653 = CARTESIAN_POINT ( 'NONE',  ( 195.1498658919753098, 292.2566161375916636, 15.21824497126251785 ) ) ;
#66654 = ORIENTED_EDGE ( 'NONE', *, *, #84765, .T. ) ;
#66655 = CARTESIAN_POINT ( 'NONE',  ( 181.5711328935895494, 270.9591510390133635, -15.96266144669950293 ) ) ;
#66656 = EDGE_LOOP ( 'NONE', ( #40806, #1220, #97073, #21750 ) ) ;
#66657 = DIRECTION ( 'NONE',  ( 1.000000000000000000, 0.000000000000000000, 0.000000000000000000 ) ) ;
#66658 = CARTESIAN_POINT ( 'NONE',  ( 174.8981841478993147, 281.3293342729474489, -14.17585464771519810 ) ) ;
#66659 = DIRECTION ( 'NONE',  ( 0.5346708562973920831, 0.8450603975019853609, 0.000000000000000000 ) ) ;
#66660 = CARTESIAN_POINT ( 'NONE',  ( 82.34616035088453145, 44.74534029615586661, -9.883898186199504110 ) ) ;
#66661 = CARTESIAN_POINT ( 'NONE',  ( 160.8938801005855908, 272.8507423001361190, 15.74055753482374698 ) ) ;
#66663 = CARTESIAN_POINT ( 'NONE',  ( 88.30945731027941292, 43.97049527616570685, 2.452112525173328450 ) ) ;
#66662 = CARTESIAN_POINT ( 'NONE',  ( 161.3681471114688293, 281.5053870741572837, -7.339062344004410043 ) ) ;
#66664 = CARTESIAN_POINT ( 'NONE',  ( -4.429217378738782962, 26.01694505731172313, -10.00000000000000000 ) ) ;
#66665 = ORIENTED_EDGE ( 'NONE', *, *, #60060, .T. ) ;
#66666 = VERTEX_POINT ( 'NONE', #82739 ) ;
#66667 = CARTESIAN_POINT ( 'NONE',  ( 41.10245927640360009, 127.8322459559854138, -10.00000000000000000 ) ) ;
#66668 = CARTESIAN_POINT ( 'NONE',  ( -49.78034631855286563, 29.87998972566340683, 10.00000000000000000 ) ) ;
#66669 = CARTESIAN_POINT ( 'NONE',  ( 85.68734770396230260, 48.85621462398719217, -12.54449143327926208 ) ) ;
#66670 = CARTESIAN_POINT ( 'NONE',  ( 175.6092358407374547, 290.9609716272898368, 2.612219778893893007 ) ) ;
#66671 = CARTESIAN_POINT ( 'NONE',  ( 192.5049767439991513, 297.2185948999652965, 12.57567268027295881 ) ) ;
#66672 = CARTESIAN_POINT ( 'NONE',  ( 80.76429156517131958, 43.10381631070730890, -9.805890018733025570 ) ) ;
#66673 = CARTESIAN_POINT ( 'NONE',  ( 29.59124024723001867, 43.31574901297116043, -10.00000000000000000 ) ) ;
#66674 = EDGE_CURVE ( 'NONE', #59735, #87466, #66150, .T. ) ;
#66675 = CARTESIAN_POINT ( 'NONE',  ( 4.207654042216683266, 182.4244531367911293, -4.594050593750046652 ) ) ;
#66676 = CARTESIAN_POINT ( 'NONE',  ( 107.7251869580316281, 226.8768266524160140, 9.188101187500098632 ) ) ;
#66677 = CARTESIAN_POINT ( 'NONE',  ( 186.6437685709837524, 295.7868322423274208, -7.682377513881603726 ) ) ;
#66678 = CARTESIAN_POINT ( 'NONE',  ( 79.39086535420604207, 59.11638920646624484, 16.20638822945242197 ) ) ;
#66679 = ADVANCED_FACE ( 'NONE', ( #82242 ), #76548, .T. ) ;
#66680 = AXIS2_PLACEMENT_3D ( 'NONE', #19796, #97794, #28364 ) ;
#66681 = CARTESIAN_POINT ( 'NONE',  ( 194.3794555884949773, 282.9248721468028975, 17.82082507299162089 ) ) ;
#66682 = CARTESIAN_POINT ( 'NONE',  ( 193.9966098916996771, 294.6350105018939871, 13.97117019253516013 ) ) ;
#66683 = LINE ( 'NONE', #51483, #1174 ) ;
#66684 = CARTESIAN_POINT ( 'NONE',  ( 194.9819925439454664, 292.9282776833073285, -15.33279721168237586 ) ) ;
#66685 = ADVANCED_FACE ( 'NONE', ( #29976 ), #1083, .T. ) ;
#66686 = CARTESIAN_POINT ( 'NONE',  ( 84.34693788441749973, 50.67364717229969528, 13.78469515595785033 ) ) ;
#66687 = CARTESIAN_POINT ( 'NONE',  ( 186.7826593668773398, 299.1805613592297846, -0.6094521799418902708 ) ) ;
#66688 = CARTESIAN_POINT ( 'NONE',  ( 165.2952469160895816, 253.4663260364826556, -13.06521362961797550 ) ) ;
#66689 = DIRECTION ( 'NONE',  ( 0.000000000000000000, -1.000000000000000000, 0.000000000000000000 ) ) ;
#66690 = CARTESIAN_POINT ( 'NONE',  ( 174.5980114852178815, 264.9326092916348330, -15.54993198801018472 ) ) ;
#66691 = CARTESIAN_POINT ( 'NONE',  ( 91.83912023130210400, 214.6423013555409796, -4.594050593750043987 ) ) ;
#66692 = CARTESIAN_POINT ( 'NONE',  ( 12.16146256644911539, 9.947547579820877672, 5.678558825948272215 ) ) ;
#66693 = CARTESIAN_POINT ( 'NONE',  ( 163.2261234402530476, 258.2666102061564857, 16.06505531561552758 ) ) ;
#66695 = CARTESIAN_POINT ( 'NONE',  ( 200.2341212244148210, 283.8313239608446565, 18.44154502101277870 ) ) ;
#66694 = CARTESIAN_POINT ( 'NONE',  ( 195.8248271798537417, 291.4684452715354155, 17.35175160929494709 ) ) ;
#66696 = CARTESIAN_POINT ( 'NONE',  ( 197.0938247690820049, 289.2704769723097797, 17.22904708886757774 ) ) ;
#66697 = B_SPLINE_CURVE_WITH_KNOTS ( 'NONE', 3,
 ( #63079, #53790, #29036, #90876 ),
 .UNSPECIFIED., .F., .F.,
 ( 4, 4 ),
 ( 0.000000000000000000, 0.002280643322503841074 ),
 .UNSPECIFIED. ) ;
#66698 = CARTESIAN_POINT ( 'NONE',  ( 151.4188942279983223, 268.3817773016460251, -14.77302265413830895 ) ) ;
#66699 = CARTESIAN_POINT ( 'NONE',  ( 79.95866072124864843, 44.52494782656018657, 11.71661119140258300 ) ) ;
#66700 = CARTESIAN_POINT ( 'NONE',  ( 35.11595366814305663, 25.98920272979928470, 7.433330006724137462 ) ) ;
#66701 = CARTESIAN_POINT ( 'NONE',  ( 193.1444937042664094, 296.1109190324805240, -12.15243020627156767 ) ) ;
#66702 = CARTESIAN_POINT ( 'NONE',  ( 83.99374970662998408, 46.89514837332161790, -11.15785913519821015 ) ) ;
#66703 = ORIENTED_EDGE ( 'NONE', *, *, #59917, .T. ) ;
#66704 = CARTESIAN_POINT ( 'NONE',  ( 21.31005897544419980, 27.70171378149919050, -9.188101187500004485 ) ) ;
#66705 = DIRECTION ( 'NONE',  ( 0.3595896960900372696, 0.9331105242498740626, 0.000000000000000000 ) ) ;
#66706 = CARTESIAN_POINT ( 'NONE',  ( 146.9700173529739970, 276.0874580858064746, -5.099093031535578469 ) ) ;
#66707 = CARTESIAN_POINT ( 'NONE',  ( 191.2921030740457411, 288.8084469331090531, -16.29029516365350005 ) ) ;
#66708 = ORIENTED_EDGE ( 'NONE', *, *, #95261, .F. ) ;
#66709 = CARTESIAN_POINT ( 'NONE',  ( 70.36476379532911096, 61.16554131547574968, 14.31790743328406101 ) ) ;
#66710 = CARTESIAN_POINT ( 'NONE',  ( 67.61549177878170269, 66.83199286464724764, -8.481431920729969320 ) ) ;
#66712 = EDGE_CURVE ( 'NONE', #26873, #12604, #7481, .T. ) ;
#66711 = CARTESIAN_POINT ( 'NONE',  ( 157.7255603307123408, 268.5163524934444013, 16.86592485641857309 ) ) ;
#66713 = LINE ( 'NONE', #59089, #11309 ) ;
#66714 = CARTESIAN_POINT ( 'NONE',  ( 181.2305971022323661, 265.9781236237157032, -15.82518789413146010 ) ) ;
#66715 = CARTESIAN_POINT ( 'NONE',  ( 129.0599100780709421, 251.9865022471903444, -10.00000000000009415 ) ) ;
#66716 = CARTESIAN_POINT ( 'NONE',  ( 204.6475128369918082, 276.1871054541632020, -13.72068618491070779 ) ) ;
#66717 = ORIENTED_EDGE ( 'NONE', *, *, #80820, .T. ) ;
#66718 = CARTESIAN_POINT ( 'NONE',  ( 81.15728453326165948, 46.74340589432950566, -12.91012880180904432 ) ) ;
#66719 = CARTESIAN_POINT ( 'NONE',  ( 165.5467306339926097, 246.9162971582917407, -1.814430410556957529 ) ) ;
#66720 = ORIENTED_EDGE ( 'NONE', *, *, #86296, .F. ) ;
#66721 = DIRECTION ( 'NONE',  ( -0.8660254037844387076, -0.4999999999999998890, -0.000000000000000000 ) ) ;
#66722 = CARTESIAN_POINT ( 'NONE',  ( -22.42236680055709641, 157.8615022471902591, 0.000000000000000000 ) ) ;
#66723 = ADVANCED_FACE ( 'NONE', ( #61858 ), #92807, .T. ) ;
#66724 = EDGE_LOOP ( 'NONE', ( #38426, #17172, #60477, #803 ) ) ;
#66725 = CARTESIAN_POINT ( 'NONE',  ( 77.19959510277064396, 63.54604015844361697, -15.07525604178641565 ) ) ;
#66726 = ORIENTED_EDGE ( 'NONE', *, *, #91616, .T. ) ;
#66727 = CARTESIAN_POINT ( 'NONE',  ( 189.4721059029944570, 290.0100815663928984, 14.44573074396852519 ) ) ;
#66728 = FACE_OUTER_BOUND ( 'NONE', #60099, .T. ) ;
#66729 = DIRECTION ( 'NONE',  ( 0.000000000000000000, 0.000000000000000000, 1.000000000000000000 ) ) ;
#66730 = CARTESIAN_POINT ( 'NONE',  ( 192.9443876183610769, 296.4575129401721370, -13.55710008152484569 ) ) ;
#66731 = CARTESIAN_POINT ( 'NONE',  ( 203.3087286698060723, 275.5229930796335793, -14.04662039663043061 ) ) ;
#66732 = CARTESIAN_POINT ( 'NONE',  ( 41.62797693021462209, 26.96004757982093025, -5.678558825948275768 ) ) ;
#66733 = CARTESIAN_POINT ( 'NONE',  ( 72.70942444841369934, 60.67579778368086352, -15.05243087098393495 ) ) ;
#66734 = CARTESIAN_POINT ( 'NONE',  ( 164.1076778612453495, 275.3502986316374859, 15.09133881111785058 ) ) ;
#66735 = CARTESIAN_POINT ( 'NONE',  ( 73.61078154397070250, 201.7592609112380160, 2.679491924311254714 ) ) ;
#66736 = ORIENTED_EDGE ( 'NONE', *, *, #95076, .F. ) ;
#66737 = ORIENTED_EDGE ( 'NONE', *, *, #99511, .T. ) ;
#66738 = CARTESIAN_POINT ( 'NONE',  ( -19.65312891409030271, 93.06504152958497400, -10.00000000000000888 ) ) ;
#66739 =( BOUNDED_CURVE ( )  B_SPLINE_CURVE ( 2, ( #96751, #10617, #56706, #64309, #34406, #35399, #97240, #26809, #72437, #57191, #19238, #87687, #18719 ),
 .UNSPECIFIED., .F., .T. ) 
 B_SPLINE_CURVE_WITH_KNOTS ( ( 3, 2, 2, 2, 2, 2, 3 ),
 ( 0.6875000000000000000, 0.6899999999999999467, 0.6949999999999999512, 0.6999999999999999556, 0.7049999999999999600, 0.7099999999999999645, 0.7125000000000000222 ),
 .UNSPECIFIED. ) 
 CURVE ( )  GEOMETRIC_REPRESENTATION_ITEM ( )  RATIONAL_B_SPLINE_CURVE ( ( 0.9755282581475768211, 0.9755282581475768211, 1.000000000000000000, 0.9510565162951535312, 1.000000000000000000, 0.9510565162951535312, 1.000000000000000000, 0.9510565162951535312, 1.000000000000000000, 0.9510565162951535312, 1.000000000000000000, 0.9755282581475761550, 0.9755282581475767101 ) ) 
 REPRESENTATION_ITEM ( '' )  );
#66741 = CARTESIAN_POINT ( 'NONE',  ( 25.96864935082048831, 154.0458036431183189, 21.50000000000008527 ) ) ;
#66740 = DIRECTION ( 'NONE',  ( -0.5270369400482041167, -0.8498423758701525443, 0.000000000000000000 ) ) ;
#66742 = CARTESIAN_POINT ( 'NONE',  ( 85.39369755680034757, 48.58767798792116821, 12.46940421135661481 ) ) ;
#66743 = CARTESIAN_POINT ( 'NONE',  ( 66.17343954913512505, 68.52301864461630032, -2.711686016849372827 ) ) ;
#66744 = CARTESIAN_POINT ( 'NONE',  ( 184.6894110187365641, 293.7322318964822330, -10.88359728165448814 ) ) ;
#66745 = CARTESIAN_POINT ( 'NONE',  ( 147.6088797830324779, 274.9809158978982850, 8.531536684623960198 ) ) ;
#66746 = LINE ( 'NONE', #97681, #91638 ) ;
#66747 = CARTESIAN_POINT ( 'NONE',  ( 169.7305867463648497, 267.4144629999083804, 17.02687474860264771 ) ) ;
#66748 = DIRECTION ( 'NONE',  ( 0.000000000000000000, 0.000000000000000000, 1.000000000000000000 ) ) ;
#66749 = CARTESIAN_POINT ( 'NONE',  ( 96.79126913948807953, 232.8149278399160949, 9.188101187500093303 ) ) ;
#66750 = ORIENTED_EDGE ( 'NONE', *, *, #13656, .T. ) ;
#66751 = CARTESIAN_POINT ( 'NONE',  ( 148.1250100625814241, 274.5153593849270237, -6.488543390179210668 ) ) ;
#66752 = B_SPLINE_CURVE_WITH_KNOTS ( 'NONE', 3,
 ( #81644, #12214, #89270, #35986 ),
 .UNSPECIFIED., .F., .F.,
 ( 4, 4 ),
 ( 0.004401395493315057861, 0.009384348131726182735 ),
 .UNSPECIFIED. ) ;
#66753 = CARTESIAN_POINT ( 'NONE',  ( 165.6972188542663389, 277.5909501293253925, -13.41042508424620294 ) ) ;
#66754 = ORIENTED_EDGE ( 'NONE', *, *, #88646, .T. ) ;
#66755 = AXIS2_PLACEMENT_3D ( 'NONE', #15592, #78430, #1921 ) ;
#66756 = AXIS2_PLACEMENT_3D ( 'NONE', #85326, #92911, #69075 ) ;
#66757 = EDGE_LOOP ( 'NONE', ( #78448, #12830, #54269, #19557 ) ) ;
#66758 = ORIENTED_EDGE ( 'NONE', *, *, #56864, .T. ) ;
#66759 = CARTESIAN_POINT ( 'NONE',  ( 87.02976255443718401, 46.40020681703909133, -8.772238895811881321 ) ) ;
#66760 = AXIS2_PLACEMENT_3D ( 'NONE', #14877, #30089, #22489 ) ;
#66762 = DIRECTION ( 'NONE',  ( 0.000000000000000000, 0.000000000000000000, 1.000000000000000000 ) ) ;
#66761 = B_SPLINE_SURFACE_WITH_KNOTS ( 'NONE', 3, 1, ( 
 ( #22556, #83397 ),
 ( #13966, #69645 ),
 ( #53441, #14938 ),
 ( #45829, #75782 ),
 ( #69144, #100073 ),
 ( #30660, #6368 ),
 ( #28657, #59540 ),
 ( #37252, #29660 ),
 ( #68151, #60537 ),
 ( #90519, #51968 ),
 ( #82908, #13480 ),
 ( #44351, #16941 ),
 ( #1770, #47827 ),
 ( #62026, #77771 ),
 ( #78766, #9353 ),
 ( #63545, #32649 ),
 ( #70644, #24047 ),
 ( #85399, #8846 ),
 ( #2270, #63049 ),
 ( #70132, #86410 ),
 ( #8356, #32141 ),
 ( #15946, #39716 ),
 ( #47341, #54942 ),
 ( #46849, #94486 ),
 ( #85919, #39225 ),
 ( #745, #71679 ),
 ( #31629, #25045 ),
 ( #1259, #93993 ),
 ( #40231, #24543 ),
 ( #17451, #62528 ),
 ( #92977, #48359 ) ),
 .UNSPECIFIED., .F., .F., .F.,
 ( 4, 3, 3, 3, 3, 3, 3, 3, 3, 3, 4 ),
 ( 2, 2 ),
 ( 0.000000000000000000, 0.1333490885032479201, 0.3007194338854572990, 0.4699862290245473417, 0.5844252810809665855, 0.6686540514502945509, 0.7354980260655585855, 0.8028463152565719074, 0.8633854507757248165, 0.9437142632667163689, 1.000000000000000000 ),
 ( 0.000000000000000000, 1.000000000000000000 ),
 .UNSPECIFIED. ) ;
#66763 = CARTESIAN_POINT ( 'NONE',  ( 196.1613785401733878, 290.8855212161054737, 15.98157687694135021 ) ) ;
#66764 = FACE_OUTER_BOUND ( 'NONE', #53029, .T. ) ;
#66765 = ADVANCED_FACE ( 'NONE', ( #54245 ), #85218, .F. ) ;
#66766 = DIRECTION ( 'NONE',  ( 0.2359789242578333723, 0.9717581732643754133, 0.000000000000000000 ) ) ;
#66767 = ORIENTED_EDGE ( 'NONE', *, *, #16299, .T. ) ;
#66768 = ADVANCED_FACE ( 'NONE', ( #47661 ), #83859, .T. ) ;
#66769 = ORIENTED_EDGE ( 'NONE', *, *, #80216, .T. ) ;
#66771 = EDGE_CURVE ( 'NONE', #58122, #46236, #48595, .T. ) ;
#66770 = LINE ( 'NONE', #11600, #33311 ) ;
#66772 = VERTEX_POINT ( 'NONE', #34473 ) ;
#66773 = EDGE_CURVE ( 'NONE', #25119, #65280, #4683, .T. ) ;
#66774 = AXIS2_PLACEMENT_3D ( 'NONE', #72031, #79665, #79162 ) ;
#66775 = PLANE ( 'NONE',  #88689 ) ;
#66776 = CARTESIAN_POINT ( 'NONE',  ( 102.9889369814290632, 220.2677522451417929, -5.000000000000041744 ) ) ;
#66777 = CARTESIAN_POINT ( 'NONE',  ( 84.00458678407764523, 49.73832886490323801, 13.34265766643008000 ) ) ;
#66779 = CARTESIAN_POINT ( 'NONE',  ( 80.32771389996757705, 57.94408260071153194, -16.24746918486169633 ) ) ;
#66778 = CARTESIAN_POINT ( 'NONE',  ( 135.2486435959970947, 239.7048013555409796, 4.594050593750051981 ) ) ;
#66780 = PLANE ( 'NONE',  #43001 ) ;
#66781 = VERTEX_POINT ( 'NONE', #52153 ) ;
#66782 = CARTESIAN_POINT ( 'NONE',  ( 157.3880781592554285, 258.0428474529849723, 18.15852591502753555 ) ) ;
#66783 = CARTESIAN_POINT ( 'NONE',  ( 81.84975730146675232, 49.11728276204326704, 13.61519513745881582 ) ) ;
#66784 = CARTESIAN_POINT ( 'NONE',  ( 48.74043828842093262, 100.0309547576005258, -10.00000000000000000 ) ) ;
#66785 = CARTESIAN_POINT ( 'NONE',  ( 172.6858628785228120, 251.2885248701833234, -0.2562763602120753936 ) ) ;
#66786 = CARTESIAN_POINT ( 'NONE',  ( 178.4306755334441448, 285.4540973033057298, 14.29586447726307874 ) ) ;
#66787 = CARTESIAN_POINT ( 'NONE',  ( 63.31414817410235685, 207.3615022471904012, 5.155647304959626652E-14 ) ) ;
#66788 = CARTESIAN_POINT ( 'NONE',  ( 198.9504127373876941, 281.7903563508199909, -16.59127471182994640 ) ) ;
#66789 = CARTESIAN_POINT ( 'NONE',  ( 81.68921996421825327, 59.23443923465870142, 0.4890738003669021228 ) ) ;
#66790 = CARTESIAN_POINT ( 'NONE',  ( 80.49194482161659892, 52.40313326226726076, 15.34488516401063229 ) ) ;
#66791 = EDGE_CURVE ( 'NONE', #12449, #56928, #90417, .T. ) ;
#66792 = CARTESIAN_POINT ( 'NONE',  ( 206.7812045875167257, 272.0977345600681474, 6.637818014026708902 ) ) ;
#66793 = CARTESIAN_POINT ( 'NONE',  ( 65.88516108981343677, 208.8458772461660544, 9.188101187500095079 ) ) ;
#66794 = CARTESIAN_POINT ( 'NONE',  ( 206.4484807199597753, 273.0677375780628608, -9.220527398138528952 ) ) ;
#66795 = CARTESIAN_POINT ( 'NONE',  ( 77.73453021100772276, 61.59708935479353897, 16.08607222837813922 ) ) ;
#66796 = CARTESIAN_POINT ( 'NONE',  ( 163.4055107321044318, 247.6203485056908846, -10.24153090796238530 ) ) ;
#66797 = CARTESIAN_POINT ( 'NONE',  ( 67.47767788923495402, 69.56616349044860215, -0.01493465584580692777 ) ) ;
#66798 = DIRECTION ( 'NONE',  ( -0.3213938048432640748, 0.5566703992264119272, -0.7660444431189857850 ) ) ;
#66799 = CARTESIAN_POINT ( 'NONE',  ( 78.91181281398866076, 50.63267699903087049, 15.50297620496208317 ) ) ;
#66800 = CARTESIAN_POINT ( 'NONE',  ( 33.24377527499414242, 31.14441083166263269, 10.00000000000000533 ) ) ;
#66801 = CARTESIAN_POINT ( 'NONE',  ( 79.40381832342256985, 56.26532398263896795, -16.55503524308543462 ) ) ;
#66802 = CARTESIAN_POINT ( 'NONE',  ( 82.70408928404155802, 54.02126990151200658, 15.49668869734769672 ) ) ;
#66803 = CARTESIAN_POINT ( 'NONE',  ( 71.79701493962480185, 71.88116747554488484, 2.917949182627429305 ) ) ;
#66804 = CARTESIAN_POINT ( 'NONE',  ( 18.30771692152332975, 187.5024278399160949, -9.188101187500093303 ) ) ;
#66805 = CARTESIAN_POINT ( 'NONE',  ( 67.73185026608422277, 68.24509447089671710, 7.391104519061957312 ) ) ;
#66806 = ORIENTED_EDGE ( 'NONE', *, *, #50984, .T. ) ;
#66807 = DIRECTION ( 'NONE',  ( 0.000000000000000000, -0.000000000000000000, 1.000000000000000000 ) ) ;
#66808 = CARTESIAN_POINT ( 'NONE',  ( 202.4560076411394220, 279.0611292670678267, 15.58065739802832717 ) ) ;
#66809 = CARTESIAN_POINT ( 'NONE',  ( -71.61465314115659453, 63.06504152958490295, -40.00000000000000000 ) ) ;
#66810 = CARTESIAN_POINT ( 'NONE',  ( 34.30385554556135475, 35.50829794293883168, -10.00000000000000355 ) ) ;
#66811 = CARTESIAN_POINT ( 'NONE',  ( 44.82974491242176640, 202.8149278399161233, 9.188101187500093303 ) ) ;
#66812 = B_SPLINE_CURVE_WITH_KNOTS ( 'NONE', 3,
 ( #16555, #47449, #63155, #94102 ),
 .UNSPECIFIED., .F., .F.,
 ( 4, 4 ),
 ( 0.02705554120967477993, 0.03627623533732127897 ),
 .UNSPECIFIED. ) ;
#66813 = EDGE_CURVE ( 'NONE', #37857, #82804, #97302, .T. ) ;
#66814 = CARTESIAN_POINT ( 'NONE',  ( 200.7523954295751594, 282.9336467052548869, 18.23634913067694185 ) ) ;
#66815 = CARTESIAN_POINT ( 'NONE',  ( 39.80235952159635815, 84.99999999999998579, 10.00000000000000000 ) ) ;
#66816 = CARTESIAN_POINT ( 'NONE',  ( 190.2287563641723978, 301.1611242470490311, -4.521471513871881953 ) ) ;
#66817 = CARTESIAN_POINT ( 'NONE',  ( 42.68871737883920048, 29.81029122506298634, 8.090169943749479842 ) ) ;
#66818 = CARTESIAN_POINT ( 'NONE',  ( 175.8346136117470166, 290.9171170946435723, -7.656592247309970567 ) ) ;
#66819 = CARTESIAN_POINT ( 'NONE',  ( 178.5384570540184370, 293.1491523154654715, 2.625233457618431299 ) ) ;
#66820 = CARTESIAN_POINT ( 'NONE',  ( 177.2719741535860578, 275.4483640892808012, 16.48456767178202043 ) ) ;
#66821 = CARTESIAN_POINT ( 'NONE',  ( -22.42236680055709641, 157.8615022471902591, 0.000000000000000000 ) ) ;
#66822 = CARTESIAN_POINT ( 'NONE',  ( 67.99639869681988102, 67.83379250622242296, -7.292278942132766062 ) ) ;
#66823 = CARTESIAN_POINT ( 'NONE',  ( 167.1132731660547961, 257.9384026749979171, -15.49077391459553432 ) ) ;
#66824 = AXIS2_PLACEMENT_3D ( 'NONE', #26199, #81929, #50976 ) ;
#66825 = CARTESIAN_POINT ( 'NONE',  ( 188.0737869051473012, 299.5124861214166572, -3.734995909225475863 ) ) ;
#66826 = CARTESIAN_POINT ( 'NONE',  ( 95.35708811412658292, 225.8615022471902591, -10.00000000000009592 ) ) ;
#66827 = CARTESIAN_POINT ( 'NONE',  ( 81.52469153597657225, 59.51941083166271795, 0.2499999999999960032 ) ) ;
#66828 = CARTESIAN_POINT ( 'NONE',  ( 165.0276504369421104, 270.2126989760424749, -16.40444607549173384 ) ) ;
#66829 = VERTEX_POINT ( 'NONE', #50659 ) ;
#66830 = CARTESIAN_POINT ( 'NONE',  ( 62.50250967810423930, 197.7048013555409796, 4.594050593750051981 ) ) ;
#66831 = ORIENTED_EDGE ( 'NONE', *, *, #91254, .T. ) ;
#66832 = CARTESIAN_POINT ( 'NONE',  ( 164.2588978958649193, 264.2780746704087846, 16.72791175256383411 ) ) ;
#66833 = CARTESIAN_POINT ( 'NONE',  ( 190.1635032421960148, 301.2741459696644029, -5.047660290019184259 ) ) ;
#66834 = CARTESIAN_POINT ( 'NONE',  ( 67.20567196973209434, 67.17854346287718670, -8.569229914137681092 ) ) ;
#66835 = EDGE_LOOP ( 'NONE', ( #27066, #6840, #88602, #89371 ) ) ;
#66837 = DIRECTION ( 'NONE',  ( -0.8660254037844387076, -0.4999999999999998890, -0.000000000000000000 ) ) ;
#66836 = AXIS2_PLACEMENT_3D ( 'NONE', #75211, #21018, #89454 ) ;
#66838 = LINE ( 'NONE', #51651, #83080 ) ;
#66839 = CARTESIAN_POINT ( 'NONE',  ( 81.17232691891706509, 55.55242957854174080, 16.36487835605630536 ) ) ;
#66840 = CARTESIAN_POINT ( 'NONE',  ( 34.35336353842534152, 22.76004757982091320, 5.678558825948272215 ) ) ;
#66841 = CARTESIAN_POINT ( 'NONE',  ( 185.7886707784097950, 263.2411039711001877, 11.08596199193305232 ) ) ;
#66842 = DIRECTION ( 'NONE',  ( 0.4525327339300069251, -0.8917477921037054722, 0.000000000000000000 ) ) ;
#66843 = CARTESIAN_POINT ( 'NONE',  ( 204.6244483240926400, 276.2270543623566255, 13.10813453876796864 ) ) ;
#66844 = ORIENTED_EDGE ( 'NONE', *, *, #79545, .T. ) ;
#66845 = CARTESIAN_POINT ( 'NONE',  ( 19.31277771287585310, 13.01110640527291551, 2.839279412974134775 ) ) ;
#66846 = DIRECTION ( 'NONE',  ( 0.8660254037844391517, 0.4999999999999990008, 0.000000000000000000 ) ) ;
#66847 = CARTESIAN_POINT ( 'NONE',  ( 66.88651227603331506, 69.13534811060253560, -1.466183419788135378 ) ) ;
#66848 = DIRECTION ( 'NONE',  ( -0.4999999999999987788, 0.8660254037844392627, 0.000000000000000000 ) ) ;
#66849 = ORIENTED_EDGE ( 'NONE', *, *, #47713, .F. ) ;
#66850 = CARTESIAN_POINT ( 'NONE',  ( 76.74641017894596473, 54.96141969970745578, 16.56981576960984626 ) ) ;
#66851 = CARTESIAN_POINT ( 'NONE',  ( 65.82437655349816907, 69.12761348810170148, -0.3171013769033947383 ) ) ;
#66852 = CARTESIAN_POINT ( 'NONE',  ( 206.5081929095101998, 272.9643130319303737, -9.215516226794479238 ) ) ;
#66853 = VERTEX_POINT ( 'NONE', #74984 ) ;
#66854 = ORIENTED_EDGE ( 'NONE', *, *, #41114, .F. ) ;
#66856 = CARTESIAN_POINT ( 'NONE',  ( 113.8346084569740242, 224.9824982072973967, 3.021315404115420679E-15 ) ) ;
#66855 = CARTESIAN_POINT ( 'NONE',  ( 161.8153478334749877, 250.3745914384277285, -14.21120979595050215 ) ) ;
#66857 = DIRECTION ( 'NONE',  ( -0.8660254037844384856, -0.5000000000000002220, 0.000000000000000000 ) ) ;
#66858 = ORIENTED_EDGE ( 'NONE', *, *, #33705, .F. ) ;
#66859 = CARTESIAN_POINT ( 'NONE',  ( 66.29454943682360124, 69.24199052645600716, -2.144636311120903471 ) ) ;
#66860 = CARTESIAN_POINT ( 'NONE',  ( 159.5284711081640125, 254.3355781173132755, 15.34104435652608522 ) ) ;
#66861 = CARTESIAN_POINT ( 'NONE',  ( 72.41389820116259557, 70.72247311216294463, 7.745007521649668547 ) ) ;
#66862 = CARTESIAN_POINT ( 'NONE',  ( 161.0638154310756818, 262.9933345025709173, -17.40812897737963283 ) ) ;
#66863 = CARTESIAN_POINT ( 'NONE',  ( 124.6666353716822186, 242.7833772461660544, -9.188101187500095079 ) ) ;
#66864 = CARTESIAN_POINT ( 'NONE',  ( 150.6655900823359389, 269.6865383554857090, 15.31288044136207205 ) ) ;
#66865 = DIRECTION ( 'NONE',  ( -0.8660254037844387076, -0.4999999999999998890, -0.000000000000000000 ) ) ;
#66866 = VERTEX_POINT ( 'NONE', #20283 ) ;
#66867 = CARTESIAN_POINT ( 'NONE',  ( 148.6500818154487433, 275.1775010768142238, 7.719411301773694944 ) ) ;
#66868 = EDGE_LOOP ( 'NONE', ( #70484, #24985, #42357, #33474 ) ) ;
#66869 = ORIENTED_EDGE ( 'NONE', *, *, #80451, .F. ) ;
#66870 = CARTESIAN_POINT ( 'NONE',  ( 159.7608930362198407, 253.9330115291272421, 15.38895778945778581 ) ) ;
#66871 = CARTESIAN_POINT ( 'NONE',  ( 204.7308350088324289, 274.2642561119486686, -12.27241466464917963 ) ) ;
#66872 = CARTESIAN_POINT ( 'NONE',  ( 82.06918437091763963, 212.0643266524160140, 9.188101187500095079 ) ) ;
#66873 = ORIENTED_EDGE ( 'NONE', *, *, #44800, .F. ) ;
#66874 = CARTESIAN_POINT ( 'NONE',  ( 39.20103187901341357, 54.69033006916458106, -10.00000000000000000 ) ) ;
#66875 = CARTESIAN_POINT ( 'NONE',  ( 81.58121470000600084, 55.78443411318616540, 16.36431025809738671 ) ) ;
#66876 = CARTESIAN_POINT ( 'NONE',  ( 151.0480362197490933, 269.0241222143274626, 14.53796507407317762 ) ) ;
#66877 = ADVANCED_FACE ( 'NONE', ( #28360 ), #82626, .T. ) ;
#66878 = CARTESIAN_POINT ( 'NONE',  ( 175.8464236115564461, 278.0655253321181704, 16.02019172894276267 ) ) ;
#66879 = CARTESIAN_POINT ( 'NONE',  ( 87.68151411726066158, 45.11153824597519701, 6.862463844403660751 ) ) ;
#66880 = ORIENTED_EDGE ( 'NONE', *, *, #26764, .T. ) ;
#66881 = EDGE_CURVE ( 'NONE', #55501, #19903, #59750, .T. ) ;
#66882 = CARTESIAN_POINT ( 'NONE',  ( 121.1754704609022752, 230.7677522451417929, -5.000000000000041744 ) ) ;
#66883 = CARTESIAN_POINT ( 'NONE',  ( 153.4613150239306094, 264.8442007126561748, -16.86932470306368259 ) ) ;
#66884 = CARTESIAN_POINT ( 'NONE',  ( 203.5555343017997529, 278.0784677578903370, -15.71723084798551362 ) ) ;
#66885 = ORIENTED_EDGE ( 'NONE', *, *, #97007, .T. ) ;
#66886 = CARTESIAN_POINT ( 'NONE',  ( 206.8806555995618055, 270.0414039046062271, 3.363062889176088976 ) ) ;
#66887 = CARTESIAN_POINT ( 'NONE',  ( 76.21618662203624694, 51.03057968305066083, -16.05037395188493576 ) ) ;
#66888 = EDGE_CURVE ( 'NONE', #61729, #62607, #82555, .T. ) ;
#66889 = CARTESIAN_POINT ( 'NONE',  ( 165.3552783545318050, 246.2432519206945472, 4.078954813822171843 ) ) ;
#66890 = B_SPLINE_CURVE_WITH_KNOTS ( 'NONE', 3,
 ( #97808, #82645, #19806, #68373 ),
 .UNSPECIFIED., .F., .F.,
 ( 4, 4 ),
 ( 0.01738225534458222657, 0.02631611770651103369 ),
 .UNSPECIFIED. ) ;
#66891 = CARTESIAN_POINT ( 'NONE',  ( 168.3557124657904467, 273.6222795104500278, 17.14480014634877136 ) ) ;
#66892 = CARTESIAN_POINT ( 'NONE',  ( 185.9427433571077586, 257.7868782628476083, -2.501399907045548598 ) ) ;
#66893 = CARTESIAN_POINT ( 'NONE',  ( 194.8870616291461886, 279.6787320282184055, 16.91106461190539179 ) ) ;
#66894 = ORIENTED_EDGE ( 'NONE', *, *, #12408, .T. ) ;
#66895 = CARTESIAN_POINT ( 'NONE',  ( 207.5230514910949182, 271.2065264061283756, 2.678931747975364708 ) ) ;
#66896 = CARTESIAN_POINT ( 'NONE',  ( 141.2833242589136375, 258.5024278399160380, 9.188101187500095079 ) ) ;
#66897 = ORIENTED_EDGE ( 'NONE', *, *, #53823, .T. ) ;
#66898 = CARTESIAN_POINT ( 'NONE',  ( -61.39381520214497101, 38.43978098112751951, -10.00000000000000000 ) ) ;
#66899 = CARTESIAN_POINT ( 'NONE',  ( 86.13696227940769745, 44.49281544815586642, 6.407054959019385265 ) ) ;
#66900 = CARTESIAN_POINT ( 'NONE',  ( 87.88174357402824910, 44.02160025480015548, -1.794566980668626188 ) ) ;
#66901 = CARTESIAN_POINT ( 'NONE',  ( 40.08283240419611815, 56.57374221892477806, 10.00000000000000000 ) ) ;
#66902 = LINE ( 'NONE', #44086, #41779 ) ;
#66903 = DIRECTION ( 'NONE',  ( -0.7005979833698863235, -0.7135562106085605594, 0.000000000000000000 ) ) ;
#66904 = ORIENTED_EDGE ( 'NONE', *, *, #51004, .F. ) ;
#66905 = CARTESIAN_POINT ( 'NONE',  ( 76.96774782091593181, 57.10333325502509183, 16.17939703112071825 ) ) ;
#66906 = DIRECTION ( 'NONE',  ( 0.000000000000000000, 0.000000000000000000, 1.000000000000000000 ) ) ;
#66907 = VECTOR ( 'NONE', #90445, 1000.000000000000000 ) ;
#66908 = CARTESIAN_POINT ( 'NONE',  ( 167.8403594995746175, 248.8093847173732058, -6.497506089718841693 ) ) ;
#66909 = CARTESIAN_POINT ( 'NONE',  ( 164.2904957002474191, 246.0875095769322911, -1.594749884056509748 ) ) ;
#66910 = CARTESIAN_POINT ( 'NONE',  ( 180.4572463832561482, 261.7460625851787199, -13.63662180976220384 ) ) ;
#66911 = CARTESIAN_POINT ( 'NONE',  ( -13.11024591527723615, 27.99999999999999645, -48.00000000000017053 ) ) ;
#66912 = CARTESIAN_POINT ( 'NONE',  ( 183.3251615928574267, 281.0033614153954886, 17.25538570714889985 ) ) ;
#66913 = CARTESIAN_POINT ( 'NONE',  ( 157.4893260420801653, 257.8674809757739013, -18.30842125257398223 ) ) ;
#66914 = CARTESIAN_POINT ( 'NONE',  ( 196.5331985480450783, 270.3460110500564610, 11.78449596397654808 ) ) ;
#66915 = CARTESIAN_POINT ( 'NONE',  ( 20.78273902371470072, 14.12755873383625627, -6.180339887498949025 ) ) ;
#66916 = CARTESIAN_POINT ( 'NONE',  ( 190.0896302098338424, 301.4020978150248311, 3.433521196325825642 ) ) ;
#66917 = CARTESIAN_POINT ( 'NONE',  ( 204.7847318215661119, 274.1906186268559509, 12.16298107665122252 ) ) ;
#66918 = DIRECTION ( 'NONE',  ( 1.235257323912246174E-15, 1.000000000000000000, -0.000000000000000000 ) ) ;
#66919 = CARTESIAN_POINT ( 'NONE',  ( 88.28592015977814356, 44.16006502160688996, -0.2344584660017056954 ) ) ;
#66920 = CARTESIAN_POINT ( 'NONE',  ( 71.85042758235270810, 71.69843285251393183, -3.789477364735254650 ) ) ;
#66921 = CARTESIAN_POINT ( 'NONE',  ( 137.9907970510501514, 237.1427522451417360, 1.119607411625061291E-15 ) ) ;
#66922 = CARTESIAN_POINT ( 'NONE',  ( 175.4968960841862895, 286.3374744733690136, -12.09459527608030172 ) ) ;
#66923 = VERTEX_POINT ( 'NONE', #35959 ) ;
#66924 = CARTESIAN_POINT ( 'NONE',  ( 157.7233946900069839, 257.4620621851055375, 16.86796251324260254 ) ) ;
#66925 = CARTESIAN_POINT ( 'NONE',  ( 198.6894790592683080, 286.5067226703918095, -17.06774375037124614 ) ) ;
#66926 = CARTESIAN_POINT ( 'NONE',  ( 16.79251956066557128, 174.3768266524160140, 9.188101187500096856 ) ) ;
#66927 = EDGE_CURVE ( 'NONE', #29146, #81396, #90213, .T. ) ;
#66928 = CARTESIAN_POINT ( 'NONE',  ( 179.8888715531147682, 274.4711782159853328, -17.82026667163308531 ) ) ;
#66929 = CARTESIAN_POINT ( 'NONE',  ( 28.12420092063944566, 24.43677371833802781, -10.00000000000000355 ) ) ;
#66930 = CARTESIAN_POINT ( 'NONE',  ( 85.29121890838305831, 49.09086179670648420, 12.44079179351374442 ) ) ;
#66931 = CARTESIAN_POINT ( 'NONE',  ( 157.3198323354746435, 258.1610526871778006, -16.77630483474704093 ) ) ;
#66932 = CARTESIAN_POINT ( 'NONE',  ( 72.19712139806571827, 71.87787970473654298, -3.871494628622227818 ) ) ;
#66933 = CARTESIAN_POINT ( 'NONE',  ( 150.0923052775327449, 276.4933692631097983, 3.710611330911921524 ) ) ;
#66935 = CARTESIAN_POINT ( 'NONE',  ( 67.04888272437477781, 219.5177522451419065, 5.000000000000046185 ) ) ;
#66934 = CARTESIAN_POINT ( 'NONE',  ( 167.4210765078939005, 256.7953526967608013, 14.03692215505185459 ) ) ;
#66936 = CARTESIAN_POINT ( 'NONE',  ( 74.59816150844692118, 67.00000980971049103, 12.52809777808814751 ) ) ;
#66937 = CARTESIAN_POINT ( 'NONE',  ( 197.9812996484125449, 287.7333253908681741, 17.50297787674340455 ) ) ;
#66938 = EDGE_CURVE ( 'NONE', #10169, #28472, #51677, .T. ) ;
#66939 = CARTESIAN_POINT ( 'NONE',  ( 50.32376711733572705, 209.8615022471902876, 5.000000000000046185 ) ) ;
#66940 = CARTESIAN_POINT ( 'NONE',  ( 181.8982906980151313, 291.6576164288949258, 9.318166351261279345 ) ) ;
#66941 = CARTESIAN_POINT ( 'NONE',  ( 147.7157269441172218, 274.7958511862549926, 8.036290321896261801 ) ) ;
#66942 = CARTESIAN_POINT ( 'NONE',  ( 17.82075117977708700, 181.0958772461660544, -9.188101187500095079 ) ) ;
#66943 = CARTESIAN_POINT ( 'NONE',  ( 72.86429505109984461, 70.96802964124920265, -7.768747002037670768 ) ) ;
#66944 = EDGE_CURVE ( 'NONE', #47529, #65006, #83102, .T. ) ;
#66945 = CARTESIAN_POINT ( 'NONE',  ( 79.42866338260434134, 59.50128377535573776, 16.18467811310512872 ) ) ;
#66946 = CARTESIAN_POINT ( 'NONE',  ( 39.17063663036994114, 34.56628583063844928, 9.188101187500006262 ) ) ;
#66947 = CARTESIAN_POINT ( 'NONE',  ( 201.4636277339562298, 280.4837806593683354, -16.45470140429584660 ) ) ;
#66948 = B_SPLINE_CURVE_WITH_KNOTS ( 'NONE', 3,
 ( #38955, #40453, #1485, #54143 ),
 .UNSPECIFIED., .F., .F.,
 ( 4, 4 ),
 ( 0.03503658997592057345, 0.04381483082515637284 ),
 .UNSPECIFIED. ) ;
#66949 = CARTESIAN_POINT ( 'NONE',  ( 164.8251969117060298, 245.1613799118173063, -1.508678420156898348 ) ) ;
#66950 = CARTESIAN_POINT ( 'NONE',  ( 18.62433137644124059, 29.49103043416549141, -8.090169943749479842 ) ) ;
#66951 = CARTESIAN_POINT ( 'NONE',  ( 153.2585711273538891, 265.9210912079520881, -16.19689858454334441 ) ) ;
#66952 = CARTESIAN_POINT ( 'NONE',  ( 177.1159597426109258, 261.0416103176956426, -13.08779172971381044 ) ) ;
#66953 = DIRECTION ( 'NONE',  ( 0.000000000000000000, 0.000000000000000000, 1.000000000000000000 ) ) ;
#66954 = CARTESIAN_POINT ( 'NONE',  ( 17.03285546273658113, 12.76004757982088655, 5.678558825948272215 ) ) ;
#66955 = CARTESIAN_POINT ( 'NONE',  ( -14.37785915960194494, 174.0530062829863027, 6.972266317189433612E-15 ) ) ;
#66956 = DIRECTION ( 'NONE',  ( -0.8660254037844378194, -0.5000000000000013323, -0.000000000000000000 ) ) ;
#66957 = CARTESIAN_POINT ( 'NONE',  ( 25.96864935082050252, 154.0458036431183189, -30.52142883766499892 ) ) ;
#66958 = CARTESIAN_POINT ( 'NONE',  ( 154.9910882912764123, 262.1945556895526579, 18.38052604520346023 ) ) ;
#66959 = ORIENTED_EDGE ( 'NONE', *, *, #32610, .T. ) ;
#66960 = CARTESIAN_POINT ( 'NONE',  ( 182.0334299555740074, 289.9311837412762998, 12.98645721431532785 ) ) ;
#66961 = CARTESIAN_POINT ( 'NONE',  ( 156.8667541408265436, 276.4807214582178858, 10.34413747573048958 ) ) ;
#66962 = CARTESIAN_POINT ( 'NONE',  ( 206.7680519836501958, 272.5142239127119979, -10.57935479673322021 ) ) ;
#66963 = ORIENTED_EDGE ( 'NONE', *, *, #62397, .T. ) ;
#66964 = CARTESIAN_POINT ( 'NONE',  ( 196.6309300382015124, 289.4139301465927474, -16.57619966563450120 ) ) ;
#66965 = CARTESIAN_POINT ( 'NONE',  ( 78.97477422587097351, 209.7365022471902307, 10.00000000000009948 ) ) ;
#66966 = CARTESIAN_POINT ( 'NONE',  ( 66.67158450822250870, 68.31487490133181950, 4.544081535773483616 ) ) ;
#66967 = CARTESIAN_POINT ( 'NONE',  ( 202.8549823380854491, 279.2918593523859272, -16.39745931995414807 ) ) ;
#66968 = AXIS2_PLACEMENT_3D ( 'NONE', #84480, #76832, #22143 ) ;
#66969 = ORIENTED_EDGE ( 'NONE', *, *, #18849, .F. ) ;
#66970 = ORIENTED_EDGE ( 'NONE', *, *, #33960, .F. ) ;
#66971 = B_SPLINE_CURVE_WITH_KNOTS ( 'NONE', 3,
 ( #55687, #86675, #54697, #17207 ),
 .UNSPECIFIED., .F., .F.,
 ( 4, 4 ),
 ( 0.008571673128587826290, 0.01494991930079212113 ),
 .UNSPECIFIED. ) ;
#66973 = CARTESIAN_POINT ( 'NONE',  ( 204.8762144138505903, 275.7909827032724479, 14.60855957933206817 ) ) ;
#66972 = CARTESIAN_POINT ( 'NONE',  ( 164.6331389003996435, 246.4978176680588717, -4.355654215571391319 ) ) ;
#66974 = CARTESIAN_POINT ( 'NONE',  ( 153.1973045377566507, 265.3014802884401320, 17.70608187426261892 ) ) ;
#66975 = ORIENTED_EDGE ( 'NONE', *, *, #35203, .F. ) ;
#66976 = CARTESIAN_POINT ( 'NONE',  ( 190.7851751463332164, 300.1973786460605425, 8.237717828100052486 ) ) ;
#66977 = CARTESIAN_POINT ( 'NONE',  ( 80.35079170152107508, 57.80872192622025807, 16.60075256504293506 ) ) ;
#66978 = CARTESIAN_POINT ( 'NONE',  ( 174.5259399585505093, 262.2319009501799201, 15.75388500574217687 ) ) ;
#66979 = ORIENTED_EDGE ( 'NONE', *, *, #15635, .F. ) ;
#66980 = PLANE ( 'NONE',  #3800 ) ;
#66981 = CIRCLE ( 'NONE', #44344, 70.00000000000001421 ) ;
#66982 = CARTESIAN_POINT ( 'NONE',  ( 80.93680789325865987, 43.53691286975769970, 9.390856855332286202 ) ) ;
#66983 = EDGE_LOOP ( 'NONE', ( #72647, #82661, #87994, #34728 ) ) ;
#66984 = CARTESIAN_POINT ( 'NONE',  ( 165.0308887387863876, 244.8051112166122891, 1.948365933089477808 ) ) ;
#66985 = CARTESIAN_POINT ( 'NONE',  ( 151.0104406072433960, 275.7624194085408362, -8.268042829941808947 ) ) ;
#66986 = B_SPLINE_SURFACE_WITH_KNOTS ( 'NONE', 3, 1, ( 
 ( #43272, #27608 ),
 ( #72730, #73210 ),
 ( #66590, #82834 ),
 ( #27105, #57990 ),
 ( #97513, #58955 ),
 ( #13403, #20003 ),
 ( #3320, #59459 ),
 ( #98000, #74219 ),
 ( #88460, #82346 ),
 ( #34201, #80852 ),
 ( #36174, #4808 ),
 ( #26602, #50882 ),
 ( #73701, #89927 ),
 ( #81830, #11424 ),
 ( #4284, #20505 ),
 ( #49894, #88971 ),
 ( #5294, #28580 ),
 ( #42276, #51378 ),
 ( #57477, #35183 ),
 ( #65091, #66092 ),
 ( #12406, #67077 ),
 ( #89447, #58474 ),
 ( #90440, #3805 ),
 ( #12914, #43773 ),
 ( #21012, #34685 ),
 ( #65587, #96535 ),
 ( #50386, #19526 ),
 ( #85320, #5781 ),
 ( #54348, #92416 ),
 ( #7269, #75696 ),
 ( #76682, #52378 ),
 ( #22479, #61467 ),
 ( #13882, #69070 ),
 ( #46250, #99997 ) ),
 .UNSPECIFIED., .T., .F., .F.,
 ( 4, 2, 2, 2, 2, 2, 2, 2, 2, 2, 2, 2, 2, 2, 2, 2, 4 ),
 ( 2, 2 ),
 ( 0.000000000000000000, 0.06250000000000000000, 0.1250000000000000000, 0.1875000000000000000, 0.2500000000000000000, 0.3125000000000000000, 0.3750000000000000000, 0.4375000000000000000, 0.5000000000000000000, 0.5625000000000000000, 0.6250000000000000000, 0.6875000000000000000, 0.7500000000000000000, 0.8125000000000000000, 0.8750000000000000000, 0.9375000000000000000, 1.000000000000000000 ),
 ( 0.000000000000000000, 1.000000000000000000 ),
 .UNSPECIFIED. ) ;
#66987 = ORIENTED_EDGE ( 'NONE', *, *, #54191, .F. ) ;
#66988 = CARTESIAN_POINT ( 'NONE',  ( 176.4997652591337669, 278.4766424938736122, -15.78386933605245623 ) ) ;
#66989 = CARTESIAN_POINT ( 'NONE',  ( 169.8069776206597226, 261.6727971985682757, -16.70353856883196286 ) ) ;
#66990 = EDGE_LOOP ( 'NONE', ( #5487, #42894, #55368, #78982 ) ) ;
#66991 = CARTESIAN_POINT ( 'NONE',  ( 83.21237853290490705, 230.3967562850347122, -4.648177544792955347E-16 ) ) ;
#66992 = CARTESIAN_POINT ( 'NONE',  ( 147.4824818982269790, 275.1998434563504929, -4.972419998968698351 ) ) ;
#66993 = ORIENTED_EDGE ( 'NONE', *, *, #9491, .T. ) ;
#66994 = CARTESIAN_POINT ( 'NONE',  ( 157.1844736846585135, 269.4583905584224794, 15.72531959550208924 ) ) ;
#66995 = ORIENTED_EDGE ( 'NONE', *, *, #59084, .F. ) ;
#66996 = CARTESIAN_POINT ( 'NONE',  ( 76.00669415887497848, 52.71670032653177174, -16.39932529399118977 ) ) ;
#66997 = CARTESIAN_POINT ( 'NONE',  ( 37.58366506746438773, 204.0530062829863027, 1.101618078115930403E-13 ) ) ;
#66998 = CARTESIAN_POINT ( 'NONE',  ( 188.6191100762007693, 298.5688725033372179, -4.585965395504582709 ) ) ;
#66999 = CARTESIAN_POINT ( 'NONE',  ( 66.57026871561890857, 68.76443072695623471, 4.738950751700697239 ) ) ;
#67000 = CARTESIAN_POINT ( 'NONE',  ( 153.2712411579340426, 265.1734183057532732, 16.26687330118495467 ) ) ;
#67001 = EDGE_CURVE ( 'NONE', #82304, #10254, #19791, .T. ) ;
#67002 = CARTESIAN_POINT ( 'NONE',  ( 178.5194744259596291, 291.5691938275101052, 6.150709895237527647 ) ) ;
#67003 = EDGE_CURVE ( 'NONE', #61768, #63364, #58263, .T. ) ;
#67004 = CARTESIAN_POINT ( 'NONE',  ( 191.8000917695741805, 298.4394914891611847, -9.452573400474340914 ) ) ;
#67005 = VERTEX_POINT ( 'NONE', #90721 ) ;
#67006 = LINE ( 'NONE', #37103, #46384 ) ;
#67007 = B_SPLINE_CURVE_WITH_KNOTS ( 'NONE', 3,
 ( #81266, #82270, #56910, #65029 ),
 .UNSPECIFIED., .F., .F.,
 ( 4, 4 ),
 ( 0.008211037360764261370, 0.01440753375246466364 ),
 .UNSPECIFIED. ) ;
#67008 = CARTESIAN_POINT ( 'NONE',  ( 36.78445495848383473, 29.43677371833804202, -10.00000000000000355 ) ) ;
#67010 = LINE ( 'NONE', #98440, #59600 ) ;
#67009 = CARTESIAN_POINT ( 'NONE',  ( 149.0164813726494799, 272.5428784278667536, -11.67305721329070423 ) ) ;
#67012 = ORIENTED_EDGE ( 'NONE', *, *, #15697, .T. ) ;
#67011 = CARTESIAN_POINT ( 'NONE',  ( 198.3150362131025588, 287.1552767044814800, 18.53472937702030521 ) ) ;
#67013 = CARTESIAN_POINT ( 'NONE',  ( 167.7405389411880208, 287.2496306518623328, 3.554903326435361333 ) ) ;
#67014 = CARTESIAN_POINT ( 'NONE',  ( 11.47080329375824981, 30.07510926853015221, 10.00000000000000000 ) ) ;
#67015 = EDGE_LOOP ( 'NONE', ( #9989, #661, #7977, #79098, #38295 ) ) ;
#67016 = CARTESIAN_POINT ( 'NONE',  ( 70.83287887816190675, 66.76925213766115519, 10.79410789241422108 ) ) ;
#67017 = CARTESIAN_POINT ( 'NONE',  ( 84.99999999999998579, 14.99999999999999467, 59.99999999999999289 ) ) ;
#67018 = CARTESIAN_POINT ( 'NONE',  ( 12.92385338608513123, 23.16454794089040092, -10.00000000000000355 ) ) ;
#67019 = CARTESIAN_POINT ( 'NONE',  ( 160.3496834799760506, 252.9131965655305692, -14.64892343956422671 ) ) ;
#67020 = CARTESIAN_POINT ( 'NONE',  ( 91.00660716696484087, 234.8967562850347122, -4.648177544792955347E-16 ) ) ;
#67021 = EDGE_LOOP ( 'NONE', ( #81359, #97121, #3817, #54629 ) ) ;
#67022 = CARTESIAN_POINT ( 'NONE',  ( 170.5601965100331654, 255.5687049720617949, -11.63993357083384872 ) ) ;
#67023 = CARTESIAN_POINT ( 'NONE',  ( 45.57373283677818421, 114.7827874512443032, 10.00000000000000000 ) ) ;
#67024 = CARTESIAN_POINT ( 'NONE',  ( 153.2583947049096764, 265.1956690150883560, -17.64103123457563882 ) ) ;
#67025 = CARTESIAN_POINT ( 'NONE',  ( 206.8968397926183229, 272.2911568841838061, 7.145103750817420440 ) ) ;
#67026 = CARTESIAN_POINT ( 'NONE',  ( 31.61400995286156501, 182.3927522451417929, -10.00000000000009059 ) ) ;
#67027 = CARTESIAN_POINT ( 'NONE',  ( 115.6001716039901055, 246.7369531367911009, -4.594050593750048428 ) ) ;
#67028 = CARTESIAN_POINT ( 'NONE',  ( 180.8832283595195349, 294.1460411169432518, -2.655356583051106778 ) ) ;
#67029 = CARTESIAN_POINT ( 'NONE',  ( 167.5733982946378546, 281.7299476539893135, -10.91913693171769495 ) ) ;
#67030 = CARTESIAN_POINT ( 'NONE',  ( 157.2744851780909414, 258.2395962677452985, 18.17792129701959070 ) ) ;
#67031 = CARTESIAN_POINT ( 'NONE',  ( -27.42236680055714260, 166.5217562850347406, 1.224646799147364892E-15 ) ) ;
#67032 = APPLICATION_CONTEXT ( 'automotive_design' ) ;
#67033 = CARTESIAN_POINT ( 'NONE',  ( 32.11017034222032862, 189.3458772461660544, 9.188101187500095079 ) ) ;
#67034 = DIRECTION ( 'NONE',  ( -0.6386832404231509441, -0.7694697644498993405, 0.000000000000000000 ) ) ;
#67035 = EDGE_LOOP ( 'NONE', ( #33792, #19459, #20522, #92364 ) ) ;
#67036 = CARTESIAN_POINT ( 'NONE',  ( 190.9765749051877037, 299.0466983684623870, 7.380296417802154174 ) ) ;
#67037 = CARTESIAN_POINT ( 'NONE',  ( -13.11024591527734628, 4.999999999999999112, 17.00000000000000000 ) ) ;
#67038 = SHAPE_REPRESENTATION ( 'MAS-322', ( #62404, #5732, #57505, #62326, #75317, #13833, #44547, #890, #52649 ), #93189 ) ;
#67039 = CARTESIAN_POINT ( 'NONE',  ( 70.77272717507024424, 71.48227800853128144, -1.166185980175507897 ) ) ;
#67040 = DIRECTION ( 'NONE',  ( -0.3535533905932853327, 0.6123724356958029080, -0.7071067811865343611 ) ) ;
#67041 = CARTESIAN_POINT ( 'NONE',  ( 81.81727448962737981, 41.72775616384396358, -5.614370285570522867 ) ) ;
#67042 = VECTOR ( 'NONE', #70791, 1000.000000000000000 ) ;
#67043 = CARTESIAN_POINT ( 'NONE',  ( 12.10719531124914283, 12.15404122711131585, 8.090169943749479842 ) ) ;
#67044 = CARTESIAN_POINT ( 'NONE',  ( 66.85041857288881317, 202.7365022471902023, -10.00000000000009237 ) ) ;
#67045 = CARTESIAN_POINT ( 'NONE',  ( 182.2775398009696630, 262.7337698959310615, 12.80426946192887527 ) ) ;
#67046 = CARTESIAN_POINT ( 'NONE',  ( 97.35977185683022128, 217.0177522451417929, 5.000000000000051514 ) ) ;
#67047 = B_SPLINE_SURFACE_WITH_KNOTS ( 'NONE', 3, 1, ( 
 ( #37639, #38128 ),
 ( #53351, #44249 ),
 ( #51357, #44740 ),
 ( #83297, #90915 ),
 ( #7246, #76658 ),
 ( #5274, #12895 ),
 ( #89905, #45250 ),
 ( #75674, #29562 ),
 ( #91901, #51874 ),
 ( #97980, #68550 ),
 ( #69046, #60436 ),
 ( #59438, #58935 ),
 ( #82326, #20993 ),
 ( #67057, #20485 ),
 ( #67555, #75185 ),
 ( #82812, #43751 ),
 ( #76186, #5759 ),
 ( #36649, #6259 ),
 ( #98488, #99975 ),
 ( #68055, #98978 ),
 ( #91392, #21956 ),
 ( #29079, #36153 ),
 ( #21464, #99475 ),
 ( #22456, #52850 ),
 ( #45735, #52352 ),
 ( #13861, #83800 ),
 ( #653, #30560 ),
 ( #54842, #69552 ),
 ( #40637, #71572 ),
 ( #32036, #8261 ),
 ( #23942, #78670 ) ),
 .UNSPECIFIED., .F., .F., .F.,
 ( 4, 3, 3, 3, 3, 3, 3, 3, 3, 3, 4 ),
 ( 2, 2 ),
 ( 0.000000000000000000, 0.1122669598086620951, 0.2243161639709352062, 0.3396355846218801489, 0.4553962076584853746, 0.5677860799922156421, 0.6749047109689344515, 0.7773884377078110752, 0.8775581155833879210, 0.9782364162377753525, 1.000000000000000000 ),
 ( 0.000000000000000000, 1.000000000000000000 ),
 .UNSPECIFIED. ) ;
#67048 = VERTEX_POINT ( 'NONE', #14168 ) ;
#67049 = CARTESIAN_POINT ( 'NONE',  ( 79.23201746742374496, 59.47846325219749986, -16.53522573291430930 ) ) ;
#67050 = VECTOR ( 'NONE', #80077, 1000.000000000000000 ) ;
#67051 = CARTESIAN_POINT ( 'NONE',  ( 202.3894997978090373, 280.0980987621804275, 16.95659012541789323 ) ) ;
#67052 = CARTESIAN_POINT ( 'NONE',  ( 207.6067494229581314, 271.0615573356529353, -1.924113146155245868 ) ) ;
#67053 = ADVANCED_FACE ( 'NONE', ( #12181 ), #98790, .T. ) ;
#67054 = CARTESIAN_POINT ( 'NONE',  ( 9.836819166815537585, 185.6744531367911293, 4.594050593750047540 ) ) ;
#67055 = CARTESIAN_POINT ( 'NONE',  ( 68.40639375505929820, 68.82859656397151582, -7.014046578571599966 ) ) ;
#67056 = PLANE ( 'NONE',  #92077 ) ;
#67057 = CARTESIAN_POINT ( 'NONE',  ( 71.47511348553831567, 59.31721159656467535, -15.74457036355328476 ) ) ;
#67058 = CARTESIAN_POINT ( 'NONE',  ( 73.50077695243341225, 69.82892408322040012, 9.256215393081268061 ) ) ;
#67059 = EDGE_CURVE ( 'NONE', #47030, #95936, #84860, .T. ) ;
#67060 = FACE_OUTER_BOUND ( 'NONE', #58047, .T. ) ;
#67061 = DIRECTION ( 'NONE',  ( -0.5891075386695772131, -0.8080546441192405505, 0.000000000000000000 ) ) ;
#67062 = CARTESIAN_POINT ( 'NONE',  ( 69.82829231741662568, 69.33103082410355000, 6.611500818549685299 ) ) ;
#67063 = CARTESIAN_POINT ( 'NONE',  ( 66.07805075493222091, 68.50101230898945914, -4.678130671095277471 ) ) ;
#67064 = ORIENTED_EDGE ( 'NONE', *, *, #15275, .F. ) ;
#67065 = CARTESIAN_POINT ( 'NONE',  ( 9.692741923115793412, 189.7365022471903444, 2.944929066748280225E-16 ) ) ;
#67066 = CARTESIAN_POINT ( 'NONE',  ( 198.4198837630707715, 268.9924007542394406, -10.80133867637042222 ) ) ;
#67067 = CARTESIAN_POINT ( 'NONE',  ( 136.0064158243085046, 240.1423013555409796, -4.594050593750043987 ) ) ;
#67068 = CARTESIAN_POINT ( 'NONE',  ( 28.29779127713939602, 18.19860640527293327, 2.839279412974134775 ) ) ;
#67070 = ADVANCED_FACE ( 'NONE', ( #95080 ), #25644, .T. ) ;
#67069 = CARTESIAN_POINT ( 'NONE',  ( -19.78514814072851280, 93.11685525788735163, 59.99999999999999289 ) ) ;
#67071 = CARTESIAN_POINT ( 'NONE',  ( 80.55977923466276991, 44.53388773495297670, 11.41474457630164707 ) ) ;
#67072 = CARTESIAN_POINT ( 'NONE',  ( 198.3089799798562467, 282.2162661195332021, -17.61972112454792949 ) ) ;
#67074 = CARTESIAN_POINT ( 'NONE',  ( 189.4308808934198680, 289.8491723414206831, 15.72891001903047048 ) ) ;
#67073 = CARTESIAN_POINT ( 'NONE',  ( 157.8740713127050981, 257.2010826190796706, 17.31862062017425075 ) ) ;
#67075 = CARTESIAN_POINT ( 'NONE',  ( 68.76218780538779640, 64.26753984631646688, 12.50656271950832732 ) ) ;
#67076 = ORIENTED_EDGE ( 'NONE', *, *, #79471, .T. ) ;
#67077 = CARTESIAN_POINT ( 'NONE',  ( 151.4281781455628675, 268.3656970847310390, 15.24742929158552585 ) ) ;
#67078 = CARTESIAN_POINT ( 'NONE',  ( 164.0386046892491549, 246.5237976059514153, 8.684266124902681128 ) ) ;
#67079 = CARTESIAN_POINT ( 'NONE',  ( 171.6154833087297789, 255.2606305366970503, 12.53362356821959978 ) ) ;
#67080 = CARTESIAN_POINT ( 'NONE',  ( 193.8726876411220701, 270.8218780147767575, -13.81544579610791956 ) ) ;
#67081 = ORIENTED_EDGE ( 'NONE', *, *, #51867, .T. ) ;
#67082 = CARTESIAN_POINT ( 'NONE',  ( 71.19507340556562269, 70.62739261389883438, 5.583761667735746670 ) ) ;
#67083 = CARTESIAN_POINT ( 'NONE',  ( 171.1535303886575434, 284.5931741264590755, -11.54123640101257919 ) ) ;
#67084 = ADVANCED_FACE ( 'NONE', ( #55505 ), #37696, .T. ) ;
#67085 = CARTESIAN_POINT ( 'NONE',  ( 71.99345368292625835, 72.28405599045356666, 0.6575919626761969061 ) ) ;
#67086 = EDGE_CURVE ( 'NONE', #39924, #20199, #80024, .T. ) ;
#67087 = CARTESIAN_POINT ( 'NONE',  ( 84.79335445094056922, 44.01882294191926093, 6.915891294802152700 ) ) ;
#67088 = CARTESIAN_POINT ( 'NONE',  ( -22.42236680055709641, 157.8615022471902591, 0.000000000000000000 ) ) ;
#67089 = CARTESIAN_POINT ( 'NONE',  ( 182.9953215290649950, 295.2195952053492647, 4.704045894889287815 ) ) ;
#67090 = CARTESIAN_POINT ( 'NONE',  ( 162.9111474110223412, 248.4766108952035211, -9.702990628959184960 ) ) ;
#67091 = CARTESIAN_POINT ( 'NONE',  ( 147.8158148994058365, 275.7822056701940028, 0.001258906972079423207 ) ) ;
#67092 = CARTESIAN_POINT ( 'NONE',  ( 72.75642134338202993, 56.99959235729843954, -16.39691005310872640 ) ) ;
#67093 = ORIENTED_EDGE ( 'NONE', *, *, #35761, .T. ) ;
#67094 = DIRECTION ( 'NONE',  ( -0.9689225787001356505, 0.2473641778533816060, 0.000000000000000000 ) ) ;
#67095 = CARTESIAN_POINT ( 'NONE',  ( 10.74796456262465050, 21.90829794293879473, 10.00000000000000355 ) ) ;
#67096 = FACE_OUTER_BOUND ( 'NONE', #76700, .T. ) ;
#67097 = ORIENTED_EDGE ( 'NONE', *, *, #2974, .F. ) ;
#67098 = CARTESIAN_POINT ( 'NONE',  ( 73.99760485042780545, 55.07988560541686951, 16.60354421704504801 ) ) ;
#67099 = CARTESIAN_POINT ( 'NONE',  ( 86.40472769894839189, 47.00022269315729773, -10.52150423465796436 ) ) ;
#67100 = CARTESIAN_POINT ( 'NONE',  ( 156.3480092461931861, 261.3368746170128816, -17.50703484634064111 ) ) ;
#67101 = ORIENTED_EDGE ( 'NONE', *, *, #25376, .T. ) ;
#67102 = CARTESIAN_POINT ( 'NONE',  ( -17.42236680055705023, 149.2012482093457777, 0.000000000000000000 ) ) ;
#67103 = CARTESIAN_POINT ( 'NONE',  ( 185.3708565686441716, 291.1367641197661555, 12.05567508508808672 ) ) ;
#67104 = CARTESIAN_POINT ( 'NONE',  ( 204.5730103890532519, 276.3161474792809145, 14.88139715235883109 ) ) ;
#67105 = CARTESIAN_POINT ( 'NONE',  ( 57.68498304950353628, 194.1115022471902023, -5.000000000000041744 ) ) ;
#67106 = ORIENTED_EDGE ( 'NONE', *, *, #69031, .T. ) ;
#67107 = CARTESIAN_POINT ( 'NONE',  ( 79.55186417146283873, 225.9244531367911293, -4.594050593750046652 ) ) ;
#67108 = CARTESIAN_POINT ( 'NONE',  ( 198.6931026323153162, 282.8313882593000130, 17.63783808752309668 ) ) ;
#67109 = CARTESIAN_POINT ( 'NONE',  ( 181.3220768623721710, 271.3444700680324218, -16.03098847413529526 ) ) ;
#67110 = CYLINDRICAL_SURFACE ( 'NONE', #91454, 17.82106496071139645 ) ;
#67111 = VERTEX_POINT ( 'NONE', #88901 ) ;
#67112 = ADVANCED_FACE ( 'NONE', ( #2753 ), #53888, .F. ) ;
#67113 = ORIENTED_EDGE ( 'NONE', *, *, #69198, .T. ) ;
#67114 = CARTESIAN_POINT ( 'NONE',  ( 207.1181895030469491, 269.9077679394811753, 1.745611964362854929 ) ) ;
#67115 = ORIENTED_EDGE ( 'NONE', *, *, #72157, .F. ) ;
#67116 = LINE ( 'NONE', #90480, #20743 ) ;
#67117 = PRESENTATION_LAYER_ASSIGNMENT (  '', '', ( #99461 ) ) ;
#67118 = ORIENTED_EDGE ( 'NONE', *, *, #87242, .F. ) ;
#67119 = CARTESIAN_POINT ( 'NONE',  ( 75.75188460778494459, 62.48029762007487165, 15.10107052133506578 ) ) ;
#67120 = CARTESIAN_POINT ( 'NONE',  ( 203.3041373168503299, 278.5139001086923827, -16.61929732091214973 ) ) ;
#67121 = ORIENTED_EDGE ( 'NONE', *, *, #54311, .F. ) ;
#67122 = EDGE_CURVE ( 'NONE', #27651, #87546, #44077, .T. ) ;
#67123 = CARTESIAN_POINT ( 'NONE',  ( 182.7847760313759409, 280.0284915794045446, -17.53211380394024843 ) ) ;
#67124 = CARTESIAN_POINT ( 'NONE',  ( 178.1281481821618797, 292.9991590599575488, -6.064681374715556572 ) ) ;
#67125 = CARTESIAN_POINT ( 'NONE',  ( -23.57381662850335147, 99.72943373905189901, 45.19944339805625333 ) ) ;
#67126 = EDGE_CURVE ( 'NONE', #63881, #58975, #46221, .T. ) ;
#67127 = CIRCLE ( 'NONE', #63878, 70.00000000000001421 ) ;
#67128 = CARTESIAN_POINT ( 'NONE',  ( 71.30800587088177167, 68.37826660670813794, -9.385020971228579256 ) ) ;
#67129 = EDGE_CURVE ( 'NONE', #32333, #30740, #81289, .T. ) ;
#67130 = CARTESIAN_POINT ( 'NONE',  ( 164.7913975190338078, 265.1675190917550822, -16.61937175513660492 ) ) ;
#67131 = VERTEX_POINT ( 'NONE', #23274 ) ;
#67132 = CARTESIAN_POINT ( 'NONE',  ( 76.63225857491576676, 59.44759824736555487, 15.94375019732647125 ) ) ;
#67133 = CARTESIAN_POINT ( 'NONE',  ( 6.417452267959404821, 25.74646525600388003, 2.839279412974139660 ) ) ;
#67134 = ORIENTED_EDGE ( 'NONE', *, *, #71824, .T. ) ;
#67135 = EDGE_CURVE ( 'NONE', #92664, #28922, #34062, .T. ) ;
#67136 = CARTESIAN_POINT ( 'NONE',  ( 167.4788697440488932, 284.1975178938891418, 9.214407018017913842 ) ) ;
#67138 = ORIENTED_EDGE ( 'NONE', *, *, #10119, .T. ) ;
#67137 = CARTESIAN_POINT ( 'NONE',  ( 199.8955426817768455, 270.2827091269795119, 9.689898955748889264 ) ) ;
#67139 = EDGE_CURVE ( 'NONE', #62095, #40534, #57004, .T. ) ;
#67140 = CARTESIAN_POINT ( 'NONE',  ( 202.3139361598622372, 280.2289788223093865, 15.93832709035092421 ) ) ;
#67141 = EDGE_CURVE ( 'NONE', #27033, #61969, #75154, .T. ) ;
#67142 = CARTESIAN_POINT ( 'NONE',  ( 206.8106726053982811, 272.4404028303941914, -10.47827087991598560 ) ) ;
#67143 = CARTESIAN_POINT ( 'NONE',  ( 149.2575837200583067, 276.2297180982410509, -5.451514945794049716 ) ) ;
#67144 = CARTESIAN_POINT ( 'NONE',  ( 165.0940603251445680, 246.6293290676431127, -1.873067877571933826 ) ) ;
#67145 = CARTESIAN_POINT ( 'NONE',  ( 185.8626946602280441, 259.3471889805154547, 7.308832903665572367 ) ) ;
#67146 = CARTESIAN_POINT ( 'NONE',  ( 86.88629399543513898, 44.27340696768450812, 4.932537521029398242 ) ) ;
#67147 = CARTESIAN_POINT ( 'NONE',  ( 88.33748333995926316, 44.07075497373336503, -2.898134731201835290 ) ) ;
#67148 = ORIENTED_EDGE ( 'NONE', *, *, #70341, .F. ) ;
#67149 = CARTESIAN_POINT ( 'NONE',  ( 181.8041777747191645, 271.4364937356251062, -15.98274022405578343 ) ) ;
#67150 = CARTESIAN_POINT ( 'NONE',  ( 28.00427808217458647, 41.79349426999503692, 10.00000000000000000 ) ) ;
#67151 = ORIENTED_EDGE ( 'NONE', *, *, #86727, .T. ) ;
#67152 = CARTESIAN_POINT ( 'NONE',  ( 193.2165179683147471, 294.2034512776308475, -14.44099136285982254 ) ) ;
#67153 = DIRECTION ( 'NONE',  ( -0.5000000000000001110, 0.8660254037844384856, 0.000000000000000000 ) ) ;
#67154 = CARTESIAN_POINT ( 'NONE',  ( 45.56181175559623142, 118.5014625327306135, 177.5919119679930134 ) ) ;
#67155 = CARTESIAN_POINT ( 'NONE',  ( 85.30422478396575059, 44.62533895320201083, -7.491170275040920146 ) ) ;
#67156 = CARTESIAN_POINT ( 'NONE',  ( 164.3560589188577410, 274.2738242027600677, 14.76370921553832360 ) ) ;
#67158 = CARTESIAN_POINT ( 'NONE',  ( 87.81592712917142762, 44.13559768126560812, 2.731183658606283871 ) ) ;
#67157 = CARTESIAN_POINT ( 'NONE',  ( -3.992090130160959482, 162.3768266524160140, 9.188101187500098632 ) ) ;
#67159 = AXIS2_PLACEMENT_3D ( 'NONE', #60470, #37674, #53383 ) ;
#67160 = DIRECTION ( 'NONE',  ( -0.000000000000000000, -1.000000000000000000, -0.000000000000000000 ) ) ;
#67161 = EDGE_LOOP ( 'NONE', ( #1831, #59914, #99781, #36723 ) ) ;
#67162 = ORIENTED_EDGE ( 'NONE', *, *, #112, .T. ) ;
#67163 = DIRECTION ( 'NONE',  ( -0.8660254037844387076, -0.4999999999999998890, -0.000000000000000000 ) ) ;
#67164 = CARTESIAN_POINT ( 'NONE',  ( 190.0738558021110691, 273.7331793950331758, -15.69528651041143519 ) ) ;
#67165 = CARTESIAN_POINT ( 'NONE',  ( 85.72965280032694579, 48.53761792183082946, -12.28028246049512973 ) ) ;
#67166 = DIRECTION ( 'NONE',  ( -0.000000000000000000, -0.000000000000000000, -1.000000000000000000 ) ) ;
#67167 = CARTESIAN_POINT ( 'NONE',  ( 86.56321455801250409, 43.53278834282398435, 3.082621468869548575 ) ) ;
#67168 = CARTESIAN_POINT ( 'NONE',  ( -19.65312891409030271, 93.06504152958497400, 10.00000000000000888 ) ) ;
#67169 = CARTESIAN_POINT ( 'NONE',  ( 166.7187202459675746, 278.5591580196478958, -14.78021074750266273 ) ) ;
#67170 = CARTESIAN_POINT ( 'NONE',  ( 5.669592554750444435, 164.8923013555410080, 4.594050593750050204 ) ) ;
#67171 = CARTESIAN_POINT ( 'NONE',  ( 109.2678814824639204, 224.7048013555410080, 4.594050593750051981 ) ) ;
#67172 = CARTESIAN_POINT ( 'NONE',  ( 40.06571587503326271, 205.4860189848785694, -2.679491924311252493 ) ) ;
#67173 = CARTESIAN_POINT ( 'NONE',  ( 186.6662094383440262, 296.0905088883881149, -7.390743538549633840 ) ) ;
#67174 = CARTESIAN_POINT ( 'NONE',  ( 78.31378090380852086, 52.71380825594539488, 15.69171095534893290 ) ) ;
#67175 = CARTESIAN_POINT ( 'NONE',  ( 176.6301829438279185, 282.3654047892467815, -14.24849079710228139 ) ) ;
#67176 = CARTESIAN_POINT ( 'NONE',  ( 80.81957833366946886, 53.31777243922379483, -15.54131231963324744 ) ) ;
#67177 = CARTESIAN_POINT ( 'NONE',  ( 193.7999837595647250, 294.9755769528473479, 15.24609078262870199 ) ) ;
#67178 = CARTESIAN_POINT ( 'NONE',  ( 184.1472144282555519, 274.8408247889214522, 16.39501531948747015 ) ) ;
#67179 = CARTESIAN_POINT ( 'NONE',  ( 194.3708539535661259, 293.9868007723104029, -16.01585187499628304 ) ) ;
#67180 = DIRECTION ( 'NONE',  ( -0.5369817302126890235, 0.8435938723211464652, 0.000000000000000000 ) ) ;
#67181 = CARTESIAN_POINT ( 'NONE',  ( 84.14087309183582875, 50.46766762800921668, 13.73480842938780278 ) ) ;
#67182 = CARTESIAN_POINT ( 'NONE',  ( 187.1286666404986363, 298.8789080593439280, -0.5945842851373613902 ) ) ;
#67183 = CARTESIAN_POINT ( 'NONE',  ( 47.29267820409018697, 208.1115022471903160, -5.000000000000047962 ) ) ;
#67184 = CARTESIAN_POINT ( 'NONE',  ( 184.2717516226944952, 268.6604825781803356, -15.25338787826597198 ) ) ;
#67185 = AXIS2_PLACEMENT_3D ( 'NONE', #90076, #27746, #12552 ) ;
#67186 = LINE ( 'NONE', #5893, #86959 ) ;
#67187 = CYLINDRICAL_SURFACE ( 'NONE', #33605, 16.60714546451156792 ) ;
#67188 = CARTESIAN_POINT ( 'NONE',  ( 84.74801659416949917, 228.9244531367911293, -4.594050593750046652 ) ) ;
#67189 = CARTESIAN_POINT ( 'NONE',  ( 3.104905098483929482, 23.83396525600387506, -2.839279412974133887 ) ) ;
#67191 = EDGE_CURVE ( 'NONE', #33084, #74024, #9091, .T. ) ;
#67190 = CARTESIAN_POINT ( 'NONE',  ( 156.6812872898450735, 261.2670451491295012, 0.000000000000000000 ) ) ;
#67192 = CARTESIAN_POINT ( 'NONE',  ( 159.0119062629668747, 259.2772906885834345, -17.27827472792992580 ) ) ;
#67194 = CARTESIAN_POINT ( 'NONE',  ( 200.2925563156679800, 283.7301114138494427, 18.37231090996849048 ) ) ;
#67193 = CARTESIAN_POINT ( 'NONE',  ( 196.1573359623355088, 290.8925231663144473, 17.55680092534192482 ) ) ;
#67195 = B_SPLINE_CURVE_WITH_KNOTS ( 'NONE', 3,
 ( #49458, #89044, #11492, #10984, #73769, #19590, #73275, #34264, #81900, #88527, #35255, #81404, #41348, #11974, #19087, #66163, #97108, #12477, #43344, #56557, #87544, #33790, #52939, #14928, #76268, #4876, #51450, #44340, #67149, #60032, #37242, #74293, #90509, #82419, #68140, #35757, #68636, #98071, #75768, #66655, #6356, #30140, #12984, #60526, #36243, #14455, #36739, #99068, #29161, #99557, #61024, #75269 ),
 .UNSPECIFIED., .F., .F.,
 ( 4, 2, 2, 2, 2, 2, 2, 2, 2, 2, 2, 2, 2, 2, 2, 2, 2, 2, 2, 2, 2, 2, 2, 2, 2, 4 ),
 ( 0.0001034768661984681600, 0.001103434164929440256, 0.001353423489612237988, 0.001603412814295035720, 0.001728407476636464402, 0.001853402138977892650, 0.001978396801319321115, 0.002103391463660749579, 0.002353380788343550998, 0.002603370113026352850, 0.003103348762392025510, 0.004103306061123445855, 0.005103263359854866635, 0.005603242009220577025, 0.005853231333903432219, 0.005978225996244816882, 0.006103220658586201545, 0.006165717989756862652, 0.006228215320927522891, 0.006353209983268867656, 0.006603199307951555450, 0.006853188632634243244, 0.007103177957316931905, 0.007353167281999618832, 0.007603156606682307493, 0.008103135256047678744 ),
 .UNSPECIFIED. ) ;
#67196 = CARTESIAN_POINT ( 'NONE',  ( 149.6188047043597180, 271.4996238147605823, 11.68007032781935628 ) ) ;
#67197 = B_SPLINE_CURVE_WITH_KNOTS ( 'NONE', 3,
 ( #41292, #17509, #78831, #32706 ),
 .UNSPECIFIED., .F., .F.,
 ( 4, 4 ),
 ( 0.009381926372693255231, 0.01459774425476862911 ),
 .UNSPECIFIED. ) ;
#67198 = CARTESIAN_POINT ( 'NONE',  ( 151.2567985338353935, 268.6625352796243646, -15.71756535662528798 ) ) ;
#67199 = CARTESIAN_POINT ( 'NONE',  ( -58.62427208439002158, 70.56504152958493137, -45.00000000000001421 ) ) ;
#67200 = CARTESIAN_POINT ( 'NONE',  ( 43.33837710268888088, 27.94754757982093096, 5.678558825948272215 ) ) ;
#67201 = CARTESIAN_POINT ( 'NONE',  ( 146.7944005049231180, 276.3916353892955726, -4.243051111306586520 ) ) ;
#67202 = FACE_BOUND ( 'NONE', #46392, .T. ) ;
#67203 = ORIENTED_EDGE ( 'NONE', *, *, #92811, .T. ) ;
#67204 = CARTESIAN_POINT ( 'NONE',  ( 16.58664519722142927, 32.68290643055186706, 3.479690158560446702E-15 ) ) ;
#67205 = DIRECTION ( 'NONE',  ( -0.9974094913373522386, -0.07193265315671491800, 0.000000000000000000 ) ) ;
#67206 = CARTESIAN_POINT ( 'NONE',  ( -40.60196443811259570, 67.26451206140657746, -10.00000000000000000 ) ) ;
#67207 = CARTESIAN_POINT ( 'NONE',  ( 191.7076580884861414, 287.9117833154688242, -15.84525881108999101 ) ) ;
#67208 = EDGE_CURVE ( 'NONE', #53616, #74626, #87434, .T. ) ;
#67209 = EDGE_CURVE ( 'NONE', #48279, #88645, #95237, .T. ) ;
#67210 = DIRECTION ( 'NONE',  ( 0.3213938048432692374, -0.5566703992264209200, -0.7660444431189770143 ) ) ;
#67211 = CARTESIAN_POINT ( 'NONE',  ( 198.5558597050348908, 286.7381581807989051, 17.16554469393394200 ) ) ;
#67212 = CARTESIAN_POINT ( 'NONE',  ( 181.0931619117654634, 256.6297595461512060, 7.400322454308797759 ) ) ;
#67213 = LINE ( 'NONE', #5919, #98660 ) ;
#67214 = CARTESIAN_POINT ( 'NONE',  ( 75.04705542663356255, 53.02407537203858823, -16.49187436516719529 ) ) ;
#67215 = CARTESIAN_POINT ( 'NONE',  ( 134.2560625007776025, 254.9865022471903444, -10.00000000000009415 ) ) ;
#67216 = EDGE_LOOP ( 'NONE', ( #72644, #57014, #51426, #25512 ) ) ;
#67217 = CARTESIAN_POINT ( 'NONE',  ( 71.81491595147093676, 67.99074982944202361, 10.79843746604593413 ) ) ;
#67218 = ORIENTED_EDGE ( 'NONE', *, *, #47331, .F. ) ;
#67219 = CARTESIAN_POINT ( 'NONE',  ( 196.9612820325353368, 264.9694946870639569, -4.623214399652447959 ) ) ;
#67220 = CARTESIAN_POINT ( 'NONE',  ( 82.89008403434760908, 41.16675059735047171, 0.2050283597234445476 ) ) ;
#67221 = ORIENTED_EDGE ( 'NONE', *, *, #39507, .F. ) ;
#67222 = CARTESIAN_POINT ( 'NONE',  ( 86.43538639504456000, 43.24186732757627993, 1.603548621781322625 ) ) ;
#67223 = VERTEX_POINT ( 'NONE', #10095 ) ;
#67224 = CARTESIAN_POINT ( 'NONE',  ( -2.590881078880516331, 25.17631125121047475, -10.00000000000000000 ) ) ;
#67225 = CARTESIAN_POINT ( 'NONE',  ( 158.6379490615327938, 255.8780075473385125, 17.62002732432160812 ) ) ;
#67226 = CARTESIAN_POINT ( 'NONE',  ( 148.0493212738620628, 256.2833772461660828, -9.188101187500095079 ) ) ;
#67227 = CARTESIAN_POINT ( 'NONE',  ( 153.6741866004717849, 264.4754963265993979, -18.11073193088522260 ) ) ;
#67228 = CARTESIAN_POINT ( 'NONE',  ( 152.9607371460978129, 265.7112270302071124, -16.17698032818104537 ) ) ;
#67229 = AXIS2_PLACEMENT_3D ( 'NONE', #96241, #26801, #57685 ) ;
#67230 = CARTESIAN_POINT ( 'NONE',  ( 34.67813663163181559, 40.99752408145594984, 5.678558825948276656 ) ) ;
#67231 = CARTESIAN_POINT ( 'NONE',  ( -19.65312891409030271, 93.06504152958497400, 10.00000000000000888 ) ) ;
#67232 = CARTESIAN_POINT ( 'NONE',  ( 164.6704117653912078, 274.4925094543679052, 14.73674799813685965 ) ) ;
#67234 = AXIS2_PLACEMENT_3D ( 'NONE', #46182, #52794, #7704 ) ;
#67233 = CARTESIAN_POINT ( 'NONE',  ( 64.97403019802248991, 214.9865022471903160, 10.00000000000009415 ) ) ;
#67235 = ORIENTED_EDGE ( 'NONE', *, *, #43248, .T. ) ;
#67236 = VERTEX_POINT ( 'NONE', #41468 ) ;
#67237 = CARTESIAN_POINT ( 'NONE',  ( 87.20542010897281671, 46.22683608894070062, -9.058801420718495478 ) ) ;
#67238 = ADVANCED_FACE ( 'NONE', ( #18198 ), #34385, .T. ) ;
#67240 = CARTESIAN_POINT ( 'NONE',  ( 162.2660344477049819, 272.4068407072390983, -16.13375623211421583 ) ) ;
#67239 = CARTESIAN_POINT ( 'NONE',  ( 164.3010377730689981, 246.0692501711882869, 7.247566249275159578 ) ) ;
#67241 = CARTESIAN_POINT ( 'NONE',  ( 195.6664450926536460, 278.3245960621525796, 17.18455885460583232 ) ) ;
#67242 = CARTESIAN_POINT ( 'NONE',  ( 194.0672051292551430, 294.5127359636757660, 15.53337744471869364 ) ) ;
#67243 = CARTESIAN_POINT ( 'NONE',  ( 74.40936191869957383, 60.98710938593095676, -15.30741647548370921 ) ) ;
#67244 = CARTESIAN_POINT ( 'NONE',  ( 147.6220714307702622, 274.9580672937808572, 8.392894244419288441 ) ) ;
#67245 = CARTESIAN_POINT ( 'NONE',  ( 167.2717594564306296, 286.8017429457753451, -4.937469463271268566 ) ) ;
#67246 = CARTESIAN_POINT ( 'NONE',  ( 77.03696703343622687, 62.90724515748721757, -15.26905322870460502 ) ) ;
#67247 = CARTESIAN_POINT ( 'NONE',  ( 178.1826077084033102, 255.5164715494353516, 4.895996780289697092 ) ) ;
#67248 = EDGE_CURVE ( 'NONE', #6051, #18914, #63783, .T. ) ;
#67249 = CARTESIAN_POINT ( 'NONE',  ( 101.1213961584103060, 235.3149278399160949, -9.188101187500095079 ) ) ;
#67250 = ORIENTED_EDGE ( 'NONE', *, *, #47420, .F. ) ;
#67251 = CARTESIAN_POINT ( 'NONE',  ( 173.0837253472800796, 264.8280141993791972, 17.07053884509587860 ) ) ;
#67252 = CARTESIAN_POINT ( 'NONE',  ( 165.3763302323083053, 271.0598910717424701, 16.49088855851117685 ) ) ;
#67253 = CARTESIAN_POINT ( 'NONE',  ( 190.3288472781666201, 274.6029090957763401, 15.82415357830627833 ) ) ;
#67254 = VERTEX_POINT ( 'NONE', #57670 ) ;
#67255 = AXIS2_PLACEMENT_3D ( 'NONE', #94229, #25283, #79022 ) ;
#67256 = VERTEX_POINT ( 'NONE', #57169 ) ;
#67257 = CARTESIAN_POINT ( 'NONE',  ( 87.06454106189060838, 46.38688501933356179, -8.729080971554649793 ) ) ;
#67258 = EDGE_CURVE ( 'NONE', #18732, #68256, #60570, .T. ) ;
#67259 = CARTESIAN_POINT ( 'NONE',  ( 180.7412255709484157, 294.1235929814394012, -2.454474088018941735 ) ) ;
#67260 = CARTESIAN_POINT ( 'NONE',  ( 196.3720681610792553, 290.5205960880691691, 16.18360420724715354 ) ) ;
#67261 = CARTESIAN_POINT ( 'NONE',  ( 190.2925905131754973, 300.4452873534128230, -0.07860713051909268279 ) ) ;
#67262 = CARTESIAN_POINT ( 'NONE',  ( -46.49770490450612215, 29.77544742692501600, 10.00000000000000000 ) ) ;
#67263 = ORIENTED_EDGE ( 'NONE', *, *, #23403, .F. ) ;
#67264 = VECTOR ( 'NONE', #88289, 1000.000000000000114 ) ;
#67265 = VERTEX_POINT ( 'NONE', #13100 ) ;
#67266 = CARTESIAN_POINT ( 'NONE',  ( 207.7837159184916231, 270.7550423741513441, -2.369602332675663448 ) ) ;
#67267 = ORIENTED_EDGE ( 'NONE', *, *, #51786, .T. ) ;
#67268 = CARTESIAN_POINT ( 'NONE',  ( -19.65312891409030271, 93.06504152958497400, 10.00000000000000888 ) ) ;
#67269 = CARTESIAN_POINT ( 'NONE',  ( 153.2595589010950334, 265.6112048380699093, 16.12693562537618419 ) ) ;
#67270 = DIRECTION ( 'NONE',  ( 0.5864613938488598688, -0.8099771808667527440, 0.000000000000000000 ) ) ;
#67272 = CARTESIAN_POINT ( 'NONE',  ( 69.39665958681418090, 62.79313245896668860, -13.73716500047468969 ) ) ;
#67271 = CARTESIAN_POINT ( 'NONE',  ( 184.3063639896893164, 288.6967878748712337, -13.31555908468126503 ) ) ;
#67273 = DIRECTION ( 'NONE',  ( -0.9538480676139692305, 0.3002896333693469422, 0.000000000000000000 ) ) ;
#67274 = ORIENTED_EDGE ( 'NONE', *, *, #61318, .F. ) ;
#67275 = CARTESIAN_POINT ( 'NONE',  ( 58.48430016207534976, 216.1199935810940929, 2.679491924311251605 ) ) ;
#67276 = B_SPLINE_CURVE_WITH_KNOTS ( 'NONE', 3,
 ( #83526, #44975, #29300, #91614 ),
 .UNSPECIFIED., .F., .F.,
 ( 4, 4 ),
 ( 0.04432367838347623518, 0.04887066958154932111 ),
 .UNSPECIFIED. ) ;
#67277 = CARTESIAN_POINT ( 'NONE',  ( 62.44812277031795134, 196.8615022471901739, 5.000000000000051514 ) ) ;
#67278 = CARTESIAN_POINT ( 'NONE',  ( 82.61675266362445313, 40.93810794203632497, -3.632981533375318595 ) ) ;
#67279 = CARTESIAN_POINT ( 'NONE',  ( 192.9108229344522840, 270.9309780692502159, 14.84737179462503676 ) ) ;
#67280 = CARTESIAN_POINT ( 'NONE',  ( 116.0695290213043620, 244.4865022471902876, -10.00000000000009592 ) ) ;
#67281 = CARTESIAN_POINT ( 'NONE',  ( 71.98582063699875278, 72.29727681381652360, 3.337216071139553542 ) ) ;
#67282 = CARTESIAN_POINT ( 'NONE',  ( 195.5549742635668622, 279.7421760486213884, -16.96403059063067431 ) ) ;
#67283 = CARTESIAN_POINT ( 'NONE',  ( 71.94941146435354540, 134.4047874917408478, -22.49999999999983658 ) ) ;
#67284 = CARTESIAN_POINT ( 'NONE',  ( 80.94861998693302496, 55.71865610027163029, 16.05787193106602118 ) ) ;
#67285 = CARTESIAN_POINT ( 'NONE',  ( 68.99683503679369778, 70.12789505165764581, -3.015407314609216183 ) ) ;
#67286 = CARTESIAN_POINT ( 'NONE',  ( 69.24135662524314228, 198.5327760586659451, 1.948934522072303157E-15 ) ) ;
#67287 = CARTESIAN_POINT ( 'NONE',  ( 206.5081929095101998, 272.9643130319303737, -9.215516226794479238 ) ) ;
#67288 = CARTESIAN_POINT ( 'NONE',  ( 77.72420466810140738, 61.55156736199941037, 16.09483585134336536 ) ) ;
#67289 = CARTESIAN_POINT ( 'NONE',  ( 208.0006710756887287, 270.3792650189220126, -0.8737665032493013850 ) ) ;
#67290 = ADVANCED_FACE ( 'NONE', ( #13587 ), #44461, .T. ) ;
#67291 = DIRECTION ( 'NONE',  ( -0.5000000000000003331, 0.8660254037844383745, -9.251858538542983907E-17 ) ) ;
#67292 = VECTOR ( 'NONE', #20974, 1000.000000000000000 ) ;
#67293 = CARTESIAN_POINT ( 'NONE',  ( 207.8792014703394671, 270.5896565469619759, -5.780233892547864905 ) ) ;
#67294 = FACE_OUTER_BOUND ( 'NONE', #15540, .T. ) ;
#67296 = CARTESIAN_POINT ( 'NONE',  ( 185.8891070060977881, 265.5474094253055455, 13.37913739288876158 ) ) ;
#67295 = CARTESIAN_POINT ( 'NONE',  ( 73.43921776615482599, 70.07059797397528200, -9.512040028895288657 ) ) ;
#67297 = CARTESIAN_POINT ( 'NONE',  ( 6.214053113703209341, 25.36126292948893379, 6.180339887498949913 ) ) ;
#67298 = CARTESIAN_POINT ( 'NONE',  ( 36.03590635313024393, 36.50829794293883168, -10.00000000000000355 ) ) ;
#67299 = CARTESIAN_POINT ( 'NONE',  ( 78.26099034771921481, 56.73960120100890236, -16.61664413875233492 ) ) ;
#67300 = CARTESIAN_POINT ( 'NONE',  ( 157.7666006523658666, 270.6297847174233766, -15.52481408403261298 ) ) ;
#67301 = VECTOR ( 'NONE', #43823, 1000.000000000000000 ) ;
#67302 = CARTESIAN_POINT ( 'NONE',  ( 72.01901178328436970, 72.02624153141685781, 2.845887144479070319 ) ) ;
#67303 = CARTESIAN_POINT ( 'NONE',  ( 27.99689677000926125, 174.7202760586659736, -5.415160957724236172E-17 ) ) ;
#67304 = CARTESIAN_POINT ( 'NONE',  ( 157.8360072705708603, 257.2670114739976839, 17.12122855844125269 ) ) ;
#67306 = EDGE_CURVE ( 'NONE', #23235, #73362, #78735, .T. ) ;
#67305 = CARTESIAN_POINT ( 'NONE',  ( -71.61465314115659453, 63.06504152958490295, 20.00000000000001776 ) ) ;
#67307 = CARTESIAN_POINT ( 'NONE',  ( 194.3177355571849318, 294.0788045336591381, -15.93712594727561616 ) ) ;
#67308 = CARTESIAN_POINT ( 'NONE',  ( 71.90447592081905270, 72.59379857415109427, -1.170934825568553439 ) ) ;
#67309 = CARTESIAN_POINT ( 'NONE',  ( 43.28705038798948124, 204.9869531367911293, 4.594050593750046652 ) ) ;
#67310 = CARTESIAN_POINT ( 'NONE',  ( 26.01786902700012405, 17.94754757982089899, 5.678558825948272215 ) ) ;
#67311 = CARTESIAN_POINT ( 'NONE',  ( 171.3082047287566922, 286.6656704798778037, 7.347939393563489574 ) ) ;
#67312 = CARTESIAN_POINT ( 'NONE',  ( -8.669243101527598583, 25.19333184544593252, 10.00000000000000000 ) ) ;
#67313 = CARTESIAN_POINT ( 'NONE',  ( 37.67689025969888661, 40.49103043416553049, -8.090169943749479842 ) ) ;
#67314 = CARTESIAN_POINT ( 'NONE',  ( 172.8951663193395234, 288.9549776225803157, 8.104654168245465584 ) ) ;
#67315 = CARTESIAN_POINT ( 'NONE',  ( 175.7518161566136996, 291.0577149723374077, 2.541557124732606976 ) ) ;
#67316 = CARTESIAN_POINT ( 'NONE',  ( 180.0693756861613508, 276.3240737636226072, 16.71396866487755517 ) ) ;
#67317 = CARTESIAN_POINT ( 'NONE',  ( 82.18753490691527475, 40.78579184768808830, -0.6546124752527386903 ) ) ;
#67318 = CARTESIAN_POINT ( 'NONE',  ( 69.83940448949712732, 67.89019746407828393, -8.846351444184202606 ) ) ;
#67319 = CARTESIAN_POINT ( 'NONE',  ( 191.9987047080313687, 267.0019276258636864, 10.95647444719745067 ) ) ;
#67320 = EDGE_CURVE ( 'NONE', #44730, #16478, #35873, .T. ) ;
#67321 = VECTOR ( 'NONE', #45490, 1000.000000000000227 ) ;
#67322 = EDGE_CURVE ( 'NONE', #38047, #26159, #83603, .T. ) ;
#67323 = DIRECTION ( 'NONE',  ( -0.9839629614562445115, 0.1783728972749415165, 0.000000000000000000 ) ) ;
#67324 = CARTESIAN_POINT ( 'NONE',  ( 87.74659634842467426, 45.27479573043824246, -7.097702524348068920 ) ) ;
#67326 =( BOUNDED_CURVE ( )  B_SPLINE_CURVE ( 2, ( #91517, #97141, #50484, #4392, #27710, #43381, #13508, #97621, #29200 ),
 .UNSPECIFIED., .F., .T. ) 
 B_SPLINE_CURVE_WITH_KNOTS ( ( 3, 2, 2, 2, 3 ),
 ( 0.5927419354838709964, 0.5940860215053763715, 0.5967741935483871218, 0.5994623655913978721, 0.6008064516129032473 ),
 .UNSPECIFIED. ) 
 CURVE ( )  GEOMETRIC_REPRESENTATION_ITEM ( )  RATIONAL_B_SPLINE_CURVE ( ( 0.9330127018922194093, 0.9330127018922194093, 1.000000000000000000, 0.8660254037844387076, 1.000000000000000000, 0.8660254037844387076, 1.000000000000000000, 0.9330127018922194093, 0.9330127018922194093 ) ) 
 REPRESENTATION_ITEM ( '' )  );
#67325 = CARTESIAN_POINT ( 'NONE',  ( 103.1513167481865310, 230.3615022471902591, -10.00000000000009592 ) ) ;
#67327 = CARTESIAN_POINT ( 'NONE',  ( 200.1782072557437857, 283.9281697954355650, 18.05177561285849208 ) ) ;
#67328 = CARTESIAN_POINT ( 'NONE',  ( 164.3266432466909635, 269.1343096826732335, -16.34300100545284806 ) ) ;
#67329 = ORIENTED_EDGE ( 'NONE', *, *, #68019, .T. ) ;
#67330 = CARTESIAN_POINT ( 'NONE',  ( 65.53359859134977228, 199.4548013555410080, -4.594050593750042211 ) ) ;
#67331 = ORIENTED_EDGE ( 'NONE', *, *, #3345, .F. ) ;
#67332 = CARTESIAN_POINT ( 'NONE',  ( 163.7906117146278007, 264.0004031999091580, 16.81624561942971141 ) ) ;
#67333 = CARTESIAN_POINT ( 'NONE',  ( 190.1607982559816890, 301.2788311432216233, -4.972636536415983244 ) ) ;
#67334 = CYLINDRICAL_SURFACE ( 'NONE', #88839, 10.00000000000010658 ) ;
#67335 = VERTEX_POINT ( 'NONE', #55055 ) ;
#67336 = DIRECTION ( 'NONE',  ( 0.4999999999999998890, -0.8660254037844385966, 0.000000000000000000 ) ) ;
#67337 = CARTESIAN_POINT ( 'NONE',  ( 79.07401460044036412, 46.11122150352828442, -12.69419382828625054 ) ) ;
#67338 = FACE_OUTER_BOUND ( 'NONE', #29758, .T. ) ;
#67339 = CARTESIAN_POINT ( 'NONE',  ( 189.1123083253427524, 265.5175477926164262, 10.65947824442831582 ) ) ;
#67340 = CARTESIAN_POINT ( 'NONE',  ( 149.2223635749290622, 272.1862799931444670, -12.97307652490353647 ) ) ;
#67341 = CARTESIAN_POINT ( 'NONE',  ( 157.4493702961534609, 257.9366863577731124, 17.30941950273115637 ) ) ;
#67342 = ORIENTED_EDGE ( 'NONE', *, *, #91626, .T. ) ;
#67343 = CARTESIAN_POINT ( 'NONE',  ( 16.63655203261577498, 31.64646525600389637, -2.839279412974133887 ) ) ;
#67344 = CARTESIAN_POINT ( 'NONE',  ( 76.27123136624052790, 61.69503254033130446, 15.45961916291305194 ) ) ;
#67345 = CARTESIAN_POINT ( 'NONE',  ( 69.85412049919082733, 70.10641299775195989, -4.912549986004115965 ) ) ;
#67346 = CARTESIAN_POINT ( 'NONE',  ( 15.68275096595825246, 169.8615022471901739, 5.000000000000051514 ) ) ;
#67347 = ORIENTED_EDGE ( 'NONE', *, *, #16992, .F. ) ;
#67348 = CARTESIAN_POINT ( 'NONE',  ( -162.0327448629461742, 33.95614270198240803, -21.50000000000000000 ) ) ;
#67349 = CARTESIAN_POINT ( 'NONE',  ( 206.1615484827472358, 273.5647187912443314, -9.556459874778100883 ) ) ;
#67350 = ORIENTED_EDGE ( 'NONE', *, *, #16849, .F. ) ;
#67351 = EDGE_CURVE ( 'NONE', #42396, #20252, #53560, .T. ) ;
#67353 = CARTESIAN_POINT ( 'NONE',  ( 167.6278246310154714, 282.5728663012718584, -12.21306354836790220 ) ) ;
#67352 = CARTESIAN_POINT ( 'NONE',  ( 159.9700686533283545, 282.3153680940349091, -3.195712497083830428 ) ) ;
#67354 = B_SPLINE_CURVE_WITH_KNOTS ( 'NONE', 3,
 ( #99994, #94776, #52868, #14385, #61464, #84811, #92413, #22962, #1560, #63341, #24834, #55708, #86698, #17231, #83144, #97836, #98831, #13713, #75523, #51728, #12742, #44588, #6107, #89762, #46458, #15556, #77389, #75033, #66417, #21318, #43090, #29413, #60282, #20835, #74543, #98330, #13236, #37003, #28405, #91240, #67913, #82671, #43606, #44090, #36002, #23164, #5611, #36503, #4623, #52196, #59285, #54055 ),
 .UNSPECIFIED., .F., .F.,
 ( 4, 2, 2, 2, 2, 2, 2, 2, 2, 2, 2, 2, 2, 2, 2, 2, 2, 2, 2, 2, 2, 2, 2, 2, 2, 4 ),
 ( 0.0001917148712815067418, 0.0006789549353198572144, 0.001166194999358207470, 0.001409815031377382706, 0.001531625047387005778, 0.001653435063396629066, 0.001775245079406251921, 0.001897055095415875210, 0.002140675127435058903, 0.002627915191473567669, 0.003115155255512077302, 0.004089635383589248357, 0.005064115511666418545, 0.005551355575704968945, 0.005794975607724279706, 0.005916785623733899525, 0.006038595639743519344, 0.006099500647748285452, 0.006160405655753053294, 0.006282215671762459742, 0.006525835703781275240, 0.006769455735800090738, 0.007013075767818906237, 0.007256695799837721735, 0.007500315831856535498, 0.007987555895894149147 ),
 .UNSPECIFIED. ) ;
#67355 = CARTESIAN_POINT ( 'NONE',  ( 196.4242782546697015, 290.4301655533025155, -16.42402868779123537 ) ) ;
#67356 = CARTESIAN_POINT ( 'NONE',  ( 66.01686776079472452, 69.09486339843543590, -2.055003258001108613 ) ) ;
#67357 = FACE_OUTER_BOUND ( 'NONE', #56256, .T. ) ;
#67358 = CARTESIAN_POINT ( 'NONE',  ( 81.80121988122709809, 55.57996685460995678, 16.31202477726384004 ) ) ;
#67359 = CARTESIAN_POINT ( 'NONE',  ( 164.1983466568012204, 264.8415231586690766, -16.64664350988114805 ) ) ;
#67360 = CARTESIAN_POINT ( 'NONE',  ( 125.9656734773588767, 243.5333772461660544, 9.188101187500095079 ) ) ;
#67361 = CARTESIAN_POINT ( 'NONE',  ( 190.8860811105559208, 300.0226043892405414, 8.636347304323541252 ) ) ;
#67362 = EDGE_LOOP ( 'NONE', ( #85073, #45889, #93399, #21372, #81829 ) ) ;
#67363 = CARTESIAN_POINT ( 'NONE',  ( 171.6951446231546754, 264.4514783956147994, 15.84364160967604107 ) ) ;
#67364 = CARTESIAN_POINT ( 'NONE',  ( 46.88368875251780565, 110.3874725885333135, 10.00000000000000000 ) ) ;
#67365 = CARTESIAN_POINT ( 'NONE',  ( 205.7627300303947209, 272.2554926137148072, 9.584172220806708609 ) ) ;
#67366 = AXIS2_PLACEMENT_3D ( 'NONE', #5082, #11208, #43048 ) ;
#67367 = EDGE_LOOP ( 'NONE', ( #94599, #72036, #67081, #55162 ) ) ;
#67368 = CARTESIAN_POINT ( 'NONE',  ( 15.36455789491911794, 32.15369338429142942, -10.00000000000000000 ) ) ;
#67369 = VECTOR ( 'NONE', #70244, 1000.000000000000000 ) ;
#67370 = ORIENTED_EDGE ( 'NONE', *, *, #59302, .T. ) ;
#67371 = ORIENTED_EDGE ( 'NONE', *, *, #99272, .T. ) ;
#67372 = FACE_BOUND ( 'NONE', #7117, .T. ) ;
#67373 = CARTESIAN_POINT ( 'NONE',  ( 167.7752291157694060, 263.0549901451653909, 17.37553087914205108 ) ) ;
#67374 = CARTESIAN_POINT ( 'NONE',  ( 79.47110815956433783, 210.5643266524160424, 9.188101187500095079 ) ) ;
#67375 = CARTESIAN_POINT ( 'NONE',  ( -30.74362438759401428, 96.14847806106469363, 12.64899930806661033 ) ) ;
#67376 = CARTESIAN_POINT ( 'NONE',  ( 93.96857342517718337, 0.000000000000000000, -9.212605237762131694 ) ) ;
#67377 = CARTESIAN_POINT ( 'NONE',  ( 194.2321518193436987, 294.2270399159019121, 13.98132384850917020 ) ) ;
#67378 = AXIS2_PLACEMENT_3D ( 'NONE', #59641, #99665, #75376 ) ;
#67379 = CARTESIAN_POINT ( 'NONE',  ( 81.52103558181507026, 206.3262482093457493, 3.021315404115420679E-15 ) ) ;
#67380 = ORIENTED_EDGE ( 'NONE', *, *, #36196, .F. ) ;
#67381 = CARTESIAN_POINT ( 'NONE',  ( 73.03289083599693754, 63.56301371183312199, -13.95017985831326257 ) ) ;
#67382 = CARTESIAN_POINT ( 'NONE',  ( 201.2139346379346705, 282.1342373466909521, -16.65315141107179286 ) ) ;
#67383 = CARTESIAN_POINT ( 'NONE',  ( 66.08613192275012693, 68.48609657996226474, -4.736323467610598748 ) ) ;
#67384 = ORIENTED_EDGE ( 'NONE', *, *, #35886, .T. ) ;
#67385 = CARTESIAN_POINT ( 'NONE',  ( 164.9101359252495627, 286.5608941336866451, 1.040025780022917790 ) ) ;
#67386 = CARTESIAN_POINT ( 'NONE',  ( 76.07260682810830588, 51.20992803192402931, -15.61887773062573181 ) ) ;
#67387 = CARTESIAN_POINT ( 'NONE',  ( -107.5954152546898257, 65.38554960527383741, 36.50000000000000000 ) ) ;
#67388 = CARTESIAN_POINT ( 'NONE',  ( 163.1711007600727896, 271.8830279655337563, 16.80804004369181470 ) ) ;
#67389 = B_SPLINE_CURVE_WITH_KNOTS ( 'NONE', 3,
 ( #51521, #4944, #21146, #2572, #64862, #52025, #82965, #13539, #35823, #95809, #97652, #66718, #26363, #58604, #7404, #53505 ),
 .UNSPECIFIED., .F., .F.,
 ( 4, 1, 2, 2, 2, 1, 2, 2, 4 ),
 ( 0.000000000000000000, 0.1249999999999996947, 0.1874999999999995837, 0.2499999999999995004, 0.5000000000000003331, 0.6250000000000009992, 0.6874999999999995559, 0.7499999999999981126, 1.000000000000000000 ),
 .UNSPECIFIED. ) ;
#67390 = EDGE_CURVE ( 'NONE', #17277, #3978, #92822, .T. ) ;
#67391 = CARTESIAN_POINT ( 'NONE',  ( 25.96864935082048831, 154.0458036431183189, 22.50000000000001421 ) ) ;
#67393 = AXIS2_PLACEMENT_3D ( 'NONE', #6002, #60672, #97725 ) ;
#67392 = CARTESIAN_POINT ( 'NONE',  ( 171.5015609157691756, 284.1786740197875361, -12.77546238284419644 ) ) ;
#67394 = ORIENTED_EDGE ( 'NONE', *, *, #36945, .T. ) ;
#67395 = CARTESIAN_POINT ( 'NONE',  ( 163.9910908123517288, 246.6060940548019289, -7.333295033952830444 ) ) ;
#67396 = CARTESIAN_POINT ( 'NONE',  ( 131.9464011004214115, 256.1744531367911009, 4.594050593750047540 ) ) ;
#67397 = EDGE_LOOP ( 'NONE', ( #30206, #30114, #5569, #33075 ) ) ;
#67398 = CARTESIAN_POINT ( 'NONE',  ( 88.14062891587492743, 44.42319542341160599, 4.630203861778127816 ) ) ;
#67399 = CARTESIAN_POINT ( 'NONE',  ( 182.2526911774749863, 258.0866462446188621, 6.496747210627928482 ) ) ;
#67400 = CARTESIAN_POINT ( 'NONE',  ( 155.9752437318130092, 261.9691388090409987, -16.96517095716611223 ) ) ;
#67401 = VECTOR ( 'NONE', #9072, 1000.000000000000000 ) ;
#67402 = CARTESIAN_POINT ( 'NONE',  ( 79.32006575253170411, 59.07617305244814787, -16.22726605023456870 ) ) ;
#67403 = CARTESIAN_POINT ( 'NONE',  ( 24.35067441160642687, 40.23626134430271861, 10.00000000000000000 ) ) ;
#67404 = VERTEX_POINT ( 'NONE', #84512 ) ;
#67405 = CARTESIAN_POINT ( 'NONE',  ( 76.73836869982963549, 55.83238297101823377, 16.17114945624216560 ) ) ;
#67406 = CARTESIAN_POINT ( 'NONE',  ( -56.16025090550425602, 33.03454289568183100, 10.00000000000000000 ) ) ;
#67407 = CARTESIAN_POINT ( 'NONE',  ( 167.7367314525692450, 248.9893787533955845, -6.380446527117325850 ) ) ;
#67408 = CARTESIAN_POINT ( 'NONE',  ( 79.87836239028537477, 47.43443509841839756, 13.25449791563737456 ) ) ;
#67409 = CARTESIAN_POINT ( 'NONE',  ( 202.6348823940195416, 267.5801589924517430, 0.8677112048283521784 ) ) ;
#67410 = CARTESIAN_POINT ( 'NONE',  ( 198.4463628819689518, 266.2085727128749681, 0.7937034711031139000 ) ) ;
#67411 = FACE_OUTER_BOUND ( 'NONE', #33992, .T. ) ;
#67412 = CARTESIAN_POINT ( 'NONE',  ( 71.33706390578697665, 71.87455509392472663, 0.2141773752858076585 ) ) ;
#67413 = FACE_BOUND ( 'NONE', #3241, .T. ) ;
#67414 = CARTESIAN_POINT ( 'NONE',  ( 25.96360177180014972, 20.15404122711134249, 8.090169943749479842 ) ) ;
#67415 = CARTESIAN_POINT ( 'NONE',  ( 148.9232972370683399, 272.7042780851529642, 12.27045554427055940 ) ) ;
#67416 = CARTESIAN_POINT ( 'NONE',  ( 57.60966550219797710, 179.2419560658249225, -17.47570218321534696 ) ) ;
#67417 = LINE ( 'NONE', #61309, #58204 ) ;
#67418 = CARTESIAN_POINT ( 'NONE',  ( 198.4706398937704819, 286.8857632237200619, 17.04020736381253798 ) ) ;
#67419 = CARTESIAN_POINT ( 'NONE',  ( 207.1656244175204904, 271.8256082575600772, 5.677357035859670553 ) ) ;
#67420 = CARTESIAN_POINT ( 'NONE',  ( 138.8568224548345142, 257.6427522451418781, 10.00000000000009237 ) ) ;
#67421 = CARTESIAN_POINT ( 'NONE',  ( 175.6294869978224824, 285.1187962335359884, -12.03725621959783965 ) ) ;
#67422 = ORIENTED_EDGE ( 'NONE', *, *, #11483, .F. ) ;
#67423 = CARTESIAN_POINT ( 'NONE',  ( 66.54077760113520412, 67.98430679024006906, -6.561883603421821753 ) ) ;
#67424 = CARTESIAN_POINT ( 'NONE',  ( 198.5954523381739989, 286.6695817285962562, -18.45134152028667174 ) ) ;
#67425 = CARTESIAN_POINT ( 'NONE',  ( 8.375921941576814689, 166.4548013555410080, -4.594050593750042211 ) ) ;
#67426 = AXIS2_PLACEMENT_3D ( 'NONE', #93119, #56064, #891 ) ;
#67427 = CARTESIAN_POINT ( 'NONE',  ( 176.5041649521335785, 257.7439588032058850, -10.43691933783435033 ) ) ;
#67428 = CARTESIAN_POINT ( 'NONE',  ( 29.26302659224649361, 17.86426979415090699, -3.090169943749474069 ) ) ;
#67429 = DIRECTION ( 'NONE',  ( 0.000000000000000000, 0.000000000000000000, 1.000000000000000000 ) ) ;
#67430 = CARTESIAN_POINT ( 'NONE',  ( 173.3022401097396994, 272.4925259712034062, -16.36549126867647885 ) ) ;
#67432 = VECTOR ( 'NONE', #8939, 1000.000000000000000 ) ;
#67431 = DIRECTION ( 'NONE',  ( -0.6623377501714446947, 0.7492053821869066876, 0.000000000000000000 ) ) ;
#67433 = CARTESIAN_POINT ( 'NONE',  ( 159.9924463476198753, 283.3850188831759169, -3.371971149216307140 ) ) ;
#67434 = CARTESIAN_POINT ( 'NONE',  ( 199.2940578277500947, 270.9390390980777852, -11.07481327316625475 ) ) ;
#67435 = CARTESIAN_POINT ( 'NONE',  ( 84.43598368786032893, 47.43396312368651024, 11.99281069980813896 ) ) ;
#67436 = CARTESIAN_POINT ( 'NONE',  ( 198.3452313965520375, 287.1029771126029573, 18.55943827821351988 ) ) ;
#67437 = EDGE_CURVE ( 'NONE', #22269, #8176, #92045, .T. ) ;
#67438 = EDGE_CURVE ( 'NONE', #94399, #37194, #38354, .T. ) ;
#67440 = CARTESIAN_POINT ( 'NONE',  ( 179.6472821955170502, 294.1049463973150750, 1.034999459313757031 ) ) ;
#67439 = AXIS2_PLACEMENT_3D ( 'NONE', #88024, #18573, #9971 ) ;
#67441 = CARTESIAN_POINT ( 'NONE',  ( 58.98402115518014455, 204.8615022471902307, -10.00000000000009592 ) ) ;
#67442 = CARTESIAN_POINT ( 'NONE',  ( 38.52196584993465223, 56.41980893122115504, -10.00000000000000000 ) ) ;
#67443 = CARTESIAN_POINT ( 'NONE',  ( 147.7870527676176948, 274.6723112360602386, 9.257357958194809555 ) ) ;
#67444 = EDGE_CURVE ( 'NONE', #41212, #32812, #7293, .T. ) ;
#67445 = CARTESIAN_POINT ( 'NONE',  ( 19.87790860953014160, 170.0327760586659736, 1.948934522072303157E-15 ) ) ;
#67446 = CARTESIAN_POINT ( 'NONE',  ( 164.3611296587836534, 285.2410164061814726, 4.345597304788310744 ) ) ;
#67447 = EDGE_CURVE ( 'NONE', #60091, #55813, #69013, .T. ) ;
#67448 = CARTESIAN_POINT ( 'NONE',  ( -112.5954152546897262, 74.04580364311806306, 21.50000000000000000 ) ) ;
#67449 = CARTESIAN_POINT ( 'NONE',  ( 37.59133656659163591, 37.10171378149920685, 9.188101187500008038 ) ) ;
#67450 = CARTESIAN_POINT ( 'NONE',  ( 202.0843741143341674, 280.2366252626259211, -15.81775788646446301 ) ) ;
#67451 = CARTESIAN_POINT ( 'NONE',  ( 206.9878665138179770, 272.1334939782196329, 6.566295309274049252 ) ) ;
#67452 = CARTESIAN_POINT ( 'NONE',  ( 188.3628283273592956, 268.0339897934310329, 13.46669696773310498 ) ) ;
#67453 = CARTESIAN_POINT ( 'NONE',  ( 74.14312167556930433, 66.30466486950707861, 1.224646799147354045E-15 ) ) ;
#67454 = CARTESIAN_POINT ( 'NONE',  ( 179.7688937921471677, 262.9204303630262984, -13.99243624848556244 ) ) ;
#67455 =( LENGTH_UNIT ( ) NAMED_UNIT ( * ) SI_UNIT ( .MILLI., .METRE. ) );
#67456 = CARTESIAN_POINT ( 'NONE',  ( 17.58072690530697813, 12.01110640527291373, 2.839279412974134775 ) ) ;
#67457 = CARTESIAN_POINT ( 'NONE',  ( 71.96852905813888412, 72.61068693531508700, 1.394764389614176148 ) ) ;
#67458 = CARTESIAN_POINT ( 'NONE',  ( 82.77428392532827672, 53.84857159627674150, 15.43231797370390623 ) ) ;
#67459 = DIRECTION ( 'NONE',  ( 1.000000000000000000, 0.000000000000000000, 0.000000000000000000 ) ) ;
#67460 = CARTESIAN_POINT ( 'NONE',  ( 193.9844289374573520, 294.6561085335266625, 15.49818881749970245 ) ) ;
#67461 = ORIENTED_EDGE ( 'NONE', *, *, #95893, .T. ) ;
#67462 = VECTOR ( 'NONE', #31983, 1000.000000000000000 ) ;
#67463 = DIRECTION ( 'NONE',  ( -1.000000000000000000, 0.000000000000000000, 0.000000000000000000 ) ) ;
#67464 = CARTESIAN_POINT ( 'NONE',  ( -50.26415955272096880, 51.36194717159466450, 59.99999999999999289 ) ) ;
#67465 = CARTESIAN_POINT ( 'NONE',  ( 74.96743300375965191, 53.32485851529158793, -16.04568551637340335 ) ) ;
#67466 = CARTESIAN_POINT ( 'NONE',  ( 81.34506373925208322, 42.08414435209094506, 7.957546939141312947 ) ) ;
#67467 = ORIENTED_EDGE ( 'NONE', *, *, #88646, .F. ) ;
#67468 = DIRECTION ( 'NONE',  ( -0.8660254037844379305, -0.5000000000000014433, -0.000000000000000000 ) ) ;
#67469 = CARTESIAN_POINT ( 'NONE',  ( 29.13110022456613635, 42.86445400964586838, 177.5919119679930134 ) ) ;
#67470 = CARTESIAN_POINT ( 'NONE',  ( 81.81010722587693351, 59.02505635547797169, -0.4806308479691593916 ) ) ;
#67471 = CARTESIAN_POINT ( 'NONE',  ( 202.9547455376043672, 279.1190644220934018, -15.19669173352461478 ) ) ;
#67472 = EDGE_LOOP ( 'NONE', ( #5252, #80817, #27041, #74755 ) ) ;
#67473 = ORIENTED_EDGE ( 'NONE', *, *, #4231, .F. ) ;
#67475 = CARTESIAN_POINT ( 'NONE',  ( 204.9608076533459950, 275.6444629144898499, 14.31488288944633069 ) ) ;
#67474 = CARTESIAN_POINT ( 'NONE',  ( 201.5801617693437890, 279.7599021095377907, 16.47958900488177036 ) ) ;
#67476 = CARTESIAN_POINT ( 'NONE',  ( 153.4477557824949940, 264.8676860077344486, 17.16010094972647693 ) ) ;
#67477 = ORIENTED_EDGE ( 'NONE', *, *, #44629, .F. ) ;
#67478 = CARTESIAN_POINT ( 'NONE',  ( 150.6571681785161445, 269.7011255207979730, 15.24894850018880454 ) ) ;
#67479 = CARTESIAN_POINT ( 'NONE',  ( 80.54858391640954096, 57.70359709413047966, 16.24103893543703592 ) ) ;
#67480 = DIRECTION ( 'NONE',  ( -0.5634352399127592337, -0.8261602328994366307, 0.000000000000000000 ) ) ;
#67481 = ORIENTED_EDGE ( 'NONE', *, *, #82257, .T. ) ;
#67482 = CARTESIAN_POINT ( 'NONE',  ( 147.6220714307702622, 274.9580672937808572, 8.392894244419288441 ) ) ;
#67483 = CARTESIAN_POINT ( 'NONE',  ( 81.27023270499687158, 43.21841413807894838, 9.592188031249742508 ) ) ;
#67484 = ORIENTED_EDGE ( 'NONE', *, *, #50380, .F. ) ;
#67485 = CARTESIAN_POINT ( 'NONE',  ( 164.3754245770190039, 245.9404084473339083, 1.667926061651832992 ) ) ;
#67486 = CARTESIAN_POINT ( 'NONE',  ( 75.02043720394767945, 65.61285698292792290, 13.53072932596785272 ) ) ;
#67487 = ORIENTED_EDGE ( 'NONE', *, *, #11338, .T. ) ;
#67488 = CARTESIAN_POINT ( 'NONE',  ( 177.7398568146338107, 279.4700101068085019, -16.54123403330698849 ) ) ;
#67489 = CARTESIAN_POINT ( 'NONE',  ( 172.2915296418940443, 263.9746128868251276, -15.63729134622028205 ) ) ;
#67490 = ORIENTED_EDGE ( 'NONE', *, *, #78427, .F. ) ;
#67491 = CARTESIAN_POINT ( 'NONE',  ( 158.6626729816061925, 274.8399133342844607, -13.49366594499505645 ) ) ;
#67492 = CARTESIAN_POINT ( 'NONE',  ( 60.96635096964421763, 217.5530062829863027, -4.648177544792955347E-16 ) ) ;
#67493 = CARTESIAN_POINT ( 'NONE',  ( -52.88606886026012432, 92.76052029034119073, -10.00000000000000000 ) ) ;
#67494 = ORIENTED_EDGE ( 'NONE', *, *, #29269, .F. ) ;
#67495 = ORIENTED_EDGE ( 'NONE', *, *, #71902, .T. ) ;
#67496 = CARTESIAN_POINT ( 'NONE',  ( 77.87286301834419078, 52.13848254994933740, -16.08542584302312051 ) ) ;
#67497 = CARTESIAN_POINT ( 'NONE',  ( 87.34409271548551601, 43.66013200155327922, 0.5981997646405022850 ) ) ;
#67498 = DIRECTION ( 'NONE',  ( -0.8660254037844378194, -0.5000000000000013323, -0.000000000000000000 ) ) ;
#67499 = CARTESIAN_POINT ( 'NONE',  ( 82.50452235219570696, 53.86480448276187616, 15.85105177732746817 ) ) ;
#67500 = CARTESIAN_POINT ( 'NONE',  ( 148.9498507103374152, 272.6582861203333437, 11.90061892622094852 ) ) ;
#67501 = CARTESIAN_POINT ( 'NONE',  ( 157.0701535447001334, 259.2118014948599694, -17.01617165317321323 ) ) ;
#67502 = CARTESIAN_POINT ( 'NONE',  ( 147.2048811707249456, 275.6806620206021421, -0.5293868638167661400 ) ) ;
#67503 = CARTESIAN_POINT ( 'NONE',  ( 191.2111338740054975, 299.4595964878050154, -9.718193530796334301 ) ) ;
#67504 = ORIENTED_EDGE ( 'NONE', *, *, #36705, .T. ) ;
#67505 = CARTESIAN_POINT ( 'NONE',  ( 77.17331351098810899, 56.95370604848049823, -16.18904554513164484 ) ) ;
#67507 = ADVANCED_FACE ( 'NONE', ( #8473 ), #372, .F. ) ;
#67506 = VECTOR ( 'NONE', #19484, 1000.000000000000000 ) ;
#67508 = CARTESIAN_POINT ( 'NONE',  ( 149.3545991938273971, 273.9572411826421217, -10.14243178476390028 ) ) ;
#67509 = DIRECTION ( 'NONE',  ( -0.4245406647209920559, -0.9054088711727195093, 0.000000000000000000 ) ) ;
#67510 = DIRECTION ( 'NONE',  ( -0.5696381972391160176, 0.8218955677251033043, 0.000000000000000000 ) ) ;
#67511 = CARTESIAN_POINT ( 'NONE',  ( 171.5371663410915630, 288.9842175639024617, 4.255310109042821587 ) ) ;
#67512 = LINE ( 'NONE', #74653, #1015 ) ;
#67513 = AXIS2_PLACEMENT_3D ( 'NONE', #89009, #74256, #59500 ) ;
#67514 = VERTEX_POINT ( 'NONE', #85004 ) ;
#67515 = CARTESIAN_POINT ( 'NONE',  ( 149.0323978447938202, 272.5153102894354333, -11.84998907946122060 ) ) ;
#67516 = CARTESIAN_POINT ( 'NONE',  ( 198.2505066714982149, 285.2670451491296149, 0.000000000000000000 ) ) ;
#67517 = CARTESIAN_POINT ( 'NONE',  ( 202.4560076411394220, 279.0611292670678267, 15.58065739802832717 ) ) ;
#67518 = CARTESIAN_POINT ( 'NONE',  ( 78.96518011614999466, 46.19984413241925836, 12.79727321583966493 ) ) ;
#67519 = CARTESIAN_POINT ( 'NONE',  ( 39.49844957003023893, 203.6115022471903160, -5.000000000000047962 ) ) ;
#67520 = CARTESIAN_POINT ( 'NONE',  ( 78.63357992691169329, 55.03961015548562585, -16.49924009853327078 ) ) ;
#67521 = ORIENTED_EDGE ( 'NONE', *, *, #23962, .F. ) ;
#67522 = CARTESIAN_POINT ( 'NONE',  ( 170.4914208022274522, 255.7692698374902136, -12.13427622590457844 ) ) ;
#67523 = AXIS2_PLACEMENT_3D ( 'NONE', #45955, #53568, #9490 ) ;
#67524 = CARTESIAN_POINT ( 'NONE',  ( 205.7350094608039228, 273.2218331975091132, 10.02726759709120330 ) ) ;
#67526 = ADVANCED_FACE ( 'NONE', ( #45460 ), #61165, .F. ) ;
#67525 = CARTESIAN_POINT ( 'NONE',  ( 155.3085688348458007, 262.3516442638374997, 17.09768579440982705 ) ) ;
#67527 = CARTESIAN_POINT ( 'NONE',  ( 38.47004439948830168, 203.0177522451419350, 5.000000000000046185 ) ) ;
#67528 = CARTESIAN_POINT ( 'NONE',  ( 114.1117772151768577, 242.8149278399161233, -9.188101187500095079 ) ) ;
#67529 = CARTESIAN_POINT ( 'NONE',  ( 151.0388915836658725, 269.0399611886400635, -14.24896787280406585 ) ) ;
#67530 = CARTESIAN_POINT ( 'NONE',  ( 166.1193465202780715, 270.2353025340392492, 17.56265815376753636 ) ) ;
#67531 = CARTESIAN_POINT ( 'NONE',  ( 84.32777827622054190, 50.66816837149428210, 13.78787580221864140 ) ) ;
#67532 = CARTESIAN_POINT ( 'NONE',  ( 172.3284624602130748, 251.0446003553498713, -4.012660189023237400 ) ) ;
#67533 = CARTESIAN_POINT ( 'NONE',  ( 32.89474554257621719, 198.9869531367911293, 4.594050593750046652 ) ) ;
#67534 = CARTESIAN_POINT ( 'NONE',  ( 147.6853019674385337, 275.3811002756974062, -3.519384196793790220 ) ) ;
#67535 = CIRCLE ( 'NONE', #19051, 70.00000000000001421 ) ;
#67536 = EDGE_LOOP ( 'NONE', ( #36706, #91808, #61755, #17130 ) ) ;
#67537 = DIRECTION ( 'NONE',  ( -0.8660254037844387076, -0.4999999999999998890, -0.000000000000000000 ) ) ;
#67538 = CARTESIAN_POINT ( 'NONE',  ( 177.8945296157199039, 265.5031784322380304, 15.66114811942481033 ) ) ;
#67539 = DIRECTION ( 'NONE',  ( 1.000000000000000000, 0.000000000000000000, 0.000000000000000000 ) ) ;
#67540 = CARTESIAN_POINT ( 'NONE',  ( 190.8545714895799392, 300.0771806536980648, -5.516553996882049837 ) ) ;
#67541 = CARTESIAN_POINT ( 'NONE',  ( 150.2076754159204484, 245.9824982072973683, 3.021315404115420679E-15 ) ) ;
#67542 = CARTESIAN_POINT ( 'NONE',  ( 168.8244094625508751, 257.0541383169796745, -14.93690306707719628 ) ) ;
#67543 = CARTESIAN_POINT ( 'NONE',  ( 178.2996191249796425, 286.8120259801574434, -12.18722290671415465 ) ) ;
#67544 = CARTESIAN_POINT ( 'NONE',  ( 68.83366497510655790, 64.72209559286066849, -12.18477093088157481 ) ) ;
#67545 = AXIS2_PLACEMENT_3D ( 'NONE', #45025, #75968, #5050 ) ;
#67546 = CARTESIAN_POINT ( 'NONE',  ( 96.49374645304573050, 226.5177522451418781, -10.00000000000009592 ) ) ;
#67547 = B_SPLINE_CURVE_WITH_KNOTS ( 'NONE', 3,
 ( #33197, #64098, #95044, #44278, #76210, #51384, #97517, #29587, #13407, #98004, #67080, #28089, #14873, #13886, #58959, #98513, #67581, #21492, #36178, #21981, #74223, #29104, #52875, #6786, #83826, #52382, #59969, #82838, #53375, #75208, #44768, #28584, #89931, #82350, #5785, #37666, #12918, #20509, #60463, #36673, #59463, #68576 ),
 .UNSPECIFIED., .F., .F.,
 ( 4, 2, 2, 2, 2, 2, 2, 2, 2, 2, 2, 2, 2, 2, 2, 2, 2, 2, 2, 2, 4 ),
 ( 0.002284396617591029702, 0.002715654238588044358, 0.002931283049086530652, 0.003146911859585016947, 0.003254726264834252071, 0.003362540670083487629, 0.003578169480582080175, 0.004009427101579153378, 0.004871942343573404735, 0.005734457585567655225, 0.006596972827561904847, 0.007028230448559109021, 0.007459488069556312329, 0.007567302474805549621, 0.007621209677430168701, 0.007675116880054787781, 0.007782931285304025074, 0.007890745690553263234, 0.008322003311550044136, 0.008753260932546826772, 0.009184518553543607675 ),
 .UNSPECIFIED. ) ;
#67548 = VERTEX_POINT ( 'NONE', #86531 ) ;
#67549 = DIRECTION ( 'NONE',  ( -0.8660254037844378194, -0.5000000000000013323, -0.000000000000000000 ) ) ;
#67550 = CARTESIAN_POINT ( 'NONE',  ( 155.4406061314905969, 279.7141320257344432, -1.823194431127334258 ) ) ;
#67551 = CARTESIAN_POINT ( 'NONE',  ( 84.55206357306229847, 46.71456743556125701, -11.30110183101671062 ) ) ;
#67552 = CARTESIAN_POINT ( 'NONE',  ( 11.92112666437810908, 171.5643266524160140, 9.188101187500095079 ) ) ;
#67553 = CARTESIAN_POINT ( 'NONE',  ( 7.019590965729775256, 22.79103043416547081, 8.090169943749478065 ) ) ;
#67554 = CARTESIAN_POINT ( 'NONE',  ( 194.0768453189403431, 272.9027882872081818, 14.29780024873114819 ) ) ;
#67555 = CARTESIAN_POINT ( 'NONE',  ( 71.48584797926407930, 59.35514066858884519, -15.73530635236135922 ) ) ;
#67556 = CARTESIAN_POINT ( 'NONE',  ( 30.62489312496363425, 46.16797101519271962, -10.00000000000000000 ) ) ;
#67557 = ADVANCED_FACE ( 'NONE', ( #82906 ), #66170, .F. ) ;
#67558 = CARTESIAN_POINT ( 'NONE',  ( 43.61180991440864574, 205.1744531367911293, 4.594050593750047540 ) ) ;
#67559 = CARTESIAN_POINT ( 'NONE',  ( 163.8111161534324935, 246.9178193081252743, -7.110480325054721717 ) ) ;
#67560 = CARTESIAN_POINT ( 'NONE',  ( 72.48211761085248384, 57.49817692938951552, 15.81360302781613036 ) ) ;
#67561 = LINE ( 'NONE', #83306, #68283 ) ;
#67562 = CARTESIAN_POINT ( 'NONE',  ( 164.9971748156432056, 244.8635054444190757, -1.825016704039769788 ) ) ;
#67563 = EDGE_LOOP ( 'NONE', ( #72345, #64357, #43910, #84239 ) ) ;
#67564 = CARTESIAN_POINT ( 'NONE',  ( 23.90999230191042102, 174.6115022471901739, -5.000000000000041744 ) ) ;
#67565 = CARTESIAN_POINT ( 'NONE',  ( 207.5792673731680793, 271.1091576421853233, 2.359198794924813214 ) ) ;
#67566 = VECTOR ( 'NONE', #97145, 1000.000000000000000 ) ;
#67567 = CARTESIAN_POINT ( 'NONE',  ( 133.4890956248536895, 254.0024278399161233, 9.188101187500095079 ) ) ;
#67568 = CARTESIAN_POINT ( 'NONE',  ( 25.16147942602835386, 23.03085787977763843, 9.188101187500006262 ) ) ;
#67569 = CARTESIAN_POINT ( 'NONE',  ( 165.0777597283848195, 244.7239282812269039, 1.811418920707685842 ) ) ;
#67570 = EDGE_CURVE ( 'NONE', #14773, #50052, #9848, .T. ) ;
#67571 = DIRECTION ( 'NONE',  ( 1.000000000000000000, 0.000000000000000000, 0.000000000000000000 ) ) ;
#67572 = CARTESIAN_POINT ( 'NONE',  ( 25.34687108590969729, 93.06504152958497400, 60.00000000000000000 ) ) ;
#67574 = CARTESIAN_POINT ( 'NONE',  ( 187.9901615146041536, 289.1405255857209795, 14.44262214775099373 ) ) ;
#67573 = CARTESIAN_POINT ( 'NONE',  ( 157.8849654228661166, 257.1822134667773980, 17.43614750057631468 ) ) ;
#67575 = CARTESIAN_POINT ( 'NONE',  ( 68.79717273036834513, 64.27923393059754176, 12.51298953402340963 ) ) ;
#67576 = ORIENTED_EDGE ( 'NONE', *, *, #91951, .T. ) ;
#67577 = CARTESIAN_POINT ( 'NONE',  ( 80.34760537404680747, 47.87480626140324347, 13.91709158461522655 ) ) ;
#67578 = CARTESIAN_POINT ( 'NONE',  ( 208.3482402183368833, 269.7772576047121902, -1.475194656411285443 ) ) ;
#67579 = CARTESIAN_POINT ( 'NONE',  ( 189.3775153017087973, 300.6355170167246911, -1.634152055493470757 ) ) ;
#67580 = CARTESIAN_POINT ( 'NONE',  ( 169.5420174322075013, 266.0148534173676467, -17.05181222767901872 ) ) ;
#67581 = CARTESIAN_POINT ( 'NONE',  ( 194.7603117279403477, 271.6192734837231910, -13.48552198304586547 ) ) ;
#67582 = ORIENTED_EDGE ( 'NONE', *, *, #91875, .F. ) ;
#67583 = LINE ( 'NONE', #75703, #445 ) ;
#67584 = AXIS2_PLACEMENT_3D ( 'NONE', #80891, #3360, #10438 ) ;
#67585 = CARTESIAN_POINT ( 'NONE',  ( 169.5727729373952002, 284.0798650663272156, -11.84966624384599676 ) ) ;
#67586 = CARTESIAN_POINT ( 'NONE',  ( 71.78242053751054641, 72.53632993589367572, 0.9980050652678308376 ) ) ;
#67587 = B_SPLINE_SURFACE_WITH_KNOTS ( 'NONE', 3, 1, ( 
 ( #46499, #84073 ),
 ( #53116, #85576 ),
 ( #54096, #15599 ),
 ( #54594, #62197 ),
 ( #420, #31309 ),
 ( #61208, #29820 ),
 ( #76438, #77933 ),
 ( #77435, #69810 ),
 ( #93148, #16120 ),
 ( #23205, #8524 ),
 ( #62701, #39393 ),
 ( #92175, #14626 ),
 ( #22725, #7507 ),
 ( #7013, #38404 ),
 ( #78437, #24223 ),
 ( #37898, #100239 ),
 ( #99234, #68806 ),
 ( #70310, #923 ),
 ( #69317, #55103 ),
 ( #30823, #47510 ),
 ( #86090, #37405 ),
 ( #68311, #91652 ),
 ( #22218, #33318 ),
 ( #64217, #1929 ),
 ( #39890, #56097 ),
 ( #10031, #51373 ),
 ( #32815, #87090 ),
 ( #56616, #63720 ),
 ( #48007, #80467 ),
 ( #66585, #88084 ),
 ( #95168, #87600 ) ),
 .UNSPECIFIED., .F., .F., .F.,
 ( 4, 3, 3, 3, 3, 3, 3, 3, 3, 3, 4 ),
 ( 2, 2 ),
 ( 0.000000000000000000, 0.1333490885032357909, 0.3007194338854210502, 0.4699862290245036545, 0.5844252810809178467, 0.6686540514502550270, 0.7354980260655467061, 0.8028463152565693539, 0.8633854507757410257, 0.9437142632667440134, 1.000000000000000000 ),
 ( 0.000000000000000000, 1.000000000000000000 ),
 .UNSPECIFIED. ) ;
#67588 = DIRECTION ( 'NONE',  ( 0.5000000000000013323, -0.8660254037844378194, 0.000000000000000000 ) ) ;
#67589 = LINE ( 'NONE', #29596, #39069 ) ;
#67590 = CARTESIAN_POINT ( 'NONE',  ( 181.8958890403558541, 295.0801465899038476, 4.827918899673129260 ) ) ;
#67591 = CARTESIAN_POINT ( 'NONE',  ( 67.98269450004784176, 69.23742185243530400, 4.145183063120581934 ) ) ;
#67592 = CARTESIAN_POINT ( 'NONE',  ( 201.2535035105529744, 282.0657020489176716, -18.08976065250591958 ) ) ;
#67593 = CIRCLE ( 'NONE', #12593, 14.82106496071134671 ) ;
#67594 = CARTESIAN_POINT ( 'NONE',  ( 82.86586985908988368, 152.2544130683315871, 0.000000000000000000 ) ) ;
#67595 = CARTESIAN_POINT ( 'NONE',  ( 7.184267760421183091, 27.08080186712590631, -3.090169943749475845 ) ) ;
#67596 = CARTESIAN_POINT ( 'NONE',  ( 82.48921279030038534, 44.14273019941255427, 9.857891367207361810 ) ) ;
#67597 = ORIENTED_EDGE ( 'NONE', *, *, #30639, .F. ) ;
#67598 = CARTESIAN_POINT ( 'NONE',  ( -65.00000000000000000, 93.06504152958497400, -54.99999999999999289 ) ) ;
#67599 = CARTESIAN_POINT ( 'NONE',  ( 86.55406513359314147, 47.25665231443431935, -10.69898602647500496 ) ) ;
#67600 = CARTESIAN_POINT ( 'NONE',  ( 81.57461113938337860, 45.47094929192444113, -11.08393736095532844 ) ) ;
#67601 = VERTEX_POINT ( 'NONE', #21089 ) ;
#67602 = CARTESIAN_POINT ( 'NONE',  ( 165.5298684834693574, 269.3554679133272884, -17.63324793928101997 ) ) ;
#67603 = DIRECTION ( 'NONE',  ( 0.7893155279419866721, 0.6139877827364833562, 0.000000000000000000 ) ) ;
#67604 = VECTOR ( 'NONE', #43668, 1000.000000000000000 ) ;
#67605 = CARTESIAN_POINT ( 'NONE',  ( 163.9704062730716032, 246.6419207277664327, 7.317582738093436845 ) ) ;
#67606 = FACE_OUTER_BOUND ( 'NONE', #96306, .T. ) ;
#67607 = VERTEX_POINT ( 'NONE', #4367 ) ;
#67608 = CARTESIAN_POINT ( 'NONE',  ( 93.32751462011536603, 218.5643266524159856, -9.188101187500093303 ) ) ;
#67609 = CARTESIAN_POINT ( 'NONE',  ( 155.5009445773975187, 261.3114586974326130, 17.03375350714145142 ) ) ;
#67610 = CARTESIAN_POINT ( 'NONE',  ( 181.1363957779798284, 271.6931546333026972, -17.04292735804997605 ) ) ;
#67611 = DIRECTION ( 'NONE',  ( -0.000000000000000000, -0.000000000000000000, -1.000000000000000000 ) ) ;
#67612 = B_SPLINE_SURFACE_WITH_KNOTS ( 'NONE', 3, 1, ( 
 ( #70943, #55208 ),
 ( #61316, #92279 ),
 ( #68918, #78544 ),
 ( #86189, #39009 ),
 ( #530, #93261 ),
 ( #38515, #77019 ),
 ( #16725, #22826 ),
 ( #45611, #40 ),
 ( #47617, #7623 ),
 ( #30925, #9132 ),
 ( #40003, #7121 ),
 ( #41001, #19257 ),
 ( #34425, #80068 ),
 ( #11152, #95286 ),
 ( #32920, #26829 ),
 ( #49620, #42502 ),
 ( #96262, #25846 ),
 ( #17740, #73439 ),
 ( #95782, #18736 ),
 ( #71445, #49134 ),
 ( #34907, #80573 ),
 ( #57708, #11643 ),
 ( #42021, #2033 ),
 ( #4023, #33948 ),
 ( #71943, #65807 ),
 ( #96767, #63824 ),
 ( #79066, #55695 ),
 ( #56723, #94759 ),
 ( #81077, #40510 ),
 ( #25323, #56209 ),
 ( #26334, #87705 ) ),
 .UNSPECIFIED., .F., .F., .F.,
 ( 4, 3, 3, 3, 3, 3, 3, 3, 3, 3, 4 ),
 ( 2, 2 ),
 ( 0.000000000000000000, 0.1122669598086724063, 0.2243161639709572719, 0.3396355846218986341, 0.4553962076585058583, 0.5677860799922284096, 0.6749047109689497725, 0.7773884377078336128, 0.8775581155834173419, 0.9782364162377894523, 1.000000000000000000 ),
 ( 0.000000000000000000, 1.000000000000000000 ),
 .UNSPECIFIED. ) ;
#67613 = ORIENTED_EDGE ( 'NONE', *, *, #55531, .F. ) ;
#67614 = ORIENTED_EDGE ( 'NONE', *, *, #25360, .T. ) ;
#67615 = B_SPLINE_CURVE_WITH_KNOTS ( 'NONE', 3,
 ( #3385, #34257, #65153, #96100, #95106, #87537, #18069, #26659, #11486, #80915, #57541, #88520, #49957, #98064, #44829, #60517, #60026, #91473, #59019, #6349, #4870, #12469, #13946, #83886, #12977, #5848, #68134, #66647, #90990, #67639, #37236, #35750, #75762, #22035, #83380, #74776, #43838, #14448, #28641, #99062, #89989, #43338, #36236, #29644, #21551, #82412, #52433, #5355, #52933, #74286 ),
 .UNSPECIFIED., .F., .F.,
 ( 4, 2, 2, 2, 2, 2, 2, 2, 2, 2, 2, 2, 2, 2, 2, 2, 2, 2, 2, 2, 2, 2, 2, 2, 4 ),
 ( 0.0005071336019138968695, 0.0009528387457653599620, 0.001175691317691181063, 0.001287117603654161328, 0.001398543889617141593, 0.001509970175580121858, 0.001621396461543102123, 0.001844249033469137896, 0.002289954177321128562, 0.003181364465025150225, 0.004072774752729171888, 0.004964185040433193551, 0.005409890184285204816, 0.005632742756211172284, 0.005744169042174153417, 0.005799882185155722479, 0.005855595328137289807, 0.005911308471118858002, 0.005967021614100427064, 0.006078447900063561719, 0.006301300471989755569, 0.006747005615842055666, 0.007192710759694355763, 0.007415563331620505377, 0.007638415903546654992 ),
 .UNSPECIFIED. ) ;
#67616 = CARTESIAN_POINT ( 'NONE',  ( 88.28323348104321155, 43.74655523625713016, 0.1991997974169892882 ) ) ;
#67617 = EDGE_LOOP ( 'NONE', ( #58513, #91053 ) ) ;
#67618 = CARTESIAN_POINT ( 'NONE',  ( 81.66405316814116588, 51.22542360033385478, 14.71426855131227462 ) ) ;
#67619 = ORIENTED_EDGE ( 'NONE', *, *, #75277, .F. ) ;
#67620 = CARTESIAN_POINT ( 'NONE',  ( 76.14474959763187201, 64.73882662526121123, 14.33715962598121152 ) ) ;
#67621 = ORIENTED_EDGE ( 'NONE', *, *, #14843, .F. ) ;
#67622 = CARTESIAN_POINT ( 'NONE',  ( 190.6556843249743167, 294.0696558316880100, -13.68617225801477666 ) ) ;
#67623 = CARTESIAN_POINT ( 'NONE',  ( 19.18375657693640335, 36.32959363016014720, -10.00000000000000000 ) ) ;
#67624 = CARTESIAN_POINT ( 'NONE',  ( -23.44353372814872216, 99.78638950773219563, 45.19941947175312436 ) ) ;
#67625 = CARTESIAN_POINT ( 'NONE',  ( 82.57676729861134390, 54.19068042909008653, -15.92587557605581061 ) ) ;
#67626 = CARTESIAN_POINT ( 'NONE',  ( 164.7820965459765148, 264.9732998066323262, -16.63464453842744462 ) ) ;
#67627 = ORIENTED_EDGE ( 'NONE', *, *, #28077, .F. ) ;
#67628 = CARTESIAN_POINT ( 'NONE',  ( 66.41068231923046028, 68.91878406202458507, 0.07809209811752516883 ) ) ;
#67629 = B_SPLINE_CURVE_WITH_KNOTS ( 'NONE', 3,
 ( #51992, #68669, #13017, #29199, #37767, #90031, #99594, #92034, #91030, #28186, #60067, #12509, #43380, #97620, #5890, #74324, #35790, #90544, #20605, #75809, #51486, #99103, #6394, #59060, #82455, #43877, #5399, #21594, #36283, #98106, #28688, #37279, #68176, #29687, #60559, #91516, #22083, #53957, #38767, #92514, #100102, #86440, #31164, #31657, #70162, #62053, #3184, #93004, #62554, #93517 ),
 .UNSPECIFIED., .F., .F.,
 ( 4, 2, 2, 2, 2, 2, 2, 2, 2, 2, 2, 2, 2, 2, 2, 2, 2, 2, 2, 2, 2, 2, 2, 2, 4 ),
 ( 0.0004205494687147382340, 0.0008747062255947330497, 0.001101784604034729970, 0.001328862982474727106, 0.001442402171694725458, 0.001555941360914724243, 0.001669480550134722595, 0.001783019739354720946, 0.002010098117794719384, 0.002237176496234717822, 0.003145490009994790070, 0.004053803523754863185, 0.004962117037514935866, 0.005416273794394934477, 0.005643352172834971078, 0.005756891362054951215, 0.005813660956664978147, 0.005870430551275005078, 0.005927200145885032009, 0.005983969740495058941, 0.006097508929715112803, 0.006324587308155201447, 0.006778744065035404755, 0.007232900821915607195, 0.007687057578795810503 ),
 .UNSPECIFIED. ) ;
#67630 = CARTESIAN_POINT ( 'NONE',  ( 12.38457448260035143, 9.011106405272903075, 2.839279412974134775 ) ) ;
#67631 = ORIENTED_EDGE ( 'NONE', *, *, #68937, .F. ) ;
#67632 = ADVANCED_FACE ( 'NONE', ( #51966 ), #6366, .F. ) ;
#67633 = CARTESIAN_POINT ( 'NONE',  ( 165.4602035580446397, 282.3930620430364229, 8.860554159259999452 ) ) ;
#67635 = EDGE_LOOP ( 'NONE', ( #97888, #40155, #18702, #34118, #81517 ) ) ;
#67634 = CARTESIAN_POINT ( 'NONE',  ( 168.4809247738020019, 252.9187805847961670, 12.05003015331094041 ) ) ;
#67636 = CARTESIAN_POINT ( 'NONE',  ( 162.8037981520209314, 248.6625452659484381, 9.809699077002424161 ) ) ;
#67637 = EDGE_CURVE ( 'NONE', #16766, #41280, #6343, .T. ) ;
#67638 = CARTESIAN_POINT ( 'NONE',  ( 188.1792557714354928, 260.7783204226367388, 2.818005635731814618 ) ) ;
#67639 = CARTESIAN_POINT ( 'NONE',  ( 161.2587810186207662, 281.3878282502170123, -6.584893775719714348 ) ) ;
#67640 = PLANE ( 'NONE',  #2061 ) ;
#67641 =( BOUNDED_CURVE ( )  B_SPLINE_CURVE ( 2, ( #9005, #16601, #39877, #87078, #47499, #8023, #71326, #31298, #94147 ),
 .UNSPECIFIED., .F., .T. ) 
 B_SPLINE_CURVE_WITH_KNOTS ( ( 3, 2, 2, 2, 3 ),
 ( 0.4637096774193548154, 0.4650537634408601906, 0.4677419354838709409, 0.4704301075268817467, 0.4717741935483871218 ),
 .UNSPECIFIED. ) 
 CURVE ( )  GEOMETRIC_REPRESENTATION_ITEM ( )  RATIONAL_B_SPLINE_CURVE ( ( 0.9330127018922194093, 0.9330127018922194093, 1.000000000000000000, 0.8660254037844387076, 1.000000000000000000, 0.8660254037844387076, 1.000000000000000000, 0.9330127018922194093, 0.9330127018922194093 ) ) 
 REPRESENTATION_ITEM ( '' )  );
#67642 = CARTESIAN_POINT ( 'NONE',  ( 41.19957572438558913, 58.46810036157969392, -10.00000000000000000 ) ) ;
#67643 = FACE_OUTER_BOUND ( 'NONE', #84358, .T. ) ;
#67644 = CARTESIAN_POINT ( 'NONE',  ( 77.72205534048291042, 61.52847525230062331, 16.09962475150208405 ) ) ;
#67645 = ORIENTED_EDGE ( 'NONE', *, *, #89260, .F. ) ;
#67646 = CARTESIAN_POINT ( 'NONE',  ( 95.28491933047783391, 232.4865022471902876, -10.00000000000009592 ) ) ;
#67647 = CARTESIAN_POINT ( 'NONE',  ( 70.09145387123612636, 63.58422643240743355, -12.93064994232666010 ) ) ;
#67648 = ORIENTED_EDGE ( 'NONE', *, *, #43563, .T. ) ;
#67649 = CIRCLE ( 'NONE', #96762, 0.1418229129680897982 ) ;
#67651 = EDGE_CURVE ( 'NONE', #70217, #26616, #14463, .T. ) ;
#67650 = CARTESIAN_POINT ( 'NONE',  ( -19.65312891409030271, 93.06504152958497400, 60.00000000000000000 ) ) ;
#67652 = CARTESIAN_POINT ( 'NONE',  ( -7.501470784735642106, 173.1427522451419350, -10.00000000000009415 ) ) ;
#67653 = CARTESIAN_POINT ( 'NONE',  ( 192.7865293790353860, 266.9527545350466653, -11.24613748226589927 ) ) ;
#67654 = CARTESIAN_POINT ( 'NONE',  ( 171.3024615537961495, 279.7431976243712484, -14.91927184813412843 ) ) ;
#67655 = CARTESIAN_POINT ( 'NONE',  ( 163.3482521698857113, 247.7195232446219677, -7.972463205267773745 ) ) ;
#67656 = CARTESIAN_POINT ( 'NONE',  ( 84.43667057297049894, 44.63661754160224149, -8.257540914285325329 ) ) ;
#67657 = AXIS2_PLACEMENT_3D ( 'NONE', #11982, #49972, #96116 ) ;
#67658 = CARTESIAN_POINT ( 'NONE',  ( 161.0985561068035850, 273.0316086281096659, 15.84788186387147135 ) ) ;
#67660 = CARTESIAN_POINT ( 'NONE',  ( 108.2753003872444424, 239.9865022471903444, -10.00000000000009592 ) ) ;
#67659 = CARTESIAN_POINT ( 'NONE',  ( -7.619092152155812592, 178.6589784336661637, -6.496448406907675876E-16 ) ) ;
#67661 = CARTESIAN_POINT ( 'NONE',  ( 22.44857442947622417, 183.7677522451418497, 10.00000000000009592 ) ) ;
#67662 = ORIENTED_EDGE ( 'NONE', *, *, #37885, .T. ) ;
#67663 = CIRCLE ( 'NONE', #49870, 70.00000000000001421 ) ;
#67664 = ORIENTED_EDGE ( 'NONE', *, *, #34312, .F. ) ;
#67665 = PLANE ( 'NONE',  #56449 ) ;
#67666 = CARTESIAN_POINT ( 'NONE',  ( 9.476883925432959543, 29.12856466152289414, -10.00000000000000000 ) ) ;
#67667 = EDGE_CURVE ( 'NONE', #5574, #37857, #55714, .T. ) ;
#67668 = CARTESIAN_POINT ( 'NONE',  ( 175.5066696105806443, 290.9053867346144102, 2.574525986029098323 ) ) ;
#67669 = CARTESIAN_POINT ( 'NONE',  ( -51.16543076746616947, 82.50588140424335393, -10.00000000000000000 ) ) ;
#67670 = CARTESIAN_POINT ( 'NONE',  ( 81.98204644731730184, 41.14170830008083612, -5.380964918418897902 ) ) ;
#67671 = VECTOR ( 'NONE', #59695, 999.9999999999998863 ) ;
#67672 = CARTESIAN_POINT ( 'NONE',  ( 72.10617024684209753, 72.18421392457030095, 4.031754617348218162 ) ) ;
#67673 = CARTESIAN_POINT ( 'NONE',  ( 149.6148422561466305, 277.4437614652936190, 3.137689077364430368 ) ) ;
#67674 = CARTESIAN_POINT ( 'NONE',  ( 12.43489537816885537, 187.1744531367911293, 4.594050593750047540 ) ) ;
#67675 = CARTESIAN_POINT ( 'NONE',  ( 123.8009570636627785, 230.0327760586659736, 1.948934522072303157E-15 ) ) ;
#67676 = CARTESIAN_POINT ( 'NONE',  ( 48.88270317314112390, 187.4824982072973967, 3.021315404115420679E-15 ) ) ;
#67677 = CARTESIAN_POINT ( 'NONE',  ( 183.7975612849717777, 256.6346208101135176, -2.981236333899912161 ) ) ;
#67678 = CARTESIAN_POINT ( 'NONE',  ( 79.16712529945354504, 57.32610516721600646, 16.21374135531271321 ) ) ;
#67679 = AXIS2_PLACEMENT_3D ( 'NONE', #93137, #62689, #38393 ) ;
#67680 = DIRECTION ( 'NONE',  ( -0.9979227057047524996, 0.06442261589617470641, 0.000000000000000000 ) ) ;
#67681 = CARTESIAN_POINT ( 'NONE',  ( 38.67678797688638070, 22.73415679381825072, -6.890680421881970419E-14 ) ) ;
#67682 = CARTESIAN_POINT ( 'NONE',  ( 154.8679462054080318, 262.4078440388265676, 17.98338675682672871 ) ) ;
#67683 = CARTESIAN_POINT ( 'NONE',  ( 184.4117451362204179, 274.3934482926966894, 16.89443952929603654 ) ) ;
#67684 = LINE ( 'NONE', #98614, #84045 ) ;
#67685 = EDGE_CURVE ( 'NONE', #99270, #81649, #95650, .T. ) ;
#67686 = EDGE_CURVE ( 'NONE', #15116, #42801, #85957, .T. ) ;
#67687 = CARTESIAN_POINT ( 'NONE',  ( 84.29444876203692161, 50.65533303003044807, 13.79152508277374345 ) ) ;
#67688 = CARTESIAN_POINT ( 'NONE',  ( 187.9021647126450318, 299.0900879367926564, -0.5875642311020390363 ) ) ;
#67689 = DIRECTION ( 'NONE',  ( 0.7886751345947972114, -0.2113248654051897435, 0.5773502691896462702 ) ) ;
#67690 = CARTESIAN_POINT ( 'NONE',  ( 164.9483336881469882, 253.3134267730691249, -13.01688559776908427 ) ) ;
#67691 = CARTESIAN_POINT ( 'NONE',  ( 45.32607884611513072, 203.6427522451419065, 10.00000000000009415 ) ) ;
#67692 = EDGE_CURVE ( 'NONE', #30899, #5086, #53439, .T. ) ;
#67693 = AXIS2_PLACEMENT_3D ( 'NONE', #32216, #85989, #86484 ) ;
#67694 = CARTESIAN_POINT ( 'NONE',  ( -32.23964971562050863, 42.88792865763274875, 59.99999999999999289 ) ) ;
#67695 = CARTESIAN_POINT ( 'NONE',  ( 92.54224522822943300, 233.4244531367911009, -4.594050593750046652 ) ) ;
#67696 = CARTESIAN_POINT ( 'NONE',  ( 9.878523645489616811, 21.10171378149917487, 9.188101187500008038 ) ) ;
#67697 = CARTESIAN_POINT ( 'NONE',  ( 150.6533415055477008, 269.7077535128032082, 14.84621632544246062 ) ) ;
#67698 = EDGE_CURVE ( 'NONE', #11479, #38046, #31131, .T. ) ;
#67699 = CARTESIAN_POINT ( 'NONE',  ( 79.14312167556931854, 57.64441083166269664, 0.000000000000000000 ) ) ;
#67701 = CARTESIAN_POINT ( 'NONE',  ( 151.9591939046548532, 267.4459508103639109, 16.94431124488332685 ) ) ;
#67700 = CARTESIAN_POINT ( 'NONE',  ( 195.9920715006079490, 291.1787696107118677, 15.99608784761372071 ) ) ;
#67702 = B_SPLINE_CURVE_WITH_KNOTS ( 'NONE', 3,
 ( #82160, #66410, #73040, #51193, #81652, #89278, #41603, #27426, #74027, #43084 ),
 .UNSPECIFIED., .F., .F.,
 ( 4, 2, 2, 2, 4 ),
 ( 1.223810221527376531E-16, 0.0004261671925493324634, 0.0008523343850985425204, 0.001278501577647752577, 0.001704668770196962526 ),
 .UNSPECIFIED. ) ;
#67703 = CARTESIAN_POINT ( 'NONE',  ( 202.4098895269932257, 271.6205993907875040, -9.777904950607410939 ) ) ;
#67704 = CARTESIAN_POINT ( 'NONE',  ( 151.3898985249405200, 268.4319993325432847, -14.65018536945715510 ) ) ;
#67705 = CARTESIAN_POINT ( 'NONE',  ( 173.3835669379080002, 267.7164584622601069, -16.42089471915695142 ) ) ;
#67706 = CARTESIAN_POINT ( 'NONE',  ( 45.61829935282815995, 28.19860640527296525, 2.839279412974134775 ) ) ;
#67707 = CARTESIAN_POINT ( 'NONE',  ( 192.7705129102570822, 296.7586727687594816, -13.39629674907774692 ) ) ;
#67708 = CARTESIAN_POINT ( 'NONE',  ( 7.197458387703633775, 163.4155109091896065, 2.679491924311254714 ) ) ;
#67709 = ORIENTED_EDGE ( 'NONE', *, *, #16914, .T. ) ;
#67710 = CARTESIAN_POINT ( 'NONE',  ( 17.13451663979182626, 31.93396525600390135, 2.839279412974139660 ) ) ;
#67711 = CARTESIAN_POINT ( 'NONE',  ( -22.42236680055709641, 157.8615022471902591, 0.000000000000000000 ) ) ;
#67712 = CARTESIAN_POINT ( 'NONE',  ( 192.5143468344189728, 297.2023654272867361, -12.06830393602581530 ) ) ;
#67713 = DIRECTION ( 'NONE',  ( 0.8660254037844385966, 0.5000000000000002220, 7.511572993685832627E-16 ) ) ;
#67714 = EDGE_CURVE ( 'NONE', #90614, #12230, #6698, .T. ) ;
#67715 = ADVANCED_FACE ( 'NONE', ( #18838 ), #58794, .F. ) ;
#67716 = EDGE_LOOP ( 'NONE', ( #29769, #65391, #55663, #41060 ) ) ;
#67717 = CARTESIAN_POINT ( 'NONE',  ( 70.44740873159727812, 60.97318155419277019, 14.95046560365730137 ) ) ;
#67718 = CARTESIAN_POINT ( 'NONE',  ( 198.3150362131025588, 287.1552767044814800, 18.53472937702030521 ) ) ;
#67719 = CARTESIAN_POINT ( 'NONE',  ( 157.5665571574053274, 268.7536433892211676, 15.66352472898817005 ) ) ;
#67720 = DIRECTION ( 'NONE',  ( -0.000000000000000000, 0.000000000000000000, -1.000000000000000000 ) ) ;
#67721 = CARTESIAN_POINT ( 'NONE',  ( 143.4214980241629291, 253.6115022471902591, 10.00000000000009592 ) ) ;
#67722 = EDGE_LOOP ( 'NONE', ( #42315, #82774, #85478, #48728 ) ) ;
#67723 = CARTESIAN_POINT ( 'NONE',  ( 191.1741556875616936, 299.0312637876858730, -7.234752218208361896 ) ) ;
#67724 = AXIS2_PLACEMENT_3D ( 'NONE', #42736, #89896, #73673 ) ;
#67725 = ORIENTED_EDGE ( 'NONE', *, *, #82936, .T. ) ;
#67726 = CARTESIAN_POINT ( 'NONE',  ( 196.3812503439841350, 265.2916093225964005, -4.467972469483993514 ) ) ;
#67727 = CARTESIAN_POINT ( 'NONE',  ( 66.05805092528737532, 68.60151024935468911, 4.334430423793950382 ) ) ;
#67728 = ORIENTED_EDGE ( 'NONE', *, *, #54218, .F. ) ;
#67729 = CARTESIAN_POINT ( 'NONE',  ( 181.5366145304931251, 290.8356853596638416, -11.02968432880147276 ) ) ;
#67730 = ORIENTED_EDGE ( 'NONE', *, *, #70803, .F. ) ;
#67731 = VECTOR ( 'NONE', #96275, 1000.000000000000000 ) ;
#67732 = CARTESIAN_POINT ( 'NONE',  ( 50.22809564179084418, 188.2592609112380160, 2.679491924311254714 ) ) ;
#67733 = CARTESIAN_POINT ( 'NONE',  ( 205.5135663444060583, 274.6870567772484151, 11.64894633698279591 ) ) ;
#67734 = CARTESIAN_POINT ( 'NONE',  ( 190.6351135318297167, 278.8567387100862902, -16.51791015838286469 ) ) ;
#67735 = CARTESIAN_POINT ( 'NONE',  ( 88.11801461435689475, 44.35549720747543745, -4.463913325698411150 ) ) ;
#67736 = CARTESIAN_POINT ( 'NONE',  ( 201.3505934466285510, 281.8975373467312693, -16.83770227898004279 ) ) ;
#67737 = VECTOR ( 'NONE', #5089, 1000.000000000000114 ) ;
#67738 = VECTOR ( 'NONE', #70199, 1000.000000000000114 ) ;
#67739 = CARTESIAN_POINT ( 'NONE',  ( 37.18479240120036167, 39.65586893147759895, -7.433330006724137462 ) ) ;
#67740 = CARTESIAN_POINT ( 'NONE',  ( 78.87587414727704527, 58.57443402504730301, -16.19777088011071342 ) ) ;
#67741 = CARTESIAN_POINT ( 'NONE',  ( 164.3917948186382034, 274.8648391023518798, 14.67700265856982789 ) ) ;
#67742 = CARTESIAN_POINT ( 'NONE',  ( 87.66739418633859771, 45.39771433737033135, 6.570038411687281865 ) ) ;
#67743 = ORIENTED_EDGE ( 'NONE', *, *, #88222, .F. ) ;
#67744 = VERTEX_POINT ( 'NONE', #35010 ) ;
#67745 = CARTESIAN_POINT ( 'NONE',  ( 72.07243891101380484, 72.25875221884653854, -1.540673756851268283 ) ) ;
#67746 = CARTESIAN_POINT ( 'NONE',  ( 182.7510761219226367, 296.3781783941799972, 0.2738238006057779894 ) ) ;
#67747 = VECTOR ( 'NONE', #295, 1000.000000000000000 ) ;
#67749 = CARTESIAN_POINT ( 'NONE',  ( 165.8580863246405102, 274.0275451967436879, -15.18278219619561220 ) ) ;
#67748 = CARTESIAN_POINT ( 'NONE',  ( 174.3158243945931929, 257.3296975315241184, -11.92724987409102866 ) ) ;
#67750 = CARTESIAN_POINT ( 'NONE',  ( 165.0604371780248982, 244.7539318185670822, -1.421758703131883017 ) ) ;
#67751 = CARTESIAN_POINT ( 'NONE',  ( 68.24228953960120236, 68.25579693966338368, 7.841510002861836526 ) ) ;
#67752 = CARTESIAN_POINT ( 'NONE',  ( 156.5291010833105645, 261.3563040595462894, -17.73323587247505984 ) ) ;
#67753 = CARTESIAN_POINT ( 'NONE',  ( 82.10540399970709302, 40.78094143542895011, 1.224565905253431675 ) ) ;
#67754 = CARTESIAN_POINT ( 'NONE',  ( 170.4100357732785938, 288.8733093880243814, -4.275907419887600369 ) ) ;
#67755 = CARTESIAN_POINT ( 'NONE',  ( 77.05240863693448716, 63.46827552167501096, -15.45063268884610785 ) ) ;
#67756 = CARTESIAN_POINT ( 'NONE',  ( 178.0778109109441516, 255.4644557467126162, 4.928885342270551639 ) ) ;
#67757 = CARTESIAN_POINT ( 'NONE',  ( 106.6962611473900893, 244.6589784336661069, -6.496448406907675876E-16 ) ) ;
#67758 = EDGE_LOOP ( 'NONE', ( #24999, #51927, #13049, #43025 ) ) ;
#67759 = CARTESIAN_POINT ( 'NONE',  ( -19.65312891409030271, 93.06504152958497400, 177.5919119679930134 ) ) ;
#67760 = CARTESIAN_POINT ( 'NONE',  ( 39.54951596113196644, 25.76004757982093096, 5.678558825948272215 ) ) ;
#67761 = CARTESIAN_POINT ( 'NONE',  ( 191.5084189041053833, 275.1726936830797285, 16.11283378800830590 ) ) ;
#67762 = ORIENTED_EDGE ( 'NONE', *, *, #37707, .T. ) ;
#67763 = AXIS2_PLACEMENT_3D ( 'NONE', #55318, #96878, #57822 ) ;
#67764 = EDGE_CURVE ( 'NONE', #69911, #25397, #24351, .T. ) ;
#67765 = EDGE_LOOP ( 'NONE', ( #97253, #56678, #99745, #12290, #44151, #32859, #99532, #54663, #50793, #72753, #53134, #20540, #13197, #78727, #23446, #30990, #54411, #91203, #92072, #38110 ) ) ;
#67766 = CARTESIAN_POINT ( 'NONE',  ( 73.95565718806818722, 68.30423517461105121, -11.66005733018688773 ) ) ;
#67767 = CARTESIAN_POINT ( 'NONE',  ( -19.65312891409030271, 93.06504152958497400, 20.00000000000000355 ) ) ;
#67768 = CARTESIAN_POINT ( 'NONE',  ( 195.7617614321055157, 291.5776783508526364, 16.33009124109666033 ) ) ;
#67769 = CARTESIAN_POINT ( 'NONE',  ( 34.66168140297119038, 20.41603393254328580, -1.583844403245396437 ) ) ;
#67770 = LINE ( 'NONE', #29275, #36647 ) ;
#67771 = ORIENTED_EDGE ( 'NONE', *, *, #82938, .F. ) ;
#67772 = VERTEX_POINT ( 'NONE', #57314 ) ;
#67773 = CARTESIAN_POINT ( 'NONE',  ( 33.23512877817899636, 89.27284934918669990, 59.99999999999999289 ) ) ;
#67774 = EDGE_LOOP ( 'NONE', ( #59225, #99127, #84373, #90181 ) ) ;
#67775 = ADVANCED_FACE ( 'NONE', ( #50706 ), #88284, .T. ) ;
#67776 = CARTESIAN_POINT ( 'NONE',  ( 192.0661820761754655, 264.6237416276316026, -7.838450156236553390 ) ) ;
#67777 = DIRECTION ( 'NONE',  ( -0.9805290675673918876, -0.1963739994383708332, 0.000000000000000000 ) ) ;
#67778 = CARTESIAN_POINT ( 'NONE',  ( 82.95635226107660287, 46.18328785982301810, 11.04540840999154661 ) ) ;
#67780 = CARTESIAN_POINT ( 'NONE',  ( 156.9053997192012559, 280.1665077765802039, 5.870242185082841679 ) ) ;
#67779 = CARTESIAN_POINT ( 'NONE',  ( 184.3186041294927122, 288.8517029907596907, -13.19130426104491605 ) ) ;
#67781 = FACE_OUTER_BOUND ( 'NONE', #996, .T. ) ;
#67782 = EDGE_LOOP ( 'NONE', ( #81275, #42824, #91310, #27662, #69226, #41783, #12218, #90615, #74522, #93920, #50522, #49564, #90896, #39255, #46071, #81258, #59458, #25319, #81247, #7313, #4949, #94204, #7300, #75125, #1465, #85973, #45794, #97310, #17772, #49031, #50412, #56402, #69875, #100035, #88184, #15386, #9673, #60104, #89369, #11584, #42313, #33008, #77724, #38923, #64592, #46134, #12950, #11552, #12440, #89963, #92667, #50764, #33621, #66132, #40911, #98919, #93956, #61503, #21269, #42527, #55312, #42689, #99314, #97560, #26135, #77953, #61570, #78228, #30368, #46665, #43451, #94714, #10379, #21685, #45408, #52284, #77519, #38916, #19323, #42180, #52689, #10541, #21397, #52161, #49791, #93295, #83594, #26553, #77071, #67101, #30082, #38729, #49208, #24589, #23637, #63489, #72274, #11315, #43461, #26277, #255, #22979, #11183, #60631, #74688, #84017, #74609, #4476, #60868, #21387, #73393, #64251, #88613, #87346, #89391, #85921, #44430, #78613, #49444, #71002, #70201, #54319, #50408, #42665, #1518, #67342 ) ) ;
#67783 = CARTESIAN_POINT ( 'NONE',  ( 204.6487448717501252, 276.1849715073653897, 14.68262965895386607 ) ) ;
#67784 = CARTESIAN_POINT ( 'NONE',  ( 71.32140601477664177, 62.18330075258982959, 14.10657701148000065 ) ) ;
#67785 = CARTESIAN_POINT ( 'NONE',  ( 82.59165424625105345, 40.92964489041076348, -3.656265280277670282 ) ) ;
#67786 = CARTESIAN_POINT ( 'NONE',  ( 173.2829648012871644, 251.6371116567045476, -0.4726387605917980461 ) ) ;
#67788 = ADVANCED_FACE ( 'NONE', ( #58309 ), #89286, .F. ) ;
#67787 = CARTESIAN_POINT ( 'NONE',  ( 191.7054276324227260, 271.4226667163613911, -14.33086474662383836 ) ) ;
#67789 = DIRECTION ( 'NONE',  ( -1.000000000000000000, 0.000000000000000000, 0.000000000000000000 ) ) ;
#67790 = EDGE_CURVE ( 'NONE', #62928, #2866, #62945, .T. ) ;
#67791 = CARTESIAN_POINT ( 'NONE',  ( 84.25902073258765768, 45.00982432294706825, 8.916331552282562356 ) ) ;
#67792 = CARTESIAN_POINT ( 'NONE',  ( 146.7232198725432113, 245.5177522451417644, 5.000000000000051514 ) ) ;
#67793 = CARTESIAN_POINT ( 'NONE',  ( 191.1548165151656349, 283.2771438751705091, -16.59944851309598235 ) ) ;
#67794 = CARTESIAN_POINT ( 'NONE',  ( 71.99494277328302871, 70.73507547392100037, -6.404330814823480544 ) ) ;
#67795 = AXIS2_PLACEMENT_3D ( 'NONE', #55051, #39340, #69759 ) ;
#67796 = CARTESIAN_POINT ( 'NONE',  ( 77.06204113558260360, 224.4869531367911293, 4.594050593750046652 ) ) ;
#67797 = CARTESIAN_POINT ( 'NONE',  ( 159.9470087484377814, 253.6106496594791508, -16.54933891566789939 ) ) ;
#67798 = DIRECTION ( 'NONE',  ( 0.000000000000000000, 0.000000000000000000, 1.000000000000000000 ) ) ;
#67800 = DIRECTION ( 'NONE',  ( 0.3213938048432692374, -0.5566703992264209200, -0.7660444431189770143 ) ) ;
#67799 = AXIS2_PLACEMENT_3D ( 'NONE', #54326, #85822, #10261 ) ;
#67801 = AXIS2_PLACEMENT_3D ( 'NONE', #73293, #49473, #19610 ) ;
#67802 = VECTOR ( 'NONE', #37369, 1000.000000000000000 ) ;
#67803 = CARTESIAN_POINT ( 'NONE',  ( 161.6755750489535046, 250.6166850027345276, -13.01404233079112061 ) ) ;
#67804 = CARTESIAN_POINT ( 'NONE',  ( 66.10780414051450293, 68.63670250712272036, 1.777645618418523865 ) ) ;
#67805 = CARTESIAN_POINT ( 'NONE',  ( -20.77630098335523812, 95.20697321020988113, 45.19938011207119644 ) ) ;
#67806 =( NAMED_UNIT ( * ) PLANE_ANGLE_UNIT ( ) SI_UNIT ( $, .RADIAN. ) );
#67807 = CARTESIAN_POINT ( 'NONE',  ( 43.29939952211008602, 27.12755873383629890, -6.180339887498949025 ) ) ;
#67808 = CARTESIAN_POINT ( 'NONE',  ( 58.47569090598246788, 179.7419560658249509, -18.47570218321542868 ) ) ;
#67809 = DIRECTION ( 'NONE',  ( -7.401486830834377265E-16, 7.401486830834377265E-16, -1.000000000000000000 ) ) ;
#67810 = CARTESIAN_POINT ( 'NONE',  ( 71.97049335289784722, 72.00104994887270493, 2.833700686527681256 ) ) ;
#67811 = AXIS2_PLACEMENT_3D ( 'NONE', #18533, #39782, #10426 ) ;
#67812 = ADVANCED_FACE ( 'NONE', ( #41330 ), #58401, .T. ) ;
#67813 = CARTESIAN_POINT ( 'NONE',  ( 20.22912401222880519, 191.6744531367911293, 4.594050593750047540 ) ) ;
#67814 = ADVANCED_FACE ( 'NONE', ( #3270 ), #71163, .T. ) ;
#67815 = CARTESIAN_POINT ( 'NONE',  ( 196.3021893095863959, 290.6416298092292436, 17.45656988653421138 ) ) ;
#67816 = FACE_OUTER_BOUND ( 'NONE', #41798, .T. ) ;
#67817 = EDGE_CURVE ( 'NONE', #27077, #16029, #65045, .T. ) ;
#67818 = CARTESIAN_POINT ( 'NONE',  ( -61.08640853961129835, 36.64444830801921427, -10.00000000000000000 ) ) ;
#67819 = CARTESIAN_POINT ( 'NONE',  ( 71.59149729713742261, 72.39908022291972145, -1.330894502438451754 ) ) ;
#67820 = CARTESIAN_POINT ( 'NONE',  ( 47.34706511187656020, 188.9548013555409796, -4.594050593750042211 ) ) ;
#67821 = VECTOR ( 'NONE', #51887, 1000.000000000000114 ) ;
#67822 = CARTESIAN_POINT ( 'NONE',  ( 24.12224894148702248, 22.43085787977763701, -9.188101187500008038 ) ) ;
#67823 = CARTESIAN_POINT ( 'NONE',  ( 171.4669319504922385, 286.6849807880217895, 7.449759704774402636 ) ) ;
#67824 = DIRECTION ( 'NONE',  ( -1.000000000000000000, 0.000000000000000000, 0.000000000000000000 ) ) ;
#67825 = CARTESIAN_POINT ( 'NONE',  ( 43.71265818875933462, 33.43677371833804557, -10.00000000000000355 ) ) ;
#67826 = CARTESIAN_POINT ( 'NONE',  ( 205.1793861064249711, 275.2658739283173759, -14.08953480709093675 ) ) ;
#67827 = CARTESIAN_POINT ( 'NONE',  ( 199.9617906637654414, 268.0814914357001157, -6.510969352826504242 ) ) ;
#67828 = CARTESIAN_POINT ( 'NONE',  ( 75.71473607284134744, 57.60838419999664239, 16.52739276483602993 ) ) ;
#67829 = EDGE_CURVE ( 'NONE', #17199, #41822, #18965, .T. ) ;
#67830 = CARTESIAN_POINT ( 'NONE',  ( 179.0370437084304456, 276.4408010370251532, 16.31123546408546687 ) ) ;
#67831 = DIRECTION ( 'NONE',  ( -0.8660254037844387076, -0.4999999999999998890, -0.000000000000000000 ) ) ;
#67832 = DIRECTION ( 'NONE',  ( 0.5000000000000002220, -0.8660254037844387076, -0.000000000000000000 ) ) ;
#67833 = CARTESIAN_POINT ( 'NONE',  ( 163.3268748246386508, 256.0845449802187090, -14.91924337074942208 ) ) ;
#67834 = EDGE_CURVE ( 'NONE', #14298, #121, #51364, .T. ) ;
#67835 = CARTESIAN_POINT ( 'NONE',  ( 71.47791206682282450, 72.34364865201936823, -1.216664393387151488 ) ) ;
#67836 = CARTESIAN_POINT ( 'NONE',  ( 97.95516432547988472, 227.3615022471902591, -10.00000000000009592 ) ) ;
#67837 = CARTESIAN_POINT ( 'NONE',  ( 200.7583183585857967, 282.9233878912788214, 16.96937806979494212 ) ) ;
#67838 = CARTESIAN_POINT ( 'NONE',  ( 162.6022651249607804, 268.1935412368399625, -16.60785439006982855 ) ) ;
#67839 = ORIENTED_EDGE ( 'NONE', *, *, #7635, .F. ) ;
#67840 = CARTESIAN_POINT ( 'NONE',  ( 61.82584055745639517, 200.3768266524159856, -9.188101187500091527 ) ) ;
#67841 = ORIENTED_EDGE ( 'NONE', *, *, #87685, .T. ) ;
#67842 = CARTESIAN_POINT ( 'NONE',  ( 76.67567146729663818, 63.34086528488000312, -15.41964329106467346 ) ) ;
#67843 = CARTESIAN_POINT ( 'NONE',  ( 190.1693911629507738, 301.2639477917662703, -5.112716700269980485 ) ) ;
#67844 = B_SPLINE_CURVE_WITH_KNOTS ( 'NONE', 3,
 ( #88678, #19251, #88181, #34416, #43499, #3540, #42014, #72947, #11633, #58209, #95772, #65317, #66315, #64319, #96256, #50116, #96757, #26328, #42986, #89186, #56714, #87697, #81070, #97248, #64827, #57202, #51095, #4508, #26821, #57702, #42494, #80061, #73427, #72447, #95277, #18229, #58689, #27814, #4016, #73924, #89663, #3053, #19735, #65800, #12120, #50601 ),
 .UNSPECIFIED., .F., .F.,
 ( 4, 1, 2, 2, 1, 2, 2, 1, 1, 2, 2, 1, 1, 2, 2, 1, 1, 2, 2, 1, 1, 1, 2, 2, 1, 1, 1, 2, 2, 4 ),
 ( 0.000000000000000000, 0.06250000000001718070, 0.09375000000002577105, 0.1250000000000343614, 0.1875000000000512090, 0.2187500000000597578, 0.2500000000000683342, 0.3125000000000877076, 0.3437500000000959788, 0.3593750000001001976, 0.3750000000001043610, 0.4375000000001160738, 0.4687500000001217915, 0.4843750000001234568, 0.5000000000001250111, 0.5625000000001235678, 0.5937500000001214584, 0.6093750000001189049, 0.6250000000001162404, 0.6875000000000976996, 0.7187500000000870415, 0.7343750000000816014, 0.7421875000000790479, 0.7500000000000763833, 0.8125000000000579536, 0.8437500000000504041, 0.8593750000000451861, 0.8671875000000426326, 0.8750000000000400791, 1.000000000000000000 ),
 .UNSPECIFIED. ) ;
#67845 = CARTESIAN_POINT ( 'NONE',  ( 190.7405042774493324, 298.2747508605859821, 9.591131971744578877 ) ) ;
#67846 = ORIENTED_EDGE ( 'NONE', *, *, #99405, .F. ) ;
#67847 = CARTESIAN_POINT ( 'NONE',  ( -19.65312891409030271, 93.06504152958497400, -10.00000000000000888 ) ) ;
#67848 = CARTESIAN_POINT ( 'NONE',  ( 79.35516988872859656, 46.20647275665685783, -13.25012323394358127 ) ) ;
#67849 = CARTESIAN_POINT ( 'NONE',  ( 33.21408624426133827, 88.98998513028048762, 59.99999999999999289 ) ) ;
#67850 = CARTESIAN_POINT ( 'NONE',  ( 73.10697178893200032, 70.59305037885800971, -7.867401265066643390 ) ) ;
#67851 = DIRECTION ( 'NONE',  ( -0.4897629171537585258, 0.8718556560469402639, 0.000000000000000000 ) ) ;
#67852 = CARTESIAN_POINT ( 'NONE',  ( 116.4326846683273544, 226.4824982072973683, 3.021315404115420679E-15 ) ) ;
#67853 = VERTEX_POINT ( 'NONE', #87430 ) ;
#67854 = CARTESIAN_POINT ( 'NONE',  ( 23.25741983583088413, 25.37878583063841376, 9.188101187500006262 ) ) ;
#67855 = CARTESIAN_POINT ( 'NONE',  ( 79.74231254351767006, 44.89165149099596874, 11.47344340298346133 ) ) ;
#67856 = CARTESIAN_POINT ( 'NONE',  ( 72.34276783205245920, 70.28584662377375025, -7.644984185308641322 ) ) ;
#67857 = CARTESIAN_POINT ( 'NONE',  ( 155.3943609330853519, 266.5197459419810571, 17.05013864555025549 ) ) ;
#67858 = ORIENTED_EDGE ( 'NONE', *, *, #61460, .T. ) ;
#67859 = CARTESIAN_POINT ( 'NONE',  ( 76.38954935904880017, 53.24951976528166853, 16.44149648979542278 ) ) ;
#67860 = PLANE ( 'NONE',  #54473 ) ;
#67861 = ORIENTED_EDGE ( 'NONE', *, *, #186, .T. ) ;
#67862 = ORIENTED_EDGE ( 'NONE', *, *, #54218, .T. ) ;
#67864 = DIRECTION ( 'NONE',  ( -1.000000000000000000, 0.000000000000000000, 0.000000000000000000 ) ) ;
#67863 = CARTESIAN_POINT ( 'NONE',  ( 161.0109787555256275, 282.6433080515603251, -3.149774697262186507 ) ) ;
#67865 = CARTESIAN_POINT ( 'NONE',  ( 162.9383752892161397, 248.4294508267893491, -11.25953730674605957 ) ) ;
#67866 = CARTESIAN_POINT ( 'NONE',  ( 164.0741338217690668, 246.4622593432776796, 7.359073626423302983 ) ) ;
#67867 = CARTESIAN_POINT ( 'NONE',  ( 198.3523905153085423, 287.0905771551796306, 18.52598547438866206 ) ) ;
#67868 = CARTESIAN_POINT ( 'NONE',  ( 81.62315923969183018, 55.76054528319124159, 16.35706999678057727 ) ) ;
#67869 = CYLINDRICAL_SURFACE ( 'NONE', #90575, 10.00000000000010658 ) ;
#67870 = ADVANCED_FACE ( 'NONE', ( #79791 ), #72164, .T. ) ;
#67871 = CARTESIAN_POINT ( 'NONE',  ( 123.7191597644692393, 251.4244531367911293, -4.594050593750046652 ) ) ;
#67872 = VECTOR ( 'NONE', #70817, 1000.000000000000114 ) ;
#67873 = CARTESIAN_POINT ( 'NONE',  ( 80.01237403692960015, 210.8768266524159856, -9.188101187500091527 ) ) ;
#67874 = ORIENTED_EDGE ( 'NONE', *, *, #40393, .F. ) ;
#67875 = CARTESIAN_POINT ( 'NONE',  ( 170.1952319857192037, 264.1055084534233401, 17.01733452839312832 ) ) ;
#67876 = CARTESIAN_POINT ( 'NONE',  ( -6.281727404287059890, 25.63055774385195917, 10.00000000000000000 ) ) ;
#67877 = VERTEX_POINT ( 'NONE', #67023 ) ;
#67878 = AXIS2_PLACEMENT_3D ( 'NONE', #25857, #71954, #63336 ) ;
#67879 = CARTESIAN_POINT ( 'NONE',  ( 200.6938931563371398, 281.7467196835406753, 16.93566535195513723 ) ) ;
#67880 = ORIENTED_EDGE ( 'NONE', *, *, #82939, .F. ) ;
#67881 = EDGE_LOOP ( 'NONE', ( #84605, #90352, #82591, #25750 ) ) ;
#67882 = CARTESIAN_POINT ( 'NONE',  ( 84.80240350195582266, 219.7677522451418497, 10.00000000000009592 ) ) ;
#67883 = CARTESIAN_POINT ( 'NONE',  ( 206.8073682671177664, 270.4461261121818438, -4.970999383176901709 ) ) ;
#67884 = CARTESIAN_POINT ( 'NONE',  ( -2.233149578380279721, 169.5177522451418781, -10.00000000000009592 ) ) ;
#67885 = CARTESIAN_POINT ( 'NONE',  ( 147.2180753513904961, 275.6578090293250511, 0.4909717733184589261 ) ) ;
#67886 = CARTESIAN_POINT ( 'NONE',  ( 81.67557174052036828, 55.75159692325900096, 15.99231456053679423 ) ) ;
#67887 = CARTESIAN_POINT ( 'NONE',  ( 193.9204722154232741, 294.7668848255750049, 15.43855698596013859 ) ) ;
#67888 = CARTESIAN_POINT ( 'NONE',  ( 74.50030963965132003, 220.4865022471902876, -10.00000000000009592 ) ) ;
#67889 = LINE ( 'NONE', #28379, #65530 ) ;
#67890 = EDGE_LOOP ( 'NONE', ( #40041, #83010, #62350, #18449 ) ) ;
#67891 = AXIS2_PLACEMENT_3D ( 'NONE', #10995, #34273, #26673 ) ;
#67892 = B_SPLINE_SURFACE_WITH_KNOTS ( 'NONE', 3, 1, ( 
 ( #96128, #10487 ),
 ( #42363, #48991 ),
 ( #65671, #18093 ),
 ( #34283, #81921 ),
 ( #74313, #4895 ),
 ( #41368, #79927 ),
 ( #56577, #11996 ),
 ( #73296, #27192 ),
 ( #97130, #18597 ),
 ( #34770, #87564 ),
 ( #66672, #58081 ),
 ( #72306, #2915 ),
 ( #33807, #89060 ),
 ( #65180, #72817 ),
 ( #64691, #95643 ),
 ( #26682, #26190 ),
 ( #3408, #57068 ),
 ( #27696, #58566 ),
 ( #19613, #88049 ),
 ( #42853, #4378 ),
 ( #89537, #88543 ),
 ( #80432, #81424 ),
 ( #50471, #19109 ),
 ( #49985, #49476 ),
 ( #80941, #11509 ),
 ( #35278, #11005 ),
 ( #20098, #66184 ),
 ( #50969, #12497 ),
 ( #41879, #35779 ),
 ( #25697, #45357 ),
 ( #36269, #13978 ) ),
 .UNSPECIFIED., .F., .F., .F.,
 ( 4, 3, 3, 3, 3, 3, 3, 3, 3, 3, 4 ),
 ( 2, 2 ),
 ( 0.000000000000000000, 0.1122669598086675907, 0.2243161639709637112, 0.3396355846219057395, 0.4553962076585009733, 0.5677860799922324064, 0.6749047109689443324, 0.7773884377078320584, 0.8775581155834342173, 0.9782364162377927830, 1.000000000000000000 ),
 ( 0.000000000000000000, 1.000000000000000000 ),
 .UNSPECIFIED. ) ;
#67893 = CARTESIAN_POINT ( 'NONE',  ( 161.5489325017909437, 250.8360363288196311, -12.69404255266198867 ) ) ;
#67894 = ORIENTED_EDGE ( 'NONE', *, *, #65995, .T. ) ;
#67895 = CARTESIAN_POINT ( 'NONE',  ( 163.9712236968778711, 260.5412544304000448, -16.17885422200931345 ) ) ;
#67896 = CARTESIAN_POINT ( 'NONE',  ( 164.3420876084788347, 246.7786081070618991, 5.291571273027417810 ) ) ;
#67897 = EDGE_CURVE ( 'NONE', #86378, #94311, #72689, .T. ) ;
#67898 = CIRCLE ( 'NONE', #74433, 70.00000000000001421 ) ;
#67899 = CARTESIAN_POINT ( 'NONE',  ( 196.4808189786114951, 290.3322341467384717, -17.84817245450773271 ) ) ;
#67900 = CARTESIAN_POINT ( 'NONE',  ( 195.0720061818549880, 279.3691163892412987, 16.41141732502160622 ) ) ;
#67901 = CARTESIAN_POINT ( 'NONE',  ( 156.1797501576022569, 269.6359076562748101, -16.17116838778184018 ) ) ;
#67902 = CARTESIAN_POINT ( 'NONE',  ( 133.0017827873424494, 259.8464784336661637, 1.353441290958777327E-15 ) ) ;
#67903 = ORIENTED_EDGE ( 'NONE', *, *, #84494, .F. ) ;
#67904 = CARTESIAN_POINT ( 'NONE',  ( 81.28967588850363768, 44.30488066837197181, -10.06605756411466857 ) ) ;
#67905 = CARTESIAN_POINT ( 'NONE',  ( 73.03327713030915902, 67.29942500083180335, -12.06190433575985210 ) ) ;
#67906 = CARTESIAN_POINT ( 'NONE',  ( 183.5953950971229744, 289.9057545191589043, -13.74357891376704544 ) ) ;
#67907 = EDGE_CURVE ( 'NONE', #90329, #61768, #26690, .T. ) ;
#67908 = CARTESIAN_POINT ( 'NONE',  ( 79.51860058571794809, 59.43534202413220413, -16.20610000061713407 ) ) ;
#67909 = EDGE_CURVE ( 'NONE', #35604, #54122, #54458, .T. ) ;
#67910 = CARTESIAN_POINT ( 'NONE',  ( 71.09310640586875252, 67.27851065979278644, -10.44888890291803030 ) ) ;
#67911 = ORIENTED_EDGE ( 'NONE', *, *, #12126, .T. ) ;
#67912 = CARTESIAN_POINT ( 'NONE',  ( 75.84856439504059722, 51.76521084193598909, 15.76359423700355755 ) ) ;
#67913 = CARTESIAN_POINT ( 'NONE',  ( 182.2364423096436497, 275.3866057150171969, -16.52884722923822380 ) ) ;
#67914 = CARTESIAN_POINT ( 'NONE',  ( 72.62875853510576007, 71.42134003127335973, -5.810135019581663229 ) ) ;
#67915 = CARTESIAN_POINT ( 'NONE',  ( 80.57406551557809848, 49.71488727638417515, 14.27527881381214847 ) ) ;
#67916 = CARTESIAN_POINT ( 'NONE',  ( 201.6192218642991349, 267.5720127751881705, 0.8431288817150176529 ) ) ;
#67917 = CARTESIAN_POINT ( 'NONE',  ( 197.0461256858581294, 265.3860351196537408, 0.8220420341949939980 ) ) ;
#67918 = CARTESIAN_POINT ( 'NONE',  ( 147.5498377207569263, 275.0831797495432056, 4.097967709737811326 ) ) ;
#67919 = CARTESIAN_POINT ( 'NONE',  ( 186.6116014577160058, 282.5156129276005004, 16.21094600413495357 ) ) ;
#67920 = CARTESIAN_POINT ( 'NONE',  ( 157.6921299354026189, 257.5162143285667753, -18.18720974599499840 ) ) ;
#67921 = CARTESIAN_POINT ( 'NONE',  ( 196.7445171685907894, 269.9811659379847129, 11.91596940811355765 ) ) ;
#67922 = CARTESIAN_POINT ( 'NONE',  ( 19.73933908736162124, 30.13478043621388380, 8.090169943749478065 ) ) ;
#67923 = DIRECTION ( 'NONE',  ( 0.000000000000000000, -0.000000000000000000, 1.000000000000000000 ) ) ;
#67924 = CARTESIAN_POINT ( 'NONE',  ( 205.2615535051069742, 274.5664020556757237, 11.36949175128528111 ) ) ;
#67925 = LINE ( 'NONE', #97848, #77404 ) ;
#67926 = CARTESIAN_POINT ( 'NONE',  ( 198.3449891235413531, 287.1033967417670283, 16.95540786497457120 ) ) ;
#67927 = CARTESIAN_POINT ( 'NONE',  ( 72.29835728126460026, 71.99361178985304832, -3.639781104770197562 ) ) ;
#67928 =( BOUNDED_CURVE ( )  B_SPLINE_CURVE ( 2, ( #42019, #57210, #34905, #35909, #96765, #89192, #58214, #81560, #59184 ),
 .UNSPECIFIED., .F., .T. ) 
 B_SPLINE_CURVE_WITH_KNOTS ( ( 3, 2, 2, 2, 3 ),
 ( 0.2862903225806451846, 0.2876344086021505597, 0.2903225806451613100, 0.2930107526881720603, 0.2943548387096774355 ),
 .UNSPECIFIED. ) 
 CURVE ( )  GEOMETRIC_REPRESENTATION_ITEM ( )  RATIONAL_B_SPLINE_CURVE ( ( 0.9330127018922194093, 0.9330127018922194093, 1.000000000000000000, 0.8660254037844387076, 1.000000000000000000, 0.8660254037844387076, 1.000000000000000000, 0.9330127018922194093, 0.9330127018922194093 ) ) 
 REPRESENTATION_ITEM ( '' )  );
#67929 = EDGE_CURVE ( 'NONE', #46611, #72868, #1404, .T. ) ;
#67930 = CARTESIAN_POINT ( 'NONE',  ( 151.9193722952498717, 248.5177522451417644, 5.000000000000051514 ) ) ;
#67931 = CARTESIAN_POINT ( 'NONE',  ( 175.4039180538638050, 286.4985578832265105, -12.71199677751706503 ) ) ;
#67932 = EDGE_LOOP ( 'NONE', ( #98899, #74379, #81095, #41350 ) ) ;
#67933 = AXIS2_PLACEMENT_3D ( 'NONE', #93964, #63519, #76725 ) ;
#67934 = CARTESIAN_POINT ( 'NONE',  ( 66.90338203151232221, 68.17684508661041320, -6.595631787949806757 ) ) ;
#67935 = CARTESIAN_POINT ( 'NONE',  ( 72.95589830849367274, 70.34902050982091737, -8.120948148125345156 ) ) ;
#67936 = CARTESIAN_POINT ( 'NONE',  ( 150.7133245577828689, 269.6038598187387834, -14.58664962216439598 ) ) ;
#67937 = CARTESIAN_POINT ( 'NONE',  ( 10.54098545103790840, 167.7048013555410080, 4.594050593750051981 ) ) ;
#67938 = CARTESIAN_POINT ( 'NONE',  ( 181.6434012404215821, 276.3923190036793471, -17.32158067431182147 ) ) ;
#67939 = CARTESIAN_POINT ( 'NONE',  ( 24.66009930550170282, 22.43677371833801715, -10.00000000000000355 ) ) ;
#67940 = CARTESIAN_POINT ( 'NONE',  ( 85.45224931747254971, 49.07960547787612882, 12.36068907126763960 ) ) ;
#67941 = CARTESIAN_POINT ( 'NONE',  ( 157.6500260163024620, 257.5891404556457474, -18.23450497588216379 ) ) ;
#67942 = CARTESIAN_POINT ( 'NONE',  ( 71.91831898124014799, 71.71822762647316551, -3.866383333238705866 ) ) ;
#67943 = CARTESIAN_POINT ( 'NONE',  ( 158.2916163944991865, 282.4761429051572463, -3.043442648455108479 ) ) ;
#67944 = ADVANCED_FACE ( 'NONE', ( #74159 ), #21434, .F. ) ;
#67945 = CARTESIAN_POINT ( 'NONE',  ( 198.2505066714982149, 285.2670451491296149, 0.000000000000000000 ) ) ;
#67946 = CARTESIAN_POINT ( 'NONE',  ( 198.1915864813676933, 287.3690979120270867, 17.02875488965938189 ) ) ;
#67947 = AXIS2_PLACEMENT_3D ( 'NONE', #91749, #7107, #92743 ) ;
#67948 = CARTESIAN_POINT ( 'NONE',  ( 183.0954089547747685, 295.7244723176602292, 1.069539124438823929 ) ) ;
#67949 = CARTESIAN_POINT ( 'NONE',  ( 56.45811372747549228, 216.7365022471903444, 2.944929066748280225E-16 ) ) ;
#67950 = CARTESIAN_POINT ( 'NONE',  ( 41.28778705816291961, 32.03677371833806120, 10.00000000000000533 ) ) ;
#67951 = CARTESIAN_POINT ( 'NONE',  ( 147.9748066657072627, 274.3471119452502762, 9.387104374042873900 ) ) ;
#67952 = CARTESIAN_POINT ( 'NONE',  ( 9.079046938504149011, 185.2369531367911293, -4.594050593750048428 ) ) ;
#67953 = CARTESIAN_POINT ( 'NONE',  ( 80.86586985908986946, 155.7185146834693512, 3.300000000000006484 ) ) ;
#67954 = CARTESIAN_POINT ( 'NONE',  ( 37.43858582280105907, 33.56628583063844218, 9.188101187500006262 ) ) ;
#67955 = FACE_OUTER_BOUND ( 'NONE', #25663, .T. ) ;
#67956 = CYLINDRICAL_SURFACE ( 'NONE', #1422, 17.82106496071139645 ) ;
#67957 = CARTESIAN_POINT ( 'NONE',  ( 185.4027513566571201, 266.5856925186359945, 13.20686768916569243 ) ) ;
#67958 = CARTESIAN_POINT ( 'NONE',  ( 171.6154833087297789, 255.2606305366970503, 12.53362356821959978 ) ) ;
#67959 = CARTESIAN_POINT ( 'NONE',  ( 163.8257527437161514, 281.4247057528291975, 8.856190409526824681 ) ) ;
#67960 = CONTEXT_DEPENDENT_SHAPE_REPRESENTATION ( #60624, #10320 ) ;
#67961 = EDGE_CURVE ( 'NONE', #67254, #71229, #75151, .T. ) ;
#67962 = CARTESIAN_POINT ( 'NONE',  ( 18.06126741312425921, 22.37878583063840310, 9.188101187500006262 ) ) ;
#67963 = CARTESIAN_POINT ( 'NONE',  ( 190.4750160083620472, 300.7345900314585947, -1.159659205620361400 ) ) ;
#67964 = CARTESIAN_POINT ( 'NONE',  ( 71.70303330742534342, 59.04301762528319131, 15.35811543448661531 ) ) ;
#67965 = CARTESIAN_POINT ( 'NONE',  ( 196.0051728737935832, 265.8263463907475170, 8.406970388261065352 ) ) ;
#67966 = EDGE_LOOP ( 'NONE', ( #647, #55900, #72289, #5075 ) ) ;
#67967 = CARTESIAN_POINT ( 'NONE',  ( 185.4084872802253585, 290.9630408421091943, 12.18521566798547795 ) ) ;
#67968 = CARTESIAN_POINT ( 'NONE',  ( 88.28714907786486776, 44.35112667690796684, 2.372838034520684314 ) ) ;
#67969 = ORIENTED_EDGE ( 'NONE', *, *, #98080, .T. ) ;
#67970 = FACE_OUTER_BOUND ( 'NONE', #33364, .T. ) ;
#67971 = CARTESIAN_POINT ( 'NONE',  ( 68.86429500837576256, 70.35746111282902859, -0.7754140821421253715 ) ) ;
#67972 = CARTESIAN_POINT ( 'NONE',  ( 24.85415417228448121, 26.30066082961422680, -10.00000000000000533 ) ) ;
#67973 = CARTESIAN_POINT ( 'NONE',  ( 202.8151641853381477, 279.3608264160075692, -16.28741359973609448 ) ) ;
#67974 = ADVANCED_FACE ( 'NONE', ( #12351 ), #5728, .F. ) ;
#67975 = ORIENTED_EDGE ( 'NONE', *, *, #2588, .F. ) ;
#67976 = ORIENTED_EDGE ( 'NONE', *, *, #5384, .F. ) ;
#67978 = CARTESIAN_POINT ( 'NONE',  ( 149.8622666665893632, 273.0779353264732663, 11.47145096717591528 ) ) ;
#67977 = CARTESIAN_POINT ( 'NONE',  ( 186.4055657536957540, 271.9883927876483654, -16.52192294486705038 ) ) ;
#67979 = ORIENTED_EDGE ( 'NONE', *, *, #44364, .F. ) ;
#67980 = CARTESIAN_POINT ( 'NONE',  ( 150.6533415055477008, 269.7077535128032082, 14.84621632544246062 ) ) ;
#67981 = CARTESIAN_POINT ( 'NONE',  ( 70.27209832060933081, 65.59710146439343248, 12.14989064463910040 ) ) ;
#67982 = CARTESIAN_POINT ( 'NONE',  ( 80.32304696881857353, 58.04909235870844952, 16.26133398640363126 ) ) ;
#67983 = DIRECTION ( 'NONE',  ( 0.000000000000000000, 0.000000000000000000, 1.000000000000000000 ) ) ;
#67985 = ORIENTED_EDGE ( 'NONE', *, *, #33447, .F. ) ;
#67984 = EDGE_CURVE ( 'NONE', #85768, #84087, #13427, .T. ) ;
#67986 = CARTESIAN_POINT ( 'NONE',  ( 147.6300909839706321, 274.9441770201837585, 8.328755691084779755 ) ) ;
#67987 = ORIENTED_EDGE ( 'NONE', *, *, #73005, .T. ) ;
#67988 = CARTESIAN_POINT ( 'NONE',  ( 205.9240884482826175, 273.9760116357041966, 10.27504561427317142 ) ) ;
#67989 = CARTESIAN_POINT ( 'NONE',  ( 74.84928291413068280, 64.80482755438514175, 13.90247044424336309 ) ) ;
#67990 = ORIENTED_EDGE ( 'NONE', *, *, #15192, .F. ) ;
#67991 = CARTESIAN_POINT ( 'NONE',  ( 190.0707697440390689, 301.4347651000360884, 4.271360729158901748 ) ) ;
#67992 = CARTESIAN_POINT ( 'NONE',  ( 172.3986314675530309, 263.7922717222033384, -16.89442142407995107 ) ) ;
#67993 = ORIENTED_EDGE ( 'NONE', *, *, #16047, .F. ) ;
#67994 = CARTESIAN_POINT ( 'NONE',  ( -8.010917706491644807, 72.92290384248846635, 15.00660040458968503 ) ) ;
#67995 = CARTESIAN_POINT ( 'NONE',  ( 149.0237174825091415, 274.5263358477994871, 9.114370506038131481 ) ) ;
#67996 = DIRECTION ( 'NONE',  ( 0.8660254037844385966, 0.4999999999999999445, 0.000000000000000000 ) ) ;
#67997 = CARTESIAN_POINT ( 'NONE',  ( 33.00035307926291495, 37.79103043416552055, 8.090169943749478065 ) ) ;
#67998 = ORIENTED_EDGE ( 'NONE', *, *, #56357, .F. ) ;
#67999 = ORIENTED_EDGE ( 'NONE', *, *, #7207, .F. ) ;
#68000 = CARTESIAN_POINT ( 'NONE',  ( 73.61712177582347749, 69.75295271933504182, 9.424901393032142138 ) ) ;
#68001 = CARTESIAN_POINT ( 'NONE',  ( 81.82006362146523770, 42.66096406068295011, -7.441249945456725357 ) ) ;
#68002 = CARTESIAN_POINT ( 'NONE',  ( 190.9335643195044838, 299.9403610588350944, -4.692880224846124548 ) ) ;
#68003 = LINE ( 'NONE', #57912, #64190 ) ;
#68004 = CARTESIAN_POINT ( 'NONE',  ( 190.7516742497373059, 300.2554039010641418, 4.342609251298632067 ) ) ;
#68005 = CARTESIAN_POINT ( 'NONE',  ( 152.9262073036446168, 265.7710344717137900, 16.19159804214501008 ) ) ;
#68006 = CARTESIAN_POINT ( 'NONE',  ( 191.1100977347303456, 299.6345962144299619, 9.508964441650325838 ) ) ;
#68007 = CARTESIAN_POINT ( 'NONE',  ( 191.8453338867844877, 298.3611298435110371, -9.039024722281077118 ) ) ;
#68008 = CARTESIAN_POINT ( 'NONE',  ( -18.76211276271274997, 171.5217562850347406, 1.224646799147364892E-15 ) ) ;
#68009 = DIRECTION ( 'NONE',  ( -0.8452030915256490973, -0.5344452582589588330, 0.000000000000000000 ) ) ;
#68010 = CARTESIAN_POINT ( 'NONE',  ( 68.04803862442108198, 70.41495816557659282, 0.2082392626603555841 ) ) ;
#68011 = CARTESIAN_POINT ( 'NONE',  ( 71.47791206682282450, 72.34364865201936823, -1.216664393387151488 ) ) ;
#68012 = CARTESIAN_POINT ( 'NONE',  ( 39.81344631580554250, 23.39040679176985904, -6.890680421881970419E-14 ) ) ;
#68013 = LINE ( 'NONE', #29520, #72349 ) ;
#68014 = ORIENTED_EDGE ( 'NONE', *, *, #30515, .T. ) ;
#68015 = CARTESIAN_POINT ( 'NONE',  ( 149.7327968382200538, 271.3021836472514678, -12.62649163920564988 ) ) ;
#68016 = DIRECTION ( 'NONE',  ( 0.5000000000000048850, -0.8660254037844358210, 0.000000000000000000 ) ) ;
#68017 = CARTESIAN_POINT ( 'NONE',  ( 149.1235161367207240, 273.2503626557173106, 9.887280554828780765 ) ) ;
#68018 = DIRECTION ( 'NONE',  ( 0.000000000000000000, -0.000000000000000000, -1.000000000000000000 ) ) ;
#68019 = EDGE_CURVE ( 'NONE', #20265, #32467, #35634, .T. ) ;
#68020 = CARTESIAN_POINT ( 'NONE',  ( 183.1940556755976104, 284.5769249909878909, -14.99598816525897504 ) ) ;
#68021 = EDGE_CURVE ( 'NONE', #31449, #94911, #27559, .T. ) ;
#68022 = CARTESIAN_POINT ( 'NONE',  ( 73.69427750731760796, 56.72192345538155678, -16.50807356290637173 ) ) ;
#68023 = AXIS2_PLACEMENT_3D ( 'NONE', #50701, #21315, #42596 ) ;
#68024 = VERTEX_POINT ( 'NONE', #28030 ) ;
#68025 = CARTESIAN_POINT ( 'NONE',  ( 170.4442219353800283, 255.4737032154624217, -11.62118961212506996 ) ) ;
#68026 = CARTESIAN_POINT ( 'NONE',  ( -46.31994871380127421, 28.06264584988120347, -10.00000000000000000 ) ) ;
#68027 = ADVANCED_FACE ( 'NONE', ( #60905 ), #84272, .T. ) ;
#68028 = CARTESIAN_POINT ( 'NONE',  ( 72.40589440182066028, 71.76200285602328677, 5.709577571112527394 ) ) ;
#68029 = EDGE_CURVE ( 'NONE', #62277, #89481, #91870, .T. ) ;
#68030 = CARTESIAN_POINT ( 'NONE',  ( 44.60439100962815218, 189.8927522451418213, -10.00000000000009059 ) ) ;
#68031 = CARTESIAN_POINT ( 'NONE',  ( 113.4351080945290278, 245.4869531367911009, 4.594050593750046652 ) ) ;
#68032 = CARTESIAN_POINT ( 'NONE',  ( 145.0115229932138163, 242.9824982072973683, 3.021315404115420679E-15 ) ) ;
#68033 = CARTESIAN_POINT ( 'NONE',  ( 66.85524610400479162, 67.34209505064850987, -6.990925417236247164 ) ) ;
#68034 = CARTESIAN_POINT ( 'NONE',  ( 157.1135969804030310, 258.5182628004787944, 17.19660297500358226 ) ) ;
#68035 = CARTESIAN_POINT ( 'NONE',  ( 175.7684342158191555, 253.0281421584272721, -4.824161474433333652 ) ) ;
#68036 = CARTESIAN_POINT ( 'NONE',  ( 23.55782238408397689, 196.6589784336661637, -6.496448406907675876E-16 ) ) ;
#68037 = DIRECTION ( 'NONE',  ( -0.8660254037844375974, -0.5000000000000016653, 0.000000000000000000 ) ) ;
#68038 = ORIENTED_EDGE ( 'NONE', *, *, #3598, .T. ) ;
#68039 = CARTESIAN_POINT ( 'NONE',  ( 191.2827847134780654, 298.6246597018299553, 8.274781095337747416 ) ) ;
#68040 = CARTESIAN_POINT ( 'NONE',  ( 181.7309266518924744, 267.1772924037041435, 15.05018902152789906 ) ) ;
#68041 = CARTESIAN_POINT ( 'NONE',  ( 71.11777852545861833, 71.64480956778183440, -1.649610073217940398 ) ) ;
#68042 = CARTESIAN_POINT ( 'NONE',  ( 190.7908437487391780, 300.1875603386860689, -4.317984972589949955 ) ) ;
#68043 = CARTESIAN_POINT ( 'NONE',  ( 81.69476477490047728, 41.61625632775264449, -5.521120823311375325 ) ) ;
#68044 = CARTESIAN_POINT ( 'NONE',  ( 196.9080397933726942, 269.7016881256661804, 12.39056067425276630 ) ) ;
#68045 = CARTESIAN_POINT ( 'NONE',  ( 176.8277677751233625, 285.8241435940994393, -12.06137026359123432 ) ) ;
#68046 = CARTESIAN_POINT ( 'NONE',  ( 182.2730873982721391, 262.7650441757560884, 12.77154113705879901 ) ) ;
#68047 = CARTESIAN_POINT ( 'NONE',  ( 112.1543725048143614, 228.8927522451418213, -10.00000000000009059 ) ) ;
#68048 = ORIENTED_EDGE ( 'NONE', *, *, #81869, .F. ) ;
#68049 = CARTESIAN_POINT ( 'NONE',  ( 198.3800612005289281, 267.8743580568481093, -8.018411648243336742 ) ) ;
#68050 = CARTESIAN_POINT ( 'NONE',  ( 162.6264071486809542, 248.9697954965390920, 10.36322805486644683 ) ) ;
#68051 = CARTESIAN_POINT ( 'NONE',  ( 207.6875671281972870, 270.9215769640275653, -2.211577121115235300 ) ) ;
#68052 = CARTESIAN_POINT ( 'NONE',  ( 9.052243966459650792, 176.0333772461660828, 9.188101187500095079 ) ) ;
#68053 = CARTESIAN_POINT ( 'NONE',  ( 6.688470478837179378, 19.56454794089038884, 10.00000000000000355 ) ) ;
#68054 = CARTESIAN_POINT ( 'NONE',  ( -16.91593106145283087, 105.3412939927731173, 44.39172944529203590 ) ) ;
#68055 = CARTESIAN_POINT ( 'NONE',  ( 71.59361115369081574, 59.50488489875972675, -15.70950865668593188 ) ) ;
#68056 = CARTESIAN_POINT ( 'NONE',  ( 73.17035075335006411, 69.75913569003169812, 9.110019559117217725 ) ) ;
#68058 = CARTESIAN_POINT ( 'NONE',  ( 62.15060008387555257, 200.5643266524159856, -9.188101187500093303 ) ) ;
#68057 = CARTESIAN_POINT ( 'NONE',  ( 198.2470831392502646, 277.3477145600038511, -15.34583922742456430 ) ) ;
#68059 = CARTESIAN_POINT ( 'NONE',  ( 208.3117541397001844, 269.8404533466799080, 2.895672523916592578 ) ) ;
#68060 = CARTESIAN_POINT ( 'NONE',  ( 73.60341520791058656, 55.46590081124723071, 16.11001259655113316 ) ) ;
#68061 = CARTESIAN_POINT ( 'NONE',  ( -32.35580655284284290, 96.47003284356902952, 44.23339904099978526 ) ) ;
#68062 = CARTESIAN_POINT ( 'NONE',  ( 66.33274517095223644, 68.13410765588996298, -4.505544708085248651 ) ) ;
#68063 = VERTEX_POINT ( 'NONE', #9097 ) ;
#68064 = CARTESIAN_POINT ( 'NONE',  ( 22.53878541258507795, 170.4865022471901455, 1.119607411625061291E-15 ) ) ;
#68065 = CARTESIAN_POINT ( 'NONE',  ( 207.5215400641004351, 271.2091442744748520, 2.886080616848571534 ) ) ;
#68066 = CARTESIAN_POINT ( 'NONE',  ( 141.2025682470151366, 243.1423013555409796, -4.594050593750043987 ) ) ;
#68067 = CARTESIAN_POINT ( 'NONE',  ( 30.02984208470827454, 19.19860640527293327, 2.839279412974134775 ) ) ;
#68068 = DIRECTION ( 'NONE',  ( -0.5951734788405994570, 0.8035972437015811431, 0.000000000000000000 ) ) ;
#68069 = CARTESIAN_POINT ( 'NONE',  ( 83.83309058964263727, 51.93283190383716885, -14.92096955093740362 ) ) ;
#68070 = CARTESIAN_POINT ( 'NONE',  ( 73.97708595465037718, 203.5177522451417929, 5.000000000000051514 ) ) ;
#68072 = CARTESIAN_POINT ( 'NONE',  ( 74.72173318163055455, 67.07206250228034605, 12.96729955693541569 ) ) ;
#68071 = CARTESIAN_POINT ( 'NONE',  ( 84.08513284186659575, 41.35086568230796189, -1.059521581035436366 ) ) ;
#68073 = B_SPLINE_CURVE_WITH_KNOTS ( 'NONE', 3,
 ( #38451, #21766, #15147, #67365 ),
 .UNSPECIFIED., .F., .F.,
 ( 4, 4 ),
 ( 0.04698075955296258932, 0.04887120950165263489 ),
 .UNSPECIFIED. ) ;
#68074 = CARTESIAN_POINT ( 'NONE',  ( 69.13163807604178146, 64.30638122866986350, 12.00391912781525505 ) ) ;
#68075 = ORIENTED_EDGE ( 'NONE', *, *, #67139, .T. ) ;
#68076 = CARTESIAN_POINT ( 'NONE',  ( 79.70677143361787387, 46.01134058561531504, 12.98241517792750699 ) ) ;
#68077 = CARTESIAN_POINT ( 'NONE',  ( 208.3927134385237991, 269.7002277277721873, -0.7867555975313439420 ) ) ;
#68078 = ADVANCED_FACE ( 'NONE', ( #33394 ), #7814, .F. ) ;
#68079 = CARTESIAN_POINT ( 'NONE',  ( 151.9329737526506960, 268.5275331363711757, -15.02064953801001757 ) ) ;
#68080 = DIRECTION ( 'NONE',  ( 0.000000000000000000, -0.000000000000000000, 1.000000000000000000 ) ) ;
#68081 = CARTESIAN_POINT ( 'NONE',  ( 6.414422030351863313, 19.10171378149916777, 9.188101187500008038 ) ) ;
#68082 = VERTEX_POINT ( 'NONE', #26795 ) ;
#68083 = LINE ( 'NONE', #43279, #73217 ) ;
#68084 = CARTESIAN_POINT ( 'NONE',  ( 169.8816400817638623, 284.2167566447287754, -11.81736336128774134 ) ) ;
#68085 = CARTESIAN_POINT ( 'NONE',  ( 75.40537576526305941, 53.18750470143674391, 16.48738048042240223 ) ) ;
#68086 = CARTESIAN_POINT ( 'NONE',  ( 71.47384123275854506, 72.35069954344791654, 1.100233114707650506 ) ) ;
#68087 = CARTESIAN_POINT ( 'NONE',  ( 148.7541592998676947, 273.6883713208891322, -8.831557984469299072 ) ) ;
#68088 = FACE_BOUND ( 'NONE', #58609, .T. ) ;
#68089 = FACE_OUTER_BOUND ( 'NONE', #34126, .T. ) ;
#68090 = CARTESIAN_POINT ( 'NONE',  ( 143.4214980241629291, 253.6115022471902591, 10.00000000000009592 ) ) ;
#68091 = VECTOR ( 'NONE', #83335, 1000.000000000000000 ) ;
#68092 = CARTESIAN_POINT ( 'NONE',  ( 200.7134601498536028, 283.0010845879393742, -16.98649239173277792 ) ) ;
#68093 = DIRECTION ( 'NONE',  ( -0.8660254037844387076, -0.4999999999999998890, -0.000000000000000000 ) ) ;
#68094 = CARTESIAN_POINT ( 'NONE',  ( 7.357472841178069878, 27.18080186712591484, 3.090169943749475401 ) ) ;
#68095 = CARTESIAN_POINT ( 'NONE',  ( 84.01508409052884474, 48.27837738685627045, 12.82889063469658630 ) ) ;
#68096 = ORIENTED_EDGE ( 'NONE', *, *, #93944, .F. ) ;
#68097 = CARTESIAN_POINT ( 'NONE',  ( 149.0802055316563326, 272.4325049467973940, 12.84384348890831085 ) ) ;
#68098 = EDGE_CURVE ( 'NONE', #45306, #51277, #87226, .T. ) ;
#68099 = DIRECTION ( 'NONE',  ( -0.000000000000000000, -0.000000000000000000, -1.000000000000000000 ) ) ;
#68100 = CARTESIAN_POINT ( 'NONE',  ( 86.60342109795770682, 45.00234098353818979, -6.966275957478193170 ) ) ;
#68101 = ORIENTED_EDGE ( 'NONE', *, *, #95869, .T. ) ;
#68102 = CARTESIAN_POINT ( 'NONE',  ( 191.8453338867844877, 298.3611298435110371, -9.039024722281077118 ) ) ;
#68103 = CARTESIAN_POINT ( 'NONE',  ( 79.33144427914538710, 59.81174478577791831, -16.15603203001268540 ) ) ;
#68104 = CARTESIAN_POINT ( 'NONE',  ( 164.3853877993040840, 245.9231516401292197, 5.995325337583643943 ) ) ;
#68105 = CARTESIAN_POINT ( 'NONE',  ( 69.33797530432867973, 62.88103157235104845, 13.66491503495263871 ) ) ;
#68106 = EDGE_LOOP ( 'NONE', ( #49225, #9632, #67350, #28384 ) ) ;
#68107 = CARTESIAN_POINT ( 'NONE',  ( 92.54224522822943300, 233.4244531367911009, -4.594050593750046652 ) ) ;
#68108 = CARTESIAN_POINT ( 'NONE',  ( 198.6807893054935619, 282.8457944317249826, 17.49506086463898313 ) ) ;
#68109 = CARTESIAN_POINT ( 'NONE',  ( 178.1262429318011016, 269.1995414919144309, -16.42947538547102226 ) ) ;
#68110 = CARTESIAN_POINT ( 'NONE',  ( 81.74299993193413627, 42.33909358938161205, -7.997327082880324234 ) ) ;
#68111 = ORIENTED_EDGE ( 'NONE', *, *, #34398, .T. ) ;
#68112 = ORIENTED_EDGE ( 'NONE', *, *, #38188, .T. ) ;
#68113 = ORIENTED_EDGE ( 'NONE', *, *, #24339, .F. ) ;
#68114 = CARTESIAN_POINT ( 'NONE',  ( 81.30167161776530804, 49.59675704108522609, 14.04897986542503041 ) ) ;
#68115 = ORIENTED_EDGE ( 'NONE', *, *, #68646, .T. ) ;
#68116 = CARTESIAN_POINT ( 'NONE',  ( 68.59458835999485871, 68.94540003394581618, 5.879567767820735646 ) ) ;
#68117 = DIRECTION ( 'NONE',  ( -0.000000000000000000, -0.000000000000000000, 1.000000000000000000 ) ) ;
#68118 = ORIENTED_EDGE ( 'NONE', *, *, #26811, .T. ) ;
#68119 = CARTESIAN_POINT ( 'NONE',  ( 208.1757572214753793, 270.0760069187178374, 2.172546422564154867 ) ) ;
#68120 = CARTESIAN_POINT ( 'NONE',  ( -77.42978507651396569, 55.80833764325424085, 10.00000000000000000 ) ) ;
#68121 = CARTESIAN_POINT ( 'NONE',  ( -23.56652710931154360, 99.64324603395651536, 45.19937630303415688 ) ) ;
#68122 = CARTESIAN_POINT ( 'NONE',  ( 68.41665967678483184, 68.37445157850072519, -6.807967649046275049 ) ) ;
#68123 = CARTESIAN_POINT ( 'NONE',  ( 165.0818462652269432, 264.4362006198225572, -17.63156621922489720 ) ) ;
#68124 = EDGE_LOOP ( 'NONE', ( #84121, #49935, #12444, #30374 ) ) ;
#68125 = CARTESIAN_POINT ( 'NONE',  ( 77.22649460905378760, 63.31555197798695644, 15.15381191669832184 ) ) ;
#68126 = CARTESIAN_POINT ( 'NONE',  ( 13.54711677929152636, 28.79752408145592213, -5.678558825948271327 ) ) ;
#68127 = VERTEX_POINT ( 'NONE', #80034 ) ;
#68128 = CARTESIAN_POINT ( 'NONE',  ( 167.6010540021560189, 247.4270797612363708, 3.638657435017179864 ) ) ;
#68129 = CARTESIAN_POINT ( 'NONE',  ( 188.7930588916510999, 290.9633865388665299, 14.97457979531618832 ) ) ;
#68131 = EDGE_LOOP ( 'NONE', ( #5572, #70773, #93546 ) ) ;
#68130 = CARTESIAN_POINT ( 'NONE',  ( 200.1482866522123629, 269.8493581831766619, 10.43834433840694587 ) ) ;
#68132 = CARTESIAN_POINT ( 'NONE',  ( 203.0398866899141126, 278.9715956204779559, 16.57839218037009132 ) ) ;
#68133 = CARTESIAN_POINT ( 'NONE',  ( 187.9395208661097740, 260.6475812410266713, 2.852896766392861494 ) ) ;
#68134 = CARTESIAN_POINT ( 'NONE',  ( 161.0824001485583494, 281.2882558135126487, -6.595532366314904138 ) ) ;
#68135 = FACE_OUTER_BOUND ( 'NONE', #96942, .T. ) ;
#68136 = CARTESIAN_POINT ( 'NONE',  ( 192.7720849525608742, 292.1153051028871346, -15.41102863861109107 ) ) ;
#68137 = CARTESIAN_POINT ( 'NONE',  ( 170.2269576865593308, 254.8920245254076633, 11.28111190939480046 ) ) ;
#68138 = CARTESIAN_POINT ( 'NONE',  ( 194.7198309261459030, 262.9852205752617351, -0.8009190715571888886 ) ) ;
#68139 = EDGE_LOOP ( 'NONE', ( #26782, #3110, #61114, #71248, #97802, #27257, #34691, #70730, #56503, #90875, #4184 ) ) ;
#68140 = CARTESIAN_POINT ( 'NONE',  ( 181.4944501622172197, 271.2267610228687431, -15.97090179654585640 ) ) ;
#68141 = CARTESIAN_POINT ( 'NONE',  ( 70.41420743703629626, 63.52079831010913580, -13.09409908041479831 ) ) ;
#68142 = CARTESIAN_POINT ( 'NONE',  ( 156.0507216674837707, 279.5060275253360373, 7.618106348741741307 ) ) ;
#68143 = EDGE_CURVE ( 'NONE', #1972, #50533, #50093, .T. ) ;
#68144 = CARTESIAN_POINT ( 'NONE',  ( 13.28313890609096504, 165.1427522451417929, 1.119607411625061291E-15 ) ) ;
#68145 = CARTESIAN_POINT ( 'NONE',  ( 82.87333762504050583, 53.62476702604639200, -15.35949376849550596 ) ) ;
#68146 = CARTESIAN_POINT ( 'NONE',  ( 42.87900647455834502, 24.75620593066997444, 8.404119662683931360E-14 ) ) ;
#68147 = CARTESIAN_POINT ( 'NONE',  ( 163.4971673378707067, 247.4615946076538648, -7.522761844253225583 ) ) ;
#68148 = DIRECTION ( 'NONE',  ( -0.8769651246872975925, 0.4805540241036304061, 0.000000000000000000 ) ) ;
#68149 = CARTESIAN_POINT ( 'NONE',  ( 164.7521540125055992, 274.2224693477860455, 15.96929761590263475 ) ) ;
#68151 = CARTESIAN_POINT ( 'NONE',  ( 76.11661262897267477, 65.38883171293761620, 14.43021505105785174 ) ) ;
#68150 = CARTESIAN_POINT ( 'NONE',  ( -8.674473839076844328, 174.9869531367911293, 4.594050593750046652 ) ) ;
#68152 = CARTESIAN_POINT ( 'NONE',  ( 189.1219514243199455, 296.9589831032453162, 8.554710403106881245 ) ) ;
#68153 = VERTEX_POINT ( 'NONE', #3027 ) ;
#68154 = ORIENTED_EDGE ( 'NONE', *, *, #79614, .T. ) ;
#68155 = FACE_BOUND ( 'NONE', #73599, .T. ) ;
#68156 = PLANE ( 'NONE',  #86917 ) ;
#68157 = CARTESIAN_POINT ( 'NONE',  ( 174.3227904276429001, 290.2577864514880162, 2.565156313979267910 ) ) ;
#68158 = DIRECTION ( 'NONE',  ( -0.8660254037844387076, -0.4999999999999998890, -0.000000000000000000 ) ) ;
#68159 = VECTOR ( 'NONE', #38456, 1000.000000000000114 ) ;
#68160 = CARTESIAN_POINT ( 'NONE',  ( 202.3483817376306035, 280.1693173315183003, -17.41571691969629043 ) ) ;
#68161 = CARTESIAN_POINT ( 'NONE',  ( 84.95073541789081162, 48.44820618829425740, 12.09123390135387766 ) ) ;
#68162 = CARTESIAN_POINT ( 'NONE',  ( -21.75249381947928740, 146.7012482093458914, 37.49999999999996447 ) ) ;
#68163 = CARTESIAN_POINT ( 'NONE',  ( 24.28913873611587348, 175.6423013555409796, -4.594050593750043987 ) ) ;
#68164 = CARTESIAN_POINT ( 'NONE',  ( 123.0428377395863890, 241.8458772461660544, 9.188101187500095079 ) ) ;
#68165 = DIRECTION ( 'NONE',  ( -0.000000000000000000, -0.000000000000000000, -1.000000000000000000 ) ) ;
#68166 = CARTESIAN_POINT ( 'NONE',  ( 80.74974841587442143, 43.27611110060701805, 10.01619596027649806 ) ) ;
#68167 = CARTESIAN_POINT ( 'NONE',  ( 206.6995622243289858, 271.9034532870905991, -6.768494619944537050 ) ) ;
#68168 = DIRECTION ( 'NONE',  ( -0.8660254037844378194, -0.5000000000000014433, -0.000000000000000000 ) ) ;
#68169 = CARTESIAN_POINT ( 'NONE',  ( 79.06689284147950048, 53.93734539651928372, -15.86389558664243538 ) ) ;
#68170 = PRODUCT_RELATED_PRODUCT_CATEGORY ( 'part', '', ( #49980 ) ) ;
#68171 = CARTESIAN_POINT ( 'NONE',  ( 193.9401685343300699, 294.7327698005063326, 14.01047396938887069 ) ) ;
#68172 = CARTESIAN_POINT ( 'NONE',  ( 207.8575108622103755, 270.6272257822888037, -6.381720258959569847 ) ) ;
#68173 = CARTESIAN_POINT ( 'NONE',  ( 189.8411839564327863, 284.6317981244556563, 16.72185364084435832 ) ) ;
#68174 = CARTESIAN_POINT ( 'NONE',  ( 70.65333620286477867, 60.57558753426528142, -14.63893798347084818 ) ) ;
#68175 = CARTESIAN_POINT ( 'NONE',  ( 165.0248146787475321, 249.8254979808875760, -10.64519944682263031 ) ) ;
#68176 = CARTESIAN_POINT ( 'NONE',  ( 192.6536174980028875, 265.2563178382590650, 7.796075781698757368 ) ) ;
#68177 = CARTESIAN_POINT ( 'NONE',  ( 197.0106579294310620, 265.8628023436195917, -7.468568667325064858 ) ) ;
#68178 = CARTESIAN_POINT ( 'NONE',  ( 162.2926170091170945, 251.8178718525326190, -12.93660524614211482 ) ) ;
#68179 = CARTESIAN_POINT ( 'NONE',  ( 81.84472095112539591, 41.18814569898182043, -5.689628007502441243 ) ) ;
#68180 = CARTESIAN_POINT ( 'NONE',  ( 98.17141035282828909, 236.6744531367911293, 4.594050593750047540 ) ) ;
#68181 = CARTESIAN_POINT ( 'NONE',  ( 11.30507296547734697, 15.03085787977761179, 9.188101187500006262 ) ) ;
#68182 = CARTESIAN_POINT ( 'NONE',  ( 150.8167050463783312, 269.4247995599803289, 14.38040671671637938 ) ) ;
#68183 = DIRECTION ( 'NONE',  ( 0.4999999999999998890, -0.8660254037844385966, 0.000000000000000000 ) ) ;
#68185 = CARTESIAN_POINT ( 'NONE',  ( 152.2681919351047952, 266.9107505221858219, 15.47691051422547837 ) ) ;
#68184 = CARTESIAN_POINT ( 'NONE',  ( 66.27049696474395546, 68.63756696002002400, 2.357326866573562718 ) ) ;
#68186 = CARTESIAN_POINT ( 'NONE',  ( 157.5373507488561131, 281.8578703925237505, -3.864990440558811358 ) ) ;
#68187 = DIRECTION ( 'NONE',  ( 0.000000000000000000, 0.000000000000000000, 1.000000000000000000 ) ) ;
#68188 = CARTESIAN_POINT ( 'NONE',  ( 204.1541407990405332, 272.6956988606675623, 11.22829397770025395 ) ) ;
#68189 = ADVANCED_FACE ( 'NONE', ( #57178 ), #57678, .T. ) ;
#68190 = CARTESIAN_POINT ( 'NONE',  ( 35.77750112005064409, 38.84336893147759184, -7.433330006724137462 ) ) ;
#68191 = CARTESIAN_POINT ( 'NONE',  ( 192.9523350703175311, 296.4437475495926719, -13.35611922184540923 ) ) ;
#68192 = CARTESIAN_POINT ( 'NONE',  ( 201.0277610203388008, 266.5939165858319484, 3.083042990266529060 ) ) ;
#68193 = ORIENTED_EDGE ( 'NONE', *, *, #74668, .F. ) ;
#68194 = CARTESIAN_POINT ( 'NONE',  ( 18.69336236660381090, 32.83396525600390703, -2.839279412974133887 ) ) ;
#68195 = CARTESIAN_POINT ( 'NONE',  ( 178.7021693527624677, 264.3200711924779398, 15.74069764637753366 ) ) ;
#68196 = CARTESIAN_POINT ( 'NONE',  ( 192.9523350703175311, 296.4437475495926719, -13.35611922184540923 ) ) ;
#68197 = DIRECTION ( 'NONE',  ( -0.3940053768033626169, 0.6824373310787468228, 0.6156614753256509642 ) ) ;
#68198 = VERTEX_POINT ( 'NONE', #27300 ) ;
#68199 = B_SPLINE_SURFACE_WITH_KNOTS ( 'NONE', 3, 1, ( 
 ( #10675, #87246 ),
 ( #49176, #2080 ),
 ( #93811, #17779 ),
 ( #39537, #93299 ),
 ( #16760, #24371 ),
 ( #48680, #62344 ),
 ( #79613, #85733 ),
 ( #9170, #569 ),
 ( #70460, #78079 ),
 ( #41044, #33471 ),
 ( #8667, #31452 ),
 ( #64365, #56759 ),
 ( #31952, #55243 ),
 ( #47649, #40045 ),
 ( #70985, #32470 ),
 ( #74490, #72991 ),
 ( #3583, #34463 ),
 ( #73974, #43550 ),
 ( #81115, #13179 ),
 ( #11682, #96811 ),
 ( #89712, #27860 ),
 ( #4558, #72497 ),
 ( #18778, #3100 ),
 ( #49656, #65361 ),
 ( #19295, #58737 ),
 ( #81602, #51665 ),
 ( #59227, #42544 ),
 ( #33989, #4059 ),
 ( #50162, #97780 ),
 ( #64875, #20273 ),
 ( #80612, #27369 ),
 ( #51147, #96300 ),
 ( #66360, #58252 ),
 ( #26870, #97293 ) ),
 .UNSPECIFIED., .T., .F., .F.,
 ( 4, 2, 2, 2, 2, 2, 2, 2, 2, 2, 2, 2, 2, 2, 2, 2, 4 ),
 ( 2, 2 ),
 ( 0.000000000000000000, 0.06250000000000000000, 0.1250000000000000000, 0.1875000000000000000, 0.2500000000000000000, 0.3125000000000000000, 0.3750000000000000000, 0.4375000000000000000, 0.5000000000000000000, 0.5625000000000000000, 0.6250000000000000000, 0.6875000000000000000, 0.7500000000000000000, 0.8125000000000000000, 0.8750000000000000000, 0.9375000000000000000, 1.000000000000000000 ),
 ( 0.000000000000000000, 1.000000000000000000 ),
 .UNSPECIFIED. ) ;
#68200 = B_SPLINE_CURVE_WITH_KNOTS ( 'NONE', 3,
 ( #90660, #23677, #68174, #76303, #75307, #90542, #22579, #84416, #99101, #14964 ),
 .UNSPECIFIED., .F., .F.,
 ( 4, 2, 2, 2, 4 ),
 ( 0.000000000000000000, 0.2500000000000000000, 0.5000000000000000000, 0.7500000000000000000, 1.000000000000000000 ),
 .UNSPECIFIED. ) ;
#68201 = CARTESIAN_POINT ( 'NONE',  ( 70.51409906297000418, 60.89179027048928106, 14.47183175352521722 ) ) ;
#68202 = CARTESIAN_POINT ( 'NONE',  ( 75.98877566108227199, 65.64741556006092082, -14.26224329751477349 ) ) ;
#68203 = ADVANCED_FACE ( 'NONE', ( #88657 ), #45791, .T. ) ;
#68204 = CARTESIAN_POINT ( 'NONE',  ( 169.7329090781420291, 252.3771132214117188, -8.760384215664782204 ) ) ;
#68205 = CARTESIAN_POINT ( 'NONE',  ( 75.06758043940683933, 52.95706437108803755, -16.00702414185586164 ) ) ;
#68206 = CARTESIAN_POINT ( 'NONE',  ( 142.9884853222707477, 243.3615022471901739, 5.000000000000051514 ) ) ;
#68207 = ORIENTED_EDGE ( 'NONE', *, *, #46516, .T. ) ;
#68208 = CARTESIAN_POINT ( 'NONE',  ( 73.02433024948126672, 69.66517378990661769, 9.714162469163332148 ) ) ;
#68209 = VERTEX_POINT ( 'NONE', #66784 ) ;
#68210 = CARTESIAN_POINT ( 'NONE',  ( 81.37996698483264879, 42.05785630660916752, -7.883612591813013104 ) ) ;
#68211 = EDGE_CURVE ( 'NONE', #93198, #28495, #6977, .T. ) ;
#68212 = CARTESIAN_POINT ( 'NONE',  ( 185.0613556293041597, 292.4148342362145740, -10.69734790306066152 ) ) ;
#68213 = ORIENTED_EDGE ( 'NONE', *, *, #70795, .F. ) ;
#68214 = CARTESIAN_POINT ( 'NONE',  ( 71.90400658755810070, 72.53437165389429708, 1.750395423964772990 ) ) ;
#68215 = CARTESIAN_POINT ( 'NONE',  ( 159.0816921219542905, 255.7002322326580952, 16.02278834591242784 ) ) ;
#68216 = CARTESIAN_POINT ( 'NONE',  ( 85.01541621076924571, 50.02003410940323391, 13.59443226853714926 ) ) ;
#68217 = CARTESIAN_POINT ( 'NONE',  ( 153.6331558325334754, 264.5465637013422224, -16.53762606136138658 ) ) ;
#68218 = CARTESIAN_POINT ( 'NONE',  ( 200.9061540366740246, 282.6673289856585143, -18.13083321883407351 ) ) ;
#68219 = CARTESIAN_POINT ( 'NONE',  ( 70.81316579126401223, 61.41551742065354347, -14.85192641751565823 ) ) ;
#68220 = CARTESIAN_POINT ( 'NONE',  ( 36.41018743920069056, 41.99752408145594984, 5.678558825948276656 ) ) ;
#68221 = CARTESIAN_POINT ( 'NONE',  ( 81.56781671333388317, 55.98423300004855463, -16.39433532902864954 ) ) ;
#68222 = DIRECTION ( 'NONE',  ( -0.4999999999999987788, 0.8660254037844392627, 0.000000000000000000 ) ) ;
#68223 =( BOUNDED_CURVE ( )  B_SPLINE_CURVE ( 2, ( #23695, #38902, #16116, #69806, #416, #54590, #47014, #33837, #11534 ),
 .UNSPECIFIED., .F., .T. ) 
 B_SPLINE_CURVE_WITH_KNOTS ( ( 3, 2, 2, 2, 3 ),
 ( 0.8991935483870967527, 0.9005376344086021279, 0.9032258064516128782, 0.9059139784946236285, 0.9072580645161290036 ),
 .UNSPECIFIED. ) 
 CURVE ( )  GEOMETRIC_REPRESENTATION_ITEM ( )  RATIONAL_B_SPLINE_CURVE ( ( 0.9330127018922194093, 0.9330127018922194093, 1.000000000000000000, 0.8660254037844387076, 1.000000000000000000, 0.8660254037844387076, 1.000000000000000000, 0.9330127018922194093, 0.9330127018922194093 ) ) 
 REPRESENTATION_ITEM ( '' )  );
#68224 = FACE_OUTER_BOUND ( 'NONE', #78346, .T. ) ;
#68225 = ORIENTED_EDGE ( 'NONE', *, *, #14955, .F. ) ;
#68226 = VECTOR ( 'NONE', #21988, 1000.000000000000227 ) ;
#68227 = ORIENTED_EDGE ( 'NONE', *, *, #23716, .F. ) ;
#68228 = CARTESIAN_POINT ( 'NONE',  ( 72.10191719723457027, 72.28141447668717490, -1.471618146119747284 ) ) ;
#68229 = CARTESIAN_POINT ( 'NONE',  ( 176.5791842843404140, 272.9161298461250453, 17.82309232038752000 ) ) ;
#68230 = CARTESIAN_POINT ( 'NONE',  ( 79.66714386024425210, 56.18315950032808104, 16.16506256184515777 ) ) ;
#68232 = CARTESIAN_POINT ( 'NONE',  ( 165.8263255788853030, 274.0082066433705563, -15.18430102088745137 ) ) ;
#68231 = LINE ( 'NONE', #59116, #71436 ) ;
#68233 = B_SPLINE_CURVE_WITH_KNOTS ( 'NONE', 3,
 ( #66910, #28928, #99327, #44093 ),
 .UNSPECIFIED., .F., .F.,
 ( 4, 4 ),
 ( 0.01280637797058834827, 0.01912828568769148890 ),
 .UNSPECIFIED. ) ;
#68234 = FACE_OUTER_BOUND ( 'NONE', #7536, .T. ) ;
#68235 = CARTESIAN_POINT ( 'NONE',  ( 69.88766240224211401, 70.52056060877789889, 5.189453427646838257 ) ) ;
#68236 = CARTESIAN_POINT ( 'NONE',  ( 73.22046044295466061, 61.35883500877204710, -14.94439587469189945 ) ) ;
#68237 = CARTESIAN_POINT ( 'NONE',  ( -19.65312891409030271, 93.06504152958497400, -10.00000000000000888 ) ) ;
#68238 = CARTESIAN_POINT ( 'NONE',  ( 168.2820353728258738, 287.7095463320123940, -5.019694092131335772 ) ) ;
#68239 = CARTESIAN_POINT ( 'NONE',  ( 77.29607140482774241, 63.09965268300504704, -15.25444628986662998 ) ) ;
#68240 = CARTESIAN_POINT ( 'NONE',  ( 184.6191043844399644, 285.4259123777357559, -15.07684468139096445 ) ) ;
#68241 = CARTESIAN_POINT ( 'NONE',  ( 107.4543804714665072, 232.8458772461660544, 9.188101187500095079 ) ) ;
#68242 = ORIENTED_EDGE ( 'NONE', *, *, #13551, .T. ) ;
#68243 = LINE ( 'NONE', #22155, #96578 ) ;
#68244 = CARTESIAN_POINT ( 'NONE',  ( 37.97985170016632850, 33.87878583063844928, -9.188101187500006262 ) ) ;
#68245 = CARTESIAN_POINT ( 'NONE',  ( 191.3077102587145646, 274.7514833773715850, 16.90660339326615969 ) ) ;
#68246 = ORIENTED_EDGE ( 'NONE', *, *, #91995, .F. ) ;
#68247 = EDGE_CURVE ( 'NONE', #29382, #86525, #46035, .T. ) ;
#68248 = CARTESIAN_POINT ( 'NONE',  ( 162.8822533913248094, 248.9136777285836217, -9.954654975717463827 ) ) ;
#68249 = EDGE_CURVE ( 'NONE', #50641, #93452, #59306, .T. ) ;
#68250 = DIRECTION ( 'NONE',  ( -0.000000000000000000, -0.000000000000000000, 1.000000000000000000 ) ) ;
#68251 = CARTESIAN_POINT ( 'NONE',  ( 147.3103884059524376, 275.4979181286220182, 2.739230376052490090 ) ) ;
#68252 = CARTESIAN_POINT ( 'NONE',  ( 69.59618255175185197, 71.01531595566491717, 2.954799671095214020 ) ) ;
#68253 = DIRECTION ( 'NONE',  ( 0.2500151307524129951, -0.9682419296822740717, 0.000000000000000000 ) ) ;
#68254 = ORIENTED_EDGE ( 'NONE', *, *, #21058, .T. ) ;
#68255 = FACE_OUTER_BOUND ( 'NONE', #4835, .T. ) ;
#68256 = VERTEX_POINT ( 'NONE', #70777 ) ;
#68257 = DIRECTION ( 'NONE',  ( -0.3986482622784180974, -0.9171038997749370036, 0.000000000000000000 ) ) ;
#68258 = ORIENTED_EDGE ( 'NONE', *, *, #56357, .T. ) ;
#68259 = CARTESIAN_POINT ( 'NONE',  ( 165.0538309624641613, 244.7653741195639157, 2.311334310144196547 ) ) ;
#68260 = EDGE_CURVE ( 'NONE', #72102, #58450, #8567, .T. ) ;
#68261 = B_SPLINE_CURVE_WITH_KNOTS ( 'NONE', 3,
 ( #10875, #64573, #11394, #51347, #42247, #4774, #35657, #34171, #12883, #73183, #96013, #95529, #3775, #72184, #26074, #49365, #88429, #76648, #45239, #22443, #30547, #28545, #44728, #21454, #43741, #75174, #82802, #36142, #60425, #14351, #45725, #29551, #59427, #84782, #91382, #51863, #90405, #21943 ),
 .UNSPECIFIED., .F., .F.,
 ( 4, 2, 2, 2, 2, 2, 2, 2, 2, 2, 2, 2, 2, 2, 2, 2, 2, 2, 4 ),
 ( 0.003224435166570254439, 0.003418643166137364138, 0.003612851165704473403, 0.003709955165488081161, 0.003807059165271688920, 0.004001267164838904003, 0.004389683163973335037, 0.004778099163107765203, 0.005554931161376563953, 0.006331763159645363570, 0.007885427156183113725, 0.007982531155966712810, 0.008079635155750313630, 0.008128187155642150469, 0.008176739155533987308, 0.008273843155317693945, 0.008662259154452636722, 0.009050675153587579500, 0.009439091152722522277 ),
 .UNSPECIFIED. ) ;
#68263 = EDGE_CURVE ( 'NONE', #27838, #76194, #76228, .T. ) ;
#68262 = B_SPLINE_CURVE_WITH_KNOTS ( 'NONE', 3,
 ( #92087, #7421, #22635, #71629 ),
 .UNSPECIFIED., .F., .F.,
 ( 4, 4 ),
 ( 0.0007376998311747307935, 0.008666068401041223529 ),
 .UNSPECIFIED. ) ;
#68264 = CARTESIAN_POINT ( 'NONE',  ( 196.3956310503436953, 264.1850728776087180, 4.154333235580330630 ) ) ;
#68265 = CARTESIAN_POINT ( 'NONE',  ( -107.5954152546898257, 65.38554960527383741, 36.50000000000000000 ) ) ;
#68266 = CARTESIAN_POINT ( 'NONE',  ( 83.63236669786769539, 48.19556681045689572, 12.42628442967038538 ) ) ;
#68268 = CARTESIAN_POINT ( 'NONE',  ( 157.4827499296481506, 280.1768083929792965, 5.769207439127447046 ) ) ;
#68267 = DIRECTION ( 'NONE',  ( 0.6793907169778464761, 0.000000000000000000, -0.7337767056021385903 ) ) ;
#68269 = CARTESIAN_POINT ( 'NONE',  ( 155.9200296242932495, 280.3860598674420430, -5.539708607631867565 ) ) ;
#68270 = ORIENTED_EDGE ( 'NONE', *, *, #86864, .F. ) ;
#68271 = FACE_OUTER_BOUND ( 'NONE', #13483, .T. ) ;
#68272 = CARTESIAN_POINT ( 'NONE',  ( 5.968649350820469657, 188.6868197944958752, 37.50000000000000000 ) ) ;
#68273 = CARTESIAN_POINT ( 'NONE',  ( 82.35088575792271115, 40.80351433566520569, -3.705252894541431363 ) ) ;
#68274 = EDGE_CURVE ( 'NONE', #49112, #50075, #34766, .T. ) ;
#68275 = CARTESIAN_POINT ( 'NONE',  ( 173.1431250042722922, 251.5821726865244443, -0.2645228944078902855 ) ) ;
#68276 = CARTESIAN_POINT ( 'NONE',  ( 192.8054871723947201, 271.6419448112512214, -14.92314579000926145 ) ) ;
#68277 = DIRECTION ( 'NONE',  ( -0.8660254037844379305, -0.5000000000000014433, -0.000000000000000000 ) ) ;
#68278 = LINE ( 'NONE', #37373, #71160 ) ;
#68279 = CARTESIAN_POINT ( 'NONE',  ( 200.3293654959697392, 273.7156512906800572, 13.98704503334941229 ) ) ;
#68280 = CARTESIAN_POINT ( 'NONE',  ( 194.3562588153086779, 294.0120802933159325, 14.11474987148825200 ) ) ;
#68281 = CARTESIAN_POINT ( 'NONE',  ( 190.1774295428112396, 299.2500249094251217, 7.542682482482700124 ) ) ;
#68283 = VECTOR ( 'NONE', #82331, 1000.000000000000000 ) ;
#68282 = CARTESIAN_POINT ( 'NONE',  ( 82.74895235971042950, 53.70034252712168410, -15.76590362002541035 ) ) ;
#68284 = CARTESIAN_POINT ( 'NONE',  ( 76.62902843369037953, 224.2369531367911293, -4.594050593750048428 ) ) ;
#68285 = CARTESIAN_POINT ( 'NONE',  ( 159.6288139302610887, 254.1617792512662675, -15.32287760493869477 ) ) ;
#68286 = CARTESIAN_POINT ( 'NONE',  ( 197.4237242065244402, 287.4445287091903083, 17.29625570825889369 ) ) ;
#68287 = CARTESIAN_POINT ( 'NONE',  ( 47.96820964746023463, 80.67316705762479501, 10.00000000000000000 ) ) ;
#68288 = CARTESIAN_POINT ( 'NONE',  ( 197.3452912936916732, 287.9947459898783109, -17.00996526260133734 ) ) ;
#68289 = CARTESIAN_POINT ( 'NONE',  ( 207.2167723318516153, 271.7370174712370954, -6.606038862010207957 ) ) ;
#68290 = CARTESIAN_POINT ( 'NONE',  ( -60.12289532704065920, 50.57929518357629206, 59.99999999999999289 ) ) ;
#68292 = DIRECTION ( 'NONE',  ( -1.000000000000000000, 0.000000000000000000, 0.000000000000000000 ) ) ;
#68291 = CARTESIAN_POINT ( 'NONE',  ( 101.6177300921036419, 236.1427522451419065, -10.00000000000009592 ) ) ;
#68293 = CARTESIAN_POINT ( 'NONE',  ( 186.9240681684178469, 258.1497295257914857, -0.2642925951357694148 ) ) ;
#68294 = CARTESIAN_POINT ( 'NONE',  ( 37.76795716069910469, 37.50829794293884589, -10.00000000000000355 ) ) ;
#68295 = DIRECTION ( 'NONE',  ( 0.000000000000000000, 0.000000000000000000, 1.000000000000000000 ) ) ;
#68296 = CARTESIAN_POINT ( 'NONE',  ( 82.14587413470448496, 54.18172936202615375, 15.63325719219342957 ) ) ;
#68297 = CARTESIAN_POINT ( 'NONE',  ( 71.86118671916545964, 71.93196444170322934, 2.859464606235072370 ) ) ;
#68298 = CARTESIAN_POINT ( 'NONE',  ( 34.24843087963692767, 181.3923013555409796, 4.594050593750050204 ) ) ;
#68299 = CARTESIAN_POINT ( 'NONE',  ( 52.08270766911643079, 207.0024278399160664, -9.188101187500093303 ) ) ;
#68300 = CARTESIAN_POINT ( 'NONE',  ( 157.3025066944120454, 258.1910615777721887, 18.21299529665260053 ) ) ;
#68301 = CARTESIAN_POINT ( 'NONE',  ( 74.91863663735624357, 66.38413888100485849, -13.07019282884167843 ) ) ;
#68302 = CARTESIAN_POINT ( 'NONE',  ( 81.23729515884194541, 50.24360654307113094, -14.35787940686896569 ) ) ;
#68303 = CARTESIAN_POINT ( 'NONE',  ( 71.77728350350676578, 72.07728907414252717, -1.665459805617878652 ) ) ;
#68304 = CARTESIAN_POINT ( 'NONE',  ( 45.10055139898691579, 196.8458772461660544, 9.188101187500095079 ) ) ;
#68305 = EDGE_CURVE ( 'NONE', #42521, #10970, #2888, .T. ) ;
#68306 = CARTESIAN_POINT ( 'NONE',  ( 23.04210978301306767, 28.70171378149919406, -9.188101187500004485 ) ) ;
#68307 = CARTESIAN_POINT ( 'NONE',  ( -3.078821053925192786, 157.4824982072974251, -4.415768667553308270E-15 ) ) ;
#68308 = CARTESIAN_POINT ( 'NONE',  ( 149.6191398986701415, 271.4990432411842676, -11.66821883946526839 ) ) ;
#68309 = CARTESIAN_POINT ( 'NONE',  ( 3.479571460297436136, 22.98502408145589726, -5.678558825948271327 ) ) ;
#68310 = CARTESIAN_POINT ( 'NONE',  ( 40.08283240419611815, 56.57374221892477806, -10.00000000000000000 ) ) ;
#68311 = CARTESIAN_POINT ( 'NONE',  ( 76.72979488479921883, 63.64413466080264214, 15.32332512078611053 ) ) ;
#68312 = CARTESIAN_POINT ( 'NONE',  ( 194.9471474500919896, 290.9886311562445371, 16.55118206508679890 ) ) ;
#68313 = CARTESIAN_POINT ( 'NONE',  ( 180.1034954954120053, 276.2679041092388275, 16.95561710916604170 ) ) ;
#68314 = CARTESIAN_POINT ( 'NONE',  ( 82.13437494121951943, 40.75881571130759085, -0.7180065468227782022 ) ) ;
#68315 = CARTESIAN_POINT ( 'NONE',  ( -64.94778771796556782, 41.33875607593970614, 10.00000000000000000 ) ) ;
#68316 = EDGE_CURVE ( 'NONE', #63769, #16015, #96698, .T. ) ;
#68317 = CARTESIAN_POINT ( 'NONE',  ( 73.33599517600377737, 57.35580166543588376, -15.91338689994087652 ) ) ;
#68318 = CARTESIAN_POINT ( 'NONE',  ( 92.83118068642190224, 237.7365022471903728, 2.944929066748280225E-16 ) ) ;
#68319 = CARTESIAN_POINT ( 'NONE',  ( 161.5504728662519369, 250.8333683393111926, 12.94300825113363373 ) ) ;
#68320 = CARTESIAN_POINT ( 'NONE',  ( 164.8610104253742463, 270.4993528865625194, -17.13915278852090296 ) ) ;
#68321 = ORIENTED_EDGE ( 'NONE', *, *, #70925, .F. ) ;
#68322 = CARTESIAN_POINT ( 'NONE',  ( 55.22204975783502334, 208.8149278399160664, 9.188101187500093303 ) ) ;
#68323 = ORIENTED_EDGE ( 'NONE', *, *, #53266, .T. ) ;
#68324 = CARTESIAN_POINT ( 'NONE',  ( 166.5534370075956190, 264.7307956230007449, 16.99907680286884215 ) ) ;
#68325 = CARTESIAN_POINT ( 'NONE',  ( 147.4963928429778264, 275.1757489932608109, 4.929816573182678852 ) ) ;
#68326 = EDGE_CURVE ( 'NONE', #70323, #55128, #4373, .T. ) ;
#68327 = CARTESIAN_POINT ( 'NONE',  ( 175.1183745746886871, 267.9007702990796247, 17.47926410801357022 ) ) ;
#68328 = ORIENTED_EDGE ( 'NONE', *, *, #39130, .T. ) ;
#68329 = B_SPLINE_CURVE_WITH_KNOTS ( 'NONE', 3,
 ( #58126, #4948, #52028, #28223, #68210, #20147, #51018, #35827, #82491, #74853 ),
 .UNSPECIFIED., .F., .F.,
 ( 4, 2, 2, 2, 4 ),
 ( 0.000000000000000000, 0.0002622400424272762205, 0.0005244800848545524410, 0.0007867201272818286073, 0.001048960169709104882 ),
 .UNSPECIFIED. ) ;
#68330 = CARTESIAN_POINT ( 'NONE',  ( -19.65312891409030271, 93.06504152958497400, -10.00000000000000888 ) ) ;
#68331 = CARTESIAN_POINT ( 'NONE',  ( 79.15343291076531784, 46.26937536990111255, -12.76842876231724055 ) ) ;
#68332 = CARTESIAN_POINT ( 'NONE',  ( 147.6884207308302450, 274.8431469350302336, -8.096293592099874203 ) ) ;
#68333 = CARTESIAN_POINT ( 'NONE',  ( 73.10407572603702420, 70.56422230472695389, -7.912081317950750758 ) ) ;
#68334 = DIRECTION ( 'NONE',  ( 0.4999999999999998890, -0.8660254037844385966, 0.000000000000000000 ) ) ;
#68335 = CARTESIAN_POINT ( 'NONE',  ( 157.1184542243154567, 258.5098498072379698, 16.84490127433854667 ) ) ;
#68337 = EDGE_LOOP ( 'NONE', ( #44187, #14788, #19514, #28521 ) ) ;
#68336 = CIRCLE ( 'NONE', #91023, 5.000000000000116351 ) ;
#68338 = CARTESIAN_POINT ( 'NONE',  ( 21.67811977205258245, 27.91421378149919263, 9.188101187500008038 ) ) ;
#68339 = CARTESIAN_POINT ( 'NONE',  ( 68.18103004421558921, 69.66170404906247882, -2.995069279367296389 ) ) ;
#68340 = CARTESIAN_POINT ( 'NONE',  ( 74.90372969979991069, 67.45002815973559507, -12.77473495645215174 ) ) ;
#68341 = EDGE_CURVE ( 'NONE', #48849, #20062, #36262, .T. ) ;
#68342 = EDGE_LOOP ( 'NONE', ( #33913, #82102, #32326, #29018, #76486, #93318, #48673, #57615, #95959, #1783, #25754 ) ) ;
#68343 = CARTESIAN_POINT ( 'NONE',  ( 205.2564848266901834, 271.9733254596621350, -9.597888780111448526 ) ) ;
#68344 = EDGE_CURVE ( 'NONE', #82418, #59756, #21095, .T. ) ;
#68345 = CARTESIAN_POINT ( 'NONE',  ( 160.0061168334508750, 253.5082714530983026, -16.02306982074888708 ) ) ;
#68346 = EDGE_LOOP ( 'NONE', ( #97582, #46047, #13255, #69724 ) ) ;
#68347 = ORIENTED_EDGE ( 'NONE', *, *, #7725, .F. ) ;
#68348 = CARTESIAN_POINT ( 'NONE',  ( 82.60366837242126792, 49.14327676238544740, -13.42131973624779917 ) ) ;
#68350 = CARTESIAN_POINT ( 'NONE',  ( 42.55442611339157821, 60.96799964870728417, -10.00000000000000000 ) ) ;
#68349 = DIRECTION ( 'NONE',  ( -0.9991767892008870389, -0.04056776950001317328, 0.000000000000000000 ) ) ;
#68351 = CARTESIAN_POINT ( 'NONE',  ( 163.4055107321044318, 247.6203485056908846, -10.24153090796238530 ) ) ;
#68352 = CARTESIAN_POINT ( 'NONE',  ( 164.3961040135806968, 245.9045906125373904, 7.095190383188031191 ) ) ;
#68353 = CARTESIAN_POINT ( 'NONE',  ( 81.19656099875513178, 43.43094936621162105, -9.896970666190503252 ) ) ;
#68354 = CARTESIAN_POINT ( 'NONE',  ( 162.3559333012107118, 263.7644763565641597, -16.88032918853872744 ) ) ;
#68355 = CARTESIAN_POINT ( 'NONE',  ( 136.6287848093373043, 243.5643266524160140, 9.188101187500095079 ) ) ;
#68356 = FACE_OUTER_BOUND ( 'NONE', #28462, .T. ) ;
#68357 = AXIS2_PLACEMENT_3D ( 'NONE', #57423, #66035, #82283 ) ;
#68358 = CARTESIAN_POINT ( 'NONE',  ( 179.3127290521982218, 257.7669455533229552, 10.17447558847459632 ) ) ;
#68359 = CARTESIAN_POINT ( 'NONE',  ( 74.97842782955004282, 214.0958772461660544, -9.188101187500095079 ) ) ;
#68360 = ORIENTED_EDGE ( 'NONE', *, *, #20933, .T. ) ;
#68361 = CYLINDRICAL_SURFACE ( 'NONE', #64052, 16.60714546451156792 ) ;
#68362 = CARTESIAN_POINT ( 'NONE',  ( 71.45645241242529266, 60.59795021819308403, -15.33783228552337441 ) ) ;
#68363 = DIRECTION ( 'NONE',  ( -0.8660254037844387076, -0.4999999999999998890, -0.000000000000000000 ) ) ;
#68364 = ORIENTED_EDGE ( 'NONE', *, *, #20019, .T. ) ;
#68365 = CARTESIAN_POINT ( 'NONE',  ( -38.42080210277662644, 44.85759688798118816, 59.99999999999999289 ) ) ;
#68366 = ORIENTED_EDGE ( 'NONE', *, *, #51003, .F. ) ;
#68367 = ORIENTED_EDGE ( 'NONE', *, *, #69849, .F. ) ;
#68368 = ADVANCED_FACE ( 'NONE', ( #68155, #36756, #5376 ), #5871, .T. ) ;
#68369 = CARTESIAN_POINT ( 'NONE',  ( 157.6304115535352537, 270.8650229002738001, -16.00510772102553858 ) ) ;
#68370 = CARTESIAN_POINT ( 'NONE',  ( 67.13485331027831648, 67.70160943399379505, 6.609904295312462708 ) ) ;
#68371 = FACE_OUTER_BOUND ( 'NONE', #87453, .T. ) ;
#68372 = FACE_OUTER_BOUND ( 'NONE', #38755, .T. ) ;
#68373 = CARTESIAN_POINT ( 'NONE',  ( 171.3751619920873281, 280.2398791927632828, 15.33202389549764888 ) ) ;
#68374 = CARTESIAN_POINT ( 'NONE',  ( 193.8365934467825298, 294.9121671145370556, 14.14845633038902584 ) ) ;
#68375 = CARTESIAN_POINT ( 'NONE',  ( 70.76444730179969156, 64.91245173198861096, 12.28581614439569591 ) ) ;
#68376 = B_SPLINE_CURVE_WITH_KNOTS ( 'NONE', 3,
 ( #12069, #89611, #74389, #81019 ),
 .UNSPECIFIED., .F., .F.,
 ( 4, 4 ),
 ( 0.03433908428602378687, 0.04316694911830618042 ),
 .UNSPECIFIED. ) ;
#68377 = ORIENTED_EDGE ( 'NONE', *, *, #41367, .T. ) ;
#68378 = EDGE_CURVE ( 'NONE', #47742, #17718, #74798, .T. ) ;
#68379 = CARTESIAN_POINT ( 'NONE',  ( 201.1115987356403991, 282.3114883289032377, -17.53098215541816529 ) ) ;
#68380 = ORIENTED_EDGE ( 'NONE', *, *, #37140, .F. ) ;
#68381 = CARTESIAN_POINT ( 'NONE',  ( 163.7663664781766215, 260.9532688520450279, -16.55063263794407646 ) ) ;
#68382 = EDGE_CURVE ( 'NONE', #58260, #79765, #51467, .T. ) ;
#68383 = CARTESIAN_POINT ( 'NONE',  ( 76.08688909832571312, 65.40073596803624412, -14.00630179347337290 ) ) ;
#68384 = CARTESIAN_POINT ( 'NONE',  ( 165.0297293518065658, 244.8071193337670195, 2.517333243890161665 ) ) ;
#68385 = EDGE_CURVE ( 'NONE', #29620, #37787, #35771, .T. ) ;
#68386 = CARTESIAN_POINT ( 'NONE',  ( 194.9394717063963753, 279.5944888486219497, 16.67925351014588031 ) ) ;
#68387 = CARTESIAN_POINT ( 'NONE',  ( 117.8941025407614802, 227.3262482093457777, 3.021315404115420679E-15 ) ) ;
#68388 = CARTESIAN_POINT ( 'NONE',  ( 145.2890388471816721, 248.5643266524159856, -9.188101187500093303 ) ) ;
#68389 = ORIENTED_EDGE ( 'NONE', *, *, #91671, .T. ) ;
#68390 = CARTESIAN_POINT ( 'NONE',  ( 88.25642124133898392, 44.32248799199468436, 4.097629997315075379 ) ) ;
#68391 = ADVANCED_FACE ( 'NONE', ( #30155 ), #13972, .F. ) ;
#68392 = CARTESIAN_POINT ( 'NONE',  ( 68.79582220353250932, 67.86037842356454064, -8.901523894718444296 ) ) ;
#68393 = FACE_OUTER_BOUND ( 'NONE', #26771, .T. ) ;
#68394 = CARTESIAN_POINT ( 'NONE',  ( 73.05626849676114887, 70.73388556528652771, 7.585159314558868715 ) ) ;
#68395 = CARTESIAN_POINT ( 'NONE',  ( 67.87977117728330256, 67.41497322856321261, -7.879648046888831026 ) ) ;
#68396 = VERTEX_POINT ( 'NONE', #6856 ) ;
#68397 = CARTESIAN_POINT ( 'NONE',  ( 196.7437068507956042, 265.9214190645141116, 4.435905237238339183 ) ) ;
#68398 = CARTESIAN_POINT ( 'NONE',  ( 148.3688939817520236, 276.4429351530926624, -3.884194220488612626 ) ) ;
#68399 = CARTESIAN_POINT ( 'NONE',  ( 80.99695547787925420, 51.41970790135942337, 14.90329327012050697 ) ) ;
#68400 = DIRECTION ( 'NONE',  ( -0.9576970189910627429, -0.2877784213863714968, 0.000000000000000000 ) ) ;
#68401 = CARTESIAN_POINT ( 'NONE',  ( 198.5251006538473746, 266.1771426250413128, 0.5392996383993550191 ) ) ;
#68402 = ORIENTED_EDGE ( 'NONE', *, *, #54719, .F. ) ;
#68403 = DIRECTION ( 'NONE',  ( -0.000000000000000000, -0.000000000000000000, -1.000000000000000000 ) ) ;
#68404 = CARTESIAN_POINT ( 'NONE',  ( 186.7936673567182311, 282.2315393728885624, 16.42543875383614349 ) ) ;
#68405 = AXIS2_PLACEMENT_3D ( 'NONE', #38866, #97344, #82166 ) ;
#68406 = CARTESIAN_POINT ( 'NONE',  ( 164.3706594650489023, 245.9486618633701482, -1.665857659249071698 ) ) ;
#68408 = FACE_BOUND ( 'NONE', #16286, .T. ) ;
#68407 = CARTESIAN_POINT ( 'NONE',  ( 177.3702169793795633, 264.4761424787041051, -15.61276723233572916 ) ) ;
#68409 = AXIS2_PLACEMENT_3D ( 'NONE', #52266, #67468, #45161 ) ;
#68410 = B_SPLINE_SURFACE_WITH_KNOTS ( 'NONE', 3, 1, ( 
 ( #90665, #6998 ),
 ( #51611, #52592 ),
 ( #29805, #75937 ),
 ( #61191, #74929 ),
 ( #21222, #97730 ),
 ( #22712, #5512 ),
 ( #76426, #91145 ),
 ( #20726, #83046 ),
 ( #59697, #13619 ),
 ( #75423, #37882 ),
 ( #52101, #60678 ),
 ( #68792, #21707 ),
 ( #6007, #43987 ),
 ( #91639, #44492 ),
 ( #83549, #22205 ),
 ( #90150, #36396 ),
 ( #98228, #14111 ),
 ( #30306, #67302 ),
 ( #99718, #37393 ),
 ( #36900, #67810 ),
 ( #44992, #53590 ),
 ( #53100, #6515 ),
 ( #28810, #98738 ),
 ( #15088, #29316 ),
 ( #60181, #68297 ),
 ( #84056, #92159 ),
 ( #76893, #45976 ),
 ( #35903, #66803 ),
 ( #1416, #100223 ),
 ( #46484, #86560 ),
 ( #17093, #77415 ) ),
 .UNSPECIFIED., .F., .F., .F.,
 ( 4, 3, 3, 3, 3, 3, 3, 3, 3, 3, 4 ),
 ( 2, 2 ),
 ( 0.000000000000000000, 0.1333490885032329043, 0.3007194338854160542, 0.4699862290244992691, 0.5844252810809290599, 0.6686540514502579136, 0.7354980260655432645, 0.8028463152565632477, 0.8633854507757217078, 0.9437142632667381292, 1.000000000000000000 ),
 ( 0.000000000000000000, 1.000000000000000000 ),
 .UNSPECIFIED. ) ;
#68411 = CARTESIAN_POINT ( 'NONE',  ( 22.17949989257922638, 28.50829794293881037, -10.00000000000000355 ) ) ;
#68412 = CARTESIAN_POINT ( 'NONE',  ( 148.9719199701866899, 272.6200610409887872, 12.59512981512031438 ) ) ;
#68413 = CARTESIAN_POINT ( 'NONE',  ( -19.51183051894608766, 93.07722767632783700, 59.99999999999999289 ) ) ;
#68414 = CARTESIAN_POINT ( 'NONE',  ( 32.15758756610207314, 177.8262482093457777, 3.021315404115420679E-15 ) ) ;
#68415 = CARTESIAN_POINT ( 'NONE',  ( 159.4889735931715222, 254.4039898200529706, 16.88104032092801887 ) ) ;
#68416 = CARTESIAN_POINT ( 'NONE',  ( 176.5750811079351763, 290.0661888821730372, -9.631901365267058424 ) ) ;
#68417 = CARTESIAN_POINT ( 'NONE',  ( 138.1351346183474220, 263.8927522451419918, 2.944929066748280225E-16 ) ) ;
#68418 = DIRECTION ( 'NONE',  ( 0.000000000000000000, -0.000000000000000000, -1.000000000000000000 ) ) ;
#68419 = ORIENTED_EDGE ( 'NONE', *, *, #22528, .T. ) ;
#68420 = CARTESIAN_POINT ( 'NONE',  ( 66.46987139367209352, 67.81550840317085260, -6.813679838459789195 ) ) ;
#68421 = CARTESIAN_POINT ( 'NONE',  ( 72.60008616680403293, 70.69752196365912766, -7.958780822297740976 ) ) ;
#68422 = CARTESIAN_POINT ( 'NONE',  ( 150.9003228897357189, 269.2799692068659283, -14.30003212299500781 ) ) ;
#68423 = CARTESIAN_POINT ( 'NONE',  ( 0.6624493194153854292, 177.3149278399161233, 9.188101187500093303 ) ) ;
#68424 = CARTESIAN_POINT ( 'NONE',  ( 32.31170220804710880, 20.78380873178788590, -6.180339887498949025 ) ) ;
#68425 = CARTESIAN_POINT ( 'NONE',  ( 85.04811473893079210, 48.86618300925753999, 12.37604778915560466 ) ) ;
#68426 = CARTESIAN_POINT ( 'NONE',  ( 170.1980103241066899, 270.7537944251233739, -16.96031082736039508 ) ) ;
#68427 = FACE_OUTER_BOUND ( 'NONE', #99651, .T. ) ;
#68428 = CARTESIAN_POINT ( 'NONE',  ( 150.1511997935914735, 276.5102290984758611, 3.993493173212648184 ) ) ;
#68429 = B_SPLINE_SURFACE_WITH_KNOTS ( 'NONE', 3, 1, ( 
 ( #65950, #3195 ),
 ( #28956, #5158 ),
 ( #29937, #66452 ),
 ( #36535, #98368 ),
 ( #37037, #44622 ),
 ( #83182, #43639 ),
 ( #66937, #19873 ),
 ( #81695, #91276 ),
 ( #97867, #82702 ),
 ( #67946, #75556 ),
 ( #13742, #74578 ),
 ( #90799, #28438 ),
 ( #58827, #29443 ),
 ( #59834, #52237 ),
 ( #21353, #98866 ),
 ( #83686, #6141 ),
 ( #60319, #35550 ),
 ( #59320, #21842 ),
 ( #36037, #90300 ),
 ( #89788, #20869 ),
 ( #60814, #76072 ),
 ( #52725, #14247 ),
 ( #51760, #45132 ),
 ( #20364, #12269 ),
 ( #6651, #13268 ),
 ( #44131, #75065 ),
 ( #43127, #5642 ),
 ( #67436, #37525 ),
 ( #68431, #74070 ),
 ( #99359, #50740 ),
 ( #4659, #97378 ),
 ( #27944, #51236 ),
 ( #82203, #12774 ),
 ( #40016, #1044 ) ),
 .UNSPECIFIED., .T., .F., .F.,
 ( 4, 2, 2, 2, 2, 2, 2, 2, 2, 2, 2, 2, 2, 2, 2, 2, 4 ),
 ( 2, 2 ),
 ( 0.000000000000000000, 0.06250000000000000000, 0.1250000000000000000, 0.1875000000000000000, 0.2500000000000000000, 0.3125000000000000000, 0.3750000000000000000, 0.4375000000000000000, 0.5000000000000000000, 0.5625000000000000000, 0.6250000000000000000, 0.6875000000000000000, 0.7500000000000000000, 0.8125000000000000000, 0.8750000000000000000, 0.9375000000000000000, 1.000000000000000000 ),
 ( 0.000000000000000000, 1.000000000000000000 ),
 .UNSPECIFIED. ) ;
#68430 = CARTESIAN_POINT ( 'NONE',  ( 179.3296690506923596, 255.1525901867891548, -3.997749341247230248 ) ) ;
#68431 = CARTESIAN_POINT ( 'NONE',  ( 198.2860450010354043, 287.2054909567549430, 18.54284983329501557 ) ) ;
#68432 = CARTESIAN_POINT ( 'NONE',  ( 62.88113547221017541, 197.1115022471902023, -5.000000000000041744 ) ) ;
#68433 = LINE ( 'NONE', #67442, #91162 ) ;
#68434 = CARTESIAN_POINT ( 'NONE',  ( 148.3519871123208986, 273.6938162480936398, 8.180046468253793890 ) ) ;
#68435 = CARTESIAN_POINT ( 'NONE',  ( 24.58674819472551931, 178.8768266524160140, 9.188101187500098632 ) ) ;
#68436 = CARTESIAN_POINT ( 'NONE',  ( 72.64601778605845084, 70.71744408260789783, -7.969226289351845516 ) ) ;
#68437 = B_SPLINE_CURVE_WITH_KNOTS ( 'NONE', 3,
 ( #86309, #47734, #24942, #16844, #78668, #71071, #94389, #40636, #35038, #96391, #35545, #19385, #11767, #97374, #82199, #87826, #18365, #26465, #43634, #12261, #51230, #4143, #49260, #96896, #3188, #12769, #80196, #11280, #50244, #4652, #81198, #27466, #74573, #64962, #27940, #19866, #26955, #36032, #88315, #18869 ),
 .UNSPECIFIED., .F., .F.,
 ( 4, 2, 2, 2, 2, 2, 2, 2, 2, 2, 2, 2, 2, 2, 2, 2, 2, 2, 2, 4 ),
 ( 0.003212077463089395204, 0.003408847110664717413, 0.003605616758240039622, 0.003704001582027700509, 0.003802386405815361397, 0.003999156053390615952, 0.004392695348541125061, 0.004786234643691634170, 0.005573313233992653257, 0.006360391824293673210, 0.007934549004895784241, 0.008032933828683409133, 0.008131318652471034025, 0.008155914858417923768, 0.008180511064364815246, 0.008229703476258487180, 0.008328088300045874415, 0.008721627595195399069, 0.009115166890344923722, 0.009508706185494448376 ),
 .UNSPECIFIED. ) ;
#68438 = CARTESIAN_POINT ( 'NONE',  ( 192.1640094933931096, 297.8091675017319062, 12.36911124822534447 ) ) ;
#68439 = DIRECTION ( 'NONE',  ( 0.000000000000000000, 0.000000000000000000, 1.000000000000000000 ) ) ;
#68440 = DIRECTION ( 'NONE',  ( -0.8452030915256490973, -0.5344452582589588330, 0.000000000000000000 ) ) ;
#68441 = EDGE_CURVE ( 'NONE', #70911, #50641, #87334, .T. ) ;
#68442 = CARTESIAN_POINT ( 'NONE',  ( 164.3774690880109119, 245.9368672504194819, -2.805681983503304000 ) ) ;
#68443 = CARTESIAN_POINT ( 'NONE',  ( 185.3632523845489288, 266.5794829961192818, 13.21810060833462863 ) ) ;
#68444 = CARTESIAN_POINT ( 'NONE',  ( 174.8023382843919080, 257.6605964823669979, 13.01024177398429060 ) ) ;
#68445 = CARTESIAN_POINT ( 'NONE',  ( 162.7215588690989989, 280.8608052963692217, 8.891366490498469943 ) ) ;
#68446 = CONTEXT_DEPENDENT_SHAPE_REPRESENTATION ( #79342, #25691 ) ;
#68447 = CARTESIAN_POINT ( 'NONE',  ( 14.59716579798650571, 20.37878583063839955, 9.188101187500006262 ) ) ;
#68448 = CARTESIAN_POINT ( 'NONE',  ( 147.6430623265936219, 274.9217099957185155, 8.258152514891218487 ) ) ;
#68449 = CARTESIAN_POINT ( 'NONE',  ( 71.98731340802646628, 59.17192410441948169, 15.36756879449314361 ) ) ;
#68450 = CARTESIAN_POINT ( 'NONE',  ( 193.8365934467825298, 294.9121671145370556, 14.14845633038902584 ) ) ;
#68451 = VERTEX_POINT ( 'NONE', #91010 ) ;
#68452 = CARTESIAN_POINT ( 'NONE',  ( 185.1474448761376834, 290.8322720534641803, 12.15833316867892044 ) ) ;
#68453 = CARTESIAN_POINT ( 'NONE',  ( 85.75095561453852611, 45.41483102380262693, -9.096727499225101710 ) ) ;
#68454 = CARTESIAN_POINT ( 'NONE',  ( 88.20309331078988180, 44.34480599067857298, 2.645673501954918905 ) ) ;
#68455 = CARTESIAN_POINT ( 'NONE',  ( 156.0554652282150983, 271.1402087238444665, 15.46858972464315229 ) ) ;
#68456 = ADVANCED_FACE ( 'NONE', ( #44849 ), #67665, .F. ) ;
#68457 = VERTEX_POINT ( 'NONE', #59545 ) ;
#68458 = CARTESIAN_POINT ( 'NONE',  ( -19.83262083840137180, 133.3759306620404459, -30.52142883766495629 ) ) ;
#68459 = CARTESIAN_POINT ( 'NONE',  ( 75.87151652897671283, 214.6115022471902591, 10.00000000000009592 ) ) ;
#68460 = CARTESIAN_POINT ( 'NONE',  ( 23.31615823149839173, 29.16454794089042224, -10.00000000000000355 ) ) ;
#68461 = EDGE_CURVE ( 'NONE', #95115, #78977, #43359, .T. ) ;
#68462 = CARTESIAN_POINT ( 'NONE',  ( 203.3740894404336927, 278.3927394765486838, -15.19753795879846869 ) ) ;
#68463 = VERTEX_POINT ( 'NONE', #4890 ) ;
#68464 = VERTEX_POINT ( 'NONE', #21573 ) ;
#68466 = DIRECTION ( 'NONE',  ( -0.000000000000000000, -0.000000000000000000, -1.000000000000000000 ) ) ;
#68465 = CARTESIAN_POINT ( 'NONE',  ( 202.3903227094629926, 279.6965068557100267, 15.56271535450856192 ) ) ;
#68467 = ORIENTED_EDGE ( 'NONE', *, *, #28064, .F. ) ;
#68468 = CARTESIAN_POINT ( 'NONE',  ( 191.2729698983822288, 299.3524933518466469, 8.871011392605806734 ) ) ;
#68469 = CARTESIAN_POINT ( 'NONE',  ( 20.88255934282640425, 35.55466486950700045, -1.111400068045478839E-16 ) ) ;
#68470 = CARTESIAN_POINT ( 'NONE',  ( 80.45778748667572700, 57.56998633490270123, -16.59146305250142817 ) ) ;
#68471 = CARTESIAN_POINT ( 'NONE',  ( 53.62548896571606605, 191.7677522451418213, -5.000000000000041744 ) ) ;
#68472 = ORIENTED_EDGE ( 'NONE', *, *, #89040, .F. ) ;
#68473 = CARTESIAN_POINT ( 'NONE',  ( 87.70425917765611246, 45.32258268275877811, -6.393467233578020270 ) ) ;
#68474 = ORIENTED_EDGE ( 'NONE', *, *, #99560, .F. ) ;
#68475 = CARTESIAN_POINT ( 'NONE',  ( 205.7668501412109663, 274.2483563724483133, 11.09689540819876896 ) ) ;
#68476 = CARTESIAN_POINT ( 'NONE',  ( 148.7305541605275607, 275.0381188865328568, -8.045727261058747359 ) ) ;
#68477 = VERTEX_POINT ( 'NONE', #66667 ) ;
#68478 = CARTESIAN_POINT ( 'NONE',  ( 149.6896757981861583, 271.3768714794653647, 12.49809796062302603 ) ) ;
#68479 = CARTESIAN_POINT ( 'NONE',  ( 78.21017654319952328, 47.49421537874133037, -13.82074165126671161 ) ) ;
#68480 = AXIS2_PLACEMENT_3D ( 'NONE', #80085, #26847, #96277 ) ;
#68481 = EDGE_LOOP ( 'NONE', ( #94230, #87265, #52138, #41912 ) ) ;
#68482 = B_SPLINE_CURVE_WITH_KNOTS ( 'NONE', 3,
 ( #87187, #33932, #2015, #1531, #63307, #64817, #79559, #41497, #95765, #40981, #94249, #80052, #10619, #24803, #57193, #88173, #18720, #49602, #80556, #55681, #86668, #17201, #79046, #9636, #34407, #96249, #50108, #11626, #81063, #65307, #57694, #26812, #42486, #88670, #73420, #19241, #93354, #129, #14327, #70514, #78135, #60902, #29529, #69514, #54294, #61409 ),
 .UNSPECIFIED., .F., .F.,
 ( 4, 1, 2, 2, 1, 2, 2, 1, 1, 2, 2, 1, 1, 2, 2, 1, 1, 2, 2, 1, 1, 1, 2, 2, 1, 1, 1, 2, 2, 4 ),
 ( 0.000000000000000000, 0.06249999999999741873, 0.09374999999999802935, 0.1249999999999986400, 0.1875000000000015266, 0.2187500000000030531, 0.2500000000000046074, 0.3125000000000126565, 0.3437500000000192069, 0.3593750000000220379, 0.3750000000000248135, 0.4375000000000291989, 0.4687500000000297540, 0.4843750000000322520, 0.5000000000000347500, 0.5625000000000445199, 0.5937500000000497380, 0.6093750000000524025, 0.6250000000000550671, 0.6875000000000631717, 0.7187500000000650591, 0.7343750000000655032, 0.7421875000000640599, 0.7500000000000626166, 0.8125000000000711653, 0.8437500000000753841, 0.8593750000000757172, 0.8671875000000740519, 0.8750000000000723865, 1.000000000000000000 ),
 .UNSPECIFIED. ) ;
#68483 = CARTESIAN_POINT ( 'NONE',  ( -10.53546450992863370, 72.07795844810249264, 14.77482737668580270 ) ) ;
#68484 = CARTESIAN_POINT ( 'NONE',  ( 93.62503730655774348, 214.8615022471902023, 5.000000000000051514 ) ) ;
#68485 = CARTESIAN_POINT ( 'NONE',  ( 78.33451385638642250, 47.33805271545526239, -14.25445639310817825 ) ) ;
#68486 = CARTESIAN_POINT ( 'NONE',  ( 83.83376537196386380, 51.97730738287452823, 14.54470171158602732 ) ) ;
#68487 = ORIENTED_EDGE ( 'NONE', *, *, #99295, .F. ) ;
#68488 = ORIENTED_EDGE ( 'NONE', *, *, #31190, .F. ) ;
#68490 = ADVANCED_FACE ( 'NONE', ( #98085 ), #60045, .F. ) ;
#68489 = B_SPLINE_CURVE_WITH_KNOTS ( 'NONE', 3,
 ( #64843, #65333, #17224, #33957, #94273, #2555, #70951, #33438, #1554, #24828 ),
 .UNSPECIFIED., .F., .F.,
 ( 4, 2, 2, 2, 4 ),
 ( 0.000000000000000000, 0.0002622400424272748110, 0.0005244800848545496221, 0.0007867201272818244873, 0.001048960169709099244 ),
 .UNSPECIFIED. ) ;
#68491 = CARTESIAN_POINT ( 'NONE',  ( 73.48837899454035494, 69.83143880527059366, 9.244587476903205925 ) ) ;
#68493 = VECTOR ( 'NONE', #41911, 1000.000000000000000 ) ;
#68492 = CARTESIAN_POINT ( 'NONE',  ( 83.46095475844008149, 42.81445974211163730, -5.980450563400608210 ) ) ;
#68494 = CARTESIAN_POINT ( 'NONE',  ( 146.9709166616330549, 276.0859004375172390, 3.755270622130282732 ) ) ;
#68495 = CARTESIAN_POINT ( 'NONE',  ( 82.30387339498274457, 53.64944443644738215, 15.82386716188995557 ) ) ;
#68496 = CARTESIAN_POINT ( 'NONE',  ( 190.8153366230912411, 300.1451374358846920, 3.771947273125533684 ) ) ;
#68497 = CARTESIAN_POINT ( 'NONE',  ( 153.3920560952016956, 264.9641606960921649, 16.50453917291963535 ) ) ;
#68498 = CARTESIAN_POINT ( 'NONE',  ( 147.2812597312705805, 275.5483704731282728, -0.2636021916935415432 ) ) ;
#68499 = CARTESIAN_POINT ( 'NONE',  ( 146.7818291168261453, 276.4134096722012828, -0.7617065417431535534 ) ) ;
#68500 = AXIS2_PLACEMENT_3D ( 'NONE', #83848, #4831, #6309 ) ;
#68501 = EDGE_CURVE ( 'NONE', #45411, #91719, #22604, .T. ) ;
#68502 = CARTESIAN_POINT ( 'NONE',  ( 190.0896302098338424, 301.4020978150248311, 3.433521196325825642 ) ) ;
#68503 = CARTESIAN_POINT ( 'NONE',  ( 70.58255314538416769, 68.84473063892380651, 8.184723017349652352 ) ) ;
#68505 = LINE ( 'NONE', #99427, #12716 ) ;
#68504 = CARTESIAN_POINT ( 'NONE',  ( 196.9431415128477170, 289.5314680279574304, -16.61413060656005669 ) ) ;
#68506 = DIRECTION ( 'NONE',  ( -0.2776767122488494333, -0.9606745773021526658, 0.000000000000000000 ) ) ;
#68507 = CARTESIAN_POINT ( 'NONE',  ( 168.2066918328904706, 286.4521719584415678, 3.767673903196911755 ) ) ;
#68508 = CARTESIAN_POINT ( 'NONE',  ( 78.43104943820020480, 47.80709632928548558, 13.91158340242805025 ) ) ;
#68509 = CARTESIAN_POINT ( 'NONE',  ( 105.4518702730974979, 225.5643266524160140, 9.188101187500095079 ) ) ;
#68510 = ORIENTED_EDGE ( 'NONE', *, *, #76717, .F. ) ;
#68511 = CARTESIAN_POINT ( 'NONE',  ( -22.42236680055709641, 157.8615022471902591, 0.000000000000000000 ) ) ;
#68512 = CARTESIAN_POINT ( 'NONE',  ( 71.97367111486161662, 69.50864518808729997, 8.459197605334548342 ) ) ;
#68513 = EDGE_CURVE ( 'NONE', #68082, #34660, #59041, .T. ) ;
#68514 = DIRECTION ( 'NONE',  ( -0.7226656227773308183, -0.6911977992267138715, 0.000000000000000000 ) ) ;
#68515 = CARTESIAN_POINT ( 'NONE',  ( 79.32956177646403262, 46.17935033225089825, 12.63826207646849120 ) ) ;
#68516 = DIRECTION ( 'NONE',  ( 0.5000000000000014433, -0.8660254037844378194, 0.000000000000000000 ) ) ;
#68517 = CARTESIAN_POINT ( 'NONE',  ( 187.7282692072121222, 287.3763760864540586, 16.35809696136310976 ) ) ;
#68518 = CARTESIAN_POINT ( 'NONE',  ( 166.2797251853322109, 284.7563794900764265, -8.621111623322635253 ) ) ;
#68519 = ORIENTED_EDGE ( 'NONE', *, *, #73090, .F. ) ;
#68520 = CARTESIAN_POINT ( 'NONE',  ( 208.1303168694798273, 270.1547119170880364, -0.9257663487928086132 ) ) ;
#68521 =( BOUNDED_CURVE ( )  B_SPLINE_CURVE ( 2, ( #90199, #97290, #74973, #5554, #88722, #19292, #67346, #89228, #58733 ),
 .UNSPECIFIED., .F., .T. ) 
 B_SPLINE_CURVE_WITH_KNOTS ( ( 3, 2, 2, 2, 3 ),
 ( 0.1491935483870967805, 0.1505376344086021556, 0.1532258064516129059, 0.1559139784946236562, 0.1572580645161290314 ),
 .UNSPECIFIED. ) 
 CURVE ( )  GEOMETRIC_REPRESENTATION_ITEM ( )  RATIONAL_B_SPLINE_CURVE ( ( 0.9330127018922194093, 0.9330127018922194093, 1.000000000000000000, 0.8660254037844387076, 1.000000000000000000, 0.8660254037844387076, 1.000000000000000000, 0.9330127018922194093, 0.9330127018922194093 ) ) 
 REPRESENTATION_ITEM ( '' )  );
#68522 = CARTESIAN_POINT ( 'NONE',  ( 159.2394649670193303, 254.8361514374751664, -16.43133403737800791 ) ) ;
#68523 = CARTESIAN_POINT ( 'NONE',  ( 72.38244233070295763, 71.76593646792086645, 5.668245152086877958 ) ) ;
#68524 = CARTESIAN_POINT ( 'NONE',  ( 43.73836560584370403, 189.3927522451417929, 10.00000000000009592 ) ) ;
#68525 = CARTESIAN_POINT ( 'NONE',  ( 111.5137010038235417, 241.3149278399160949, -9.188101187500095079 ) ) ;
#68526 = CARTESIAN_POINT ( 'NONE',  ( 180.7361392967986831, 294.1568954366646267, -3.145899629403025699 ) ) ;
#68527 = FACE_OUTER_BOUND ( 'NONE', #35609, .T. ) ;
#68528 = CARTESIAN_POINT ( 'NONE',  ( 195.9359860111818250, 291.2759125279654882, 17.49638312768267312 ) ) ;
#68529 = CARTESIAN_POINT ( 'NONE',  ( 175.5064957684375884, 253.4785342928385603, -4.458035672056321452 ) ) ;
#68530 = CARTESIAN_POINT ( 'NONE',  ( 39.11982377592438809, 184.2048013555409796, 4.594050593750051981 ) ) ;
#68531 = CARTESIAN_POINT ( 'NONE',  ( 15.77038241084232517, 34.14663330942826747, -10.00000000000000000 ) ) ;
#68532 = VERTEX_POINT ( 'NONE', #12998 ) ;
#68533 = CARTESIAN_POINT ( 'NONE',  ( 4.262040950003013862, 173.2677522451418781, 10.00000000000009592 ) ) ;
#68534 = CARTESIAN_POINT ( 'NONE',  ( 181.9013721714349856, 266.8816343884801086, 15.77960664470944430 ) ) ;
#68535 = DIRECTION ( 'NONE',  ( -0.8660254037844387076, -0.4999999999999998890, -0.000000000000000000 ) ) ;
#68536 = CARTESIAN_POINT ( 'NONE',  ( 147.3984236761635884, 275.3454365677582700, 5.108566646342994844 ) ) ;
#68537 = CARTESIAN_POINT ( 'NONE',  ( 81.95415531698857592, 41.13631750917600982, -5.408051707503558347 ) ) ;
#68538 = CARTESIAN_POINT ( 'NONE',  ( 81.92698409329203457, 58.82261968288553078, -0.3345653031794284527 ) ) ;
#68539 = LINE ( 'NONE', #30040, #38561 ) ;
#68540 = CARTESIAN_POINT ( 'NONE',  ( 97.79278455872236009, 237.2677522451419065, -5.000000000000047962 ) ) ;
#68541 = ORIENTED_EDGE ( 'NONE', *, *, #112, .F. ) ;
#68542 = ADVANCED_FACE ( 'NONE', ( #6373 ), #37256, .T. ) ;
#68543 = CARTESIAN_POINT ( 'NONE',  ( 207.4218731373931632, 271.3817724553659332, -5.249531240730909154 ) ) ;
#68544 = CARTESIAN_POINT ( 'NONE',  ( 158.6837034624547016, 282.0065499102733497, -1.619886856338979886 ) ) ;
#68545 = CARTESIAN_POINT ( 'NONE',  ( 207.7837159184916231, 270.7550423741513441, -2.369602332675663448 ) ) ;
#68546 = VECTOR ( 'NONE', #93281, 1000.000000000000000 ) ;
#68547 = CARTESIAN_POINT ( 'NONE',  ( 9.323050453024791295, 170.0643266524160140, 9.188101187500095079 ) ) ;
#68548 = CARTESIAN_POINT ( 'NONE',  ( 9.459751770947381289, 21.16454794089040092, -10.00000000000000355 ) ) ;
#68549 = CARTESIAN_POINT ( 'NONE',  ( 196.1346637562676278, 273.7134257057076070, 14.83932934806210113 ) ) ;
#68550 = CARTESIAN_POINT ( 'NONE',  ( 71.62750703794239371, 58.90906671320517773, -15.38493269445189426 ) ) ;
#68551 = DIRECTION ( 'NONE',  ( -0.8660254037844379305, -0.5000000000000014433, -0.000000000000000000 ) ) ;
#68553 = CARTESIAN_POINT ( 'NONE',  ( 62.47501251452968773, 213.0024278399160949, -9.188101187500093303 ) ) ;
#68552 = CARTESIAN_POINT ( 'NONE',  ( 194.7866383867829256, 274.9940630606773198, -16.01128562500261054 ) ) ;
#68554 = CARTESIAN_POINT ( 'NONE',  ( 163.8398374448017591, 246.8680725722146008, -5.948785025486735378 ) ) ;
#68555 = CARTESIAN_POINT ( 'NONE',  ( 72.83054026352687060, 57.09011829142805539, 16.39008592795239494 ) ) ;
#68556 = CARTESIAN_POINT ( 'NONE',  ( -31.69055000258023824, 96.81751122025097800, 44.38391476979933969 ) ) ;
#68557 = CARTESIAN_POINT ( 'NONE',  ( 66.06942622996319869, 68.50909977235997417, -4.639585442171386021 ) ) ;
#68558 = VERTEX_POINT ( 'NONE', #91495 ) ;
#68559 = MECHANICAL_DESIGN_GEOMETRIC_PRESENTATION_REPRESENTATION (  '', ( #39400 ), #96104 ) ;
#68560 = CARTESIAN_POINT ( 'NONE',  ( 7.816353548249534100, 181.9865022471903160, 10.00000000000009237 ) ) ;
#68561 = CARTESIAN_POINT ( 'NONE',  ( 207.5570596878370679, 271.1476224814971374, 2.444960520848353358 ) ) ;
#68562 = VECTOR ( 'NONE', #60674, 1000.000000000000114 ) ;
#68563 = CARTESIAN_POINT ( 'NONE',  ( 138.6852480475602931, 257.0024278399161517, 9.188101187500095079 ) ) ;
#68564 = CARTESIAN_POINT ( 'NONE',  ( 25.79477067763620468, 36.93396525600391556, 2.839279412974139660 ) ) ;
#68565 = CARTESIAN_POINT ( 'NONE',  ( -52.86010516724736163, 91.71679868308304151, -10.00000000000000000 ) ) ;
#68566 = LINE ( 'NONE', #45751, #40010 ) ;
#68567 = VECTOR ( 'NONE', #97540, 1000.000000000000000 ) ;
#68569 = DIRECTION ( 'NONE',  ( -1.000000000000000000, 0.000000000000000000, 0.000000000000000000 ) ) ;
#68568 = CARTESIAN_POINT ( 'NONE',  ( 83.21354822495420933, 40.96322299393881394, -2.105546863297833582 ) ) ;
#68570 = CARTESIAN_POINT ( 'NONE',  ( 69.03518170980191826, 64.49507618479454152, 12.45339560626615949 ) ) ;
#68571 = ORIENTED_EDGE ( 'NONE', *, *, #38722, .T. ) ;
#68572 = CARTESIAN_POINT ( 'NONE',  ( 62.79092448910137847, 200.3927522451417929, -10.00000000000009237 ) ) ;
#68573 = CARTESIAN_POINT ( 'NONE',  ( 208.3055888496142813, 269.8511319423524242, -0.4960542269038109575 ) ) ;
#68574 = CARTESIAN_POINT ( 'NONE',  ( 72.51084313652232538, 66.78536858707103363, -12.23974485817613100 ) ) ;
#68575 = CARTESIAN_POINT ( 'NONE',  ( 156.6930436047642843, 280.2728101775987284, -5.381237359922138808 ) ) ;
#68576 = CARTESIAN_POINT ( 'NONE',  ( 197.4075646047015482, 273.1427705089788560, -14.69744958829762815 ) ) ;
#68577 = EDGE_LOOP ( 'NONE', ( #74255, #97787, #69883, #51269 ) ) ;
#68578 = CARTESIAN_POINT ( 'NONE',  ( 165.5752708168755305, 245.8622137986321832, -1.085626278946311585 ) ) ;
#68579 = CARTESIAN_POINT ( 'NONE',  ( -27.42236680055714260, 166.5217562850347406, 1.224646799147364892E-15 ) ) ;
#68580 = CARTESIAN_POINT ( 'NONE',  ( -1.846057691949487101, 43.12070627514476229, 59.99999999999999289 ) ) ;
#68581 = EDGE_CURVE ( 'NONE', #93085, #57035, #60385, .T. ) ;
#68582 = LINE ( 'NONE', #21987, #6875 ) ;
#68583 = CARTESIAN_POINT ( 'NONE',  ( 26.50806851326369440, 186.1115022471902591, 10.00000000000009592 ) ) ;
#68584 = CARTESIAN_POINT ( 'NONE',  ( 40.20209520705726192, 184.0177522451417929, 5.000000000000051514 ) ) ;
#68585 = EDGE_CURVE ( 'NONE', #24573, #38349, #38717, .T. ) ;
#68586 = CARTESIAN_POINT ( 'NONE',  ( 163.1096928939807924, 248.1327200311062882, -9.690381021358412283 ) ) ;
#68587 = CARTESIAN_POINT ( 'NONE',  ( 153.0308080659177392, 265.5898606369461277, -17.74682723936668438 ) ) ;
#68588 = EDGE_LOOP ( 'NONE', ( #65716, #6075, #59889, #91964 ) ) ;
#68589 = CARTESIAN_POINT ( 'NONE',  ( 190.8462995483115776, 280.9575646962753126, 16.64796827995540696 ) ) ;
#68590 = CARTESIAN_POINT ( 'NONE',  ( 7.946103921272086090, 26.36126292948893735, 6.180339887498949913 ) ) ;
#68591 = LINE ( 'NONE', #99514, #15879 ) ;
#68592 = VERTEX_POINT ( 'NONE', #54427 ) ;
#68593 = CARTESIAN_POINT ( 'NONE',  ( 149.2561433752359505, 272.1277716627430436, 12.99353668144589946 ) ) ;
#68594 = CARTESIAN_POINT ( 'NONE',  ( 86.33167747996513697, 46.96304910452010262, -10.52679092302835251 ) ) ;
#68595 = CARTESIAN_POINT ( 'NONE',  ( 83.75784171508648512, 45.20434354284536482, -9.539610091384043145 ) ) ;
#68596 = ORIENTED_EDGE ( 'NONE', *, *, #60522, .T. ) ;
#68597 = CARTESIAN_POINT ( 'NONE',  ( 191.2111338740054975, 299.4595964878050154, -9.718193530796334301 ) ) ;
#68598 = DIRECTION ( 'NONE',  ( -0.6139877827364833562, 0.7893155279419866721, 0.000000000000000000 ) ) ;
#68599 = CARTESIAN_POINT ( 'NONE',  ( 204.3951397407346064, 276.6242284793436852, 14.79595971842109137 ) ) ;
#68600 = CARTESIAN_POINT ( 'NONE',  ( 69.84702423369627411, 62.74498161306693333, 13.91467287971852329 ) ) ;
#68601 = ORIENTED_EDGE ( 'NONE', *, *, #2021, .T. ) ;
#68602 = CARTESIAN_POINT ( 'NONE',  ( 97.38683515247240052, 227.0333772461660544, 9.188101187500095079 ) ) ;
#68603 = CARTESIAN_POINT ( 'NONE',  ( 155.0006381209259132, 262.1780148993956345, 17.98662963467628728 ) ) ;
#68604 = CARTESIAN_POINT ( 'NONE',  ( 73.36513840663161545, 69.69468182635826281, -9.911920066630193205 ) ) ;
#68605 = CARTESIAN_POINT ( 'NONE',  ( 181.3429656143923694, 271.2897672401974205, -16.00655333216852938 ) ) ;
#68606 = CARTESIAN_POINT ( 'NONE',  ( 81.50676111512028399, 42.61959527892759070, -7.662561320371898077 ) ) ;
#68607 = ORIENTED_EDGE ( 'NONE', *, *, #13041, .F. ) ;
#68608 = ORIENTED_EDGE ( 'NONE', *, *, #26647, .T. ) ;
#68609 = ORIENTED_EDGE ( 'NONE', *, *, #79150, .F. ) ;
#68610 = CARTESIAN_POINT ( 'NONE',  ( 159.0836013084991123, 281.9351143348985715, -6.237652159340437485 ) ) ;
#68611 = VERTEX_POINT ( 'NONE', #15434 ) ;
#68612 = CARTESIAN_POINT ( 'NONE',  ( 68.34715014356760321, 68.60616615819722597, 6.278734008161547919 ) ) ;
#68613 = CARTESIAN_POINT ( 'NONE',  ( 87.88245627177123254, 44.92329797532172364, 6.249457923817313798 ) ) ;
#68614 = ORIENTED_EDGE ( 'NONE', *, *, #70380, .T. ) ;
#68615 = LINE ( 'NONE', #38706, #18660 ) ;
#68616 = EDGE_CURVE ( 'NONE', #63738, #81254, #63054, .T. ) ;
#68617 = CARTESIAN_POINT ( 'NONE',  ( 167.7068093616764486, 281.0861989796462694, 11.58686271003535850 ) ) ;
#68618 = CARTESIAN_POINT ( 'NONE',  ( -23.52037902133706027, 99.78538021036720806, 45.19948689642177442 ) ) ;
#68619 = CARTESIAN_POINT ( 'NONE',  ( 68.61954826535414043, 68.39247321939140534, -6.997216880091692737 ) ) ;
#68620 = ORIENTED_EDGE ( 'NONE', *, *, #78491, .F. ) ;
#68621 = DIRECTION ( 'NONE',  ( -0.5000000000000014433, 0.8660254037844378194, 0.000000000000000000 ) ) ;
#68622 = CARTESIAN_POINT ( 'NONE',  ( 19.86064915544625009, 12.26216523072493914, -2.296566073217252530E-15 ) ) ;
#68623 = CARTESIAN_POINT ( 'NONE',  ( 201.2356561511845143, 278.8713745403558164, -15.71208516001683364 ) ) ;
#68624 = B_SPLINE_CURVE_WITH_KNOTS ( 'NONE', 3,
 ( #20482, #65568, #92394, #76184, #75183, #30049, #20991, #82324, #22454, #44737, #52350, #67055, #21954, #98976, #5272, #59942 ),
 .UNSPECIFIED., .F., .F.,
 ( 4, 1, 2, 2, 2, 1, 2, 2, 4 ),
 ( 0.000000000000000000, 0.1250000000000021649, 0.1875000000000032474, 0.2500000000000043299, 0.5000000000000027756, 0.6250000000000019984, 0.6875000000000016653, 0.7500000000000013323, 1.000000000000000000 ),
 .UNSPECIFIED. ) ;
#68625 = CARTESIAN_POINT ( 'NONE',  ( 80.03143596134809457, 57.61873189500684589, 16.60059503390608882 ) ) ;
#68627 = VERTEX_POINT ( 'NONE', #94491 ) ;
#68626 = CARTESIAN_POINT ( 'NONE',  ( -65.66987298107781612, 17.49999999999999645, 10.00000000000000178 ) ) ;
#68628 = CARTESIAN_POINT ( 'NONE',  ( 202.9685995779611858, 279.0950685203052899, 16.84977534244423580 ) ) ;
#68629 = CARTESIAN_POINT ( 'NONE',  ( 186.1008340985782752, 259.4276452379801299, 2.884016300632598284 ) ) ;
#68630 = CARTESIAN_POINT ( 'NONE',  ( 80.24160137367489654, 44.78810531146535823, 11.12097059984180980 ) ) ;
#68631 = CARTESIAN_POINT ( 'NONE',  ( -38.35373792487678202, 26.90998726756845727, 10.00000000000000000 ) ) ;
#68632 = AXIS2_PLACEMENT_3D ( 'NONE', #69664, #54960, #85939 ) ;
#68633 = CARTESIAN_POINT ( 'NONE',  ( 161.2799361541916028, 251.3019516699124836, 14.40628917569557110 ) ) ;
#68634 = CARTESIAN_POINT ( 'NONE',  ( 194.7648128082431072, 263.0520082674682953, -0.7993879730480621948 ) ) ;
#68635 = EDGE_LOOP ( 'NONE', ( #11727, #8439, #77734, #28473 ) ) ;
#68636 = CARTESIAN_POINT ( 'NONE',  ( 181.4811969836216861, 271.1666789078223019, -15.96325902370808159 ) ) ;
#68637 = CARTESIAN_POINT ( 'NONE',  ( 73.75273084276152247, 62.67190600634478415, -14.57620950672273707 ) ) ;
#68638 = FACE_OUTER_BOUND ( 'NONE', #90369, .T. ) ;
#68639 = CARTESIAN_POINT ( 'NONE',  ( 9.458193372709686741, 166.2677522451418213, -5.000000000000041744 ) ) ;
#68640 = CIRCLE ( 'NONE', #57358, 7.273499999999997634 ) ;
#68641 = CARTESIAN_POINT ( 'NONE',  ( 82.86119955336803855, 53.69823230216047705, -15.38187069736933665 ) ) ;
#68642 = CARTESIAN_POINT ( 'NONE',  ( 175.0267821627883507, 281.5489919625649122, -14.11785333599694425 ) ) ;
#68643 = CARTESIAN_POINT ( 'NONE',  ( 204.2021211322627892, 276.9585465160237732, -15.48642194502425440 ) ) ;
#68644 = B_SPLINE_CURVE_WITH_KNOTS ( 'NONE', 3,
 ( #45887, #99134, #70195, #15493, #38297, #804, #22118, #61098, #22619, #100132, #92069, #30719, #45407, #16008, #76338, #6911, #68705, #84948, #92552, #99633, #69207, #23098, #53989, #38799, #54484, #69705, #85463, #63106, #56996, #47889, #57495, #55486, #33209, #10927, #18027, #32202, #88476, #96058, #64619, #33729, #86472, #94052, #25620, #16999, #47401, #86978, #10420, #55981 ),
 .UNSPECIFIED., .F., .F.,
 ( 4, 2, 2, 2, 2, 2, 2, 2, 2, 2, 2, 2, 2, 2, 2, 2, 2, 2, 2, 2, 2, 2, 2, 4 ),
 ( 0.001976462477795229607, 0.002421830707482981737, 0.002644514822326855634, 0.002867198937170729964, 0.002978540994592638290, 0.003089883052014547483, 0.003201225109436455808, 0.003312567166858364567, 0.003535251281702188157, 0.003757935396546011747, 0.004648671855921450088, 0.005539408315296888430, 0.006430144774672326771, 0.006875513004360045075, 0.007320881234047764245, 0.007432223291469675606, 0.007487894320180630420, 0.007543565348891586100, 0.007654907406313499196, 0.007766249463735411425, 0.008211617693423052533, 0.008656985923110694509, 0.008879670037954518966, 0.009102354152798343423 ),
 .UNSPECIFIED. ) ;
#68645 = CARTESIAN_POINT ( 'NONE',  ( 82.45365866864536031, 44.73731268782142934, -9.806852841930714604 ) ) ;
#68646 = EDGE_CURVE ( 'NONE', #53225, #76651, #91843, .T. ) ;
#68648 = CARTESIAN_POINT ( 'NONE',  ( -5.697251193518073187, 177.5177522451419350, 5.000000000000046185 ) ) ;
#68647 = CARTESIAN_POINT ( 'NONE',  ( -7.997804718428996651, 172.3149278399160949, -9.188101187500095079 ) ) ;
#68649 = CARTESIAN_POINT ( 'NONE',  ( 163.8066603109232346, 248.5069834890703078, 9.830012707353159129 ) ) ;
#68650 = VERTEX_POINT ( 'NONE', #77256 ) ;
#68651 = ORIENTED_EDGE ( 'NONE', *, *, #51690, .T. ) ;
#68652 = DIRECTION ( 'NONE',  ( 1.000000000000000000, 0.000000000000000000, -0.000000000000000000 ) ) ;
#68653 = CARTESIAN_POINT ( 'NONE',  ( -22.42236680055709641, 157.8615022471902591, 0.000000000000000000 ) ) ;
#68654 = CARTESIAN_POINT ( 'NONE',  ( 163.8835510476618254, 277.4261113242017132, -14.47671527678674330 ) ) ;
#68655 = CARTESIAN_POINT ( 'NONE',  ( 197.9278932102866122, 265.8241103735087449, -6.306740378884746256 ) ) ;
#68656 = CARTESIAN_POINT ( 'NONE',  ( 162.6049147221665123, 249.0070214712401935, -10.34353492225723059 ) ) ;
#68657 = CARTESIAN_POINT ( 'NONE',  ( 151.9458057874326755, 277.5688626660769387, 3.700970285374547419 ) ) ;
#68658 = CARTESIAN_POINT ( 'NONE',  ( 10.89220085373657199, 189.3464784336661353, 1.353441290958777525E-15 ) ) ;
#68659 = CARTESIAN_POINT ( 'NONE',  ( 113.9495709998497688, 236.5958772461660544, -9.188101187500095079 ) ) ;
#68660 = CARTESIAN_POINT ( 'NONE',  ( 179.1166397756549316, 291.9316799655679233, -6.147037684395432855 ) ) ;
#68661 = CARTESIAN_POINT ( 'NONE',  ( 121.6288370910339722, 229.4824982072973398, 3.021315404115420679E-15 ) ) ;
#68662 = CARTESIAN_POINT ( 'NONE',  ( 79.24882819772426501, 57.92845866569951596, 16.22381856495110597 ) ) ;
#68663 = CARTESIAN_POINT ( 'NONE',  ( -19.65312891409030271, 93.06504152958497400, 177.5919119679930134 ) ) ;
#68664 = CYLINDRICAL_SURFACE ( 'NONE', #68632, 10.00000000000010658 ) ;
#68665 = CARTESIAN_POINT ( 'NONE',  ( -7.332799823397643024, 36.44574457902104569, 59.99999999999999289 ) ) ;
#68666 = CARTESIAN_POINT ( 'NONE',  ( 161.7767236248226084, 250.4414905302161287, -13.15904643207033153 ) ) ;
#68667 = DIRECTION ( 'NONE',  ( -0.000000000000000000, -0.000000000000000000, -1.000000000000000000 ) ) ;
#68668 = CARTESIAN_POINT ( 'NONE',  ( 165.0391502558331069, 249.6778246878102436, -10.74756611015070717 ) ) ;
#68669 = CARTESIAN_POINT ( 'NONE',  ( 196.1190320836150249, 265.9249367091900353, 8.391681110388155673 ) ) ;
#68671 = CARTESIAN_POINT ( 'NONE',  ( 70.37262225357338252, 70.61908426682903439, 4.266529024624744260 ) ) ;
#68670 = B_SPLINE_CURVE_WITH_KNOTS ( 'NONE', 3,
 ( #56389, #93939, #9300, #40176 ),
 .UNSPECIFIED., .F., .F.,
 ( 4, 4 ),
 ( 0.001557053815687444972, 0.008487571838833373600 ),
 .UNSPECIFIED. ) ;
#68672 = CARTESIAN_POINT ( 'NONE',  ( 206.9985020284622408, 270.1150727264914053, 3.388313042214953441 ) ) ;
#68673 = CARTESIAN_POINT ( 'NONE',  ( 79.14312167556931854, 57.64441083166269664, 0.000000000000000000 ) ) ;
#68674 = ORIENTED_EDGE ( 'NONE', *, *, #29594, .F. ) ;
#68675 = DIRECTION ( 'NONE',  ( -0.9008877160804935613, -0.4340522123146846045, 0.000000000000000000 ) ) ;
#68676 = CARTESIAN_POINT ( 'NONE',  ( 81.85743566648118019, 41.23085629097093374, -5.772627936764054724 ) ) ;
#68677 = CARTESIAN_POINT ( 'NONE',  ( 92.97525793012167128, 233.6744531367911293, 4.594050593750047540 ) ) ;
#68678 = CARTESIAN_POINT ( 'NONE',  ( 12.70933400901951416, 9.198606405272903075, 2.839279412974134775 ) ) ;
#68679 = CARTESIAN_POINT ( 'NONE',  ( 190.9061255863007318, 299.9878863388391892, 7.497146773253707153 ) ) ;
#68680 = CARTESIAN_POINT ( 'NONE',  ( 21.13464251418870532, 61.24490853227566589, 59.99999999999999289 ) ) ;
#68682 = CARTESIAN_POINT ( 'NONE',  ( 192.3574160861219298, 277.4804554469715185, 16.46682601177359473 ) ) ;
#68681 = CARTESIAN_POINT ( 'NONE',  ( 140.6610420460521311, 252.0177522451418213, -10.00000000000009592 ) ) ;
#68683 = CARTESIAN_POINT ( 'NONE',  ( 196.3322077676189394, 290.5896363147520560, 17.46901783180497603 ) ) ;
#68684 = CARTESIAN_POINT ( 'NONE',  ( 156.1857201963304362, 277.6936791020598889, 10.39727624116721749 ) ) ;
#68685 = DIRECTION ( 'NONE',  ( 1.000000000000000000, 0.000000000000000000, 0.000000000000000000 ) ) ;
#68686 = CARTESIAN_POINT ( 'NONE',  ( 36.38853680410607438, 41.98502408145596121, -5.678558825948271327 ) ) ;
#68687 = CARTESIAN_POINT ( 'NONE',  ( -22.42236680055709641, 157.8615022471902591, 0.000000000000000000 ) ) ;
#68688 = VERTEX_POINT ( 'NONE', #7864 ) ;
#68689 = CARTESIAN_POINT ( 'NONE',  ( 23.88951478931043937, 35.83396525600391413, -2.839279412974133887 ) ) ;
#68690 = CARTESIAN_POINT ( 'NONE',  ( 178.7251872717625929, 280.4929491208731065, 15.86704982540033981 ) ) ;
#68691 = CARTESIAN_POINT ( 'NONE',  ( 147.5540328368684300, 275.0759135952944234, -4.750028533202499403 ) ) ;
#68692 = CARTESIAN_POINT ( 'NONE',  ( 149.2765980486851731, 272.0923431290771646, -11.40617906909507973 ) ) ;
#68693 = EDGE_LOOP ( 'NONE', ( #38059, #30982, #29098, #37835 ) ) ;
#68694 = B_SPLINE_CURVE_WITH_KNOTS ( 'NONE', 3,
 ( #90299, #5641, #59319, #88825, #89316, #57844, #19390, #81203, #50249, #11772, #74068, #4147, #73564, #27943, #35043, #65947 ),
 .UNSPECIFIED., .F., .F.,
 ( 4, 1, 2, 2, 2, 1, 2, 2, 4 ),
 ( 0.000000000000000000, 0.1249999999999996114, 0.1874999999999998612, 0.2500000000000001110, 0.5000000000000000000, 0.6249999999999997780, 0.6874999999999998890, 0.7499999999999998890, 1.000000000000000000 ),
 .UNSPECIFIED. ) ;
#68695 = EDGE_CURVE ( 'NONE', #1759, #81254, #8009, .T. ) ;
#68696 = CARTESIAN_POINT ( 'NONE',  ( 152.7731995575106509, 275.0936207477257085, 10.86798791317738200 ) ) ;
#68697 = CARTESIAN_POINT ( 'NONE',  ( 198.6742831389107096, 286.5330427765190393, 17.60232614297041565 ) ) ;
#68698 =( GEOMETRIC_REPRESENTATION_CONTEXT ( 3 ) GLOBAL_UNCERTAINTY_ASSIGNED_CONTEXT ( ( #33154 ) ) GLOBAL_UNIT_ASSIGNED_CONTEXT ( ( #20316, #25927, #22291 ) ) REPRESENTATION_CONTEXT ( 'NONE', 'WORKASPACE' ) );
#68699 = CARTESIAN_POINT ( 'NONE',  ( 180.4665312189673330, 261.7265043435623966, -13.29892058382729481 ) ) ;
#68700 = ADVANCED_FACE ( 'NONE', ( #85403 ), #93493, .F. ) ;
#68701 = CARTESIAN_POINT ( 'NONE',  ( 169.3882425167235795, 252.1626239731313888, -8.756318688425812624 ) ) ;
#68702 = DIRECTION ( 'NONE',  ( 0.000000000000000000, 0.000000000000000000, 1.000000000000000000 ) ) ;
#68703 = CARTESIAN_POINT ( 'NONE',  ( 147.3186123411928747, 255.8615022471902307, -10.00000000000009592 ) ) ;
#68704 = VERTEX_POINT ( 'NONE', #70137 ) ;
#68705 = CARTESIAN_POINT ( 'NONE',  ( 187.4090223870812792, 278.8944490661542659, 17.04039641662812343 ) ) ;
#68706 = B_SPLINE_SURFACE_WITH_KNOTS ( 'NONE', 3, 1, ( 
 ( #78288, #85943 ),
 ( #17474, #9896 ),
 ( #55945, #7887 ),
 ( #16469, #39738 ),
 ( #86942, #64078 ),
 ( #62551, #31159 ),
 ( #94015, #46352 ),
 ( #56471, #32168 ),
 ( #40257, #48384 ),
 ( #71197, #95022 ),
 ( #32672, #1790 ),
 ( #62048, #15970 ),
 ( #47365, #46872 ),
 ( #93514, #93001 ),
 ( #79328, #40754 ),
 ( #47854, #77796 ),
 ( #63571, #94514 ),
 ( #71703, #24071 ),
 ( #1284, #54964 ),
 ( #8872, #24567 ),
 ( #55450, #86437 ),
 ( #70669, #16963 ),
 ( #78791, #70157 ),
 ( #2297, #25068 ),
 ( #33177, #25585 ),
 ( #23554, #38763 ),
 ( #9379, #15454 ),
 ( #54446, #77276 ),
 ( #69668, #274 ),
 ( #8381, #39247 ),
 ( #767, #31654 ),
 ( #44497, #98741 ),
 ( #67307, #21713 ),
 ( #13625, #54087 ) ),
 .UNSPECIFIED., .T., .F., .F.,
 ( 4, 2, 2, 2, 2, 2, 2, 2, 2, 2, 2, 2, 2, 2, 2, 2, 4 ),
 ( 2, 2 ),
 ( 0.000000000000000000, 0.06250000000000000000, 0.1250000000000000000, 0.1875000000000000000, 0.2500000000000000000, 0.3125000000000000000, 0.3750000000000000000, 0.4375000000000000000, 0.5000000000000000000, 0.5625000000000000000, 0.6250000000000000000, 0.6875000000000000000, 0.7500000000000000000, 0.8125000000000000000, 0.8750000000000000000, 0.9375000000000000000, 1.000000000000000000 ),
 ( 0.000000000000000000, 1.000000000000000000 ),
 .UNSPECIFIED. ) ;
#68707 = ADVANCED_FACE ( 'NONE', ( #32147 ), #8363, .F. ) ;
#68708 = CARTESIAN_POINT ( 'NONE',  ( 36.52324494929276710, 26.80170272979929180, 7.433330006724137462 ) ) ;
#68709 = ORIENTED_EDGE ( 'NONE', *, *, #2322, .F. ) ;
#68710 = CARTESIAN_POINT ( 'NONE',  ( 167.2398491818434536, 249.6619807853312238, 6.963124153055272991 ) ) ;
#68711 = EDGE_CURVE ( 'NONE', #18010, #566, #85924, .T. ) ;
#68712 = CARTESIAN_POINT ( 'NONE',  ( 184.9360691488573423, 292.3413084151380303, -10.69521170824177503 ) ) ;
#68714 = ORIENTED_EDGE ( 'NONE', *, *, #57133, .F. ) ;
#68713 = VECTOR ( 'NONE', #48149, 1000.000000000000000 ) ;
#68715 = DIRECTION ( 'NONE',  ( -0.9862134920484689760, -0.1654779384134469067, 0.000000000000000000 ) ) ;
#68716 = LINE ( 'NONE', #30222, #71860 ) ;
#68717 = CARTESIAN_POINT ( 'NONE',  ( 190.8509455208771044, 278.0625209715795449, -16.97381849757700678 ) ) ;
#68718 = CARTESIAN_POINT ( 'NONE',  ( 192.7905631387375820, 296.7239447543280448, -13.53553090723447205 ) ) ;
#68719 = CARTESIAN_POINT ( 'NONE',  ( 153.3506059258413643, 265.0359544954067132, -16.39100908615009899 ) ) ;
#68720 = CARTESIAN_POINT ( 'NONE',  ( 41.82943821127123840, 26.01110640527295814, 2.839279412974134775 ) ) ;
#68721 = CARTESIAN_POINT ( 'NONE',  ( 81.62646408706272894, 55.64454924624774890, -16.33875670839028516 ) ) ;
#68722 = B_SPLINE_CURVE_WITH_KNOTS ( 'NONE', 3,
 ( #44714, #60412, #7730, #69019, #21443, #99949, #84280, #14338, #45227, #13838, #30028, #67532, #82792, #51851, #91368, #91879, #53324, #76164, #52329, #83270, #21931, #84771, #20969, #46206, #38106, #75647, #138, #6741, #15307, #14825, #61420, #6233, #45714, #13358, #52821, #37618, #30533, #83777, #38618, #68529, #22432, #99452, #37128, #75160, #68035, #69527, #76637, #92372, #98956, #22920 ),
 .UNSPECIFIED., .F., .F.,
 ( 4, 2, 2, 2, 2, 2, 2, 2, 2, 2, 2, 2, 2, 2, 2, 2, 2, 2, 2, 2, 2, 2, 2, 2, 4 ),
 ( 0.0006152650805149372047, 0.001045760051675842604, 0.001261007537256295195, 0.001368631280046588711, 0.001476255022836882227, 0.001691502508417469476, 0.001906749993998056725, 0.002337244965159098950, 0.003198234907481184268, 0.004059224849803269586, 0.004920214792125354904, 0.005350709763286351159, 0.005565957248866859261, 0.005673580991657032647, 0.005727392863052129315, 0.005781204734447225983, 0.005835016605842323519, 0.005888828477237420186, 0.005996452220027617859, 0.006211699705608018408, 0.006642194676768819507, 0.006857442162349277302, 0.007072689647929735098, 0.007287937133510192893, 0.007503184619090650688 ),
 .UNSPECIFIED. ) ;
#68723 = B_SPLINE_CURVE_WITH_KNOTS ( 'NONE', 3,
 ( #52888, #6300, #45772, #77714 ),
 .UNSPECIFIED., .F., .F.,
 ( 4, 4 ),
 ( 0.04263745385576789282, 0.04887120950165272509 ),
 .UNSPECIFIED. ) ;
#68724 = CARTESIAN_POINT ( 'NONE',  ( -27.77457187288641904, 24.79904599702367562, -10.00000000000000000 ) ) ;
#68725 = VERTEX_POINT ( 'NONE', #55428 ) ;
#68726 = CARTESIAN_POINT ( 'NONE',  ( 162.7395313153677989, 249.4784413565320165, 10.93946270999009052 ) ) ;
#68727 = ORIENTED_EDGE ( 'NONE', *, *, #57745, .T. ) ;
#68728 = ORIENTED_EDGE ( 'NONE', *, *, #46448, .F. ) ;
#68729 = CARTESIAN_POINT ( 'NONE',  ( 198.1322097300599125, 286.5433749449028937, 17.04145067767304056 ) ) ;
#68730 = CARTESIAN_POINT ( 'NONE',  ( 164.0781508658037637, 275.4055464209769752, 15.63836535835214114 ) ) ;
#68732 = LINE ( 'NONE', #8936, #94495 ) ;
#68731 = CARTESIAN_POINT ( 'NONE',  ( 183.3634088509504352, 284.6525016221286251, -16.42631288611494256 ) ) ;
#68733 = FACE_OUTER_BOUND ( 'NONE', #11220, .T. ) ;
#68734 = CARTESIAN_POINT ( 'NONE',  ( 197.4191597201339619, 273.2215227944986395, -13.36937406163023390 ) ) ;
#68735 = CARTESIAN_POINT ( 'NONE',  ( 75.96712627484227198, 60.44064756120551607, -15.70488828003969672 ) ) ;
#68736 = CARTESIAN_POINT ( 'NONE',  ( 82.32788549632455499, 40.35540550160623496, 1.181641335447100483 ) ) ;
#68737 = CARTESIAN_POINT ( 'NONE',  ( 188.2892141557378807, 278.5232933803065976, -17.80357329707993941 ) ) ;
#68738 = CARTESIAN_POINT ( 'NONE',  ( 165.8190036485819689, 266.0137150170749010, 17.53662559932599407 ) ) ;
#68739 = CARTESIAN_POINT ( 'NONE',  ( 186.8225631894460150, 287.0909073165248628, -15.81189067252249458 ) ) ;
#68740 = CARTESIAN_POINT ( 'NONE',  ( 115.2486091055264410, 237.3458772461660544, 9.188101187500095079 ) ) ;
#68741 = ORIENTED_EDGE ( 'NONE', *, *, #15010, .F. ) ;
#68742 = CARTESIAN_POINT ( 'NONE',  ( 148.0508535842240008, 274.6303860046891145, -6.128032407862696651 ) ) ;
#68743 = CARTESIAN_POINT ( 'NONE',  ( 160.0166746459236435, 283.6086068001695253, 2.232576205374148248 ) ) ;
#68744 = CARTESIAN_POINT ( 'NONE',  ( 188.0633326902639624, 273.6994922365734055, 15.81873844000643992 ) ) ;
#68745 = ORIENTED_EDGE ( 'NONE', *, *, #62082, .F. ) ;
#68746 = AXIS2_PLACEMENT_3D ( 'NONE', #67470, #42662, #98397 ) ;
#68747 = CARTESIAN_POINT ( 'NONE',  ( 163.5466103691548483, 248.4877639346904630, -9.576932048953096910 ) ) ;
#68748 = CARTESIAN_POINT ( 'NONE',  ( 77.86555730066852732, 62.20866292688850052, -15.95979438352862445 ) ) ;
#68749 = CARTESIAN_POINT ( 'NONE',  ( 146.8833996772869170, 276.2374843009295660, 2.657187058495397824 ) ) ;
#68750 = CARTESIAN_POINT ( 'NONE',  ( 34.61729389309891758, 20.39040679176985549, -6.890680421881970419E-14 ) ) ;
#68751 = CARTESIAN_POINT ( 'NONE',  ( 81.68759648889933089, 55.58869686435339474, 15.96161034574013904 ) ) ;
#68752 = ORIENTED_EDGE ( 'NONE', *, *, #47659, .F. ) ;
#68753 = CARTESIAN_POINT ( 'NONE',  ( 81.97299385056439291, 58.74292844564591576, 0.1873032967079579780 ) ) ;
#68754 = ORIENTED_EDGE ( 'NONE', *, *, #69079, .T. ) ;
#68755 = DIRECTION ( 'NONE',  ( -0.000000000000000000, -0.000000000000000000, 1.000000000000000000 ) ) ;
#68756 = ORIENTED_EDGE ( 'NONE', *, *, #81856, .T. ) ;
#68757 = CARTESIAN_POINT ( 'NONE',  ( 191.5633020375963156, 267.7816122967149113, -12.23337175531920451 ) ) ;
#68758 = EDGE_CURVE ( 'NONE', #50548, #81396, #86417, .T. ) ;
#68759 = CARTESIAN_POINT ( 'NONE',  ( 192.9427994460758953, 263.5453600104565339, 4.477423407611991202 ) ) ;
#68760 = CARTESIAN_POINT ( 'NONE',  ( -3.078821053925192786, 157.4824982072974251, -4.415768667553307481E-15 ) ) ;
#68761 = ADVANCED_FACE ( 'NONE', ( #38508 ), #7116, .F. ) ;
#68762 = CARTESIAN_POINT ( 'NONE',  ( 10.06845959268932411, 31.07446838803123157, -10.00000000000000000 ) ) ;
#68764 = CARTESIAN_POINT ( 'NONE',  ( 160.6042429136753640, 281.4700839698870141, 5.616606705738245608 ) ) ;
#68763 = CARTESIAN_POINT ( 'NONE',  ( 184.2872616852876604, 288.7374155515942107, -13.26387661018510222 ) ) ;
#68765 = CARTESIAN_POINT ( 'NONE',  ( 201.1755594471486859, 282.2007051268825535, -18.15567516623250910 ) ) ;
#68766 = VERTEX_POINT ( 'NONE', #23812 ) ;
#68767 = CARTESIAN_POINT ( 'NONE',  ( 60.91453611423501258, 212.6427522451419350, 10.00000000000009415 ) ) ;
#68768 = CARTESIAN_POINT ( 'NONE',  ( 72.98844966468033135, 67.52117381499635940, 11.29058222731423555 ) ) ;
#68769 = CARTESIAN_POINT ( 'NONE',  ( 190.6570727744300200, 264.2611290600885354, -9.484224560939372495 ) ) ;
#68770 = CARTESIAN_POINT ( 'NONE',  ( 173.6418964612505533, 251.0299360267638349, -1.052939569641322626 ) ) ;
#68771 = DIRECTION ( 'NONE',  ( -0.000000000000000000, 0.000000000000000000, -1.000000000000000000 ) ) ;
#68772 = CARTESIAN_POINT ( 'NONE',  ( 71.64065041137482126, 72.08859242525181799, 3.376608021325386844 ) ) ;
#68773 = CIRCLE ( 'NONE', #52572, 6.749999999999992006 ) ;
#68774 = EDGE_CURVE ( 'NONE', #61620, #63141, #74778, .T. ) ;
#68775 = CARTESIAN_POINT ( 'NONE',  ( 84.96561085921061363, 46.52165563237655022, 10.26214194272153080 ) ) ;
#68776 = CARTESIAN_POINT ( 'NONE',  ( 59.39103342233883609, 193.5494855054051868, -2.679491924311248496 ) ) ;
#68777 = CARTESIAN_POINT ( 'NONE',  ( 191.1788773557503305, 283.4033951996527776, -16.58345142176195708 ) ) ;
#68778 = LINE ( 'NONE', #76879, #70555 ) ;
#68779 = CARTESIAN_POINT ( 'NONE',  ( 87.42789010471635436, 209.0327760586659451, 1.948934522072303157E-15 ) ) ;
#68780 = CARTESIAN_POINT ( 'NONE',  ( 206.3018347371251195, 273.3217358710584790, -9.309724106897926177 ) ) ;
#68781 = CARTESIAN_POINT ( 'NONE',  ( 193.1169444172380167, 296.1586357973259283, -13.13373377033755318 ) ) ;
#68782 = PLANE ( 'NONE',  #80251 ) ;
#68783 = ADVANCED_FACE ( 'NONE', ( #8131 ), #62300, .T. ) ;
#68784 = AXIS2_PLACEMENT_3D ( 'NONE', #15354, #91924, #23457 ) ;
#68785 = CARTESIAN_POINT ( 'NONE',  ( 207.5785076975260779, 271.1104734389944042, -6.824813054587777650 ) ) ;
#68786 = CARTESIAN_POINT ( 'NONE',  ( -20.51833308425736391, 22.81063138990083061, 10.00000000000000000 ) ) ;
#68788 = CARTESIAN_POINT ( 'NONE',  ( 76.27945191441585848, 51.11642808127202642, 16.06162126745443075 ) ) ;
#68787 = CARTESIAN_POINT ( 'NONE',  ( 73.32155222933093341, 69.66094733087366819, -9.921889652296787432 ) ) ;
#68789 = CARTESIAN_POINT ( 'NONE',  ( 33.33823495471120424, 42.18080186712595747, 3.090169943749475401 ) ) ;
#68790 = CARTESIAN_POINT ( 'NONE',  ( 204.8951067671525266, 275.7582601874789816, -12.50192486328161046 ) ) ;
#68791 = CARTESIAN_POINT ( 'NONE',  ( 157.7529601300917363, 257.4108533407307959, 16.91445305439664892 ) ) ;
#68792 = CARTESIAN_POINT ( 'NONE',  ( 72.03850700256526807, 72.31288868693221161, 3.399215934587869636 ) ) ;
#68793 =( BOUNDED_SURFACE ( )  B_SPLINE_SURFACE ( 1, 2, ( 
 ( #64290, #80029, #11607, #33910, #17696, #3511, #73400, #58177, #40960, #10096, #11114, #49094, #50574, #42466, #57673, #71905, #96227, #72920, #3986, #89162, #10597, #64799, #75274, #72418, #5859, #27295, #3022, #19708, #81524, #65286, #26791, #95744, #57172, #36744, #88152, #88651, #44343, #67652, #98583, #29166, #87164, #48599, #33388, #95239, #84385, #92480, #91482, #38733, #53920, #52443, #83390, #99071, #69636, #92970, #245, #29652, #44838, #14931, #6845, #61028, #37730, #62019, #6360, #22549, #13957, #91999, #85391, #75772, #22046, #61537, #83895, #60529, #15422, #99561, #7850, #52944, #37245, #14458, #69135, #8348, #45340, #76271, #68639, #53434, #38221, #45822, #76744, #30143, #7337, #100065, #30653, #23027, #84883, #68144, #46319, #77245, #31126, #23525, #54415, #15937, #46841, #77764, #39218, #21562, #70125, #738, #60034, #90999, #41226, #86908, #2263, #16439, #78760, #47821, #55417, #24037, #63538, #56934, #47334, #93986, #33145, #86402, #70638, #87433, #71167, #79794, #1252, #8839, #24536, #40727, #80289, #32133, #63041, #16934, #94480, #9870, #25035, #55914, #9347, #40223, #1763, #17445, #32643, #48351, #78259, #79301, #71673, #94990, #64045, #25552, #87919, #56440, #64551, #17967, #93482, #10861, #48862, #10360, #39710, #72167, #2772, #33661, #95512, #26058, #18462, #49350, #41735, #72679, #31622, #62520, #54936, #85912, #12356, #35637, #3273, #74666, #58427, #65048, #42718, #80804, #96486, #66539, #50337, #34156, #19954, #89879, #5243, #57432, #26558, #27562, #65538, #67026, #97466, #74163, #88411, #43222, #96991, #28033, #36123, #42230, #81288, #90389, #27056, #20963, #82294, #34640, #12864, #58909, #89403, #50831, #57937, #73655, #51846, #4234, #88920, #19480, #81780, #20453, #11862, #35134, #97953, #44217, #66045, #4755, #51327, #43724, #28526, #59409, #95998, #18969, #73169, #82787, #13351, #49845, #3759, #11380, #30022, #21926, #76159, #52815, #77118, #21437, #37612, #22427, #7217, #60907, #90888, #68524, #133, #37122, #91872, #68030, #36618, #83772, #7723, #75642, #67527, #6228, #38614, #99943, #52323, #14333, #45221, #6736, #15814, #99446, #53318, #84275, #69519, #69012, #30526, #91362, #38101, #83265, #29534, #46201, #44709, #45708, #75153, #14820, #13831, #61414, #54300, #23410, #76632, #92367, #61907, #22915, #92856, #53801, #98951, #98456, #84766, #85268, #15302, #31016, #5730, #29050, #59919, #60407, #40135, #87341, #57345, #18874, #80708, #87829, #72073, #86313, #71075, #71575, #41643, #72586, #86818, #11284, #16848, #63457, #32559, #55337, #18369, #40640, #17873, #10770, #64459, #1676, #47737, #94394, #3192, #33565, #95419, #78673, #48770, #34075, #24946, #55824, #42144, #32039, #17350, #48257, #79204, #9264, #79703, #9778, #73076, #2172, #26469, #95910, #33053, #64966, #88319, #49757, #63951, #94891, #10265, #49264, #25453, #56342, #41135, #2674, #62951, #25975, #56845, #24455, #80201, #93901, #58340, #19870, #50248, #28436, #50737, #34552, #81202, #97865, #5155, #88824, #12772, #58825, #59318, #5640, #42634, #81692, #90797, #12265, #21350, #44128, #35042, #75063, #51758, #36035, #66935, #43124, #74067, #52235, #4655, #36533, #98366, #59832, #83179, #13740, #44620, #3674, #65450, #26960, #57843, #19389, #11771, #73563, #64575, #63063, #24557, #40245, #49367, #3293, #80311, #71186, #55437, #25572, #17462, #71690, #48372, #72701, #47841, #33164, #86426, #2286, #96015, #78781, #32661, #72187, #94501, #63561, #26076, #40745, #18481, #25058, #55934, #86932, #10378, #18991, #79320, #64068, #95012, #56461, #41248, #87452, #17985, #2797, #33678, #95531, #56952, #87938, #10878, #41755, #34173, #65065, #26576, #57452, #88431, #49862, #80827, #11396, #1271, #32156, #21455, #4776, #74687, #19502, #51864, #97487, #12884, #27076, #89420, #58449, #66063, #19974, #35659, #81801, #82803, #13372, #5263, #51349, #36143, #42249, #44238, #28051, #3777, #12377, #50356, #35156, #67046, #50851, #73185, #58926, #28546, #75175, #96507, #65559, #66559, #4256, #5749, #89897, #97970, #20474, #57957, #82313, #67546, #97013, #43742, #27582, #34659, #43243, #36640, #42739, #88943, #73675, #98477, #59429, #81311, #74185, #90406, #20982, #83286, #29069, #59935, #90905, #52343, #11882, #69542, #30041, #77139, #21945, #68540, #85287, #83790, #84784, #54830, #60929, #91383, #7746, #93381, #62420, #76649, #61433, #645, #61924, #31529, #53340, #6753, #75664, #45727, #23933, #91893, #39117, #92874, #6247, #149, #7236, #52841, #69036, #70031, #13852, #44729, #31036, #53822, #68047, #14352, #84292, #23428, #54317, #99464, #37145, #98969, #45240, #76176, #29553, #15833, #22444, #99965, #46737, #46217, #37630, #60426, #14839, #77666, #15321, #38632, #38118, #30549, #8252, #92387, #22934, #95894, #85814, #9249, #40124, #1663, #1154, #40626, #62936, #26454, #8744, #80186, #49248, #63446, #64445, #10752, #3174, #24445, #55323, #63938, #2658, #79189, #70536, #86803, #24935, #16343, #16836, #86302, #78156, #55810, #32028, #47725, #71062, #93889, #10252, #32547, #47238, #78660, #41628, #17338, #48244, #87325, #9765, #71562, #41122, #2159, #33550, #33039, #94876, #25439, #56330, #34059, #17858, #48758, #79690, #72056, #95404, #25960, #56832, #87817, #18355, #72570, #64949, #39614, #50721, #73061, #74051, #4639, #20346, #97361, #57827, #82686, #96378, #90283, #11753, #18857, #36519, #19853, #89773, #34537, #66921, #12250, #27927, #42129, #4131, #73548, #81186, #35024, #81675, #96884, #97851, #28422, #51218, #66435, #82186, #57329, #59301, #43107, #49739, #27451, #65435, #50232, #12758, #65928, #88302, #35532, #43621, #20853, #11266, #80692, #58810, #19372, #51744, #74562, #5139, #3656, #36020, #13253, #44111, #75050, #26942, #58325, #5625, #42617, #67420, #98350, #88806, #89300, #22821, #53223, #84174, #52710, #99343, #77539, #68417, #14232, #83669, #76537, #53704, #60302, #6635, #33, #69909, #45119, #14723, #61311, #91261, #7618, #84659, #21333, #52217, #67930, #38507, #61805, #69421, #98852 ),
 ( #45605, #76054, #29923, #8130, #60796, #37510, #91757, #7115, #15203, #21824, #22321, #30919, #28940, #37999, #68913, #92273, #99837, #92754, #46099, #83163, #13728, #29428, #23308, #54196, #85163, #30422, #44605, #77013, #15707, #46609, #39004, #59816, #75539, #90783, #6125, #37021, #25842, #85684, #62811, #2027, #24325, #39492, #56203, #39997, #48635, #70419, #78033, #93767, #9646, #49127, #1028, #31906, #55200, #32424, #79060, #63319, #94259, #16718, #86184, #47612, #24813, #78539, #55690, #16221, #17210, #48117, #63819, #40505, #9127, #56717, #70936, #33423, #1541, #62299, #80063, #86679, #32912, #8625, #10127, #71438, #94754, #47114, #25317, #87201, #17733, #79569, #40993, #71936, #2541, #64321, #95280, #87699, #18232, #524, #10632, #41508, #93256, #31412, #23811, #54701, #35410, #19252, #3055, #89188, #58691, #43502, #26329, #95775, #96759, #34418, #35904, #66316, #42988, #57204, #81555, #65801, #97251, #27815, #51613, #20727, #34901, #19737, #59179, #20227, #90153, #11637, #65318, #33943, #4018, #82567, #50118, #97732, #51097, #64829, #89664, #27327, #80567, #58210, #28300, #13130, #72448, #82064, #12123, #88182, #11146, #42496, #12631, #74443, #26823, #18730, #49614, #3542, #72949, #42015, #5023, #81071, #50602, #66804, #4509, #96257, #57703, #88679, #73430, #73925, #6999, #67303, #29807, #15089, #44493, #6008, #85037, #43988, #67813, #29317, #60182, #59699, #60679, #52102, #74930, #98230, #38389, #69300, #52593, #53592, #100224, #61689, #83048, #13621, #53102, #61192, #37394, #28812, #75941, #83550, #5514, #36902, #14113, #36397, #6517, #90666, #68298, #84058, #45492, #68794, #37884, #99721, #30307, #92161, #84548, #45978, #76894, #92642, #40878, #77918, #32300, #8509, #77418, #93641, #17606, #16104, #8021, #47004, #79451, #40383, #93135, #55088, #86075, #24208, #56598, #16599, #9003, #70811, #10015, #9521, #71322, #31785, #78933, #23684, #70295, #87074, #85559, #86563, #15585, #62686, #54577, #906, #64202, #406, #39378, #47496, #38893, #1914, #78421, #1418, #94641, #47991, #39875, #31296, #63202, #25196, #17094, #32799, #69796, #94143, #48515, #24698, #55580, #25719, #46486, #63704, #56080, #71825, #62182, #2423, #33301, #95151, #10510, #83303, #52355, #66570, #67558, #13864, #6263, #26211, #57088, #97982, #5761, #82328, #72332, #89908, #97496, #87585, #18619, #88069, #79946, #28063, #2935, #50863, #74199, #33824, #13382, #12389, #18110, #64714, #36155, #20995, #74697, #95663, #12897, #44743, #81813, #5276, #43254, #49012, #58937, #90918, #4788, #35668, #20488, #75677, #44252, #51359, #28560, #59440, #90422, #29565, #51876, #82814, #75187, #37159, #36651, #98490, #29082, #59947, #21467, #68058, #98981, #30054, #31048, #1165, #76661, #37642, #23441, #39628, #8756, #22946, #7757, #47249, #8265, #78169, #99979, #53354, #21960, #92399, #70549, #38131, #85826, #39129, #52853, #15845, #53835, #68553, #15336, #16356, #60439, #91395, #46754, #160, #14368, #99478, #30563, #70043, #656, #69049, #83803, #31543, #45254, #77681, #84795, #60946, #46231, #76189, #6764, #91904, #62431, #61935, #22459, #84304, #61447, #93394, #23945, #14852, #45739, #7249, #77155, #38651, #69555, #54845, #92887, #54330, #85302, #93721, #49484, #76973, #69377, #39953, #62763, #24282, #84619, #47075, #32377, #61767, #23264, #71397, #61266, #85115, #15667, #77496, #7576, #16179, #38463, #1987, #15161, #55651, #24772, #38964, #70891, #86636, #79012, #30880, #92714, #39451, #78497, #54658, #46057, #62255, #69870, #92235, #54154, #46561, #53664, #482, #8089, #31371, #93210, #23764, #86145, #85634, #22786, #77993, #8586, #55158, #70372, #982, #31864, #17171, #16676, #47569, #9083, #1494, #63276, #94217, #48071, #9600, #40461, #96716, #57660, #10088, #72405, #3011, #41462, #73881, #33903, #26287, #88141, #27283, #26779, #88640, #49086, #96216, #40951, #87658, #3976, #2494, #3499, #32872, #80019, #33377, #19205, #63777, #94711, #95734, #80522, #19697, #81032, #50562, #64788, #25796, #25273, #57160, #56159, #64280, #17686, #18687, #10588, #49570, #11098, #34857, #56672, #41971, #87154, #72909, #58165, #48587, #18189, #34376, #65274, #50074, #11595, #42454, #73388, #65761, #89147, #13815, #60892, #120, #44697, #37110, #21911, #14319, #99431, #45206, #76145, #6719, #37598, #68509, #22414, #76618, #46187, #31004, #61893, #20950, #82773, #5718, #93345, #17826, #31496, #25407, #47202, #54285, #72027, #55289, #24905, #69999, #2125, #47694, #63412, #77632, #39584, #8714, #16309, #70504, #86269, #31997, #33007, #63908, #55781, #1635, #86772, #92844, #94846, #78629, #85255, #62906, #614, #85780, #17308, #1119, #23395, #9215, #79158, #56299, #46706, #15801, #16807, #54803, #87295, #48213, #94351, #8216, #32519, #40090, #9739, #48727, #62388, #93858, #79660, #78126, #10223, #71533, #23901, #41091, #40595, #71033, #2629, #24413, #33519, #39086, #3629, #49706, #88273, #11726, #58297, #95864, #42102, #35503, #5111, #18822, #88776, #96855, #26422, #43079, #89274, #56803, #87788, #3147, #74023, #97332, #4611, #34032, #49224, #19345, #11239, #65408, #73036, #66405, #10722, #26916, #18328, #96351, #89753, #80157, #57302, #65899, #80661, #64920, #19823, #34507, #12220, #57796, #41598, #50207, #73521, #12731, #81159, #42588, #4104, #34997, #27422, #50693, #81648, #27901, #58781, #20319, #51188, #82156, #43595, #72542, #74532, #64415, #95378, #25930, #75020, #84148, #13223, #22293, #98321, #97825, #37970, #44578, #52680, #82660, #99313, #36993, #21796, #90251, #90757, #59787, #67396, #21308, #75511, #52185, #29892, #60765, #83641, #60273, #14202, #35991, #91728, #67902, #28395, #83134, #44080, #28913, #45093, #13704, #59273, #98822, #37477, #53193, #20824, #51718, #29403, #6097, #14694, #76027, #6604, #5602, #91229, #68388, #45577, #76505, #36493, #7086, #68878, #66896, #43920, #4954, #57627, #35833, #20155, #50525, #81479, #50043, #96681, #74859, #65724, #11561, #80996, #73845, #51023, #88605, #3941, #97662, #67226 ) ),
 .UNSPECIFIED., .F., .F., .T. ) 
 B_SPLINE_SURFACE_WITH_KNOTS ( ( 2, 2 ),
 ( 3, 2, 2, 2, 2, 2, 2, 2, 2, 2, 2, 2, 2, 2, 2, 2, 2, 2, 2, 2, 2, 2, 2, 2, 2, 2, 2, 2, 2, 2, 2, 2, 2, 2, 2, 2, 2, 2, 2, 2, 2, 2, 2, 2, 2, 2, 2, 2, 2, 2, 2, 2, 2, 2, 2, 2, 2, 2, 2, 2, 2, 2, 2, 2, 2, 2, 2, 2, 2, 2, 2, 2, 2, 2, 2, 2, 2, 2, 2, 2, 2, 2, 2, 2, 2, 2, 2, 2, 2, 2, 2, 2, 2, 2, 2, 2, 2, 2, 2, 2, 2, 2, 2, 2, 2, 2, 2, 2, 2, 2, 2, 2, 2, 2, 2, 2, 2, 2, 2, 2, 2, 2, 2, 2, 2, 2, 2, 2, 2, 2, 2, 2, 2, 2, 2, 2, 2, 2, 2, 2, 2, 2, 2, 2, 2, 2, 2, 2, 2, 2, 2, 2, 2, 2, 2, 2, 2, 2, 2, 2, 2, 2, 2, 2, 2, 2, 2, 2, 2, 2, 2, 2, 2, 2, 2, 2, 2, 2, 2, 2, 2, 2, 2, 2, 2, 2, 2, 2, 2, 2, 2, 2, 2, 2, 2, 2, 2, 2, 2, 2, 2, 2, 2, 2, 2, 2, 2, 2, 2, 2, 2, 2, 2, 2, 2, 2, 2, 2, 2, 2, 2, 2, 2, 2, 2, 2, 2, 2, 2, 2, 2, 2, 2, 2, 2, 2, 2, 2, 2, 2, 2, 2, 2, 2, 2, 2, 2, 2, 2, 2, 2, 2, 2, 2, 2, 2, 2, 2, 2, 2, 2, 2, 2, 2, 2, 2, 2, 2, 2, 2, 2, 2, 2, 2, 2, 2, 2, 2, 2, 2, 2, 2, 2, 2, 2, 2, 2, 2, 2, 2, 2, 2, 2, 2, 2, 2, 2, 2, 2, 2, 2, 2, 2, 2, 2, 2, 2, 2, 2, 2, 2, 2, 2, 2, 2, 2, 2, 2, 2, 2, 2, 2, 2, 2, 2, 2, 2, 2, 2, 2, 2, 2, 2, 2, 2, 2, 2, 2, 2, 2, 2, 2, 2, 2, 2, 2, 2, 2, 2, 2, 2, 2, 2, 2, 2, 2, 2, 2, 2, 2, 2, 2, 2, 2, 2, 2, 2, 2, 2, 2, 2, 2, 3 ),
 ( 0.000000000000000000, 1.000000000000000000 ),
 ( 0.000000000000000000, 0.002688172043010752903, 0.005376344086021505805, 0.008064516129032257841, 0.01075268817204301161, 0.01344086021505376365, 0.01612903225806451568, 0.01881720430107526945, 0.02150537634408602322, 0.02419354838709677352, 0.02688172043010752729, 0.02956989247311828106, 0.03225806451612903136, 0.03494623655913978166, 0.03763440860215053890, 0.04032258064516128920, 0.04301075268817204644, 0.04569892473118279674, 0.04838709677419354704, 0.05107526881720430428, 0.05376344086021505458, 0.05645161290322580488, 0.05913978494623656212, 0.06182795698924731242, 0.06451612903225806273, 0.06720430107526881303, 0.06989247311827956333, 0.07258064516129032751, 0.07526881720430107781, 0.07795698924731182811, 0.08064516129032257841, 0.08333333333333332871, 0.08602150537634409289, 0.08870967741935484319, 0.09139784946236559349, 0.09408602150537634379, 0.09677419354838709409, 0.09946236559139784439, 0.1021505376344086086, 0.1048387096774193589, 0.1075268817204301092, 0.1102150537634408595, 0.1129032258064516098, 0.1155913978494623601, 0.1182795698924731242, 0.1209677419354838745, 0.1236559139784946248, 0.1263440860215053752, 0.1290322580645161255, 0.1317204301075268758, 0.1344086021505376261, 0.1370967741935483764, 0.1397849462365591267, 0.1424731182795699047, 0.1451612903225806550, 0.1478494623655914053, 0.1505376344086021556, 0.1532258064516129059, 0.1559139784946236562, 0.1586021505376344065, 0.1612903225806451568, 0.1639784946236559071, 0.1666666666666666574, 0.1693548387096774077, 0.1720430107526881858, 0.1747311827956989361, 0.1774193548387096864, 0.1801075268817204367, 0.1827956989247311870, 0.1854838709677419373, 0.1881720430107526876, 0.1908602150537634379, 0.1935483870967741882, 0.1962365591397849385, 0.1989247311827956888, 0.2016129032258064391, 0.2043010752688172171, 0.2069892473118279674, 0.2096774193548387177, 0.2123655913978494680, 0.2150537634408602183, 0.2177419354838709686, 0.2204301075268817189, 0.2231182795698924692, 0.2258064516129032195, 0.2284946236559139698, 0.2311827956989247201, 0.2338709677419354704, 0.2365591397849462485, 0.2392473118279569988, 0.2419354838709677491, 0.2446236559139784994, 0.2473118279569892497, 0.2500000000000000000, 0.2526881720430107503, 0.2553763440860215006, 0.2580645161290322509, 0.2607526881720430012, 0.2634408602150537515, 0.2661290322580645018, 0.2688172043010752521, 0.2715053763440860024, 0.2741935483870967527, 0.2768817204301075030, 0.2795698924731182533, 0.2822580645161290591, 0.2849462365591398094, 0.2876344086021505597, 0.2903225806451613100, 0.2930107526881720603, 0.2956989247311828106, 0.2983870967741935609, 0.3010752688172043112, 0.3037634408602150615, 0.3064516129032258118, 0.3091397849462365621, 0.3118279569892473124, 0.3145161290322580627, 0.3172043010752688130, 0.3198924731182795633, 0.3225806451612903136, 0.3252688172043010639, 0.3279569892473118142, 0.3306451612903225645, 0.3333333333333333148, 0.3360215053763440651, 0.3387096774193548154, 0.3413978494623655657, 0.3440860215053763715, 0.3467741935483871218, 0.3494623655913978721, 0.3521505376344086224, 0.3548387096774193727, 0.3575268817204301230, 0.3602150537634408733, 0.3629032258064516236, 0.3655913978494623739, 0.3682795698924731242, 0.3709677419354838745, 0.3736559139784946248, 0.3763440860215053752, 0.3790322580645161255, 0.3817204301075268758, 0.3844086021505376261, 0.3870967741935483764, 0.3897849462365591267, 0.3924731182795698770, 0.3951612903225806273, 0.3978494623655913776, 0.4005376344086021279, 0.4032258064516128782, 0.4059139784946236285, 0.4086021505376344343, 0.4112903225806451846, 0.4139784946236559349, 0.4166666666666666852, 0.4193548387096774355, 0.4220430107526881858, 0.4247311827956989361, 0.4274193548387096864, 0.4301075268817204367, 0.4327956989247311870, 0.4354838709677419373, 0.4381720430107526876, 0.4408602150537634379, 0.4435483870967741882, 0.4462365591397849385, 0.4489247311827956888, 0.4516129032258064391, 0.4543010752688171894, 0.4569892473118279397, 0.4596774193548386900, 0.4623655913978494403, 0.4650537634408601906, 0.4677419354838709409, 0.4704301075268817467, 0.4731182795698924970, 0.4758064516129032473, 0.4784946236559139976, 0.4811827956989247479, 0.4838709677419354982, 0.4865591397849462485, 0.4892473118279569988, 0.4919354838709677491, 0.4946236559139784994, 0.4973118279569892497, 0.5000000000000000000, 0.5026881720430107503, 0.5053763440860215006, 0.5080645161290322509, 0.5107526881720430012, 0.5134408602150537515, 0.5161290322580645018, 0.5188172043010752521, 0.5215053763440860024, 0.5241935483870967527, 0.5268817204301075030, 0.5295698924731182533, 0.5322580645161290036, 0.5349462365591397539, 0.5376344086021505042, 0.5403225806451612545, 0.5430107526881720048, 0.5456989247311827551, 0.5483870967741935054, 0.5510752688172042557, 0.5537634408602150060, 0.5564516129032257563, 0.5591397849462365066, 0.5618279569892472569, 0.5645161290322581182, 0.5672043010752688685, 0.5698924731182796188, 0.5725806451612903691, 0.5752688172043011194, 0.5779569892473118697, 0.5806451612903226200, 0.5833333333333333703, 0.5860215053763441206, 0.5887096774193548709, 0.5913978494623656212, 0.5940860215053763715, 0.5967741935483871218, 0.5994623655913978721, 0.6021505376344086224, 0.6048387096774193727, 0.6075268817204301230, 0.6102150537634408733, 0.6129032258064516236, 0.6155913978494623739, 0.6182795698924731242, 0.6209677419354838745, 0.6236559139784946248, 0.6263440860215053752, 0.6290322580645161255, 0.6317204301075268758, 0.6344086021505376261, 0.6370967741935483764, 0.6397849462365591267, 0.6424731182795698770, 0.6451612903225806273, 0.6478494623655913776, 0.6505376344086021279, 0.6532258064516128782, 0.6559139784946236285, 0.6586021505376343788, 0.6612903225806451291, 0.6639784946236558794, 0.6666666666666666297, 0.6693548387096773800, 0.6720430107526881303, 0.6747311827956988806, 0.6774193548387096309, 0.6801075268817203812, 0.6827956989247311315, 0.6854838709677418818, 0.6881720430107527431, 0.6908602150537634934, 0.6935483870967742437, 0.6962365591397849940, 0.6989247311827957443, 0.7016129032258064946, 0.7043010752688172449, 0.7069892473118279952, 0.7096774193548387455, 0.7123655913978494958, 0.7150537634408602461, 0.7177419354838709964, 0.7204301075268817467, 0.7231182795698924970, 0.7258064516129032473, 0.7284946236559139976, 0.7311827956989247479, 0.7338709677419354982, 0.7365591397849462485, 0.7392473118279569988, 0.7419354838709677491, 0.7446236559139784994, 0.7473118279569892497, 0.7500000000000000000, 0.7526881720430107503, 0.7553763440860215006, 0.7580645161290322509, 0.7607526881720430012, 0.7634408602150537515, 0.7661290322580645018, 0.7688172043010752521, 0.7715053763440860024, 0.7741935483870967527, 0.7768817204301075030, 0.7795698924731182533, 0.7822580645161290036, 0.7849462365591397539, 0.7876344086021505042, 0.7903225806451612545, 0.7930107526881720048, 0.7956989247311827551, 0.7983870967741935054, 0.8010752688172042557, 0.8037634408602150060, 0.8064516129032257563, 0.8091397849462365066, 0.8118279569892472569, 0.8145161290322581182, 0.8172043010752688685, 0.8198924731182796188, 0.8225806451612903691, 0.8252688172043011194, 0.8279569892473118697, 0.8306451612903226200, 0.8333333333333333703, 0.8360215053763441206, 0.8387096774193548709, 0.8413978494623656212, 0.8440860215053763715, 0.8467741935483871218, 0.8494623655913978721, 0.8521505376344086224, 0.8548387096774193727, 0.8575268817204301230, 0.8602150537634408733, 0.8629032258064516236, 0.8655913978494623739, 0.8682795698924731242, 0.8709677419354838745, 0.8736559139784946248, 0.8763440860215053752, 0.8790322580645161255, 0.8817204301075268758, 0.8844086021505376261, 0.8870967741935483764, 0.8897849462365591267, 0.8924731182795698770, 0.8951612903225806273, 0.8978494623655913776, 0.9005376344086021279, 0.9032258064516128782, 0.9059139784946236285, 0.9086021505376343788, 0.9112903225806451291, 0.9139784946236558794, 0.9166666666666666297, 0.9193548387096773800, 0.9220430107526881303, 0.9247311827956988806, 0.9274193548387096309, 0.9301075268817203812, 0.9327956989247311315, 0.9354838709677418818, 0.9381720430107527431, 0.9408602150537634934, 0.9435483870967742437, 0.9462365591397849940, 0.9489247311827957443, 0.9516129032258064946, 0.9543010752688172449, 0.9569892473118279952, 0.9596774193548387455, 0.9623655913978494958, 0.9650537634408602461, 0.9677419354838709964, 0.9704301075268817467, 0.9731182795698924970, 0.9758064516129032473, 0.9784946236559139976, 0.9811827956989247479, 0.9838709677419354982, 0.9865591397849462485, 0.9892473118279569988, 0.9919354838709677491, 0.9946236559139784994, 0.9973118279569892497, 1.000000000000000000 ),
 .UNSPECIFIED. ) 
 GEOMETRIC_REPRESENTATION_ITEM ( )  RATIONAL_B_SPLINE_SURFACE ( (
 ( 1.000000000000000000, 0.8660254037844387076, 1.000000000000000000, 0.8660254037844387076, 1.000000000000000000, 0.8660254037844387076, 1.000000000000000000, 0.8660254037844387076, 1.000000000000000000, 0.8660254037844387076, 1.000000000000000000, 0.8660254037844387076, 1.000000000000000000, 0.8660254037844387076, 1.000000000000000000, 0.8660254037844387076, 1.000000000000000000, 0.8660254037844387076, 1.000000000000000000, 0.8660254037844387076, 1.000000000000000000, 0.8660254037844387076, 1.000000000000000000, 0.8660254037844387076, 1.000000000000000000, 0.8660254037844387076, 1.000000000000000000, 0.8660254037844387076, 1.000000000000000000, 0.8660254037844387076, 1.000000000000000000, 0.8660254037844387076, 1.000000000000000000, 0.8660254037844387076, 1.000000000000000000, 0.8660254037844387076, 1.000000000000000000, 0.8660254037844387076, 1.000000000000000000, 0.8660254037844387076, 1.000000000000000000, 0.8660254037844387076, 1.000000000000000000, 0.8660254037844387076, 1.000000000000000000, 0.8660254037844387076, 1.000000000000000000, 0.8660254037844387076, 1.000000000000000000, 0.8660254037844387076, 1.000000000000000000, 0.8660254037844387076, 1.000000000000000000, 0.8660254037844387076, 1.000000000000000000, 0.8660254037844387076, 1.000000000000000000, 0.8660254037844387076, 1.000000000000000000, 0.8660254037844387076, 1.000000000000000000, 0.8660254037844387076, 1.000000000000000000, 0.8660254037844387076, 1.000000000000000000, 0.8660254037844387076, 1.000000000000000000, 0.8660254037844387076, 1.000000000000000000, 0.8660254037844387076, 1.000000000000000000, 0.8660254037844387076, 1.000000000000000000, 0.8660254037844387076, 1.000000000000000000, 0.8660254037844387076, 1.000000000000000000, 0.8660254037844387076, 1.000000000000000000, 0.8660254037844387076, 1.000000000000000000, 0.8660254037844387076, 1.000000000000000000, 0.8660254037844387076, 1.000000000000000000, 0.8660254037844387076, 1.000000000000000000, 0.8660254037844387076, 1.000000000000000000, 0.8660254037844387076, 1.000000000000000000, 0.8660254037844387076, 1.000000000000000000, 0.8660254037844387076, 1.000000000000000000, 0.8660254037844387076, 1.000000000000000000, 0.8660254037844387076, 1.000000000000000000, 0.8660254037844387076, 1.000000000000000000, 0.8660254037844387076, 1.000000000000000000, 0.8660254037844387076, 1.000000000000000000, 0.8660254037844387076, 1.000000000000000000, 0.8660254037844387076, 1.000000000000000000, 0.8660254037844387076, 1.000000000000000000, 0.8660254037844387076, 1.000000000000000000, 0.8660254037844387076, 1.000000000000000000, 0.8660254037844387076, 1.000000000000000000, 0.8660254037844387076, 1.000000000000000000, 0.8660254037844387076, 1.000000000000000000, 0.8660254037844387076, 1.000000000000000000, 0.8660254037844387076, 1.000000000000000000, 0.8660254037844387076, 1.000000000000000000, 0.8660254037844387076, 1.000000000000000000, 0.8660254037844387076, 1.000000000000000000, 0.8660254037844387076, 1.000000000000000000, 0.8660254037844387076, 1.000000000000000000, 0.8660254037844387076, 1.000000000000000000, 0.8660254037844387076, 1.000000000000000000, 0.8660254037844387076, 1.000000000000000000, 0.8660254037844387076, 1.000000000000000000, 0.8660254037844387076, 1.000000000000000000, 0.8660254037844387076, 1.000000000000000000, 0.8660254037844387076, 1.000000000000000000, 0.8660254037844387076, 1.000000000000000000, 0.8660254037844387076, 1.000000000000000000, 0.8660254037844387076, 1.000000000000000000, 0.8660254037844387076, 1.000000000000000000, 0.8660254037844387076, 1.000000000000000000, 0.8660254037844387076, 1.000000000000000000, 0.8660254037844387076, 1.000000000000000000, 0.8660254037844387076, 1.000000000000000000, 0.8660254037844387076, 1.000000000000000000, 0.8660254037844387076, 1.000000000000000000, 0.8660254037844387076, 1.000000000000000000, 0.8660254037844387076, 1.000000000000000000, 0.8660254037844387076, 1.000000000000000000, 0.8660254037844387076, 1.000000000000000000, 0.8660254037844387076, 1.000000000000000000, 0.8660254037844387076, 1.000000000000000000, 0.8660254037844387076, 1.000000000000000000, 0.8660254037844387076, 1.000000000000000000, 0.8660254037844387076, 1.000000000000000000, 0.8660254037844387076, 1.000000000000000000, 0.8660254037844387076, 1.000000000000000000, 0.8660254037844387076, 1.000000000000000000, 0.8660254037844387076, 1.000000000000000000, 0.8660254037844387076, 1.000000000000000000, 0.8660254037844387076, 1.000000000000000000, 0.8660254037844387076, 1.000000000000000000, 0.8660254037844387076, 1.000000000000000000, 0.8660254037844387076, 1.000000000000000000, 0.8660254037844387076, 1.000000000000000000, 0.8660254037844387076, 1.000000000000000000, 0.8660254037844387076, 1.000000000000000000, 0.8660254037844387076, 1.000000000000000000, 0.8660254037844387076, 1.000000000000000000, 0.8660254037844387076, 1.000000000000000000, 0.8660254037844387076, 1.000000000000000000, 0.8660254037844387076, 1.000000000000000000, 0.8660254037844387076, 1.000000000000000000, 0.8660254037844387076, 1.000000000000000000, 0.8660254037844387076, 1.000000000000000000, 0.8660254037844387076, 1.000000000000000000, 0.8660254037844387076, 1.000000000000000000, 0.8660254037844387076, 1.000000000000000000, 0.8660254037844387076, 1.000000000000000000, 0.8660254037844387076, 1.000000000000000000, 0.8660254037844387076, 1.000000000000000000, 0.8660254037844387076, 1.000000000000000000, 0.8660254037844387076, 1.000000000000000000, 0.8660254037844387076, 1.000000000000000000, 0.8660254037844387076, 1.000000000000000000, 0.8660254037844387076, 1.000000000000000000, 0.8660254037844387076, 1.000000000000000000, 0.8660254037844387076, 1.000000000000000000, 0.8660254037844387076, 1.000000000000000000, 0.8660254037844387076, 1.000000000000000000, 0.8660254037844387076, 1.000000000000000000, 0.8660254037844387076, 1.000000000000000000, 0.8660254037844387076, 1.000000000000000000, 0.8660254037844387076, 1.000000000000000000, 0.8660254037844387076, 1.000000000000000000, 0.8660254037844387076, 1.000000000000000000, 0.8660254037844387076, 1.000000000000000000, 0.8660254037844387076, 1.000000000000000000, 0.8660254037844387076, 1.000000000000000000, 0.8660254037844387076, 1.000000000000000000, 0.8660254037844387076, 1.000000000000000000, 0.8660254037844387076, 1.000000000000000000, 0.8660254037844387076, 1.000000000000000000, 0.8660254037844387076, 1.000000000000000000, 0.8660254037844387076, 1.000000000000000000, 0.8660254037844387076, 1.000000000000000000, 0.8660254037844387076, 1.000000000000000000, 0.8660254037844387076, 1.000000000000000000, 0.8660254037844387076, 1.000000000000000000, 0.8660254037844387076, 1.000000000000000000, 0.8660254037844387076, 1.000000000000000000, 0.8660254037844387076, 1.000000000000000000, 0.8660254037844387076, 1.000000000000000000, 0.8660254037844387076, 1.000000000000000000, 0.8660254037844387076, 1.000000000000000000, 0.8660254037844387076, 1.000000000000000000, 0.8660254037844387076, 1.000000000000000000, 0.8660254037844387076, 1.000000000000000000, 0.8660254037844387076, 1.000000000000000000, 0.8660254037844387076, 1.000000000000000000, 0.8660254037844387076, 1.000000000000000000, 0.8660254037844387076, 1.000000000000000000, 0.8660254037844387076, 1.000000000000000000, 0.8660254037844387076, 1.000000000000000000, 0.8660254037844387076, 1.000000000000000000, 0.8660254037844387076, 1.000000000000000000, 0.8660254037844387076, 1.000000000000000000, 0.8660254037844387076, 1.000000000000000000, 0.8660254037844387076, 1.000000000000000000, 0.8660254037844387076, 1.000000000000000000, 0.8660254037844387076, 1.000000000000000000, 0.8660254037844387076, 1.000000000000000000, 0.8660254037844387076, 1.000000000000000000, 0.8660254037844387076, 1.000000000000000000, 0.8660254037844387076, 1.000000000000000000, 0.8660254037844387076, 1.000000000000000000, 0.8660254037844387076, 1.000000000000000000, 0.8660254037844387076, 1.000000000000000000, 0.8660254037844387076, 1.000000000000000000, 0.8660254037844387076, 1.000000000000000000, 0.8660254037844387076, 1.000000000000000000, 0.8660254037844387076, 1.000000000000000000, 0.8660254037844387076, 1.000000000000000000, 0.8660254037844387076, 1.000000000000000000, 0.8660254037844387076, 1.000000000000000000, 0.8660254037844387076, 1.000000000000000000, 0.8660254037844387076, 1.000000000000000000, 0.8660254037844387076, 1.000000000000000000, 0.8660254037844387076, 1.000000000000000000, 0.8660254037844387076, 1.000000000000000000, 0.8660254037844387076, 1.000000000000000000, 0.8660254037844387076, 1.000000000000000000, 0.8660254037844387076, 1.000000000000000000, 0.8660254037844387076, 1.000000000000000000, 0.8660254037844387076, 1.000000000000000000, 0.8660254037844387076, 1.000000000000000000, 0.8660254037844387076, 1.000000000000000000, 0.8660254037844387076, 1.000000000000000000, 0.8660254037844387076, 1.000000000000000000, 0.8660254037844387076, 1.000000000000000000, 0.8660254037844387076, 1.000000000000000000, 0.8660254037844387076, 1.000000000000000000, 0.8660254037844387076, 1.000000000000000000, 0.8660254037844387076, 1.000000000000000000, 0.8660254037844387076, 1.000000000000000000, 0.8660254037844387076, 1.000000000000000000, 0.8660254037844387076, 1.000000000000000000, 0.8660254037844387076, 1.000000000000000000, 0.8660254037844387076, 1.000000000000000000, 0.8660254037844387076, 1.000000000000000000, 0.8660254037844387076, 1.000000000000000000, 0.8660254037844387076, 1.000000000000000000, 0.8660254037844387076, 1.000000000000000000, 0.8660254037844387076, 1.000000000000000000, 0.8660254037844387076, 1.000000000000000000, 0.8660254037844387076, 1.000000000000000000, 0.8660254037844387076, 1.000000000000000000, 0.8660254037844387076, 1.000000000000000000, 0.8660254037844387076, 1.000000000000000000, 0.8660254037844387076, 1.000000000000000000, 0.8660254037844387076, 1.000000000000000000, 0.8660254037844387076, 1.000000000000000000, 0.8660254037844387076, 1.000000000000000000, 0.8660254037844387076, 1.000000000000000000, 0.8660254037844387076, 1.000000000000000000, 0.8660254037844387076, 1.000000000000000000, 0.8660254037844387076, 1.000000000000000000, 0.8660254037844387076, 1.000000000000000000, 0.8660254037844387076, 1.000000000000000000, 0.8660254037844387076, 1.000000000000000000, 0.8660254037844387076, 1.000000000000000000, 0.8660254037844387076, 1.000000000000000000, 0.8660254037844387076, 1.000000000000000000, 0.8660254037844387076, 1.000000000000000000, 0.8660254037844387076, 1.000000000000000000, 0.8660254037844387076, 1.000000000000000000, 0.8660254037844387076, 1.000000000000000000, 0.8660254037844387076, 1.000000000000000000, 0.8660254037844387076, 1.000000000000000000, 0.8660254037844387076, 1.000000000000000000, 0.8660254037844387076, 1.000000000000000000, 0.8660254037844387076, 1.000000000000000000, 0.8660254037844387076, 1.000000000000000000, 0.8660254037844387076, 1.000000000000000000, 0.8660254037844387076, 1.000000000000000000, 0.8660254037844387076, 1.000000000000000000, 0.8660254037844387076, 1.000000000000000000, 0.8660254037844387076, 1.000000000000000000, 0.8660254037844387076, 1.000000000000000000, 0.8660254037844387076, 1.000000000000000000, 0.8660254037844387076, 1.000000000000000000, 0.8660254037844387076, 1.000000000000000000, 0.8660254037844387076, 1.000000000000000000, 0.8660254037844387076, 1.000000000000000000, 0.8660254037844387076, 1.000000000000000000, 0.8660254037844387076, 1.000000000000000000, 0.8660254037844387076, 1.000000000000000000, 0.8660254037844387076, 1.000000000000000000, 0.8660254037844387076, 1.000000000000000000, 0.8660254037844387076, 1.000000000000000000, 0.8660254037844387076, 1.000000000000000000, 0.8660254037844387076, 1.000000000000000000, 0.8660254037844387076, 1.000000000000000000, 0.8660254037844387076, 1.000000000000000000, 0.8660254037844387076, 1.000000000000000000, 0.8660254037844387076, 1.000000000000000000, 0.8660254037844387076, 1.000000000000000000, 0.8660254037844387076, 1.000000000000000000, 0.8660254037844387076, 1.000000000000000000, 0.8660254037844387076, 1.000000000000000000, 0.8660254037844387076, 1.000000000000000000, 0.8660254037844387076, 1.000000000000000000, 0.8660254037844387076, 1.000000000000000000, 0.8660254037844387076, 1.000000000000000000, 0.8660254037844387076, 1.000000000000000000, 0.8660254037844387076, 1.000000000000000000, 0.8660254037844387076, 1.000000000000000000, 0.8660254037844387076, 1.000000000000000000, 0.8660254037844387076, 1.000000000000000000, 0.8660254037844387076, 1.000000000000000000, 0.8660254037844387076, 1.000000000000000000, 0.8660254037844387076, 1.000000000000000000, 0.8660254037844387076, 1.000000000000000000, 0.8660254037844387076, 1.000000000000000000, 0.8660254037844387076, 1.000000000000000000, 0.8660254037844387076, 1.000000000000000000, 0.8660254037844387076, 1.000000000000000000, 0.8660254037844387076, 1.000000000000000000, 0.8660254037844387076, 1.000000000000000000, 0.8660254037844387076, 1.000000000000000000, 0.8660254037844387076, 1.000000000000000000, 0.8660254037844387076, 1.000000000000000000, 0.8660254037844387076, 1.000000000000000000, 0.8660254037844387076, 1.000000000000000000, 0.8660254037844387076, 1.000000000000000000, 0.8660254037844387076, 1.000000000000000000, 0.8660254037844387076, 1.000000000000000000, 0.8660254037844387076, 1.000000000000000000, 0.8660254037844387076, 1.000000000000000000, 0.8660254037844387076, 1.000000000000000000, 0.8660254037844387076, 1.000000000000000000, 0.8660254037844387076, 1.000000000000000000, 0.8660254037844387076, 1.000000000000000000, 0.8660254037844387076, 1.000000000000000000, 0.8660254037844387076, 1.000000000000000000, 0.8660254037844387076, 1.000000000000000000, 0.8660254037844387076, 1.000000000000000000, 0.8660254037844387076, 1.000000000000000000, 0.8660254037844387076, 1.000000000000000000, 0.8660254037844387076, 1.000000000000000000, 0.8660254037844387076, 1.000000000000000000, 0.8660254037844387076, 1.000000000000000000, 0.8660254037844387076, 1.000000000000000000, 0.8660254037844387076, 1.000000000000000000, 0.8660254037844387076, 1.000000000000000000, 0.8660254037844387076, 1.000000000000000000, 0.8660254037844387076, 1.000000000000000000, 0.8660254037844387076, 1.000000000000000000, 0.8660254037844387076, 1.000000000000000000, 0.8660254037844387076, 1.000000000000000000, 0.8660254037844387076, 1.000000000000000000, 0.8660254037844387076, 1.000000000000000000, 0.8660254037844387076, 1.000000000000000000, 0.8660254037844387076, 1.000000000000000000, 0.8660254037844387076, 1.000000000000000000, 0.8660254037844387076, 1.000000000000000000, 0.8660254037844387076, 1.000000000000000000, 0.8660254037844387076, 1.000000000000000000, 0.8660254037844387076, 1.000000000000000000, 0.8660254037844387076, 1.000000000000000000, 0.8660254037844387076, 1.000000000000000000, 0.8660254037844387076, 1.000000000000000000, 0.8660254037844387076, 1.000000000000000000, 0.8660254037844387076, 1.000000000000000000, 0.8660254037844387076, 1.000000000000000000, 0.8660254037844387076, 1.000000000000000000, 0.8660254037844387076, 1.000000000000000000, 0.8660254037844387076, 1.000000000000000000, 0.8660254037844387076, 1.000000000000000000, 0.8660254037844387076, 1.000000000000000000, 0.8660254037844387076, 1.000000000000000000, 0.8660254037844387076, 1.000000000000000000, 0.8660254037844387076, 1.000000000000000000, 0.8660254037844387076, 1.000000000000000000, 0.8660254037844387076, 1.000000000000000000, 0.8660254037844387076, 1.000000000000000000, 0.8660254037844387076, 1.000000000000000000, 0.8660254037844387076, 1.000000000000000000, 0.8660254037844387076, 1.000000000000000000, 0.8660254037844387076, 1.000000000000000000, 0.8660254037844387076, 1.000000000000000000, 0.8660254037844387076, 1.000000000000000000, 0.8660254037844387076, 1.000000000000000000, 0.8660254037844387076, 1.000000000000000000, 0.8660254037844387076, 1.000000000000000000, 0.8660254037844387076, 1.000000000000000000, 0.8660254037844387076, 1.000000000000000000, 0.8660254037844387076, 1.000000000000000000, 0.8660254037844387076, 1.000000000000000000, 0.8660254037844387076, 1.000000000000000000, 0.8660254037844387076, 1.000000000000000000, 0.8660254037844387076, 1.000000000000000000, 0.8660254037844387076, 1.000000000000000000, 0.8660254037844387076, 1.000000000000000000, 0.8660254037844387076, 1.000000000000000000, 0.8660254037844387076, 1.000000000000000000, 0.8660254037844387076, 1.000000000000000000, 0.8660254037844387076, 1.000000000000000000, 0.8660254037844387076, 1.000000000000000000, 0.8660254037844387076, 1.000000000000000000, 0.8660254037844387076, 1.000000000000000000, 0.8660254037844387076, 1.000000000000000000, 0.8660254037844387076, 1.000000000000000000, 0.8660254037844387076, 1.000000000000000000),
 ( 1.000000000000000000, 0.8660254037844387076, 1.000000000000000000, 0.8660254037844387076, 1.000000000000000000, 0.8660254037844387076, 1.000000000000000000, 0.8660254037844387076, 1.000000000000000000, 0.8660254037844387076, 1.000000000000000000, 0.8660254037844387076, 1.000000000000000000, 0.8660254037844387076, 1.000000000000000000, 0.8660254037844387076, 1.000000000000000000, 0.8660254037844387076, 1.000000000000000000, 0.8660254037844387076, 1.000000000000000000, 0.8660254037844387076, 1.000000000000000000, 0.8660254037844387076, 1.000000000000000000, 0.8660254037844387076, 1.000000000000000000, 0.8660254037844387076, 1.000000000000000000, 0.8660254037844387076, 1.000000000000000000, 0.8660254037844387076, 1.000000000000000000, 0.8660254037844387076, 1.000000000000000000, 0.8660254037844387076, 1.000000000000000000, 0.8660254037844387076, 1.000000000000000000, 0.8660254037844387076, 1.000000000000000000, 0.8660254037844387076, 1.000000000000000000, 0.8660254037844387076, 1.000000000000000000, 0.8660254037844387076, 1.000000000000000000, 0.8660254037844387076, 1.000000000000000000, 0.8660254037844387076, 1.000000000000000000, 0.8660254037844387076, 1.000000000000000000, 0.8660254037844387076, 1.000000000000000000, 0.8660254037844387076, 1.000000000000000000, 0.8660254037844387076, 1.000000000000000000, 0.8660254037844387076, 1.000000000000000000, 0.8660254037844387076, 1.000000000000000000, 0.8660254037844387076, 1.000000000000000000, 0.8660254037844387076, 1.000000000000000000, 0.8660254037844387076, 1.000000000000000000, 0.8660254037844387076, 1.000000000000000000, 0.8660254037844387076, 1.000000000000000000, 0.8660254037844387076, 1.000000000000000000, 0.8660254037844387076, 1.000000000000000000, 0.8660254037844387076, 1.000000000000000000, 0.8660254037844387076, 1.000000000000000000, 0.8660254037844387076, 1.000000000000000000, 0.8660254037844387076, 1.000000000000000000, 0.8660254037844387076, 1.000000000000000000, 0.8660254037844387076, 1.000000000000000000, 0.8660254037844387076, 1.000000000000000000, 0.8660254037844387076, 1.000000000000000000, 0.8660254037844387076, 1.000000000000000000, 0.8660254037844387076, 1.000000000000000000, 0.8660254037844387076, 1.000000000000000000, 0.8660254037844387076, 1.000000000000000000, 0.8660254037844387076, 1.000000000000000000, 0.8660254037844387076, 1.000000000000000000, 0.8660254037844387076, 1.000000000000000000, 0.8660254037844387076, 1.000000000000000000, 0.8660254037844387076, 1.000000000000000000, 0.8660254037844387076, 1.000000000000000000, 0.8660254037844387076, 1.000000000000000000, 0.8660254037844387076, 1.000000000000000000, 0.8660254037844387076, 1.000000000000000000, 0.8660254037844387076, 1.000000000000000000, 0.8660254037844387076, 1.000000000000000000, 0.8660254037844387076, 1.000000000000000000, 0.8660254037844387076, 1.000000000000000000, 0.8660254037844387076, 1.000000000000000000, 0.8660254037844387076, 1.000000000000000000, 0.8660254037844387076, 1.000000000000000000, 0.8660254037844387076, 1.000000000000000000, 0.8660254037844387076, 1.000000000000000000, 0.8660254037844387076, 1.000000000000000000, 0.8660254037844387076, 1.000000000000000000, 0.8660254037844387076, 1.000000000000000000, 0.8660254037844387076, 1.000000000000000000, 0.8660254037844387076, 1.000000000000000000, 0.8660254037844387076, 1.000000000000000000, 0.8660254037844387076, 1.000000000000000000, 0.8660254037844387076, 1.000000000000000000, 0.8660254037844387076, 1.000000000000000000, 0.8660254037844387076, 1.000000000000000000, 0.8660254037844387076, 1.000000000000000000, 0.8660254037844387076, 1.000000000000000000, 0.8660254037844387076, 1.000000000000000000, 0.8660254037844387076, 1.000000000000000000, 0.8660254037844387076, 1.000000000000000000, 0.8660254037844387076, 1.000000000000000000, 0.8660254037844387076, 1.000000000000000000, 0.8660254037844387076, 1.000000000000000000, 0.8660254037844387076, 1.000000000000000000, 0.8660254037844387076, 1.000000000000000000, 0.8660254037844387076, 1.000000000000000000, 0.8660254037844387076, 1.000000000000000000, 0.8660254037844387076, 1.000000000000000000, 0.8660254037844387076, 1.000000000000000000, 0.8660254037844387076, 1.000000000000000000, 0.8660254037844387076, 1.000000000000000000, 0.8660254037844387076, 1.000000000000000000, 0.8660254037844387076, 1.000000000000000000, 0.8660254037844387076, 1.000000000000000000, 0.8660254037844387076, 1.000000000000000000, 0.8660254037844387076, 1.000000000000000000, 0.8660254037844387076, 1.000000000000000000, 0.8660254037844387076, 1.000000000000000000, 0.8660254037844387076, 1.000000000000000000, 0.8660254037844387076, 1.000000000000000000, 0.8660254037844387076, 1.000000000000000000, 0.8660254037844387076, 1.000000000000000000, 0.8660254037844387076, 1.000000000000000000, 0.8660254037844387076, 1.000000000000000000, 0.8660254037844387076, 1.000000000000000000, 0.8660254037844387076, 1.000000000000000000, 0.8660254037844387076, 1.000000000000000000, 0.8660254037844387076, 1.000000000000000000, 0.8660254037844387076, 1.000000000000000000, 0.8660254037844387076, 1.000000000000000000, 0.8660254037844387076, 1.000000000000000000, 0.8660254037844387076, 1.000000000000000000, 0.8660254037844387076, 1.000000000000000000, 0.8660254037844387076, 1.000000000000000000, 0.8660254037844387076, 1.000000000000000000, 0.8660254037844387076, 1.000000000000000000, 0.8660254037844387076, 1.000000000000000000, 0.8660254037844387076, 1.000000000000000000, 0.8660254037844387076, 1.000000000000000000, 0.8660254037844387076, 1.000000000000000000, 0.8660254037844387076, 1.000000000000000000, 0.8660254037844387076, 1.000000000000000000, 0.8660254037844387076, 1.000000000000000000, 0.8660254037844387076, 1.000000000000000000, 0.8660254037844387076, 1.000000000000000000, 0.8660254037844387076, 1.000000000000000000, 0.8660254037844387076, 1.000000000000000000, 0.8660254037844387076, 1.000000000000000000, 0.8660254037844387076, 1.000000000000000000, 0.8660254037844387076, 1.000000000000000000, 0.8660254037844387076, 1.000000000000000000, 0.8660254037844387076, 1.000000000000000000, 0.8660254037844387076, 1.000000000000000000, 0.8660254037844387076, 1.000000000000000000, 0.8660254037844387076, 1.000000000000000000, 0.8660254037844387076, 1.000000000000000000, 0.8660254037844387076, 1.000000000000000000, 0.8660254037844387076, 1.000000000000000000, 0.8660254037844387076, 1.000000000000000000, 0.8660254037844387076, 1.000000000000000000, 0.8660254037844387076, 1.000000000000000000, 0.8660254037844387076, 1.000000000000000000, 0.8660254037844387076, 1.000000000000000000, 0.8660254037844387076, 1.000000000000000000, 0.8660254037844387076, 1.000000000000000000, 0.8660254037844387076, 1.000000000000000000, 0.8660254037844387076, 1.000000000000000000, 0.8660254037844387076, 1.000000000000000000, 0.8660254037844387076, 1.000000000000000000, 0.8660254037844387076, 1.000000000000000000, 0.8660254037844387076, 1.000000000000000000, 0.8660254037844387076, 1.000000000000000000, 0.8660254037844387076, 1.000000000000000000, 0.8660254037844387076, 1.000000000000000000, 0.8660254037844387076, 1.000000000000000000, 0.8660254037844387076, 1.000000000000000000, 0.8660254037844387076, 1.000000000000000000, 0.8660254037844387076, 1.000000000000000000, 0.8660254037844387076, 1.000000000000000000, 0.8660254037844387076, 1.000000000000000000, 0.8660254037844387076, 1.000000000000000000, 0.8660254037844387076, 1.000000000000000000, 0.8660254037844387076, 1.000000000000000000, 0.8660254037844387076, 1.000000000000000000, 0.8660254037844387076, 1.000000000000000000, 0.8660254037844387076, 1.000000000000000000, 0.8660254037844387076, 1.000000000000000000, 0.8660254037844387076, 1.000000000000000000, 0.8660254037844387076, 1.000000000000000000, 0.8660254037844387076, 1.000000000000000000, 0.8660254037844387076, 1.000000000000000000, 0.8660254037844387076, 1.000000000000000000, 0.8660254037844387076, 1.000000000000000000, 0.8660254037844387076, 1.000000000000000000, 0.8660254037844387076, 1.000000000000000000, 0.8660254037844387076, 1.000000000000000000, 0.8660254037844387076, 1.000000000000000000, 0.8660254037844387076, 1.000000000000000000, 0.8660254037844387076, 1.000000000000000000, 0.8660254037844387076, 1.000000000000000000, 0.8660254037844387076, 1.000000000000000000, 0.8660254037844387076, 1.000000000000000000, 0.8660254037844387076, 1.000000000000000000, 0.8660254037844387076, 1.000000000000000000, 0.8660254037844387076, 1.000000000000000000, 0.8660254037844387076, 1.000000000000000000, 0.8660254037844387076, 1.000000000000000000, 0.8660254037844387076, 1.000000000000000000, 0.8660254037844387076, 1.000000000000000000, 0.8660254037844387076, 1.000000000000000000, 0.8660254037844387076, 1.000000000000000000, 0.8660254037844387076, 1.000000000000000000, 0.8660254037844387076, 1.000000000000000000, 0.8660254037844387076, 1.000000000000000000, 0.8660254037844387076, 1.000000000000000000, 0.8660254037844387076, 1.000000000000000000, 0.8660254037844387076, 1.000000000000000000, 0.8660254037844387076, 1.000000000000000000, 0.8660254037844387076, 1.000000000000000000, 0.8660254037844387076, 1.000000000000000000, 0.8660254037844387076, 1.000000000000000000, 0.8660254037844387076, 1.000000000000000000, 0.8660254037844387076, 1.000000000000000000, 0.8660254037844387076, 1.000000000000000000, 0.8660254037844387076, 1.000000000000000000, 0.8660254037844387076, 1.000000000000000000, 0.8660254037844387076, 1.000000000000000000, 0.8660254037844387076, 1.000000000000000000, 0.8660254037844387076, 1.000000000000000000, 0.8660254037844387076, 1.000000000000000000, 0.8660254037844387076, 1.000000000000000000, 0.8660254037844387076, 1.000000000000000000, 0.8660254037844387076, 1.000000000000000000, 0.8660254037844387076, 1.000000000000000000, 0.8660254037844387076, 1.000000000000000000, 0.8660254037844387076, 1.000000000000000000, 0.8660254037844387076, 1.000000000000000000, 0.8660254037844387076, 1.000000000000000000, 0.8660254037844387076, 1.000000000000000000, 0.8660254037844387076, 1.000000000000000000, 0.8660254037844387076, 1.000000000000000000, 0.8660254037844387076, 1.000000000000000000, 0.8660254037844387076, 1.000000000000000000, 0.8660254037844387076, 1.000000000000000000, 0.8660254037844387076, 1.000000000000000000, 0.8660254037844387076, 1.000000000000000000, 0.8660254037844387076, 1.000000000000000000, 0.8660254037844387076, 1.000000000000000000, 0.8660254037844387076, 1.000000000000000000, 0.8660254037844387076, 1.000000000000000000, 0.8660254037844387076, 1.000000000000000000, 0.8660254037844387076, 1.000000000000000000, 0.8660254037844387076, 1.000000000000000000, 0.8660254037844387076, 1.000000000000000000, 0.8660254037844387076, 1.000000000000000000, 0.8660254037844387076, 1.000000000000000000, 0.8660254037844387076, 1.000000000000000000, 0.8660254037844387076, 1.000000000000000000, 0.8660254037844387076, 1.000000000000000000, 0.8660254037844387076, 1.000000000000000000, 0.8660254037844387076, 1.000000000000000000, 0.8660254037844387076, 1.000000000000000000, 0.8660254037844387076, 1.000000000000000000, 0.8660254037844387076, 1.000000000000000000, 0.8660254037844387076, 1.000000000000000000, 0.8660254037844387076, 1.000000000000000000, 0.8660254037844387076, 1.000000000000000000, 0.8660254037844387076, 1.000000000000000000, 0.8660254037844387076, 1.000000000000000000, 0.8660254037844387076, 1.000000000000000000, 0.8660254037844387076, 1.000000000000000000, 0.8660254037844387076, 1.000000000000000000, 0.8660254037844387076, 1.000000000000000000, 0.8660254037844387076, 1.000000000000000000, 0.8660254037844387076, 1.000000000000000000, 0.8660254037844387076, 1.000000000000000000, 0.8660254037844387076, 1.000000000000000000, 0.8660254037844387076, 1.000000000000000000, 0.8660254037844387076, 1.000000000000000000, 0.8660254037844387076, 1.000000000000000000, 0.8660254037844387076, 1.000000000000000000, 0.8660254037844387076, 1.000000000000000000, 0.8660254037844387076, 1.000000000000000000, 0.8660254037844387076, 1.000000000000000000, 0.8660254037844387076, 1.000000000000000000, 0.8660254037844387076, 1.000000000000000000, 0.8660254037844387076, 1.000000000000000000, 0.8660254037844387076, 1.000000000000000000, 0.8660254037844387076, 1.000000000000000000, 0.8660254037844387076, 1.000000000000000000, 0.8660254037844387076, 1.000000000000000000, 0.8660254037844387076, 1.000000000000000000, 0.8660254037844387076, 1.000000000000000000, 0.8660254037844387076, 1.000000000000000000, 0.8660254037844387076, 1.000000000000000000, 0.8660254037844387076, 1.000000000000000000, 0.8660254037844387076, 1.000000000000000000, 0.8660254037844387076, 1.000000000000000000, 0.8660254037844387076, 1.000000000000000000, 0.8660254037844387076, 1.000000000000000000, 0.8660254037844387076, 1.000000000000000000, 0.8660254037844387076, 1.000000000000000000, 0.8660254037844387076, 1.000000000000000000, 0.8660254037844387076, 1.000000000000000000, 0.8660254037844387076, 1.000000000000000000, 0.8660254037844387076, 1.000000000000000000, 0.8660254037844387076, 1.000000000000000000, 0.8660254037844387076, 1.000000000000000000, 0.8660254037844387076, 1.000000000000000000, 0.8660254037844387076, 1.000000000000000000, 0.8660254037844387076, 1.000000000000000000, 0.8660254037844387076, 1.000000000000000000, 0.8660254037844387076, 1.000000000000000000, 0.8660254037844387076, 1.000000000000000000, 0.8660254037844387076, 1.000000000000000000, 0.8660254037844387076, 1.000000000000000000, 0.8660254037844387076, 1.000000000000000000, 0.8660254037844387076, 1.000000000000000000, 0.8660254037844387076, 1.000000000000000000, 0.8660254037844387076, 1.000000000000000000, 0.8660254037844387076, 1.000000000000000000, 0.8660254037844387076, 1.000000000000000000, 0.8660254037844387076, 1.000000000000000000, 0.8660254037844387076, 1.000000000000000000, 0.8660254037844387076, 1.000000000000000000, 0.8660254037844387076, 1.000000000000000000, 0.8660254037844387076, 1.000000000000000000, 0.8660254037844387076, 1.000000000000000000, 0.8660254037844387076, 1.000000000000000000, 0.8660254037844387076, 1.000000000000000000, 0.8660254037844387076, 1.000000000000000000, 0.8660254037844387076, 1.000000000000000000, 0.8660254037844387076, 1.000000000000000000, 0.8660254037844387076, 1.000000000000000000, 0.8660254037844387076, 1.000000000000000000, 0.8660254037844387076, 1.000000000000000000, 0.8660254037844387076, 1.000000000000000000, 0.8660254037844387076, 1.000000000000000000, 0.8660254037844387076, 1.000000000000000000, 0.8660254037844387076, 1.000000000000000000, 0.8660254037844387076, 1.000000000000000000, 0.8660254037844387076, 1.000000000000000000, 0.8660254037844387076, 1.000000000000000000, 0.8660254037844387076, 1.000000000000000000, 0.8660254037844387076, 1.000000000000000000, 0.8660254037844387076, 1.000000000000000000, 0.8660254037844387076, 1.000000000000000000, 0.8660254037844387076, 1.000000000000000000, 0.8660254037844387076, 1.000000000000000000, 0.8660254037844387076, 1.000000000000000000, 0.8660254037844387076, 1.000000000000000000, 0.8660254037844387076, 1.000000000000000000, 0.8660254037844387076, 1.000000000000000000, 0.8660254037844387076, 1.000000000000000000, 0.8660254037844387076, 1.000000000000000000, 0.8660254037844387076, 1.000000000000000000, 0.8660254037844387076, 1.000000000000000000, 0.8660254037844387076, 1.000000000000000000, 0.8660254037844387076, 1.000000000000000000, 0.8660254037844387076, 1.000000000000000000, 0.8660254037844387076, 1.000000000000000000, 0.8660254037844387076, 1.000000000000000000, 0.8660254037844387076, 1.000000000000000000, 0.8660254037844387076, 1.000000000000000000, 0.8660254037844387076, 1.000000000000000000, 0.8660254037844387076, 1.000000000000000000, 0.8660254037844387076, 1.000000000000000000, 0.8660254037844387076, 1.000000000000000000, 0.8660254037844387076, 1.000000000000000000, 0.8660254037844387076, 1.000000000000000000, 0.8660254037844387076, 1.000000000000000000, 0.8660254037844387076, 1.000000000000000000, 0.8660254037844387076, 1.000000000000000000, 0.8660254037844387076, 1.000000000000000000, 0.8660254037844387076, 1.000000000000000000, 0.8660254037844387076, 1.000000000000000000, 0.8660254037844387076, 1.000000000000000000, 0.8660254037844387076, 1.000000000000000000, 0.8660254037844387076, 1.000000000000000000, 0.8660254037844387076, 1.000000000000000000, 0.8660254037844387076, 1.000000000000000000, 0.8660254037844387076, 1.000000000000000000, 0.8660254037844387076, 1.000000000000000000, 0.8660254037844387076, 1.000000000000000000, 0.8660254037844387076, 1.000000000000000000, 0.8660254037844387076, 1.000000000000000000, 0.8660254037844387076, 1.000000000000000000, 0.8660254037844387076, 1.000000000000000000, 0.8660254037844387076, 1.000000000000000000) ) ) 
 REPRESENTATION_ITEM ( '' )  SURFACE ( )  );
#68794 = CARTESIAN_POINT ( 'NONE',  ( 33.57176175898906934, 184.0643266524159856, -9.188101187500093303 ) ) ;
#68795 = CARTESIAN_POINT ( 'NONE',  ( 58.06412948370898164, 195.1423013555410080, -4.594050593750043987 ) ) ;
#68796 = CARTESIAN_POINT ( 'NONE',  ( 196.0355168007595523, 291.1035201434990540, 17.55377893960077884 ) ) ;
#68797 = CARTESIAN_POINT ( 'NONE',  ( 81.29157559341378203, 42.21858700188892044, -7.212111827135544218 ) ) ;
#68798 = CARTESIAN_POINT ( 'NONE',  ( 79.13486416932684619, 50.85352373906047063, -15.04773823355513507 ) ) ;
#68799 = CARTESIAN_POINT ( 'NONE',  ( -12.96825614257699755, 169.9865022471903160, 10.00000000000009237 ) ) ;
#68800 = CARTESIAN_POINT ( 'NONE',  ( 51.75794814269726629, 206.8149278399160949, -9.188101187500095079 ) ) ;
#68801 = AXIS2_PLACEMENT_3D ( 'NONE', #86904, #46316, #63038 ) ;
#68802 = CARTESIAN_POINT ( 'NONE',  ( 22.99159801516092472, 18.98920272979926693, 7.433330006724137462 ) ) ;
#68803 = CARTESIAN_POINT ( 'NONE',  ( -19.65312891409030271, 93.06504152958497400, 59.99999999999999289 ) ) ;
#68804 = CARTESIAN_POINT ( 'NONE',  ( 17.35761498915574563, 12.94754757982088300, 5.678558825948272215 ) ) ;
#68805 = FACE_OUTER_BOUND ( 'NONE', #9056, .T. ) ;
#68806 = CARTESIAN_POINT ( 'NONE',  ( 76.75696856028530135, 63.87261700412425114, 14.87451922956917016 ) ) ;
#68807 = CARTESIAN_POINT ( 'NONE',  ( 80.07812099633126479, 57.44764983040322193, -16.59488970948941500 ) ) ;
#68808 = CARTESIAN_POINT ( 'NONE',  ( 159.7897726928491409, 253.8829904965402875, 16.83923858130328810 ) ) ;
#68809 = CARTESIAN_POINT ( 'NONE',  ( 182.1727452308717830, 281.0742822384698911, -16.91150201624746785 ) ) ;
#68810 = CARTESIAN_POINT ( 'NONE',  ( 149.6690105117817780, 275.3633762259814830, 7.431319680574127062 ) ) ;
#68811 = EDGE_CURVE ( 'NONE', #59206, #2820, #69422, .T. ) ;
#68812 =( BOUNDED_CURVE ( )  B_SPLINE_CURVE ( 2, ( #67852, #98773, #60219, #70713, #48420, #26125, #33217, #47406, #3346 ),
 .UNSPECIFIED., .F., .T. ) 
 B_SPLINE_CURVE_WITH_KNOTS ( ( 3, 2, 2, 2, 3 ),
 ( 0.7701612903225806273, 0.7715053763440860024, 0.7741935483870967527, 0.7768817204301075030, 0.7782258064516128782 ),
 .UNSPECIFIED. ) 
 CURVE ( )  GEOMETRIC_REPRESENTATION_ITEM ( )  RATIONAL_B_SPLINE_CURVE ( ( 0.9330127018922194093, 0.9330127018922194093, 1.000000000000000000, 0.8660254037844387076, 1.000000000000000000, 0.8660254037844387076, 1.000000000000000000, 0.9330127018922194093, 0.9330127018922194093 ) ) 
 REPRESENTATION_ITEM ( '' )  );
#68813 = VECTOR ( 'NONE', #92127, 1000.000000000000000 ) ;
#68814 = CARTESIAN_POINT ( 'NONE',  ( 75.43400731199886877, 56.71754055093797575, -16.11584012409328182 ) ) ;
#68815 = CARTESIAN_POINT ( 'NONE',  ( 108.4196379545418125, 246.7365022471903444, 2.944929066748280225E-16 ) ) ;
#68816 = CARTESIAN_POINT ( 'NONE',  ( 161.4025183475459073, 251.0896330829197041, 14.50747140106038735 ) ) ;
#68817 = CARTESIAN_POINT ( 'NONE',  ( 193.8984187372643362, 285.0395281006325376, -16.96575577898347476 ) ) ;
#68818 = VERTEX_POINT ( 'NONE', #76538 ) ;
#68819 = CARTESIAN_POINT ( 'NONE',  ( -72.48190909937208914, 49.06123820388767598, -10.00000000000000000 ) ) ;
#68820 = VERTEX_POINT ( 'NONE', #85685 ) ;
#68821 = CARTESIAN_POINT ( 'NONE',  ( 166.2218486525947583, 265.2797842516039282, 16.55497466531813089 ) ) ;
#68822 = CARTESIAN_POINT ( 'NONE',  ( 194.2153129458476144, 293.5678207000269708, 14.48779561573898711 ) ) ;
#68823 = DIRECTION ( 'NONE',  ( -0.000000000000000000, -0.000000000000000000, 1.000000000000000000 ) ) ;
#68824 = EDGE_CURVE ( 'NONE', #74259, #76328, #88287, .T. ) ;
#68825 = EDGE_LOOP ( 'NONE', ( #48687, #60116, #55624, #61926 ) ) ;
#68826 = CARTESIAN_POINT ( 'NONE',  ( -22.42236680055709641, 157.8615022471902591, 0.000000000000000000 ) ) ;
#68827 = CARTESIAN_POINT ( 'NONE',  ( 79.24070844107342282, 45.72899464571315775, -12.97329291253947936 ) ) ;
#68828 = CARTESIAN_POINT ( 'NONE',  ( 194.5252985417586729, 293.7192948986070178, -14.54632727629426370 ) ) ;
#68829 = B_SPLINE_CURVE_WITH_KNOTS ( 'NONE', 3,
 ( #1370, #38846, #71278, #69751 ),
 .UNSPECIFIED., .F., .F.,
 ( 4, 4 ),
 ( 0.04862297438902305619, 0.04887066958154939050 ),
 .UNSPECIFIED. ) ;
#68830 = CARTESIAN_POINT ( 'NONE',  ( 83.10776606998568639, 40.75710275334526500, -2.573362665496658816E-06 ) ) ;
#68831 = FACE_OUTER_BOUND ( 'NONE', #34861, .T. ) ;
#68832 = ORIENTED_EDGE ( 'NONE', *, *, #44670, .F. ) ;
#68833 = CARTESIAN_POINT ( 'NONE',  ( 21.37261828447143586, 20.84335787977762777, 9.188101187500006262 ) ) ;
#68834 = VECTOR ( 'NONE', #94557, 1000.000000000000114 ) ;
#68835 = CARTESIAN_POINT ( 'NONE',  ( 75.05636926434671352, 55.10128444218372579, 16.14643111463205472 ) ) ;
#68836 = CARTESIAN_POINT ( 'NONE',  ( 174.9422875208658184, 255.1437964849715456, 8.101495581286821235 ) ) ;
#68837 = CYLINDRICAL_SURFACE ( 'NONE', #69917, 10.00000000000010658 ) ;
#68838 = ORIENTED_EDGE ( 'NONE', *, *, #88176, .F. ) ;
#68839 = CARTESIAN_POINT ( 'NONE',  ( 129.9777503372646095, 257.3967562850347122, -4.648177544792955347E-16 ) ) ;
#68840 = FACE_OUTER_BOUND ( 'NONE', #89710, .T. ) ;
#68841 = AXIS2_PLACEMENT_3D ( 'NONE', #83979, #99645, #75863 ) ;
#68842 = VERTEX_POINT ( 'NONE', #23309 ) ;
#68843 = CARTESIAN_POINT ( 'NONE',  ( 174.5193691037453050, 286.1475687296140791, 10.49811431468850031 ) ) ;
#68845 = CARTESIAN_POINT ( 'NONE',  ( 68.01214654971191464, 65.20889497348429131, -10.65419055744410315 ) ) ;
#68844 = CARTESIAN_POINT ( 'NONE',  ( 71.11357831182630207, 63.84590708448217811, 13.70173731491832392 ) ) ;
#68846 = CARTESIAN_POINT ( 'NONE',  ( 163.4178923001155681, 247.5989030008181260, -10.38047187240561442 ) ) ;
#68847 = CARTESIAN_POINT ( 'NONE',  ( 204.9004517216375518, 275.7490024547470853, 14.55104398969427670 ) ) ;
#68848 = CARTESIAN_POINT ( 'NONE',  ( 188.5315668109907961, 295.4050326786905316, -11.41571884897073552 ) ) ;
#68849 = CARTESIAN_POINT ( 'NONE',  ( 161.2535912560966551, 263.0844709175967182, -17.80682751047658030 ) ) ;
#68850 = CARTESIAN_POINT ( 'NONE',  ( 135.0589402170954827, 248.7833772461660544, -9.188101187500095079 ) ) ;
#68851 = CARTESIAN_POINT ( 'NONE',  ( 176.5127557399464422, 269.0168359773951465, 16.11272065097649886 ) ) ;
#68852 = CARTESIAN_POINT ( 'NONE',  ( 182.3555406741589877, 259.8314379914179426, 9.148843779236386808 ) ) ;
#68853 = CARTESIAN_POINT ( 'NONE',  ( 79.63366147065640632, 204.5327760586659451, 1.948934522072303157E-15 ) ) ;
#68854 = ORIENTED_EDGE ( 'NONE', *, *, #33767, .T. ) ;
#68855 = LINE ( 'NONE', #99776, #25206 ) ;
#68856 = CARTESIAN_POINT ( 'NONE',  ( 184.8387315980094172, 297.9360420897670565, 2.319442688491891502 ) ) ;
#68857 = ORIENTED_EDGE ( 'NONE', *, *, #17705, .F. ) ;
#68858 = CARTESIAN_POINT ( 'NONE',  ( 161.5515493166768977, 252.8315038724842623, 14.92355679770252053 ) ) ;
#68859 = VERTEX_POINT ( 'NONE', #54197 ) ;
#68860 = PLANE ( 'NONE',  #35778 ) ;
#68861 = CARTESIAN_POINT ( 'NONE',  ( 66.65733650514845010, 67.51765459828601479, 6.434609397296672029 ) ) ;
#68862 = CARTESIAN_POINT ( 'NONE',  ( 197.7352955435041792, 287.2275847242548821, 17.01394929260971978 ) ) ;
#68863 = CARTESIAN_POINT ( 'NONE',  ( 146.8859094598974480, 276.2331372299326517, -0.7994986043261681496 ) ) ;
#68864 = CARTESIAN_POINT ( 'NONE',  ( 84.14312167556933275, 48.98415679381830756, 0.000000000000000000 ) ) ;
#68865 = CARTESIAN_POINT ( 'NONE',  ( 154.8679462054080318, 262.4078440388265676, 17.98338675682672871 ) ) ;
#68866 = CARTESIAN_POINT ( 'NONE',  ( 73.27344031762333998, 223.1115022471903160, -5.000000000000047962 ) ) ;
#68867 = CARTESIAN_POINT ( 'NONE',  ( 87.33294734268930881, 44.88192199842172414, 6.808005391826766228 ) ) ;
#68868 = ORIENTED_EDGE ( 'NONE', *, *, #83861, .F. ) ;
#68869 = CARTESIAN_POINT ( 'NONE',  ( 24.66226663818958187, 15.20801979619928979, -3.090169943749474069 ) ) ;
#68870 = CARTESIAN_POINT ( 'NONE',  ( -19.54717911816667453, 93.15931973166004809, 59.99999999999999289 ) ) ;
#68871 = ORIENTED_EDGE ( 'NONE', *, *, #22069, .T. ) ;
#68872 = CARTESIAN_POINT ( 'NONE',  ( 76.04487332539315503, 51.27808848417036103, -16.12710007477251750 ) ) ;
#68873 = CARTESIAN_POINT ( 'NONE',  ( 75.98877566108227199, 65.64741556006092082, -14.26224329751477349 ) ) ;
#68874 = EDGE_CURVE ( 'NONE', #11051, #50774, #38688, .T. ) ;
#68875 = CARTESIAN_POINT ( 'NONE',  ( -31.86539417309037958, 93.39048508798869364, 43.98374761209485229 ) ) ;
#68876 = CARTESIAN_POINT ( 'NONE',  ( 199.0034510736379048, 281.0923298783035875, 17.31675442061273529 ) ) ;
#68877 = CARTESIAN_POINT ( 'NONE',  ( 193.9796946036068164, 292.6643086402947915, -15.64068455845557537 ) ) ;
#68878 = CARTESIAN_POINT ( 'NONE',  ( 139.7406297344813311, 260.6744531367911009, 4.594050593750047540 ) ) ;
#68879 = ORIENTED_EDGE ( 'NONE', *, *, #72640, .T. ) ;
#68880 = CARTESIAN_POINT ( 'NONE',  ( 0.5273063997305784678, 161.1115022471902023, -5.000000000000041744 ) ) ;
#68881 = CARTESIAN_POINT ( 'NONE',  ( -5.860417570053906289, 43.20579575138734896, 59.99999999999999289 ) ) ;
#68882 = ADVANCED_FACE ( 'NONE', ( #45120 ), #93768, .F. ) ;
#68883 = CARTESIAN_POINT ( 'NONE',  ( 80.01804950108486025, 44.42439889875981152, -10.91110617052017773 ) ) ;
#68884 = CARTESIAN_POINT ( 'NONE',  ( 201.4214977800931763, 281.7747274386935601, -17.04225209925078133 ) ) ;
#68885 = B_SPLINE_CURVE_WITH_KNOTS ( 'NONE', 3,
 ( #69232, #31228, #100162, #67751, #29256, #52535, #14051, #6454, #68235, #14555, #6936, #9954, #9442, #833, #78860, #72263 ),
 .UNSPECIFIED., .F., .F.,
 ( 4, 1, 2, 2, 2, 1, 2, 2, 4 ),
 ( 0.000000000000000000, 0.1250000000000008049, 0.1875000000000010270, 0.2500000000000014433, 0.5000000000000019984, 0.6250000000000022204, 0.6875000000000025535, 0.7500000000000027756, 1.000000000000000000 ),
 .UNSPECIFIED. ) ;
#68886 = AXIS2_PLACEMENT_3D ( 'NONE', #17416, #87893, #25526 ) ;
#68887 = CARTESIAN_POINT ( 'NONE',  ( 72.76085654771455324, 70.95487523876634839, 7.692118034595666565 ) ) ;
#68888 = CARTESIAN_POINT ( 'NONE',  ( 66.85524610400479162, 67.34209505064850987, -6.990925417236247164 ) ) ;
#68889 = ORIENTED_EDGE ( 'NONE', *, *, #70740, .T. ) ;
#68890 = CARTESIAN_POINT ( 'NONE',  ( 195.7435253745577484, 265.4158775244591197, 4.456225065319535439 ) ) ;
#68891 = CARTESIAN_POINT ( 'NONE',  ( 77.44118756978804186, 225.5177522451419350, 5.000000000000046185 ) ) ;
#68892 = CARTESIAN_POINT ( 'NONE',  ( 82.15463706511577868, 40.84277258114416043, 1.595534587534165549 ) ) ;
#68893 = CARTESIAN_POINT ( 'NONE',  ( 81.10131807291612915, 51.90498691781395735, 15.05979867673087291 ) ) ;
#68894 = CARTESIAN_POINT ( 'NONE',  ( 83.31927764570698969, 52.39912095965794947, 14.85548028051290181 ) ) ;
#68895 = EDGE_CURVE ( 'NONE', #61117, #100286, #55201, .T. ) ;
#68896 = CARTESIAN_POINT ( 'NONE',  ( 198.4613897724399862, 266.2157086906648260, 0.7828083158938100583 ) ) ;
#68897 = VERTEX_POINT ( 'NONE', #76055 ) ;
#68898 = PLANE ( 'NONE',  #12578 ) ;
#68899 = CARTESIAN_POINT ( 'NONE',  ( 186.1523227505650482, 282.3592835991098582, 16.17628847161935468 ) ) ;
#68900 = EDGE_CURVE ( 'NONE', #67265, #7039, #6636, .T. ) ;
#68901 = VECTOR ( 'NONE', #59925, 1000.000000000000000 ) ;
#68902 = CARTESIAN_POINT ( 'NONE',  ( 207.6477529416552557, 270.9905371579805546, 7.447146952410988341 ) ) ;
#68905 = DIRECTION ( 'NONE',  ( 0.000000000000000000, 0.000000000000000000, 1.000000000000000000 ) ) ;
#68904 = B_SPLINE_CURVE_WITH_KNOTS ( 'NONE', 3,
 ( #74397, #21182, #50069, #36353 ),
 .UNSPECIFIED., .F., .F.,
 ( 4, 4 ),
 ( 0.002991196628981945740, 0.01094109227149283985 ),
 .UNSPECIFIED. ) ;
#68903 = CARTESIAN_POINT ( 'NONE',  ( 194.0672051292551430, 294.5127359636757660, 15.53337744471869364 ) ) ;
#68906 = CARTESIAN_POINT ( 'NONE',  ( 17.16114660649731860, 34.00034080476290654, -1.878358725466461243E-16 ) ) ;
#68907 = EDGE_CURVE ( 'NONE', #27844, #26008, #37511, .T. ) ;
#68908 = CARTESIAN_POINT ( 'NONE',  ( 27.64472685218290238, 176.7677522451417929, -5.000000000000041744 ) ) ;
#68909 = CARTESIAN_POINT ( 'NONE',  ( 166.1902696474969332, 285.7546370014056265, -3.171513238404533030 ) ) ;
#68910 = LINE ( 'NONE', #51741, #98463 ) ;
#68911 = VECTOR ( 'NONE', #14350, 1000.000000000000114 ) ;
#68912 = CARTESIAN_POINT ( 'NONE',  ( 198.0792648159935538, 287.5636447432459022, 17.04758482866669667 ) ) ;
#68913 = CARTESIAN_POINT ( 'NONE',  ( -13.97887943725652882, 171.9244531367911293, -4.594050593750046652 ) ) ;
#68914 = CARTESIAN_POINT ( 'NONE',  ( 46.88368875251780565, 110.3874725885333135, 10.00000000000000000 ) ) ;
#68915 = ORIENTED_EDGE ( 'NONE', *, *, #77789, .F. ) ;
#68916 = CARTESIAN_POINT ( 'NONE',  ( 67.05214125078322240, 67.71989302486406359, -6.480270855117335138 ) ) ;
#68917 = CARTESIAN_POINT ( 'NONE',  ( 72.78963790118943677, 71.14248580567581826, -7.401817665068018748 ) ) ;
#68918 = CARTESIAN_POINT ( 'NONE',  ( 81.84240242494415440, 41.28568805806720832, 5.918639025823554611 ) ) ;
#68919 = CARTESIAN_POINT ( 'NONE',  ( 5.858601742122021783, 180.3149278399161233, 9.188101187500093303 ) ) ;
#68920 = CARTESIAN_POINT ( 'NONE',  ( 29.18428119120667574, 28.80066082961423390, 10.00000000000000533 ) ) ;
#68921 = CARTESIAN_POINT ( 'NONE',  ( 77.57594518282449769, 55.55670249163367913, 16.58798725124399454 ) ) ;
#68922 = CARTESIAN_POINT ( 'NONE',  ( 205.1793861064249711, 275.2658739283173759, -14.08953480709093675 ) ) ;
#68923 = LINE ( 'NONE', #92284, #31330 ) ;
#68924 = ADVANCED_FACE ( 'NONE', ( #53705 ), #29924, .F. ) ;
#68925 = CARTESIAN_POINT ( 'NONE',  ( 179.1363749232007194, 255.1691260420666936, -3.970956364734916200 ) ) ;
#68926 = CARTESIAN_POINT ( 'NONE',  ( 188.0010984285647453, 259.1527977912059555, -0.8004646550165761543 ) ) ;
#68927 = EDGE_CURVE ( 'NONE', #75741, #69092, #84660, .T. ) ;
#68928 = CARTESIAN_POINT ( 'NONE',  ( 60.78824074639776143, 199.2365022471902307, 10.00000000000009592 ) ) ;
#68929 = CARTESIAN_POINT ( 'NONE',  ( -7.338644212303985448, 23.89290704711799052, -10.00000000000000000 ) ) ;
#68930 = CARTESIAN_POINT ( 'NONE',  ( 189.9457600613112902, 301.6512882219586800, 0.04117870562599101891 ) ) ;
#68931 = CARTESIAN_POINT ( 'NONE',  ( 14.70821206310299978, 188.4869531367911293, 4.594050593750046652 ) ) ;
#68932 = CARTESIAN_POINT ( 'NONE',  ( 47.22349865033176286, 113.7415181542322955, 177.5919119679930134 ) ) ;
#68933 = LINE ( 'NONE', #46636, #69478 ) ;
#68934 = CARTESIAN_POINT ( 'NONE',  ( 77.28526253906952093, 49.15772476309707173, -14.80239747722083621 ) ) ;
#68935 = CARTESIAN_POINT ( 'NONE',  ( 205.0859877718122561, 268.9368413191317586, -3.038556538008958974 ) ) ;
#68936 = CARTESIAN_POINT ( 'NONE',  ( 49.80235952159635104, 79.38263285747564169, -10.00000000000000000 ) ) ;
#68937 = EDGE_CURVE ( 'NONE', #37468, #70599, #18731, .T. ) ;
#68938 = CARTESIAN_POINT ( 'NONE',  ( 188.5872477108457019, 268.1141654234737643, 13.52445048591414434 ) ) ;
#68939 = CARTESIAN_POINT ( 'NONE',  ( 163.2204695044033826, 281.0533932320078065, -10.15560040158997346 ) ) ;
#68940 = CARTESIAN_POINT ( 'NONE',  ( 160.4256035324680454, 280.6369556960792124, 9.497879217036381050 ) ) ;
#68941 = CARTESIAN_POINT ( 'NONE',  ( 22.77687932801360660, 15.01110640527292261, 2.839279412974134775 ) ) ;
#68942 = CARTESIAN_POINT ( 'NONE',  ( 148.1672759425158290, 274.0137453789218398, 7.847779094015780110 ) ) ;
#68943 = CARTESIAN_POINT ( 'NONE',  ( 71.59150237832598407, 59.07131284048556807, 15.83293140498724050 ) ) ;
#68944 = VECTOR ( 'NONE', #69258, 1000.000000000000000 ) ;
#68945 = CARTESIAN_POINT ( 'NONE',  ( 155.5660013421004919, 261.1987770755905558, 17.28709111629370199 ) ) ;
#68946 = VERTEX_POINT ( 'NONE', #39998 ) ;
#68947 = CARTESIAN_POINT ( 'NONE',  ( 86.99519960183430101, 45.47778473895603923, -7.388714814205115111 ) ) ;
#68948 = AXIS2_PLACEMENT_3D ( 'NONE', #35862, #50070, #73384 ) ;
#68949 = CARTESIAN_POINT ( 'NONE',  ( 176.0893140685097364, 259.6469405521993394, 13.94800846836438879 ) ) ;
#68950 = EDGE_CURVE ( 'NONE', #32335, #51511, #92225, .T. ) ;
#68951 = CARTESIAN_POINT ( 'NONE',  ( 148.7588072053147243, 273.7711778218048835, -8.803803025135483296 ) ) ;
#68952 = CARTESIAN_POINT ( 'NONE',  ( 88.26419143691403235, 44.30358433922314276, 2.120137394640778883 ) ) ;
#68953 = EDGE_CURVE ( 'NONE', #16754, #95045, #55691, .T. ) ;
#68954 = ORIENTED_EDGE ( 'NONE', *, *, #57306, .T. ) ;
#68955 = CARTESIAN_POINT ( 'NONE',  ( 35.39012114306879653, 16.59285393851897084, -10.00000000000000000 ) ) ;
#68956 = CARTESIAN_POINT ( 'NONE',  ( 72.29675234079142854, 71.91852905550483399, -5.160928375136445645 ) ) ;
#68957 = VECTOR ( 'NONE', #35251, 1000.000000000000000 ) ;
#68958 = CARTESIAN_POINT ( 'NONE',  ( 27.61987535298997187, 21.11029122506295508, -8.090169943749478065 ) ) ;
#68959 = CARTESIAN_POINT ( 'NONE',  ( 86.84691188820112018, 44.77746935395023087, 7.166350442650676555 ) ) ;
#68960 = VERTEX_POINT ( 'NONE', #40995 ) ;
#68961 = ORIENTED_EDGE ( 'NONE', *, *, #67258, .F. ) ;
#68963 = CARTESIAN_POINT ( 'NONE',  ( 85.70718678116344336, 42.98724156638103722, -2.704305901507331189 ) ) ;
#68962 = CARTESIAN_POINT ( 'NONE',  ( 68.68909986782581711, 64.16576715805911135, -12.55144644517788421 ) ) ;
#68964 = ORIENTED_EDGE ( 'NONE', *, *, #84191, .T. ) ;
#68965 = CARTESIAN_POINT ( 'NONE',  ( 191.5694459269389824, 298.8389818071599962, 7.944420692511652504 ) ) ;
#68966 = CARTESIAN_POINT ( 'NONE',  ( 70.59980718957763202, 66.46770090284240950, 11.57891045287148479 ) ) ;
#68967 = CARTESIAN_POINT ( 'NONE',  ( 79.98470177819076810, 58.12003377381869029, 16.26822267875589390 ) ) ;
#68968 = CARTESIAN_POINT ( 'NONE',  ( 46.08672700828314817, 69.01776843458344501, 10.00000000000000000 ) ) ;
#68969 = ORIENTED_EDGE ( 'NONE', *, *, #90976, .T. ) ;
#68970 = CARTESIAN_POINT ( 'NONE',  ( 148.3930300673291640, 273.6227277647267897, 8.375036249079425232 ) ) ;
#68971 = CARTESIAN_POINT ( 'NONE',  ( 149.4965729687386045, 271.7113353911534546, -11.48413836595348059 ) ) ;
#68972 = ORIENTED_EDGE ( 'NONE', *, *, #91303, .F. ) ;
#68973 = AXIS2_PLACEMENT_3D ( 'NONE', #61305, #16710, #47603 ) ;
#68974 = CARTESIAN_POINT ( 'NONE',  ( 195.8449251089225811, 291.4336346372613775, 16.14492769602857081 ) ) ;
#68975 = VECTOR ( 'NONE', #33500, 1000.000000000000000 ) ;
#68976 = CYLINDRICAL_SURFACE ( 'NONE', #80183, 3.300000000000010925 ) ;
#68977 = ORIENTED_EDGE ( 'NONE', *, *, #81676, .F. ) ;
#68978 = CARTESIAN_POINT ( 'NONE',  ( -19.76768764414644153, 93.14864796480769371, 59.99999999999999289 ) ) ;
#68979 = CARTESIAN_POINT ( 'NONE',  ( 78.15521468916944059, 47.58268334285837398, -13.88154174790995832 ) ) ;
#68980 = ORIENTED_EDGE ( 'NONE', *, *, #46993, .T. ) ;
#68981 = CARTESIAN_POINT ( 'NONE',  ( -17.93832473636817326, 77.02999682207506282, 13.50375772155920195 ) ) ;
#68982 = CARTESIAN_POINT ( 'NONE',  ( -62.95439910331221256, 68.06504152958493137, 40.00000000000000000 ) ) ;
#68983 = CARTESIAN_POINT ( 'NONE',  ( -19.65312891409030271, 93.06504152958497400, 177.5919119679930134 ) ) ;
#68985 = CIRCLE ( 'NONE', #38236, 70.00000000000001421 ) ;
#68984 = CARTESIAN_POINT ( 'NONE',  ( 83.40377981393274354, 52.41387144640057727, 14.84149447075486350 ) ) ;
#68986 = VERTEX_POINT ( 'NONE', #3543 ) ;
#68987 = ORIENTED_EDGE ( 'NONE', *, *, #223, .T. ) ;
#68988 = CARTESIAN_POINT ( 'NONE',  ( 87.13786027870773410, 46.31489396970533789, 8.575336957479223088 ) ) ;
#68989 = CARTESIAN_POINT ( 'NONE',  ( 190.4281805785508084, 300.8157113754859893, -1.233909217199055774 ) ) ;
#68990 = CARTESIAN_POINT ( 'NONE',  ( 190.2935937139882299, 301.0488226629397559, 4.649863831023156813 ) ) ;
#68991 = CARTESIAN_POINT ( 'NONE',  ( 171.4241271215416020, 275.6058901121958229, -15.93988569491697938 ) ) ;
#68992 = CARTESIAN_POINT ( 'NONE',  ( 146.9495969992948403, 276.1228271758872665, 0.7992850717744988120 ) ) ;
#68993 = CARTESIAN_POINT ( 'NONE',  ( 146.8637854207107409, 276.2714571898724216, 0.7988785540157756770 ) ) ;
#68994 = FACE_OUTER_BOUND ( 'NONE', #89507, .T. ) ;
#68995 = CARTESIAN_POINT ( 'NONE',  ( 72.04811769650321196, 71.35602353065118564, 5.168332083721268511 ) ) ;
#68996 = CARTESIAN_POINT ( 'NONE',  ( 66.31795133325435643, 69.20145725284447735, 2.477662600225432055 ) ) ;
#68997 = CARTESIAN_POINT ( 'NONE',  ( 66.98349674211237925, 66.92588320361704746, 8.745657410628504991 ) ) ;
#68998 = CARTESIAN_POINT ( 'NONE',  ( 167.9052210226905970, 286.9632124721071591, 3.486985599330678198 ) ) ;
#68999 = CARTESIAN_POINT ( 'NONE',  ( 77.93929205318025311, 48.04607352951135368, 14.17332408082497963 ) ) ;
#69000 = VERTEX_POINT ( 'NONE', #57704 ) ;
#69001 = LINE ( 'NONE', #83760, #70768 ) ;
#69002 = CARTESIAN_POINT ( 'NONE',  ( 71.00886383429117643, 67.21468722179194799, 10.46115210183619659 ) ) ;
#69003 = CARTESIAN_POINT ( 'NONE',  ( 173.2337249902883798, 270.7486416191997023, 17.82094672905207133 ) ) ;
#69004 = CARTESIAN_POINT ( 'NONE',  ( 79.45999046205805882, 46.29338198536788695, 12.66529585336078156 ) ) ;
#69005 = CARTESIAN_POINT ( 'NONE',  ( 190.7685386727469279, 298.2261938635710976, -9.678376712886644029 ) ) ;
#69006 = CARTESIAN_POINT ( 'NONE',  ( 74.53665744383957303, 56.45882270339276232, -16.57090531272829637 ) ) ;
#69007 = CARTESIAN_POINT ( 'NONE',  ( 168.6977591771627090, 286.2750216774235241, -7.847692359145494123 ) ) ;
#69008 = ORIENTED_EDGE ( 'NONE', *, *, #66494, .T. ) ;
#69009 = CARTESIAN_POINT ( 'NONE',  ( 163.3409975114459485, 247.7320886816312111, -10.96358124877083640 ) ) ;
#69010 = CARTESIAN_POINT ( 'NONE',  ( 206.3018347371251195, 273.3217358710584790, -9.309724106897926177 ) ) ;
#69011 = CARTESIAN_POINT ( 'NONE',  ( 72.37171713508972459, 71.57547101742603957, 5.089270018883309987 ) ) ;
#69012 = CARTESIAN_POINT ( 'NONE',  ( 42.72800263476181470, 202.1427522451419350, 10.00000000000009237 ) ) ;
#69014 = CARTESIAN_POINT ( 'NONE',  ( 124.8563387505838165, 233.7048013555409796, 4.594050593750051981 ) ) ;
#69013 = B_SPLINE_CURVE_WITH_KNOTS ( 'NONE', 3,
 ( #86038, #63167, #77380, #16566, #23155, #14582, #54046, #8968 ),
 .UNSPECIFIED., .F., .F.,
 ( 4, 2, 2, 4 ),
 ( 0.000000000000000000, 0.2251665007938979668, 0.3377497511908476580, 0.4503330015877973214 ),
 .UNSPECIFIED. ) ;
#69015 = ADVANCED_FACE ( 'NONE', ( #48636 ), #32913, .F. ) ;
#69016 = CARTESIAN_POINT ( 'NONE',  ( 151.4428545556028780, 268.3402767968688067, -15.03309903163500749 ) ) ;
#69017 = CARTESIAN_POINT ( 'NONE',  ( 66.79137522077492406, 67.56334705497756943, -6.492718058864330288 ) ) ;
#69018 = CARTESIAN_POINT ( 'NONE',  ( 196.4390255720217908, 290.4046224503736653, 16.34739044515864848 ) ) ;
#69019 = CARTESIAN_POINT ( 'NONE',  ( 172.4760895491598092, 250.5888413570013711, -4.125262657830087498 ) ) ;
#69020 = CARTESIAN_POINT ( 'NONE',  ( 42.23166870106845039, 201.3149278399160664, 9.188101187500093303 ) ) ;
#69021 = AXIS2_PLACEMENT_3D ( 'NONE', #45440, #60136, #61136 ) ;
#69022 = CARTESIAN_POINT ( 'NONE',  ( 147.6309342515288847, 275.3284714954338028, -3.240618580837187235 ) ) ;
#69023 = CARTESIAN_POINT ( 'NONE',  ( 85.71030961992515529, 48.80922481583876049, -12.49884386288095151 ) ) ;
#69024 = ORIENTED_EDGE ( 'NONE', *, *, #72281, .F. ) ;
#69025 = CARTESIAN_POINT ( 'NONE',  ( 71.64267482440028800, 65.36664440745120430, 12.36713528089073399 ) ) ;
#69026 = CARTESIAN_POINT ( 'NONE',  ( 178.3097688579141220, 265.5568989673392366, 16.02486382646369023 ) ) ;
#69027 = ADVANCED_FACE ( 'NONE', ( #64830 ), #26824, .T. ) ;
#69028 = B_SPLINE_SURFACE_WITH_KNOTS ( 'NONE', 3, 1, ( 
 ( #55771, #54277 ),
 ( #47194, #8705 ),
 ( #85246, #15791 ),
 ( #85771, #62895 ),
 ( #78115, #46697 ),
 ( #1111, #24404 ),
 ( #71525, #55280 ),
 ( #78620, #9207 ),
 ( #71025, #86259 ),
 ( #94342, #16798 ),
 ( #40080, #10215 ),
 ( #24896, #86764 ),
 ( #17298, #63899 ),
 ( #79148, #94837 ),
 ( #48718, #40584 ),
 ( #25400, #56288 ),
 ( #69990, #39077 ),
 ( #87286, #17817 ),
 ( #79649, #72018 ),
 ( #57787, #82150 ),
 ( #81640, #72531 ),
 ( #95369, #11717 ),
 ( #43071, #27412 ),
 ( #88264, #58774 ),
 ( #49216, #50198 ),
 ( #88764, #18316 ),
 ( #27894, #64911 ),
 ( #19816, #58290 ),
 ( #4600, #3140 ),
 ( #34023, #95855 ),
 ( #4095, #74014 ),
 ( #43589, #73026 ),
 ( #42579, #56794 ),
 ( #2622, #35493 ) ),
 .UNSPECIFIED., .T., .F., .F.,
 ( 4, 2, 2, 2, 2, 2, 2, 2, 2, 2, 2, 2, 2, 2, 2, 2, 4 ),
 ( 2, 2 ),
 ( 0.000000000000000000, 0.06250000000000000000, 0.1250000000000000000, 0.1875000000000000000, 0.2500000000000000000, 0.3125000000000000000, 0.3750000000000000000, 0.4375000000000000000, 0.5000000000000000000, 0.5625000000000000000, 0.6250000000000000000, 0.6875000000000000000, 0.7500000000000000000, 0.8125000000000000000, 0.8750000000000000000, 0.9375000000000000000, 1.000000000000000000 ),
 ( 0.000000000000000000, 1.000000000000000000 ),
 .UNSPECIFIED. ) ;
#69029 = CARTESIAN_POINT ( 'NONE',  ( 15.77038241084232517, 34.14663330942826036, -10.00000000000000000 ) ) ;
#69030 = VECTOR ( 'NONE', #3616, 1000.000000000000114 ) ;
#69031 = EDGE_CURVE ( 'NONE', #36202, #38035, #72452, .T. ) ;
#69032 = CARTESIAN_POINT ( 'NONE',  ( 190.9559560067148425, 299.9015775189195665, -4.895152914295826108 ) ) ;
#69033 = CARTESIAN_POINT ( 'NONE',  ( 151.9868571940785955, 278.2923008623533860, -1.631775907428277828 ) ) ;
#69034 = LINE ( 'NONE', #52838, #28494 ) ;
#69035 = CARTESIAN_POINT ( 'NONE',  ( 182.0568989607672563, 262.3880894348699258, 13.01387681392468032 ) ) ;
#69036 = CARTESIAN_POINT ( 'NONE',  ( 105.0818317072414061, 238.1427522451419065, 10.00000000000009237 ) ) ;
#69037 = CARTESIAN_POINT ( 'NONE',  ( 194.4068849611547876, 293.4209623680436039, -14.51840781236480815 ) ) ;
#69038 = ORIENTED_EDGE ( 'NONE', *, *, #21458, .F. ) ;
#69039 = CARTESIAN_POINT ( 'NONE',  ( 163.2442700311756596, 247.8996255919473697, 11.14021925110252020 ) ) ;
#69040 = CARTESIAN_POINT ( 'NONE',  ( 84.04720468787148491, 46.80380424559275809, -11.65275933647250639 ) ) ;
#69041 = AXIS2_PLACEMENT_3D ( 'NONE', #68653, #22562, #15435 ) ;
#69042 = CARTESIAN_POINT ( 'NONE',  ( 27.23877744593285755, 186.5333772461660544, 9.188101187500095079 ) ) ;
#69043 = CARTESIAN_POINT ( 'NONE',  ( 6.173449292434340485, 27.65659080271448644, -1.878358725466461243E-16 ) ) ;
#69044 = CIRCLE ( 'NONE', #35068, 15.10714546451156792 ) ;
#69045 = CARTESIAN_POINT ( 'NONE',  ( 195.0933036672505807, 273.3794171182236141, 14.45588861630873723 ) ) ;
#69046 = CARTESIAN_POINT ( 'NONE',  ( 71.47065342991831471, 59.20086974812521419, -15.77730099079427362 ) ) ;
#69047 = CARTESIAN_POINT ( 'NONE',  ( 73.06086572573603632, 69.73927861498383152, 9.650215327041465230 ) ) ;
#69049 = CARTESIAN_POINT ( 'NONE',  ( 65.07308872588301085, 214.5024278399160949, -9.188101187500093303 ) ) ;
#69048 = CARTESIAN_POINT ( 'NONE',  ( 194.7402207200854605, 275.0729057474629258, -15.80694078002163927 ) ) ;
#69050 = CARTESIAN_POINT ( 'NONE',  ( 200.6129772034685175, 283.1751261563724142, 18.36811917402039640 ) ) ;
#69051 = CARTESIAN_POINT ( 'NONE',  ( 55.79055247517715799, 193.0177522451417929, 5.000000000000051514 ) ) ;
#69052 = CARTESIAN_POINT ( 'NONE',  ( 9.331744567327184825, 27.16126292948893806, -6.180339887498951690 ) ) ;
#69053 = ORIENTED_EDGE ( 'NONE', *, *, #27885, .T. ) ;
#69054 = B_SPLINE_CURVE_WITH_KNOTS ( 'NONE', 3,
 ( #76126, #8197, #6197, #77087 ),
 .UNSPECIFIED., .F., .F.,
 ( 4, 4 ),
 ( 0.03237264616844526960, 0.04133669968024545477 ),
 .UNSPECIFIED. ) ;
#69055 = VECTOR ( 'NONE', #12438, 999.9999999999998863 ) ;
#69056 = EDGE_CURVE ( 'NONE', #36969, #28484, #1579, .T. ) ;
#69057 = CARTESIAN_POINT ( 'NONE',  ( 4.496589500409156948, 186.7365022471903444, 2.944929066748280225E-16 ) ) ;
#69058 = DIRECTION ( 'NONE',  ( -1.000000000000000000, 0.000000000000000000, 0.000000000000000000 ) ) ;
#69059 = CARTESIAN_POINT ( 'NONE',  ( 136.7095408212358052, 258.9244531367911577, -4.594050593750046652 ) ) ;
#69060 = CARTESIAN_POINT ( 'NONE',  ( 36.95804531498377798, 23.19860640527294748, 2.839279412974134775 ) ) ;
#69061 = CARTESIAN_POINT ( 'NONE',  ( 81.82670292275410873, 58.99631176529970844, 0.4698463103929552132 ) ) ;
#69062 = CARTESIAN_POINT ( 'NONE',  ( 174.6066048939933921, 262.0940252294753918, 15.79829227059981278 ) ) ;
#69063 = EDGE_CURVE ( 'NONE', #16291, #38703, #79831, .T. ) ;
#69064 = DIRECTION ( 'NONE',  ( -0.000000000000000000, -0.000000000000000000, 1.000000000000000000 ) ) ;
#69066 = DIRECTION ( 'NONE',  ( 0.8660254037844395958, 0.4999999999999985567, 0.000000000000000000 ) ) ;
#69065 = CARTESIAN_POINT ( 'NONE',  ( 88.40933139567989940, 44.00655032011064804, 2.323659332633154495 ) ) ;
#69067 = EDGE_CURVE ( 'NONE', #3105, #4844, #75958, .T. ) ;
#69068 = CARTESIAN_POINT ( 'NONE',  ( 68.86379457292682105, 64.30659086896544352, 12.52137705277578661 ) ) ;
#69069 = ORIENTED_EDGE ( 'NONE', *, *, #24192, .T. ) ;
#69070 = CARTESIAN_POINT ( 'NONE',  ( 150.6655900823359389, 269.6865383554857090, 15.31288044136207205 ) ) ;
#69071 = CARTESIAN_POINT ( 'NONE',  ( 150.2076754159204484, 245.9824982072973683, 3.021315404115420679E-15 ) ) ;
#69072 = CARTESIAN_POINT ( 'NONE',  ( 156.6715577256040035, 280.1715312555409128, -5.356107003133066868 ) ) ;
#69073 = CARTESIAN_POINT ( 'NONE',  ( 6.943673075435187414, 24.98502408145590437, -5.678558825948271327 ) ) ;
#69074 = EDGE_LOOP ( 'NONE', ( #67762, #4867, #29071, #81802 ) ) ;
#69075 = DIRECTION ( 'NONE',  ( 0.4999999999999998890, -0.8660254037844385966, 0.000000000000000000 ) ) ;
#69077 = EDGE_CURVE ( 'NONE', #68477, #35732, #73926, .T. ) ;
#69076 = CARTESIAN_POINT ( 'NONE',  ( 41.24097861217908445, 35.76159833115055164, -9.594050593750004907 ) ) ;
#69078 = CARTESIAN_POINT ( 'NONE',  ( 157.6500260163024620, 257.5891404556457474, -18.23450497588216379 ) ) ;
#69079 = EDGE_CURVE ( 'NONE', #5333, #89008, #19738, .T. ) ;
#69080 = ADVANCED_FACE ( 'NONE', ( #84423 ), #4019, .T. ) ;
#69081 = CARTESIAN_POINT ( 'NONE',  ( 200.4906113350036776, 281.3870700576555919, -17.24871243658977704 ) ) ;
#69082 = CARTESIAN_POINT ( 'NONE',  ( -13.88625461359388957, 104.5404930901994334, 43.90693181722170380 ) ) ;
#69083 = CARTESIAN_POINT ( 'NONE',  ( 188.6301707762981152, 265.0060877223691591, -12.46499516475016733 ) ) ;
#69084 = CARTESIAN_POINT ( 'NONE',  ( 163.4139553296302267, 247.6057220337265505, -10.31482883765270842 ) ) ;
#69085 = CARTESIAN_POINT ( 'NONE',  ( 152.7295469705997277, 266.1116601603806657, -17.40211458100010589 ) ) ;
#69086 = CARTESIAN_POINT ( 'NONE',  ( 190.5057874690362212, 281.5141710404896571, 17.75392602039427459 ) ) ;
#69087 = CARTESIAN_POINT ( 'NONE',  ( 73.05796794158769103, 70.59459209629945065, 7.799841062623454668 ) ) ;
#69088 = ORIENTED_EDGE ( 'NONE', *, *, #30062, .F. ) ;
#69089 = CARTESIAN_POINT ( 'NONE',  ( 190.7516742497373059, 300.2554039010641418, 4.342609251298632067 ) ) ;
#69090 = CARTESIAN_POINT ( 'NONE',  ( 7.293129863248505984, 185.0177522451419065, 5.000000000000046185 ) ) ;
#69091 = CARTESIAN_POINT ( 'NONE',  ( 84.50184486765282088, 45.13281382370418271, -8.938886561040149559 ) ) ;
#69092 = VERTEX_POINT ( 'NONE', #27816 ) ;
#69093 = CARTESIAN_POINT ( 'NONE',  ( 162.8068419036826526, 250.8157941814552885, -13.07079287990798022 ) ) ;
#69094 = CARTESIAN_POINT ( 'NONE',  ( -42.47074677134370546, 28.21475011077167849, -10.00000000000000000 ) ) ;
#69095 = CARTESIAN_POINT ( 'NONE',  ( 196.9319848161575806, 289.5507919934690335, -17.64330560362266453 ) ) ;
#69096 = CARTESIAN_POINT ( 'NONE',  ( 69.33684657993413225, 62.91444721635136261, 13.64444443003713658 ) ) ;
#69097 = ORIENTED_EDGE ( 'NONE', *, *, #20040, .F. ) ;
#69098 = CARTESIAN_POINT ( 'NONE',  ( 110.0256537107753161, 225.1423013555409796, -4.594050593750043987 ) ) ;
#69099 = CARTESIAN_POINT ( 'NONE',  ( 155.5050174552892486, 261.3044042659909110, 18.56563012484838282 ) ) ;
#69100 = CIRCLE ( 'NONE', #14150, 17.82106496071138935 ) ;
#69101 = CARTESIAN_POINT ( 'NONE',  ( 181.1059962512928507, 271.7445022709790123, -16.71226964961464390 ) ) ;
#69102 = CARTESIAN_POINT ( 'NONE',  ( 81.64076222525299897, 42.65095382059221407, -7.589903255537720383 ) ) ;
#69103 = B_SPLINE_CURVE_WITH_KNOTS ( 'NONE', 3,
 ( #13533, #44402, #28214, #14019, #75335, #91058, #37303, #27232, #58116, #19648, #81461, #12036, #73828, #76806, #77825, #85457 ),
 .UNSPECIFIED., .F., .F.,
 ( 4, 1, 2, 2, 2, 1, 2, 2, 4 ),
 ( 0.000000000000000000, 0.1249999999999977796, 0.1874999999999976130, 0.2499999999999974465, 0.4999999999999986677, 0.6249999999999964473, 0.6874999999999977796, 0.7499999999999991118, 1.000000000000000000 ),
 .UNSPECIFIED. ) ;
#69104 = VERTEX_POINT ( 'NONE', #35411 ) ;
#69105 = ORIENTED_EDGE ( 'NONE', *, *, #70380, .F. ) ;
#69106 = VERTEX_POINT ( 'NONE', #20228 ) ;
#69107 = DIRECTION ( 'NONE',  ( -0.6444573283589029034, 0.7646402761589956576, 0.000000000000000000 ) ) ;
#69108 = ORIENTED_EDGE ( 'NONE', *, *, #20676, .T. ) ;
#69109 = CARTESIAN_POINT ( 'NONE',  ( 67.87260471423661556, 67.92298336072001064, 7.036170726210575488 ) ) ;
#69110 = VERTEX_POINT ( 'NONE', #14969 ) ;
#69111 = CARTESIAN_POINT ( 'NONE',  ( 164.4698008747318738, 245.7769439046653019, -6.272955660526681854 ) ) ;
#69112 = VECTOR ( 'NONE', #70250, 1000.000000000000000 ) ;
#69113 =( BOUNDED_CURVE ( )  B_SPLINE_CURVE ( 2, ( #78818, #40278, #57483, #43651, #74591, #5168, #36047, #9918, #66950, #17500, #40776, #97879, #1811 ),
 .UNSPECIFIED., .F., .T. ) 
 B_SPLINE_CURVE_WITH_KNOTS ( ( 3, 2, 2, 2, 2, 2, 3 ),
 ( 0.3875000000000000111, 0.3900000000000000133, 0.3950000000000000178, 0.4000000000000000222, 0.4050000000000000266, 0.4099999999999999756, 0.4124999999999999778 ),
 .UNSPECIFIED. ) 
 CURVE ( )  GEOMETRIC_REPRESENTATION_ITEM ( )  RATIONAL_B_SPLINE_CURVE ( ( 0.9755282581475768211, 0.9755282581475768211, 1.000000000000000000, 0.9510565162951535312, 1.000000000000000000, 0.9510565162951535312, 1.000000000000000000, 0.9510565162951535312, 1.000000000000000000, 0.9510565162951535312, 1.000000000000000000, 0.9755282581475768211, 0.9755282581475768211 ) ) 
 REPRESENTATION_ITEM ( '' )  );
#69114 = DIRECTION ( 'NONE',  ( 0.9563064286990885510, -0.2923662333936583035, 0.000000000000000000 ) ) ;
#69116 = EDGE_CURVE ( 'NONE', #19784, #49074, #51984, .T. ) ;
#69115 = CARTESIAN_POINT ( 'NONE',  ( 170.6086979342741756, 283.5704196183729664, 12.42145073055875848 ) ) ;
#69117 = CARTESIAN_POINT ( 'NONE',  ( 147.6512387128590262, 274.9075480792844246, -8.209968531507987777 ) ) ;
#69118 = CARTESIAN_POINT ( 'NONE',  ( 67.46170827899872791, 68.25562313450184604, -5.901104080436347488 ) ) ;
#69119 = CARTESIAN_POINT ( 'NONE',  ( 156.9694903541507074, 266.1758412851487492, -17.34135443527054576 ) ) ;
#69120 = CARTESIAN_POINT ( 'NONE',  ( 15.18774714507562962, 26.95586893147754992, 7.433330006724141015 ) ) ;
#69121 = CARTESIAN_POINT ( 'NONE',  ( 198.3488621476923299, 277.3687303151504011, -15.33574521144890035 ) ) ;
#69122 = FACE_OUTER_BOUND ( 'NONE', #44088, .T. ) ;
#69124 = EDGE_LOOP ( 'NONE', ( #85336, #3867, #24746, #35593 ) ) ;
#69123 = DIRECTION ( 'NONE',  ( -0.1963739994383812415, 0.9805290675673896672, 0.000000000000000000 ) ) ;
#69125 = AXIS2_PLACEMENT_3D ( 'NONE', #43083, #80160, #87791 ) ;
#69126 = CARTESIAN_POINT ( 'NONE',  ( 202.8787628851569593, 279.2506702366259788, 17.01435431865322556 ) ) ;
#69127 = CARTESIAN_POINT ( 'NONE',  ( 185.6854299893530253, 258.0255741828406713, 3.062601813168996046 ) ) ;
#69128 = LINE ( 'NONE', #100055, #82943 ) ;
#69129 = CARTESIAN_POINT ( 'NONE',  ( 157.4371224504884594, 277.4660405788308140, -11.46929413857212410 ) ) ;
#69130 = CARTESIAN_POINT ( 'NONE',  ( 200.6129772034685175, 283.1751261563724142, 18.36811917402039640 ) ) ;
#69131 = CARTESIAN_POINT ( 'NONE',  ( 194.2393705908959305, 262.4612896885397504, -0.8107168165472325994 ) ) ;
#69132 = CARTESIAN_POINT ( 'NONE',  ( 155.0127500294823051, 262.1570364583997161, -18.06877476110779668 ) ) ;
#69133 = CIRCLE ( 'NONE', #83718, 17.82106496071138935 ) ;
#69134 = LINE ( 'NONE', #91481, #88918 ) ;
#69135 = CARTESIAN_POINT ( 'NONE',  ( 4.262040950003013862, 173.2677522451418781, 10.00000000000009592 ) ) ;
#69136 = EDGE_CURVE ( 'NONE', #34021, #91664, #30179, .T. ) ;
#69137 = CARTESIAN_POINT ( 'NONE',  ( 82.80324341411446198, 53.35862238445501049, -15.29491566309662431 ) ) ;
#69138 = B_SPLINE_CURVE_WITH_KNOTS ( 'NONE', 3,
 ( #45330, #84871, #52934, #52434, #37720, #61018, #7841, #68630, #15414, #69628 ),
 .UNSPECIFIED., .F., .F.,
 ( 4, 2, 2, 2, 4 ),
 ( 0.000000000000000000, 0.2500000000000000000, 0.5000000000000000000, 0.7500000000000000000, 1.000000000000000000 ),
 .UNSPECIFIED. ) ;
#69139 = DIRECTION ( 'NONE',  ( -0.4140345431502778228, -0.9102611697080902342, 0.000000000000000000 ) ) ;
#69140 = CARTESIAN_POINT ( 'NONE',  ( 168.7096392155106344, 280.2107777274362093, -14.47775774749160682 ) ) ;
#69141 = CARTESIAN_POINT ( 'NONE',  ( 72.00034353288134525, 72.28740038217357267, 0.6661088224210791608 ) ) ;
#69142 = CARTESIAN_POINT ( 'NONE',  ( -19.56010499341666886, 93.17209426810804018, 59.99999999999999289 ) ) ;
#69144 = CARTESIAN_POINT ( 'NONE',  ( 76.25214315863026115, 65.18377266038437767, 14.56725100193072464 ) ) ;
#69143 = CARTESIAN_POINT ( 'NONE',  ( -3.504777292649704279, 156.5327760586659451, 1.948934522072303157E-15 ) ) ;
#69145 = CARTESIAN_POINT ( 'NONE',  ( 162.9933781180035339, 248.8079414735530008, 9.823679460557467991 ) ) ;
#69146 = ORIENTED_EDGE ( 'NONE', *, *, #44251, .F. ) ;
#69147 = EDGE_LOOP ( 'NONE', ( #26667, #2098, #64176, #17920, #91435, #4062, #45068 ) ) ;
#69148 = CARTESIAN_POINT ( 'NONE',  ( -54.12856498932600147, 45.58573084041748302, 59.99999999999999289 ) ) ;
#69149 = EDGE_CURVE ( 'NONE', #69588, #69000, #23559, .T. ) ;
#69150 = CARTESIAN_POINT ( 'NONE',  ( 86.41412918452650160, 45.91353383111829345, -8.603224342125431079 ) ) ;
#69151 = DIRECTION ( 'NONE',  ( 0.4999999999999998890, -0.8660254037844385966, 0.000000000000000000 ) ) ;
#69152 = ADVANCED_FACE ( 'NONE', ( #40758 ), #92767, .F. ) ;
#69153 = CARTESIAN_POINT ( 'NONE',  ( 163.1000353707921704, 248.1494473519441044, -11.58334223833903920 ) ) ;
#69154 = CARTESIAN_POINT ( 'NONE',  ( 82.85052922654625718, 43.48557670598759728, 7.868807238270560056 ) ) ;
#69155 = CARTESIAN_POINT ( 'NONE',  ( 150.1690433348657905, 276.5427391807701838, 3.674474410530066404 ) ) ;
#69156 = CARTESIAN_POINT ( 'NONE',  ( 15.70964071017000663, 186.0024278399160949, -9.188101187500093303 ) ) ;
#69157 = CARTESIAN_POINT ( 'NONE',  ( 118.6048046409561465, 227.0327760586659451, 1.948934522072303157E-15 ) ) ;
#69158 = CARTESIAN_POINT ( 'NONE',  ( 182.0485676003057165, 294.3143584204422609, -6.380374882051434327 ) ) ;
#69159 = CARTESIAN_POINT ( 'NONE',  ( 196.0359695149273591, 275.1637149607768151, 15.92387405639232867 ) ) ;
#69160 = CARTESIAN_POINT ( 'NONE',  ( 151.0611737675045561, 272.2621515592074388, -11.66944463701014811 ) ) ;
#69161 = CARTESIAN_POINT ( 'NONE',  ( 5.871984111234073822, 29.22396284167520619, -10.00000000000000000 ) ) ;
#69162 = AXIS2_PLACEMENT_3D ( 'NONE', #67268, #98194, #21192 ) ;
#69163 = CARTESIAN_POINT ( 'NONE',  ( 76.63628273442517980, 54.74213442968584076, -16.10156611425468753 ) ) ;
#69164 = CARTESIAN_POINT ( 'NONE',  ( -86.81108781737714253, 10.00000000000000178, 14.21260523776213347 ) ) ;
#69165 = CARTESIAN_POINT ( 'NONE',  ( 155.5204415533959548, 261.2776889444089647, 17.19127227448963424 ) ) ;
#69166 = CARTESIAN_POINT ( 'NONE',  ( 207.1770866921659717, 271.8057550155037347, -5.569195235244989384 ) ) ;
#69167 = CARTESIAN_POINT ( 'NONE',  ( 83.37296956034944628, 51.74080471427829764, 14.95189368521466733 ) ) ;
#69168 = CARTESIAN_POINT ( 'NONE',  ( 192.8228917618455398, 264.7295502452923870, 7.362112655479600143 ) ) ;
#69169 = CARTESIAN_POINT ( 'NONE',  ( 164.8677655218696430, 249.8687689424382654, -10.55778266665861409 ) ) ;
#69170 = CARTESIAN_POINT ( 'NONE',  ( 175.3859657801009178, 256.5741425621262124, -10.80191140654976500 ) ) ;
#69171 = CARTESIAN_POINT ( 'NONE',  ( 146.9456733906991417, 276.1296230653242105, -0.7988785540157754550 ) ) ;
#69172 = CARTESIAN_POINT ( 'NONE',  ( 80.84168478348897224, 44.34659258387878111, 10.38138091060227275 ) ) ;
#69173 = CARTESIAN_POINT ( 'NONE',  ( 181.2803014450269359, 265.8887025142350922, -15.50142388446617048 ) ) ;
#69174 = ORIENTED_EDGE ( 'NONE', *, *, #81415, .F. ) ;
#69175 = CARTESIAN_POINT ( 'NONE',  ( 75.25561967922160989, 63.20475890752934589, 15.17030042159924008 ) ) ;
#69176 = AXIS2_PLACEMENT_3D ( 'NONE', #37384, #54072, #69291 ) ;
#69177 = EDGE_CURVE ( 'NONE', #1290, #59347, #14288, .T. ) ;
#69178 = CARTESIAN_POINT ( 'NONE',  ( 81.91900929568903678, 41.12952449508415498, -5.442184166135863421 ) ) ;
#69179 = CARTESIAN_POINT ( 'NONE',  ( 96.60225995211651195, 217.3923013555410080, 4.594050593750050204 ) ) ;
#69180 = CARTESIAN_POINT ( 'NONE',  ( 16.06339478488542127, 14.98920272979925272, 7.433330006724137462 ) ) ;
#69181 = CARTESIAN_POINT ( 'NONE',  ( 191.2729698983822288, 299.3524933518466469, 8.871011392605806734 ) ) ;
#69182 = PLANE ( 'NONE',  #69205 ) ;
#69183 = AXIS2_PLACEMENT_3D ( 'NONE', #1727, #21641, #23112 ) ;
#69185 = CARTESIAN_POINT ( 'NONE',  ( 191.7225392387177862, 276.9339074532402947, 17.14307201408091430 ) ) ;
#69184 = CARTESIAN_POINT ( 'NONE',  ( 66.54264984482914258, 68.81226801441182772, 2.258477026830895795 ) ) ;
#69186 = DIRECTION ( 'NONE',  ( -0.8660254037844359321, -0.5000000000000051070, -0.000000000000000000 ) ) ;
#69187 = CARTESIAN_POINT ( 'NONE',  ( 150.6916211261701619, 269.6414512649903941, -15.44346024757110847 ) ) ;
#69188 = CARTESIAN_POINT ( 'NONE',  ( 23.64814127513154673, 118.0650415295851019, 45.00000000000000711 ) ) ;
#69189 = CARTESIAN_POINT ( 'NONE',  ( 34.56506555475243658, 38.14336893147758900, 7.433330006724141015 ) ) ;
#69190 = PLANE ( 'NONE',  #24057 ) ;
#69191 = FACE_BOUND ( 'NONE', #86981, .T. ) ;
#69192 = ORIENTED_EDGE ( 'NONE', *, *, #66773, .F. ) ;
#69193 = CARTESIAN_POINT ( 'NONE',  ( 31.21402144970675607, 20.94754757982090609, 5.678558825948272215 ) ) ;
#69194 = AXIS2_PLACEMENT_3D ( 'NONE', #60869, #7181, #16287 ) ;
#69195 = CARTESIAN_POINT ( 'NONE',  ( 161.9632099598195509, 257.6781890077914454, 16.87053306877513847 ) ) ;
#69196 = CARTESIAN_POINT ( 'NONE',  ( 196.7524321640172218, 268.0187694790326987, 9.426055234587533249 ) ) ;
#69197 = CARTESIAN_POINT ( 'NONE',  ( 196.5114383562724072, 290.2791998289336561, -17.87308875047256862 ) ) ;
#69198 = EDGE_CURVE ( 'NONE', #66499, #49306, #11409, .T. ) ;
#69199 = ORIENTED_EDGE ( 'NONE', *, *, #97284, .F. ) ;
#69200 = CARTESIAN_POINT ( 'NONE',  ( 84.79901702372750094, 50.05075620941028092, -13.68787013058487290 ) ) ;
#69201 = CARTESIAN_POINT ( 'NONE',  ( 83.09612612754671090, 41.63338805721024016, 5.024036258903810115 ) ) ;
#69202 = CARTESIAN_POINT ( 'NONE',  ( 183.5350908500885510, 264.5469634027678580, -13.30375932693375773 ) ) ;
#69203 = CARTESIAN_POINT ( 'NONE',  ( 169.5019237854968424, 251.7534625206462806, -8.423672671575513249 ) ) ;
#69204 = CARTESIAN_POINT ( 'NONE',  ( 30.34687108590969373, 93.06504152958497400, 60.00000000000000000 ) ) ;
#69205 = AXIS2_PLACEMENT_3D ( 'NONE', #21123, #61075, #6406 ) ;
#69206 = ORIENTED_EDGE ( 'NONE', *, *, #55649, .T. ) ;
#69207 = CARTESIAN_POINT ( 'NONE',  ( 188.1462912568056538, 279.3216201851784035, 16.80002852650974177 ) ) ;
#69208 = CARTESIAN_POINT ( 'NONE',  ( 38.91320803870388545, 23.26216523072497466, -2.296566073217252530E-15 ) ) ;
#69209 = ORIENTED_EDGE ( 'NONE', *, *, #7852, .F. ) ;
#69210 = CARTESIAN_POINT ( 'NONE',  ( 167.6205390402564603, 249.8818047244939180, 6.913440952512820203 ) ) ;
#69211 = CARTESIAN_POINT ( 'NONE',  ( 185.1680939005084383, 292.9008939279111132, -10.44728957843394568 ) ) ;
#69212 = ORIENTED_EDGE ( 'NONE', *, *, #21787, .T. ) ;
#69213 = CARTESIAN_POINT ( 'NONE',  ( 86.48586980954701176, 47.12904147948177069, -10.06668187157390904 ) ) ;
#69214 = CARTESIAN_POINT ( 'NONE',  ( -76.38857681351474582, 54.22815603855766398, 10.00000000000000000 ) ) ;
#69215 = CARTESIAN_POINT ( 'NONE',  ( 84.62070576355738183, 50.25222463068733703, 13.86530520652494758 ) ) ;
#69216 = CARTESIAN_POINT ( 'NONE',  ( 192.7871527781657335, 296.7298516721106694, -12.00364781672877434 ) ) ;
#69217 = CARTESIAN_POINT ( 'NONE',  ( 185.9800042062175862, 295.3878514961374435, 9.780988852953662160 ) ) ;
#69218 = ADVANCED_FACE ( 'NONE', ( #65079 ), #77386, .F. ) ;
#69219 = DIRECTION ( 'NONE',  ( -0.8660254037844387076, -0.4999999999999998890, -0.000000000000000000 ) ) ;
#69220 = CARTESIAN_POINT ( 'NONE',  ( 110.3297989853572005, 246.0530062829863311, -4.648177544792955347E-16 ) ) ;
#69221 = CARTESIAN_POINT ( 'NONE',  ( 79.98969732019267553, 44.69009452991755893, 11.16475366590057483 ) ) ;
#69222 = CARTESIAN_POINT ( 'NONE',  ( 81.29586503113306151, 55.42867650357229081, -16.33480133305122095 ) ) ;
#69223 = CARTESIAN_POINT ( 'NONE',  ( 72.37973851903267075, 63.38476940627418799, -14.36017998060057721 ) ) ;
#69224 = ORIENTED_EDGE ( 'NONE', *, *, #26318, .F. ) ;
#69225 = DIRECTION ( 'NONE',  ( 0.4999999999999998890, -0.8660254037844385966, 0.000000000000000000 ) ) ;
#69226 = ORIENTED_EDGE ( 'NONE', *, *, #14087, .T. ) ;
#69227 = ORIENTED_EDGE ( 'NONE', *, *, #90513, .T. ) ;
#69228 = CARTESIAN_POINT ( 'NONE',  ( 87.07436038242185816, 45.84038486297258430, -8.630882807222770126 ) ) ;
#69230 = CARTESIAN_POINT ( 'NONE',  ( 185.3903474297596290, 282.1509521980658519, -17.39533353848089448 ) ) ;
#69229 = CARTESIAN_POINT ( 'NONE',  ( 170.7208318451582443, 255.3949681855457925, -11.45774138149006660 ) ) ;
#69231 = CARTESIAN_POINT ( 'NONE',  ( 80.32560484147226987, 44.93948968179056180, -11.21518412823304800 ) ) ;
#69232 = CARTESIAN_POINT ( 'NONE',  ( 67.53167658295855347, 67.09922345392760690, 8.942594108559751120 ) ) ;
#69233 = CARTESIAN_POINT ( 'NONE',  ( 71.72451190509423213, 61.77407603521598389, -14.41855241212332750 ) ) ;
#69234 = CARTESIAN_POINT ( 'NONE',  ( 79.16903247652662401, 46.12461580907955749, 12.66491118591851972 ) ) ;
#69235 = VECTOR ( 'NONE', #82336, 1000.000000000000114 ) ;
#69236 = LINE ( 'NONE', #93575, #44650 ) ;
#69237 = CARTESIAN_POINT ( 'NONE',  ( 77.13937272485186725, 63.60852409164084520, -15.03876710342725076 ) ) ;
#69238 = CARTESIAN_POINT ( 'NONE',  ( 178.0352283463558081, 255.4622352572455384, 5.186437070723915355 ) ) ;
#69239 = CARTESIAN_POINT ( 'NONE',  ( 110.4040191812834735, 243.7369531367911009, -4.594050593750048428 ) ) ;
#69240 = CARTESIAN_POINT ( 'NONE',  ( 186.6446422895439525, 262.8178198450582386, -9.153827383837436216 ) ) ;
#69241 = CARTESIAN_POINT ( 'NONE',  ( 43.45144817956826699, 30.80170272979930601, 7.433330006724137462 ) ) ;
#69242 = CARTESIAN_POINT ( 'NONE',  ( 188.8854333635352134, 273.8291574995095630, 15.67551265882508815 ) ) ;
#69243 = AXIS2_PLACEMENT_3D ( 'NONE', #96998, #81786, #34645 ) ;
#69244 = ORIENTED_EDGE ( 'NONE', *, *, #52083, .T. ) ;
#69245 = CIRCLE ( 'NONE', #93583, 17.82106496071138935 ) ;
#69246 = CARTESIAN_POINT ( 'NONE',  ( 86.87376599001147781, 45.86940958085830999, -8.177027763546412586 ) ) ;
#69247 = CARTESIAN_POINT ( 'NONE',  ( 70.21756736500132945, 64.16742292537257697, -12.57977312374782919 ) ) ;
#69248 = CARTESIAN_POINT ( 'NONE',  ( -13.79761285583127872, 128.9229902121449811, 8.559299291603829198E-14 ) ) ;
#69249 = CARTESIAN_POINT ( 'NONE',  ( 192.8406302823137821, 296.6372259178641002, 11.87010547645091663 ) ) ;
#69250 = CARTESIAN_POINT ( 'NONE',  ( 72.68991634181023187, 64.30301886947491141, 13.46146812301844164 ) ) ;
#69251 = CARTESIAN_POINT ( 'NONE',  ( 201.4066285247549786, 281.8004817444100354, -17.79749223817309201 ) ) ;
#69252 = LINE ( 'NONE', #44453, #80401 ) ;
#69253 = ORIENTED_EDGE ( 'NONE', *, *, #8988, .F. ) ;
#69254 = CARTESIAN_POINT ( 'NONE',  ( 48.73804053012793247, 107.9864336245683631, 177.5919119679930134 ) ) ;
#69255 = CIRCLE ( 'NONE', #51472, 70.00000000000001421 ) ;
#69256 = ORIENTED_EDGE ( 'NONE', *, *, #18130, .T. ) ;
#69257 = CARTESIAN_POINT ( 'NONE',  ( 79.38841588403847993, 49.82580522342896501, 15.10957065665274257 ) ) ;
#69258 = DIRECTION ( 'NONE',  ( -1.000000000000000000, -1.156482317317871331E-15, 0.000000000000000000 ) ) ;
#69259 = ORIENTED_EDGE ( 'NONE', *, *, #86564, .F. ) ;
#69260 = CARTESIAN_POINT ( 'NONE',  ( 189.4404814790326839, 266.9389309148366465, -11.88803597182145033 ) ) ;
#69261 = AXIS2_PLACEMENT_3D ( 'NONE', #47006, #32303, #16107 ) ;
#69262 = CARTESIAN_POINT ( 'NONE',  ( 151.9683803660127808, 267.4300393925500998, -16.94882632825642332 ) ) ;
#69263 = CARTESIAN_POINT ( 'NONE',  ( -4.759057006084864483, 161.3927522451417929, -10.00000000000009237 ) ) ;
#69264 = CARTESIAN_POINT ( 'NONE',  ( 81.71431622648833581, 43.56938202975830166, 8.897122998445636810 ) ) ;
#69266 = CARTESIAN_POINT ( 'NONE',  ( 156.8251583690820894, 280.2372100051578627, 5.906658021487110943 ) ) ;
#69265 = CARTESIAN_POINT ( 'NONE',  ( 198.1641410069890696, 286.1601526949679055, 17.43024458236784824 ) ) ;
#69267 = CARTESIAN_POINT ( 'NONE',  ( 153.0444155045374544, 265.5662918618958201, -16.15173036748435109 ) ) ;
#69268 = ORIENTED_EDGE ( 'NONE', *, *, #83228, .F. ) ;
#69269 = CARTESIAN_POINT ( 'NONE',  ( 190.9380839614473473, 299.9325328093580652, -5.232187664503159752 ) ) ;
#69271 = CARTESIAN_POINT ( 'NONE',  ( 72.66276004730617899, 66.52099816311097413, 11.94923289124634103 ) ) ;
#69270 = B_SPLINE_SURFACE_WITH_KNOTS ( 'NONE', 3, 1, ( 
 ( #59121, #51039 ),
 ( #44931, #13075 ),
 ( #81996, #29748 ),
 ( #83993, #75370 ),
 ( #60620, #29258 ),
 ( #45432, #75878 ),
 ( #5951, #37828 ),
 ( #21171, #12569 ),
 ( #68736, #43444 ),
 ( #74387, #91575 ),
 ( #74875, #67753 ),
 ( #35852, #20662 ),
 ( #51551, #43936 ),
 ( #36844, #5458 ),
 ( #98174, #59632 ),
 ( #52052, #98677 ),
 ( #60126, #55027 ),
 ( #32734, #39313 ),
 ( #47923, #16534 ),
 ( #8940, #77344 ),
 ( #24142, #17030 ),
 ( #76836, #62620 ),
 ( #86008, #15026 ),
 ( #32235, #23124 ),
 ( #30750, #8444 ),
 ( #93573, #7434 ),
 ( #71258, #39806 ),
 ( #38327, #84484 ),
 ( #15519, #339 ),
 ( #47431, #31230 ),
 ( #70230, #85489 ) ),
 .UNSPECIFIED., .F., .F., .F.,
 ( 4, 3, 3, 3, 3, 3, 3, 3, 3, 3, 4 ),
 ( 2, 2 ),
 ( 0.000000000000000000, 0.1122669598086814685, 0.2243161639709671529, 0.3396355846219190067, 0.4553962076585229557, 0.5677860799922529456, 0.6749047109689662038, 0.7773884377078499330, 0.8775581155834387692, 0.9782364162377882311, 1.000000000000000000 ),
 ( 0.000000000000000000, 1.000000000000000000 ),
 .UNSPECIFIED. ) ;
#69272 = CARTESIAN_POINT ( 'NONE',  ( 72.31501564753065736, 60.31777401518989024, 15.59333315930887309 ) ) ;
#69273 = CARTESIAN_POINT ( 'NONE',  ( 148.6176504468695896, 246.6115022471902023, -5.000000000000041744 ) ) ;
#69274 = CARTESIAN_POINT ( 'NONE',  ( 192.0969986600162827, 271.0201763999182845, -15.22553433325905736 ) ) ;
#69275 = EDGE_CURVE ( 'NONE', #19179, #96323, #10901, .T. ) ;
#69276 = CARTESIAN_POINT ( 'NONE',  ( 187.9556972102613486, 298.1788374127830252, -4.259537494478616182 ) ) ;
#69277 = CARTESIAN_POINT ( 'NONE',  ( 31.43297906638544603, 41.08080186712595605, -3.090169943749475845 ) ) ;
#69278 = ADVANCED_FACE ( 'NONE', ( #4793 ), #15062, .T. ) ;
#69279 = FACE_OUTER_BOUND ( 'NONE', #48941, .T. ) ;
#69280 = CARTESIAN_POINT ( 'NONE',  ( 191.2600711594267011, 283.4582610259524813, -16.58647876252101838 ) ) ;
#69281 = AXIS2_PLACEMENT_3D ( 'NONE', #33342, #94182, #87621 ) ;
#69282 = CARTESIAN_POINT ( 'NONE',  ( 72.93270222632347100, 70.75261854202813083, -7.421515863126944446 ) ) ;
#69283 = EDGE_CURVE ( 'NONE', #43244, #12691, #82503, .T. ) ;
#69284 = CARTESIAN_POINT ( 'NONE',  ( 69.26781250152264136, 219.9869531367911293, 4.594050593750046652 ) ) ;
#69285 = CARTESIAN_POINT ( 'NONE',  ( 67.43966565062764573, 66.61250739341410565, 8.643685538913882027 ) ) ;
#69286 = CARTESIAN_POINT ( 'NONE',  ( 147.2658550951450422, 275.5750520855697800, -5.215660180131691526 ) ) ;
#69287 = DIRECTION ( 'NONE',  ( 0.4924038765061026779, -0.8528685319524446085, -0.1736481776669273058 ) ) ;
#69288 = EDGE_CURVE ( 'NONE', #749, #21377, #13229, .T. ) ;
#69289 = CARTESIAN_POINT ( 'NONE',  ( 203.1044072055706806, 278.8598428092302584, -16.67109798570195878 ) ) ;
#69290 = CARTESIAN_POINT ( 'NONE',  ( 161.8150574665248200, 250.3750943687383881, -13.25074899737357903 ) ) ;
#69291 = DIRECTION ( 'NONE',  ( 0.4999999999999998890, -0.8660254037844385966, 0.000000000000000000 ) ) ;
#69292 = CARTESIAN_POINT ( 'NONE',  ( 20.88255934282640425, 35.55466486950700755, -1.111400068045478839E-16 ) ) ;
#69294 = CARTESIAN_POINT ( 'NONE',  ( 76.48813647825510031, 51.17232029059452714, 16.04681448753369821 ) ) ;
#69293 = DIRECTION ( 'NONE',  ( 0.4999999999999998890, -0.8660254037844385966, 0.000000000000000000 ) ) ;
#69295 = CARTESIAN_POINT ( 'NONE',  ( 1.830000459568766003, 24.55466486950697202, 1.000260061240931054E-15 ) ) ;
#69296 = CARTESIAN_POINT ( 'NONE',  ( 165.9646868419130215, 249.3316235501012272, -9.227677147359839793 ) ) ;
#69297 = CARTESIAN_POINT ( 'NONE',  ( 204.8103939599436387, 275.9049870736169510, -13.21557707437574081 ) ) ;
#69298 = CARTESIAN_POINT ( 'NONE',  ( 157.8849654228661166, 257.1822134667773980, 17.43614750057631468 ) ) ;
#69299 = DIRECTION ( 'NONE',  ( -0.8660254037844369313, -0.5000000000000029976, -0.000000000000000000 ) ) ;
#69300 = CARTESIAN_POINT ( 'NONE',  ( 23.50386934422995822, 190.5024278399160949, -9.188101187500093303 ) ) ;
#69301 = B_SPLINE_CURVE_WITH_KNOTS ( 'NONE', 3,
 ( #74820, #35791, #21115, #29688 ),
 .UNSPECIFIED., .F., .F.,
 ( 4, 4 ),
 ( 0.01230808397153141873, 0.01852871432776161467 ),
 .UNSPECIFIED. ) ;
#69302 = AXIS2_PLACEMENT_3D ( 'NONE', #3624, #58294, #18817 ) ;
#69303 = CARTESIAN_POINT ( 'NONE',  ( 51.40603854846860798, 209.6744531367911293, 4.594050593750047540 ) ) ;
#69304 = CARTESIAN_POINT ( 'NONE',  ( 195.6914848190668863, 279.7035040353765680, -17.46620344769279853 ) ) ;
#69305 = CARTESIAN_POINT ( 'NONE',  ( 88.12195951149128348, 43.65269896049575493, 0.1370767085644951921 ) ) ;
#69306 = VECTOR ( 'NONE', #55716, 1000.000000000000227 ) ;
#69307 = CARTESIAN_POINT ( 'NONE',  ( 44.47956695515382108, 64.36960560548604349, -10.00000000000000000 ) ) ;
#69308 = CARTESIAN_POINT ( 'NONE',  ( -7.266922234329370234, 156.6115022471902023, -5.000000000000041744 ) ) ;
#69309 = DIRECTION ( 'NONE',  ( 0.4999999999999992784, -0.8660254037844390407, 0.000000000000000000 ) ) ;
#69310 = CIRCLE ( 'NONE', #96919, 0.1418229129680863287 ) ;
#69311 = CARTESIAN_POINT ( 'NONE',  ( 196.3531314006455091, 269.5910805997556849, -10.80433586473562713 ) ) ;
#69312 = CARTESIAN_POINT ( 'NONE',  ( 23.42942861845947178, 22.03085787977763133, 9.188101187500006262 ) ) ;
#69313 = CARTESIAN_POINT ( 'NONE',  ( 198.5201458116119397, 286.8000164587433005, -18.30276554821096013 ) ) ;
#69314 = CARTESIAN_POINT ( 'NONE',  ( -79.28667360730979397, 56.40661347651924729, -10.00000000000000000 ) ) ;
#69315 = CARTESIAN_POINT ( 'NONE',  ( 15.46199490364264406, 17.43085787977761925, -9.188101187500008038 ) ) ;
#69316 = CARTESIAN_POINT ( 'NONE',  ( 66.64328041388984047, 197.0327760586659736, 1.948934522072302763E-15 ) ) ;
#69317 = CARTESIAN_POINT ( 'NONE',  ( 76.80413851785759505, 63.68367294747309870, 15.32454931363362149 ) ) ;
#69318 = CARTESIAN_POINT ( 'NONE',  ( 78.24536471662285919, 58.27182448786981439, -16.57828156733082636 ) ) ;
#69319 = VECTOR ( 'NONE', #11814, 1000.000000000000000 ) ;
#69320 = CARTESIAN_POINT ( 'NONE',  ( 160.0105735053945182, 253.5005522708592594, 16.10371386499367929 ) ) ;
#69321 = CARTESIAN_POINT ( 'NONE',  ( 69.61542750552385428, 62.56132062511080250, -13.94275833699888345 ) ) ;
#69322 = CARTESIAN_POINT ( 'NONE',  ( 149.1930131096921457, 275.4191784524399509, 7.566393461087619343 ) ) ;
#69323 = CARTESIAN_POINT ( 'NONE',  ( 156.1857201963304362, 277.6936791020598889, 10.39727624116721749 ) ) ;
#69324 = VECTOR ( 'NONE', #72522, 1000.000000000000000 ) ;
#69325 = CARTESIAN_POINT ( 'NONE',  ( 112.6775961898153184, 245.8615022471903160, 5.000000000000046185 ) ) ;
#69326 = CARTESIAN_POINT ( 'NONE',  ( 200.2316334480823912, 283.8356329158505105, 17.02791935830326508 ) ) ;
#69327 = CARTESIAN_POINT ( 'NONE',  ( 207.0200405408487541, 272.0777669287182334, 6.494273599193515878 ) ) ;
#69328 = EDGE_LOOP ( 'NONE', ( #41166, #74149, #44328, #61257, #15249, #21912, #40557, #41314, #78885, #11197, #46414, #43927, #73664, #76755, #40077, #14655, #17531, #5188, #78344, #8611, #10457 ) ) ;
#69329 = CARTESIAN_POINT ( 'NONE',  ( 76.91550034648578560, 49.81933278187382541, 15.10848294682921811 ) ) ;
#69330 = CARTESIAN_POINT ( 'NONE',  ( 82.56035143084491779, 53.86840602817221679, 15.84327991562212112 ) ) ;
#69331 = ORIENTED_EDGE ( 'NONE', *, *, #13294, .F. ) ;
#69332 = CARTESIAN_POINT ( 'NONE',  ( 206.8106726053982811, 272.4404028303941914, -10.47827087991598560 ) ) ;
#69333 = CARTESIAN_POINT ( 'NONE',  ( 186.9505214435809251, 276.6852383206837658, -16.96231179040420400 ) ) ;
#69334 = DIRECTION ( 'NONE',  ( -1.000000000000000000, 0.000000000000000000, 0.000000000000000000 ) ) ;
#69335 = ORIENTED_EDGE ( 'NONE', *, *, #25612, .F. ) ;
#69336 = ORIENTED_EDGE ( 'NONE', *, *, #87410, .T. ) ;
#69337 = CARTESIAN_POINT ( 'NONE',  ( 79.11200284437833830, 46.21030595555048137, -12.74531297726273316 ) ) ;
#69338 = CARTESIAN_POINT ( 'NONE',  ( 147.9500839974939197, 274.3899328626944225, -9.375093207164509224 ) ) ;
#69339 = FACE_OUTER_BOUND ( 'NONE', #45350, .T. ) ;
#69340 = EDGE_CURVE ( 'NONE', #81649, #31700, #40997, .T. ) ;
#69341 = AXIS2_PLACEMENT_3D ( 'NONE', #27332, #73438, #65806 ) ;
#69342 = ORIENTED_EDGE ( 'NONE', *, *, #97668, .T. ) ;
#69343 = CARTESIAN_POINT ( 'NONE',  ( 16.91979795264450459, 27.95586893147755347, 7.433330006724141015 ) ) ;
#69344 = CARTESIAN_POINT ( 'NONE',  ( 75.64215183828173394, 57.94545888253220767, 16.05204495045250468 ) ) ;
#69345 = DIRECTION ( 'NONE',  ( -0.8035972437015875824, -0.5951734788405910193, 0.000000000000000000 ) ) ;
#69346 = CARTESIAN_POINT ( 'NONE',  ( -59.87889494062799400, 37.30571521936384016, -10.00000000000000000 ) ) ;
#69347 = EDGE_LOOP ( 'NONE', ( #69824, #13692, #82486, #86279, #984, #74239 ) ) ;
#69348 = DIRECTION ( 'NONE',  ( -0.000000000000000000, -1.000000000000000000, -0.000000000000000000 ) ) ;
#69349 = CARTESIAN_POINT ( 'NONE',  ( 161.9146335138334507, 283.9927115759381877, 5.150495195206919341 ) ) ;
#69350 = ORIENTED_EDGE ( 'NONE', *, *, #68581, .F. ) ;
#69351 = CARTESIAN_POINT ( 'NONE',  ( 171.0410219469655999, 285.1196576716371851, 11.19351320761253099 ) ) ;
#69353 = CARTESIAN_POINT ( 'NONE',  ( 67.91860044382929118, 65.38732574981587220, -10.41618022401985755 ) ) ;
#69352 = CARTESIAN_POINT ( 'NONE',  ( 163.2409074158086639, 283.7204879113825768, -3.084300225432008435 ) ) ;
#69354 = CARTESIAN_POINT ( 'NONE',  ( 208.3682389855799499, 269.7426187237583690, -1.431169231381201890 ) ) ;
#69355 = CARTESIAN_POINT ( 'NONE',  ( 204.4781092559247782, 276.4805210635553863, 13.30606382016679490 ) ) ;
#69356 = CARTESIAN_POINT ( 'NONE',  ( 159.6419305724666344, 254.1390605605417079, 16.92015248457581933 ) ) ;
#69357 = CARTESIAN_POINT ( 'NONE',  ( 205.3704330671644414, 274.9349708856848338, -13.01557521325596944 ) ) ;
#69358 = EDGE_CURVE ( 'NONE', #27245, #31851, #20972, .T. ) ;
#69359 = CARTESIAN_POINT ( 'NONE',  ( 140.0928864244750685, 245.5643266524160424, -9.188101187500093303 ) ) ;
#69360 = CARTESIAN_POINT ( 'NONE',  ( 176.8005402467339024, 269.1829579716712715, 16.10165660169349877 ) ) ;
#69361 = CARTESIAN_POINT ( 'NONE',  ( 178.7083948068321888, 257.8228082974438848, 9.925691156843040375 ) ) ;
#69362 = CARTESIAN_POINT ( 'NONE',  ( 73.67938972387338481, 213.3458772461660544, 9.188101187500095079 ) ) ;
#69363 = ORIENTED_EDGE ( 'NONE', *, *, #27630, .T. ) ;
#69364 = CARTESIAN_POINT ( 'NONE',  ( 150.8167050463783312, 269.4247995599803289, 14.38040671671637938 ) ) ;
#69365 = CARTESIAN_POINT ( 'NONE',  ( 79.11275361910446691, 46.11146926033848104, 13.27945046499836579 ) ) ;
#69366 = ORIENTED_EDGE ( 'NONE', *, *, #6493, .F. ) ;
#69367 = CARTESIAN_POINT ( 'NONE',  ( 156.8626719559046876, 258.9528776918004382, -16.97501551230912042 ) ) ;
#69368 = ORIENTED_EDGE ( 'NONE', *, *, #58367, .F. ) ;
#69369 = ORIENTED_EDGE ( 'NONE', *, *, #4322, .F. ) ;
#69370 = CARTESIAN_POINT ( 'NONE',  ( 186.6673878995319455, 276.5074556901925007, 17.73048906045012529 ) ) ;
#69371 = CARTESIAN_POINT ( 'NONE',  ( 66.97748580458319623, 68.05911003915983315, 6.908000617419038036 ) ) ;
#69372 = CARTESIAN_POINT ( 'NONE',  ( 197.8876559304677585, 286.9678159391793884, 16.93603806477735318 ) ) ;
#69373 = CARTESIAN_POINT ( 'NONE',  ( -32.94356256989597398, 95.08348788047962330, 10.71240442958353256 ) ) ;
#69374 = DIRECTION ( 'NONE',  ( 0.000000000000000000, -0.000000000000000000, 1.000000000000000000 ) ) ;
#69375 = CARTESIAN_POINT ( 'NONE',  ( 155.5770330754656072, 261.1796695529068302, 18.26969263326161297 ) ) ;
#69376 = CARTESIAN_POINT ( 'NONE',  ( 70.78021245458822364, 64.95631462881182472, 12.26071011676762978 ) ) ;
#69377 = CARTESIAN_POINT ( 'NONE',  ( 78.41572647264329987, 206.8923013555409796, 4.594050593750050204 ) ) ;
#69378 = ORIENTED_EDGE ( 'NONE', *, *, #879, .T. ) ;
#69379 = ADVANCED_BREP_SHAPE_REPRESENTATION ( '', ( #76056, #68784 ), #31602 ) ;
#69380 = ORIENTED_EDGE ( 'NONE', *, *, #5342, .T. ) ;
#69381 = CARTESIAN_POINT ( 'NONE',  ( 201.0887433138568667, 282.3510750806604506, -17.79223670182895845 ) ) ;
#69382 = AXIS2_PLACEMENT_3D ( 'NONE', #25361, #55734, #79106 ) ;
#69383 = VERTEX_POINT ( 'NONE', #10773 ) ;
#69384 = CARTESIAN_POINT ( 'NONE',  ( 83.70099988003033786, 41.63496273699991690, 0.2210104254450260541 ) ) ;
#69385 = CARTESIAN_POINT ( 'NONE',  ( 183.6431167994092561, 275.7377679000179569, 17.10282768236007556 ) ) ;
#69386 = VECTOR ( 'NONE', #49013, 1000.000000000000227 ) ;
#69387 = CARTESIAN_POINT ( 'NONE',  ( 205.8610808625997208, 274.0851439753691920, 10.38803237360972531 ) ) ;
#69388 = CARTESIAN_POINT ( 'NONE',  ( 165.5245226950644053, 285.3287233769559066, 0.5282479373057951122 ) ) ;
#69389 = CARTESIAN_POINT ( 'NONE',  ( 179.4037581149374034, 257.9870511612666064, -10.76565914641300736 ) ) ;
#69390 = CARTESIAN_POINT ( 'NONE',  ( 154.7243163084728792, 268.4101332538514839, -16.32114699749692477 ) ) ;
#69391 = AXIS2_PLACEMENT_3D ( 'NONE', #88916, #41732, #40217 ) ;
#69392 = ORIENTED_EDGE ( 'NONE', *, *, #66771, .T. ) ;
#69393 = CARTESIAN_POINT ( 'NONE',  ( 188.7422858333208069, 294.9179404709084906, 11.58253606622573706 ) ) ;
#69394 = CARTESIAN_POINT ( 'NONE',  ( 156.9440562780969231, 274.4750137900673508, 13.77464823823377316 ) ) ;
#69395 = CARTESIAN_POINT ( 'NONE',  ( 37.50785463075374793, 23.78380873178789656, -6.180339887498949025 ) ) ;
#69396 = CARTESIAN_POINT ( 'NONE',  ( 200.7134601498536028, 283.0010845879393742, -16.98649239173277792 ) ) ;
#69397 = CARTESIAN_POINT ( 'NONE',  ( 72.60240557621898461, 70.90654587215668414, 7.620139211458048401 ) ) ;
#69398 = CARTESIAN_POINT ( 'NONE',  ( 74.27291791270538113, 66.59407379392037285, -12.66298293614721970 ) ) ;
#69399 = ORIENTED_EDGE ( 'NONE', *, *, #44174, .F. ) ;
#69400 = CARTESIAN_POINT ( 'NONE',  ( 195.7220586188342111, 265.4108606537332662, 4.484546202810920867 ) ) ;
#69401 = CIRCLE ( 'NONE', #90507, 0.1418229129681522482 ) ;
#69402 =( BOUNDED_CURVE ( )  B_SPLINE_CURVE ( 2, ( #32297, #63200, #23189, #47987, #63702, #9520, #40380, #1912, #94638 ),
 .UNSPECIFIED., .F., .T. ) 
 B_SPLINE_CURVE_WITH_KNOTS ( ( 3, 2, 2, 2, 3 ),
 ( 0.01209677419354838850, 0.01344086021505376365, 0.01612903225806451568, 0.01881720430107526945, 0.02016129032258064807 ),
 .UNSPECIFIED. ) 
 CURVE ( )  GEOMETRIC_REPRESENTATION_ITEM ( )  RATIONAL_B_SPLINE_CURVE ( ( 0.9330127018922194093, 0.9330127018922194093, 1.000000000000000000, 0.8660254037844387076, 1.000000000000000000, 0.8660254037844387076, 1.000000000000000000, 0.9330127018922191873, 0.9330127018922192983 ) ) 
 REPRESENTATION_ITEM ( '' )  );
#69403 = CARTESIAN_POINT ( 'NONE',  ( 181.5502188866845756, 292.0258448067215795, 10.54796749914566334 ) ) ;
#69404 = CARTESIAN_POINT ( 'NONE',  ( 20.85854946042532276, 194.3967562850347122, -4.648177544792955347E-16 ) ) ;
#69405 = CARTESIAN_POINT ( 'NONE',  ( 79.95853045724066988, 47.67161661237850723, 13.37152120557419543 ) ) ;
#69406 = CARTESIAN_POINT ( 'NONE',  ( 84.02300986820688422, 51.73893231647484470, 14.78971152351953222 ) ) ;
#69407 = CARTESIAN_POINT ( 'NONE',  ( 154.4723046951263825, 270.8738626539015968, 14.00925342371585636 ) ) ;
#69408 = ADVANCED_FACE ( 'NONE', ( #34555 ), #40644, .T. ) ;
#69409 = B_SPLINE_CURVE_WITH_KNOTS ( 'NONE', 3,
 ( #58514, #89486, #20046, #50917, #35726, #81867, #66625, #2861, #95593, #18546, #49427, #51422 ),
 .UNSPECIFIED., .F., .F.,
 ( 4, 2, 2, 2, 2, 4 ),
 ( 0.001587444564573364542, 0.001666700333226233842, 0.001745956101879103358, 0.001904467639184939535, 0.002221490713796634223, 0.002855536863020023165 ),
 .UNSPECIFIED. ) ;
#69410 = EDGE_LOOP ( 'NONE', ( #59936, #20181, #26538, #21016 ) ) ;
#69411 = CARTESIAN_POINT ( 'NONE',  ( 147.3984236761635884, 275.3454365677582700, 5.108566646342994844 ) ) ;
#69412 = CARTESIAN_POINT ( 'NONE',  ( 162.6626107288841467, 248.9070890562113902, 10.12509462564867313 ) ) ;
#69413 = CARTESIAN_POINT ( 'NONE',  ( 207.4285356523023154, 271.3702326410368642, 7.833982582429932506 ) ) ;
#69415 = CARTESIAN_POINT ( 'NONE',  ( 74.13069305858248015, 55.11053013652369259, 16.60422064088523442 ) ) ;
#69414 = CARTESIAN_POINT ( 'NONE',  ( 194.2764122224708103, 294.1503786489221284, 15.46903869661980835 ) ) ;
#69416 = CARTESIAN_POINT ( 'NONE',  ( 20.62524822163506144, 36.00034080476291365, -1.878358725466461243E-16 ) ) ;
#69417 = CARTESIAN_POINT ( 'NONE',  ( 170.8843335314017509, 274.4719442773359219, 17.28596511953734449 ) ) ;
#69418 = CARTESIAN_POINT ( 'NONE',  ( 163.2786353882781327, 283.8196446749163329, -3.634902129664387527 ) ) ;
#69419 = LINE ( 'NONE', #30916, #71179 ) ;
#69420 = CYLINDRICAL_SURFACE ( 'NONE', #78636, 17.82106496071139645 ) ;
#69421 = CARTESIAN_POINT ( 'NONE',  ( 151.1255156751140873, 251.3927522451417929, -10.00000000000009059 ) ) ;
#69422 = LINE ( 'NONE', #54702, #72758 ) ;
#69423 = ORIENTED_EDGE ( 'NONE', *, *, #49069, .F. ) ;
#69424 = CARTESIAN_POINT ( 'NONE',  ( 66.86435824960236118, 68.17012062228093328, -6.563951195314443154 ) ) ;
#69425 = CARTESIAN_POINT ( 'NONE',  ( 72.86910405259970958, 71.04354916989079527, -7.648857478963554613 ) ) ;
#69426 = FACE_OUTER_BOUND ( 'NONE', #7783, .T. ) ;
#69427 = CARTESIAN_POINT ( 'NONE',  ( 23.17910981781079371, 190.3149278399160949, -9.188101187500095079 ) ) ;
#69428 = CARTESIAN_POINT ( 'NONE',  ( 176.1700939719127064, 265.6259258544362751, -16.05018850396762176 ) ) ;
#69429 = CARTESIAN_POINT ( 'NONE',  ( 32.29641253342593643, 23.81029122506296503, 8.090169943749479842 ) ) ;
#69430 = CARTESIAN_POINT ( 'NONE',  ( 77.02919517786544645, 53.03642993313334841, 16.34676611183340356 ) ) ;
#69431 = CARTESIAN_POINT ( 'NONE',  ( 72.26538907532096800, 200.9824982072973967, 3.021315404115420679E-15 ) ) ;
#69432 = DIRECTION ( 'NONE',  ( 0.8503781557569334293, -0.05328141121994506291, -0.5234673661555683255 ) ) ;
#69433 = CARTESIAN_POINT ( 'NONE',  ( 81.89930626873778863, 42.21375885382297355, 7.647715624843501203 ) ) ;
#69434 = CARTESIAN_POINT ( 'NONE',  ( 84.06604358195920668, 51.46910565605918464, 14.65639964578790710 ) ) ;
#69435 = CARTESIAN_POINT ( 'NONE',  ( 71.90223342829800401, 218.9865022471902876, -10.00000000000009415 ) ) ;
#69436 = CARTESIAN_POINT ( 'NONE',  ( 81.89117822404196545, 41.17241246689844303, 5.587214106818517934 ) ) ;
#69437 = LINE ( 'NONE', #59324, #59532 ) ;
#69438 = CARTESIAN_POINT ( 'NONE',  ( 29.24128764430186322, 193.8149278399160664, 9.188101187500093303 ) ) ;
#69439 = CARTESIAN_POINT ( 'NONE',  ( 72.44129552685039641, 70.67501955208014408, -7.848061272651214004 ) ) ;
#69440 = CARTESIAN_POINT ( 'NONE',  ( 36.10619739613039769, 52.83927550304669296, -10.00000000000000000 ) ) ;
#69441 = CARTESIAN_POINT ( 'NONE',  ( 77.13184676329899503, 49.35096920870304871, -14.90321232162610521 ) ) ;
#69442 = CARTESIAN_POINT ( 'NONE',  ( 198.9832789858017463, 285.9978462703757600, -18.55676541969546278 ) ) ;
#69443 = CARTESIAN_POINT ( 'NONE',  ( 164.9779129355220562, 244.8968679994381148, -1.771286574179712803 ) ) ;
#69444 = CARTESIAN_POINT ( 'NONE',  ( 155.2695601165254402, 261.7122283397445131, 16.98599069618989077 ) ) ;
#69445 = CARTESIAN_POINT ( 'NONE',  ( 185.2204453182458508, 266.7228424648479859, 14.18578268008576337 ) ) ;
#69446 = CARTESIAN_POINT ( 'NONE',  ( 161.3305864230751183, 279.4054883986951836, -9.803368587617336871 ) ) ;
#69447 = CARTESIAN_POINT ( 'NONE',  ( 179.7260286473791666, 262.9842352772275262, -13.04977194216664849 ) ) ;
#69448 = PRODUCT_CONTEXT ( 'NONE', #56961, 'mechanical' ) ;
#69449 = CARTESIAN_POINT ( 'NONE',  ( 22.57541804695699028, 15.96004757982090183, -5.678558825948276656 ) ) ;
#69450 = CARTESIAN_POINT ( 'NONE',  ( 15.56473500984127512, 9.390406791769814632, -7.779800476318352071E-15 ) ) ;
#69451 = CARTESIAN_POINT ( 'NONE',  ( 71.77793909028444830, 59.04410539788438683, 15.86942587573766517 ) ) ;
#69452 = EDGE_CURVE ( 'NONE', #86705, #43553, #89318, .T. ) ;
#69453 = FACE_OUTER_BOUND ( 'NONE', #85104, .T. ) ;
#69454 = ORIENTED_EDGE ( 'NONE', *, *, #63101, .F. ) ;
#69455 = VECTOR ( 'NONE', #25457, 1000.000000000000000 ) ;
#69456 = CARTESIAN_POINT ( 'NONE',  ( 30.96785900501025424, 44.34188169337050311, 10.00000000000000000 ) ) ;
#69457 = CARTESIAN_POINT ( 'NONE',  ( 76.04865552100373804, 58.90167082828886436, -15.97767159145053739 ) ) ;
#69458 = CARTESIAN_POINT ( 'NONE',  ( 4.831432983919195401, 162.0494855054052152, -2.679491924311248496 ) ) ;
#69459 = CARTESIAN_POINT ( 'NONE',  ( 155.7716105177659927, 262.8426515368366267, -17.72795275872529430 ) ) ;
#69460 = ORIENTED_EDGE ( 'NONE', *, *, #4322, .T. ) ;
#69461 = CARTESIAN_POINT ( 'NONE',  ( 25.61604267474572083, 174.0494855054051584, -2.679491924311248496 ) ) ;
#69462 = CARTESIAN_POINT ( 'NONE',  ( 70.11804512340412998, 70.92857369726408479, -2.377407488624244447 ) ) ;
#69463 = CARTESIAN_POINT ( 'NONE',  ( 73.16956295238907160, 57.33411781477383329, 16.38320611710937058 ) ) ;
#69464 = CARTESIAN_POINT ( 'NONE',  ( 181.2267447560696496, 257.4888273829192258, -7.641912445402520682 ) ) ;
#69465 = EDGE_LOOP ( 'NONE', ( #97759, #28123, #97077, #84969 ) ) ;
#69466 = VERTEX_POINT ( 'NONE', #41139 ) ;
#69468 = CARTESIAN_POINT ( 'NONE',  ( 82.62769229327159337, 42.34900205467494771, -6.013828860758981598 ) ) ;
#69467 = CARTESIAN_POINT ( 'NONE',  ( 201.5074933251657399, 279.6257787853921286, 16.58790246189369100 ) ) ;
#69469 = VERTEX_POINT ( 'NONE', #87345 ) ;
#69470 = CARTESIAN_POINT ( 'NONE',  ( 190.9501423151522772, 299.9116471280854626, 8.746938802470586083 ) ) ;
#69471 = CARTESIAN_POINT ( 'NONE',  ( 21.21387930172907588, 35.18080186712593616, 3.090169943749475401 ) ) ;
#69472 = CARTESIAN_POINT ( 'NONE',  ( 80.10302014060799536, 57.75140007922345831, 16.60262925785714927 ) ) ;
#69473 = CARTESIAN_POINT ( 'NONE',  ( 71.88753435814669501, 69.77153974756373600, -8.727078283019331195 ) ) ;
#69475 = EDGE_CURVE ( 'NONE', #2827, #17355, #44997, .T. ) ;
#69474 = ORIENTED_EDGE ( 'NONE', *, *, #8345, .F. ) ;
#69476 = CARTESIAN_POINT ( 'NONE',  ( 190.5726849661229210, 300.5654224342945326, -0.2192718484028965964 ) ) ;
#69477 = B_SPLINE_CURVE_WITH_KNOTS ( 'NONE', 3,
 ( #99794, #75005, #98812, #60261, #5095, #35976, #91217, #21780, #90475, #96574, #21044, #82378, #34718, #12948, #97549, #27642, #58507, #27139, #73732, #51925, #42798, #88490, #65617, #3833, #26630, #58990, #11941, #89480, #43809, #35721, #42309, #19052, #11453, #74749, #4841, #66619, #57514, #20039, #5329, #58024, #89006, #49926, #50912, #50416, #4318, #81374, #36207, #80884 ),
 .UNSPECIFIED., .F., .F.,
 ( 4, 2, 2, 2, 2, 2, 2, 2, 2, 2, 2, 2, 2, 2, 2, 2, 2, 2, 2, 2, 2, 2, 2, 4 ),
 ( 0.0001524510006530677771, 0.001166763548647211995, 0.001673919822644244016, 0.001800708891143506683, 0.001927497959642768917, 0.002054287028142031367, 0.002181076096641293600, 0.002434654233639839318, 0.002688232370638384168, 0.003195388644635474302, 0.004209701192629701841, 0.005224013740623929813, 0.005731170014621009105, 0.005984748151619504949, 0.006238326288618002528, 0.006301720822867608492, 0.006365115357117216190, 0.006491904425616409902, 0.006745482562614796458, 0.007252638836611600796, 0.007506216973610002965, 0.007759795110608406002, 0.008013373247606809038, 0.008266951384605210340 ),
 .UNSPECIFIED. ) ;
#69478 = VECTOR ( 'NONE', #30443, 1000.000000000000114 ) ;
#69479 = VERTEX_POINT ( 'NONE', #87833 ) ;
#69480 = CARTESIAN_POINT ( 'NONE',  ( -19.65312891409030271, 93.06504152958497400, -10.00000000000000888 ) ) ;
#69481 = LINE ( 'NONE', #82749, #54212 ) ;
#69482 = VERTEX_POINT ( 'NONE', #80205 ) ;
#69483 = DIRECTION ( 'NONE',  ( 0.5000000000000014433, -0.8660254037844378194, 0.000000000000000000 ) ) ;
#69484 = DIRECTION ( 'NONE',  ( 1.000000000000000000, 0.000000000000000000, -0.000000000000000000 ) ) ;
#69485 = ORIENTED_EDGE ( 'NONE', *, *, #30226, .T. ) ;
#69486 = FACE_OUTER_BOUND ( 'NONE', #50281, .T. ) ;
#69487 = FACE_OUTER_BOUND ( 'NONE', #65973, .T. ) ;
#69488 = CARTESIAN_POINT ( 'NONE',  ( -61.08640853961129835, 36.64444830801921427, 10.00000000000000000 ) ) ;
#69489 = CARTESIAN_POINT ( 'NONE',  ( 83.15757460905810206, 52.25129517175852811, 14.83307945656489579 ) ) ;
#69490 = ORIENTED_EDGE ( 'NONE', *, *, #82448, .T. ) ;
#69491 = ORIENTED_EDGE ( 'NONE', *, *, #6783, .T. ) ;
#69492 = CARTESIAN_POINT ( 'NONE',  ( 87.04716231175454766, 46.44793212610622390, 8.841005624941981722 ) ) ;
#69493 = CARTESIAN_POINT ( 'NONE',  ( 47.22349865033175575, 113.7415181542323097, 10.00000000000000000 ) ) ;
#69494 = LINE ( 'NONE', #85241, #80126 ) ;
#69495 = CARTESIAN_POINT ( 'NONE',  ( 147.9748066657072627, 274.3471119452502762, 9.387104374042873900 ) ) ;
#69496 = CARTESIAN_POINT ( 'NONE',  ( 190.7862358025146534, 300.1955415356651429, 3.573119809004446257 ) ) ;
#69497 = CARTESIAN_POINT ( 'NONE',  ( 173.4808968322828946, 276.6942208921578867, -15.66287433468919943 ) ) ;
#69498 = CARTESIAN_POINT ( 'NONE',  ( 191.7001674747973539, 298.6125654446252611, 8.448318027796386076 ) ) ;
#69499 = CARTESIAN_POINT ( 'NONE',  ( 147.4563929227680603, 275.2450308873625886, -3.847749617713808412 ) ) ;
#69500 = CARTESIAN_POINT ( 'NONE',  ( 190.0445576990143195, 301.4801656937889902, 4.140328216824785912 ) ) ;
#69501 = DIRECTION ( 'NONE',  ( 0.4737039832092511671, 0.8806841296921895657, 0.000000000000000000 ) ) ;
#69502 = CARTESIAN_POINT ( 'NONE',  ( 29.59124024723001867, 43.31574901297116043, 10.00000000000000000 ) ) ;
#69503 = CARTESIAN_POINT ( 'NONE',  ( 67.06041821067908870, 66.87374097978496934, 8.879190047928029017 ) ) ;
#69504 = CARTESIAN_POINT ( 'NONE',  ( 76.67018723664637037, 63.82874193578962263, -14.84970574671165089 ) ) ;
#69505 = CARTESIAN_POINT ( 'NONE',  ( 78.71583768155939254, 47.58229240978521091, 14.26676363293138117 ) ) ;
#69506 = EDGE_LOOP ( 'NONE', ( #71754, #54500, #724, #92275 ) ) ;
#69507 = CARTESIAN_POINT ( 'NONE',  ( 190.0410346281152272, 301.4862678315846551, -4.168183356896171254 ) ) ;
#69508 = EDGE_CURVE ( 'NONE', #89960, #7425, #41646, .T. ) ;
#69509 = CARTESIAN_POINT ( 'NONE',  ( 69.68716675523791082, 63.66678453457147668, 12.72030219626601522 ) ) ;
#69510 = CARTESIAN_POINT ( 'NONE',  ( 87.76806118867082773, 45.25231315247835084, -7.033483185435909668 ) ) ;
#69511 = CARTESIAN_POINT ( 'NONE',  ( 79.15613078697549554, 46.13387411693875606, 12.67635992270581724 ) ) ;
#69512 = CARTESIAN_POINT ( 'NONE',  ( 180.1202963787140732, 282.9450741466765749, -15.29024642337825135 ) ) ;
#69513 = DIRECTION ( 'NONE',  ( -0.8660254037844387076, -0.4999999999999998890, -0.000000000000000000 ) ) ;
#69514 = CARTESIAN_POINT ( 'NONE',  ( 68.85329997757726517, 65.11108416569004476, -11.21866815422285057 ) ) ;
#69515 = EDGE_LOOP ( 'NONE', ( #65125, #98389, #27143, #93449 ) ) ;
#69517 = EDGE_CURVE ( 'NONE', #94399, #18285, #72588, .T. ) ;
#69516 = CARTESIAN_POINT ( 'NONE',  ( 208.3699316049496133, 269.7396870210121733, -1.898463622294385811 ) ) ;
#69518 = CARTESIAN_POINT ( 'NONE',  ( 72.19330168037886608, 71.72436257440323004, 5.504111378373467645 ) ) ;
#69519 = CARTESIAN_POINT ( 'NONE',  ( 41.06812061084161769, 204.5177522451419350, 5.000000000000046185 ) ) ;
#69520 = CARTESIAN_POINT ( 'NONE',  ( 131.5951856977227123, 234.5327760586659451, 1.948934522072302763E-15 ) ) ;
#69521 = CARTESIAN_POINT ( 'NONE',  ( 151.2646864780760723, 268.6488729594320830, -14.38346604407754548 ) ) ;
#69522 = VECTOR ( 'NONE', #7829, 999.9999999999998863 ) ;
#69523 = EDGE_CURVE ( 'NONE', #36145, #6477, #17877, .T. ) ;
#69524 = CARTESIAN_POINT ( 'NONE',  ( 67.09206164238648284, 67.73860045507836958, -6.489367457569042763 ) ) ;
#69525 = B_SPLINE_CURVE_WITH_KNOTS ( 'NONE', 3,
 ( #44720, #12876, #75654, #6239, #37133, #52827, #76168, #6745, #85279, #70023, #93370, #54823, #23925, #16828, #53812, #62929, #78653, #24437, #78149, #15312, #47716, #15825, #38623, #7227, #69025, #61917, #84776, #99955, #92865, #55313, #23419, #46728, #22925, #8736, #77656, #8242, #46211, #30538, #54309, #86294, #85804, #69532, #39108, #142, #16333, #77130 ),
 .UNSPECIFIED., .F., .F.,
 ( 4, 1, 2, 2, 1, 2, 2, 1, 1, 2, 2, 1, 1, 2, 2, 1, 1, 2, 2, 1, 1, 1, 2, 2, 1, 1, 1, 2, 2, 4 ),
 ( 0.000000000000000000, 0.06249999999999114597, 0.09374999999998707978, 0.1249999999999830136, 0.1874999999999724387, 0.2187499999999692746, 0.2499999999999661382, 0.3124999999999595324, 0.3437499999999579225, 0.3593749999999570899, 0.3749999999999562572, 0.4374999999999593103, 0.4687499999999615308, 0.4843749999999631406, 0.4999999999999648059, 0.5624999999999759082, 0.5937499999999826805, 0.6093749999999872324, 0.6249999999999917843, 0.6875000000000135447, 0.7187500000000266454, 0.7343750000000331957, 0.7421875000000341949, 0.7500000000000351941, 0.8125000000000338618, 0.8437500000000348610, 0.8593750000000358602, 0.8671875000000351941, 0.8750000000000327516, 1.000000000000000000 ),
 .UNSPECIFIED. ) ;
#69526 = CARTESIAN_POINT ( 'NONE',  ( 196.1573359623355088, 290.8925231663144473, 17.55680092534192482 ) ) ;
#69527 = CARTESIAN_POINT ( 'NONE',  ( 175.8386858396426646, 252.9025594026277304, -4.841821914686508244 ) ) ;
#69528 = CARTESIAN_POINT ( 'NONE',  ( 54.70828104404427705, 193.2048013555409796, 4.594050593750051981 ) ) ;
#69529 = CARTESIAN_POINT ( 'NONE',  ( -13.11024591527723615, 6.000000000000000000, -40.00000000000016342 ) ) ;
#69530 = CARTESIAN_POINT ( 'NONE',  ( 85.59595933630416198, 48.93054318311647677, -12.16992291861468978 ) ) ;
#69531 = ORIENTED_EDGE ( 'NONE', *, *, #85458, .T. ) ;
#69533 = ADVANCED_FACE ( 'NONE', ( #3677 ), #56345, .T. ) ;
#69532 = CARTESIAN_POINT ( 'NONE',  ( 70.75100853377770704, 62.48207123928882822, 13.79848856511652500 ) ) ;
#69534 = CARTESIAN_POINT ( 'NONE',  ( 87.99879469594441161, 44.76326497867475496, -4.617324391349451496 ) ) ;
#69535 = EDGE_CURVE ( 'NONE', #38046, #1759, #50089, .T. ) ;
#69536 = CARTESIAN_POINT ( 'NONE',  ( -42.74117156905490589, 79.73515388767964396, 36.50000000000000000 ) ) ;
#69537 = CARTESIAN_POINT ( 'NONE',  ( 146.7845206192450007, 276.4087478532630939, 4.443586170796542945 ) ) ;
#69538 = CARTESIAN_POINT ( 'NONE',  ( 82.16790899789049263, 41.47445355465299599, -5.920440453570812167 ) ) ;
#69539 = DIRECTION ( 'NONE',  ( -0.000000000000000000, 0.000000000000000000, -1.000000000000000000 ) ) ;
#69540 = CIRCLE ( 'NONE', #76073, 70.00000000000001421 ) ;
#69541 = CARTESIAN_POINT ( 'NONE',  ( 178.2687518921240724, 261.3481827365934578, 12.71463598045219001 ) ) ;
#69542 = CARTESIAN_POINT ( 'NONE',  ( 105.5870131927823792, 221.7677522451417929, -5.000000000000041744 ) ) ;
#69543 = B_SPLINE_SURFACE_WITH_KNOTS ( 'NONE', 3, 1, ( 
 ( #74216, #4805 ),
 ( #50880, #58953 ),
 ( #28083, #89925 ),
 ( #82344, #43771 ),
 ( #74716, #44272 ),
 ( #75202, #51891 ),
 ( #46248, #22963 ),
 ( #83318, #92414 ),
 ( #53370, #7267 ),
 ( #83820, #98997 ),
 ( #84812, #75694 ),
 ( #61465, #76680 ),
 ( #13880, #15351 ),
 ( #76204, #36667 ),
 ( #99495, #14386 ),
 ( #45271, #29581 ),
 ( #6780, #38149 ),
 ( #67075, #5779 ),
 ( #67575, #5292 ),
 ( #59963, #84321 ),
 ( #69068, #60458 ),
 ( #37659, #14867 ),
 ( #37175, #53851 ),
 ( #98507, #99995 ),
 ( #29097, #90935 ),
 ( #59457, #44762 ),
 ( #21485, #36172 ),
 ( #30577, #97998 ),
 ( #28578, #68074 ),
 ( #52376, #21010 ),
 ( #68570, #91413 ) ),
 .UNSPECIFIED., .F., .F., .F.,
 ( 4, 3, 3, 3, 3, 3, 3, 3, 3, 3, 4 ),
 ( 2, 2 ),
 ( 0.000000000000000000, 0.1122669598086597914, 0.2243161639709469468, 0.3396355846218949703, 0.4553962076584887608, 0.5677860799922231916, 0.6749047109689442214, 0.7773884377078188468, 0.8775581155834150104, 0.9782364162377956696, 1.000000000000000000 ),
 ( 0.000000000000000000, 1.000000000000000000 ),
 .UNSPECIFIED. ) ;
#69544 = CARTESIAN_POINT ( 'NONE',  ( 82.66777534753497036, 40.88273136530058594, 3.288167606880417981 ) ) ;
#69545 = ORIENTED_EDGE ( 'NONE', *, *, #42188, .F. ) ;
#69546 = CARTESIAN_POINT ( 'NONE',  ( 202.8167949821795446, 279.3580017930215149, 15.61966256214195070 ) ) ;
#69547 = CARTESIAN_POINT ( 'NONE',  ( 85.85663799992927636, 46.49267404192337239, -10.33588943598014076 ) ) ;
#69548 = MECHANICAL_DESIGN_GEOMETRIC_PRESENTATION_REPRESENTATION (  '', ( #56542 ), #4 ) ;
#69549 = CARTESIAN_POINT ( 'NONE',  ( 28.70002176693659379, 193.5024278399160949, -9.188101187500093303 ) ) ;
#69550 = CARTESIAN_POINT ( 'NONE',  ( 18.44000607287492954, 15.81029122506293838, 8.090169943749479842 ) ) ;
#69551 = CARTESIAN_POINT ( 'NONE',  ( 195.9868235513005459, 273.6972693378553458, 14.73968791429838632 ) ) ;
#69552 = CARTESIAN_POINT ( 'NONE',  ( 72.00777348356190544, 59.31339889834504930, -15.33186759774624264 ) ) ;
#69553 = CARTESIAN_POINT ( 'NONE',  ( 30.34687108590970794, 93.06504152958497400, -40.00000000000000000 ) ) ;
#69555 = CARTESIAN_POINT ( 'NONE',  ( 72.70511114461589841, 212.7833772461660544, -9.188101187500095079 ) ) ;
#69554 = CARTESIAN_POINT ( 'NONE',  ( 196.4846840357795088, 276.3116666789414353, -15.35900642488486945 ) ) ;
#69556 = CARTESIAN_POINT ( 'NONE',  ( 208.2175703429120688, 270.0035844679667889, 2.257951022351344150 ) ) ;
#69557 = CARTESIAN_POINT ( 'NONE',  ( 73.03981800122609513, 57.14498309348731908, 16.39931138066937066 ) ) ;
#69558 = CARTESIAN_POINT ( 'NONE',  ( -32.15221709332305977, 96.62083620615463531, 44.28563379145492007 ) ) ;
#69559 = CARTESIAN_POINT ( 'NONE',  ( 66.55005611329578130, 68.31410343647267780, -4.333635880301643262 ) ) ;
#69560 = ORIENTED_EDGE ( 'NONE', *, *, #89108, .T. ) ;
#69561 = B_SPLINE_CURVE_WITH_KNOTS ( 'NONE', 3,
 ( #18249, #49628, #57716, #11161 ),
 .UNSPECIFIED., .F., .F.,
 ( 4, 4 ),
 ( 0.03553003851185922851, 0.04427159934830902227 ),
 .UNSPECIFIED. ) ;
#69562 = CARTESIAN_POINT ( 'NONE',  ( 18.71383987920370728, 191.6115022471903160, -5.000000000000047962 ) ) ;
#69563 = CARTESIAN_POINT ( 'NONE',  ( 207.8725590214046406, 270.6011616060040410, 1.988011721677743093 ) ) ;
#69564 = CARTESIAN_POINT ( 'NONE',  ( -7.131779314644562717, 172.8149278399161233, 9.188101187500093303 ) ) ;
#69565 = CARTESIAN_POINT ( 'NONE',  ( 35.11595366814305663, 25.98920272979928470, 7.433330006724137462 ) ) ;
#69566 = CARTESIAN_POINT ( 'NONE',  ( 167.7808644153182911, 262.5190237135477673, -16.72764794300355717 ) ) ;
#69567 = CARTESIAN_POINT ( 'NONE',  ( 189.2906976920214106, 261.6579632016146206, 6.676593444642060504 ) ) ;
#69568 = CARTESIAN_POINT ( 'NONE',  ( 164.5813345449211624, 245.5837619211427523, 1.447064457712487373 ) ) ;
#69569 = DIRECTION ( 'NONE',  ( 0.8082118706970062849, 0.5888918169447132644, 0.000000000000000000 ) ) ;
#69570 = CARTESIAN_POINT ( 'NONE',  ( 66.06852073167053163, 68.55763805071961769, 2.146522798610484006 ) ) ;
#69571 = VERTEX_POINT ( 'NONE', #4149 ) ;
#69572 = CARTESIAN_POINT ( 'NONE',  ( 81.89485588203808675, 55.22971306509116829, 16.24120679747551677 ) ) ;
#69573 = CARTESIAN_POINT ( 'NONE',  ( 145.8571944687587632, 255.0177522451418497, -10.00000000000009592 ) ) ;
#69574 = CARTESIAN_POINT ( 'NONE',  ( 48.74043828842092552, 100.0309547576005258, -10.00000000000000000 ) ) ;
#69575 = CARTESIAN_POINT ( 'NONE',  ( 10.31635424878816742, 24.14336893147753926, 7.433330006724141015 ) ) ;
#69576 = ORIENTED_EDGE ( 'NONE', *, *, #35071, .T. ) ;
#69577 = CARTESIAN_POINT ( 'NONE',  ( 160.2542454754482151, 253.0785000383454815, 16.23321635550783881 ) ) ;
#69578 = EDGE_CURVE ( 'NONE', #61965, #88529, #6035, .T. ) ;
#69579 = CARTESIAN_POINT ( 'NONE',  ( 205.0520875136525376, 275.4863615587311756, -14.16385635411862509 ) ) ;
#69580 = EDGE_CURVE ( 'NONE', #31573, #90058, #83414, .T. ) ;
#69581 = CARTESIAN_POINT ( 'NONE',  ( 50.06890205215325551, 99.29708757740750968, -10.00000000000000000 ) ) ;
#69582 = CARTESIAN_POINT ( 'NONE',  ( 162.9383752892161397, 248.4294508267893491, -11.25953730674605957 ) ) ;
#69583 = CARTESIAN_POINT ( 'NONE',  ( 153.2283961777204695, 265.2476279883323400, -17.66880461074566000 ) ) ;
#69584 = EDGE_LOOP ( 'NONE', ( #65897, #7655, #46574, #5281 ) ) ;
#69585 = ORIENTED_EDGE ( 'NONE', *, *, #45266, .F. ) ;
#69586 = CARTESIAN_POINT ( 'NONE',  ( 190.4730208157468212, 281.5709126222003533, 17.49935528176693111 ) ) ;
#69587 = DIRECTION ( 'NONE',  ( -0.000000000000000000, -0.000000000000000000, -1.000000000000000000 ) ) ;
#69588 = VERTEX_POINT ( 'NONE', #11774 ) ;
#69589 = CARTESIAN_POINT ( 'NONE',  ( 149.1856130393175306, 272.2499337880290682, 11.44243872309708188 ) ) ;
#69590 = CARTESIAN_POINT ( 'NONE',  ( 17.58976323311689782, 169.4155109091896065, 2.679491924311254714 ) ) ;
#69591 = CARTESIAN_POINT ( 'NONE',  ( 80.76777501163020645, 45.58789323913284619, -11.58370361122461567 ) ) ;
#69593 = EDGE_CURVE ( 'NONE', #68818, #33333, #79208, .T. ) ;
#69592 = ORIENTED_EDGE ( 'NONE', *, *, #71380, .T. ) ;
#69594 = CIRCLE ( 'NONE', #72893, 0.1418229129681522482 ) ;
#69595 = CARTESIAN_POINT ( 'NONE',  ( 146.5095091551180815, 276.8850816817948726, 0.1418322875769769398 ) ) ;
#69596 = CARTESIAN_POINT ( 'NONE',  ( 79.51408477526288721, 59.30329753914238466, -16.21762607725251470 ) ) ;
#69597 = B_SPLINE_CURVE_WITH_KNOTS ( 'NONE', 3,
 ( #90932, #14383, #91918, #67072, #5289, #7263, #22474, #92411, #21482, #22960 ),
 .UNSPECIFIED., .F., .F.,
 ( 4, 3, 3, 4 ),
 ( 0.0009664718924630083313, 0.001498044977021742614, 0.004494154408225740742, 0.006233382939111537652 ),
 .UNSPECIFIED. ) ;
#69598 = CARTESIAN_POINT ( 'NONE',  ( -27.42236680055714260, 166.5217562850347406, 1.224646799147364892E-15 ) ) ;
#69599 = CARTESIAN_POINT ( 'NONE',  ( 69.51115086706674617, 62.59482774454561138, 13.31802496749108222 ) ) ;
#69600 = VERTEX_POINT ( 'NONE', #56849 ) ;
#69601 = CARTESIAN_POINT ( 'NONE',  ( 203.5810809579637635, 278.0342196514508259, 16.28980717760872210 ) ) ;
#69602 = CARTESIAN_POINT ( 'NONE',  ( 129.9259354818553902, 252.4865022471903160, 10.00000000000009415 ) ) ;
#69603 = CARTESIAN_POINT ( 'NONE',  ( 150.6571681785161445, 269.7011255207979730, 15.24894850018880454 ) ) ;
#69604 = CARTESIAN_POINT ( 'NONE',  ( 81.44338780819921908, 42.58957322285800728, -7.672848007371197987 ) ) ;
#69605 = ORIENTED_EDGE ( 'NONE', *, *, #83416, .T. ) ;
#69606 = ADVANCED_FACE ( 'NONE', ( #35045 ), #68429, .F. ) ;
#69607 = ORIENTED_EDGE ( 'NONE', *, *, #64890, .F. ) ;
#69608 = EDGE_CURVE ( 'NONE', #15648, #91729, #23824, .T. ) ;
#69609 = ORIENTED_EDGE ( 'NONE', *, *, #5103, .F. ) ;
#69610 = DIRECTION ( 'NONE',  ( 1.000000000000000000, 0.000000000000000000, 0.000000000000000000 ) ) ;
#69611 = ORIENTED_EDGE ( 'NONE', *, *, #48308, .F. ) ;
#69612 = CARTESIAN_POINT ( 'NONE',  ( 69.44013160124610806, 70.00334490696101852, 4.490412902077236978 ) ) ;
#69613 = ORIENTED_EDGE ( 'NONE', *, *, #82136, .F. ) ;
#69614 = CARTESIAN_POINT ( 'NONE',  ( 163.7012083107868534, 247.1081852757374975, -6.544933039329257518 ) ) ;
#69615 = DIRECTION ( 'NONE',  ( -0.8660254037844379305, -0.5000000000000014433, -0.000000000000000000 ) ) ;
#69616 = CARTESIAN_POINT ( 'NONE',  ( 169.6649390567766886, 283.2330872627844656, 12.60183415381040106 ) ) ;
#69617 = CARTESIAN_POINT ( 'NONE',  ( 194.8432095198904221, 293.1686569321988145, -14.74101036184996616 ) ) ;
#69618 = CARTESIAN_POINT ( 'NONE',  ( 66.43953443436691941, 68.06212878376058484, -4.898982275787033380 ) ) ;
#69619 = CARTESIAN_POINT ( 'NONE',  ( 204.5265640781558432, 272.6391941324284289, -10.93223615312516195 ) ) ;
#69620 = CARTESIAN_POINT ( 'NONE',  ( 15.46319120177094142, 20.87878583063840665, -9.188101187500006262 ) ) ;
#69621 = CARTESIAN_POINT ( 'NONE',  ( 163.6149864627186616, 282.5311289453194377, 8.575549053882928874 ) ) ;
#69622 = CARTESIAN_POINT ( 'NONE',  ( 41.19957572438558913, 58.46810036157969392, 177.5919119679930134 ) ) ;
#69624 = VERTEX_POINT ( 'NONE', #539 ) ;
#69623 = CARTESIAN_POINT ( 'NONE',  ( 174.9671601572613326, 281.6994072225486434, -15.63500919100072473 ) ) ;
#69625 = EDGE_CURVE ( 'NONE', #97296, #22952, #69924, .T. ) ;
#69626 = CARTESIAN_POINT ( 'NONE',  ( 168.2119325052577778, 256.9784041376886421, -14.56702028336546384 ) ) ;
#69627 = CARTESIAN_POINT ( 'NONE',  ( 159.6962080797732710, 254.0450491601782232, -15.33973334987084947 ) ) ;
#69628 = CARTESIAN_POINT ( 'NONE',  ( 80.33508072308801218, 44.92307697338561212, 11.19555900290710326 ) ) ;
#69629 = CARTESIAN_POINT ( 'NONE',  ( 67.67903030099223827, 65.78857475430520196, -10.59918437212530762 ) ) ;
#69630 = CARTESIAN_POINT ( 'NONE',  ( 200.1444820856229967, 283.9865835035790269, 17.93386694781497326 ) ) ;
#69631 = CARTESIAN_POINT ( 'NONE',  ( 158.6754561591581876, 281.3999859383739590, 2.074094494838789160 ) ) ;
#69632 = EDGE_LOOP ( 'NONE', ( #30772, #35088, #58768 ) ) ;
#69634 = EDGE_CURVE ( 'NONE', #19800, #68024, #30068, .T. ) ;
#69633 = CARTESIAN_POINT ( 'NONE',  ( 193.8226831119175984, 294.9362605212737662, -14.99963475610002739 ) ) ;
#69635 = CARTESIAN_POINT ( 'NONE',  ( -64.94778771796556782, 41.33875607593970614, -10.00000000000000000 ) ) ;
#69636 = CARTESIAN_POINT ( 'NONE',  ( -5.697251193518073187, 177.5177522451419350, 5.000000000000046185 ) ) ;
#69637 = EDGE_CURVE ( 'NONE', #15491, #83740, #15218, .T. ) ;
#69638 = CARTESIAN_POINT ( 'NONE',  ( 87.45434598099585344, 230.4869531367911293, 4.594050593750046652 ) ) ;
#69639 = CARTESIAN_POINT ( 'NONE',  ( 195.4769110598194573, 269.1066215422195000, -10.80299383076835618 ) ) ;
#69640 = EDGE_CURVE ( 'NONE', #30521, #74797, #33681, .T. ) ;
#69641 = CARTESIAN_POINT ( 'NONE',  ( 16.20451498836328241, 9.759783934591631294, -1.583844403245362020 ) ) ;
#69642 = CARTESIAN_POINT ( 'NONE',  ( 203.7394615857265023, 277.7598963572313551, -15.86198225853130417 ) ) ;
#69643 = CARTESIAN_POINT ( 'NONE',  ( 72.91771958014867039, 70.92947700147982459, 7.881516594485337812 ) ) ;
#69645 = CARTESIAN_POINT ( 'NONE',  ( 76.20853621364400965, 65.14312063949556375, 14.16830839953977872 ) ) ;
#69644 = CARTESIAN_POINT ( 'NONE',  ( 15.73713787374454043, 170.7048013555409796, 4.594050593750051981 ) ) ;
#69646 = CARTESIAN_POINT ( 'NONE',  ( 200.7583183585857967, 282.9233878912788214, 16.96937806979494212 ) ) ;
#69647 = ORIENTED_EDGE ( 'NONE', *, *, #26647, .F. ) ;
#69648 = EDGE_CURVE ( 'NONE', #56685, #37549, #66319, .T. ) ;
#69649 = ORIENTED_EDGE ( 'NONE', *, *, #1428, .F. ) ;
#69650 = CARTESIAN_POINT ( 'NONE',  ( -12.95261720355844126, 24.63757726406876714, 10.00000000000000000 ) ) ;
#69651 = CARTESIAN_POINT ( 'NONE',  ( 82.49917951009925332, 46.56262670516255753, -11.60890028354300085 ) ) ;
#69652 = CARTESIAN_POINT ( 'NONE',  ( 162.4577219308423821, 249.2619668643215221, -10.67964597906097346 ) ) ;
#69653 = CARTESIAN_POINT ( 'NONE',  ( 81.62374368218522136, 41.76230689378201788, 5.959470817902202455 ) ) ;
#69654 = CARTESIAN_POINT ( 'NONE',  ( -46.74660806181546491, 29.87360136034011049, -10.00000000000000000 ) ) ;
#69655 = CARTESIAN_POINT ( 'NONE',  ( 20.22912401222880519, 191.6744531367911293, 4.594050593750047540 ) ) ;
#69656 = CARTESIAN_POINT ( 'NONE',  ( 131.5951856977227123, 234.5327760586659451, 1.948934522072303157E-15 ) ) ;
#69657 = CARTESIAN_POINT ( 'NONE',  ( 183.1121120950856209, 257.7704774469726203, -2.388561198499064897 ) ) ;
#69658 = ORIENTED_EDGE ( 'NONE', *, *, #84547, .F. ) ;
#69659 = CARTESIAN_POINT ( 'NONE',  ( 153.4758031774517235, 274.2325035235903101, -12.14170705152958796 ) ) ;
#69660 = B_SPLINE_CURVE_WITH_KNOTS ( 'NONE', 3,
 ( #77524, #9107, #39981, #71419, #1523, #93236, #87179, #85665, #94736, #47096, #54178, #40974, #24309, #94242, #39474, #2009, #56185, #17714, #8115, #1010, #62794, #48615, #79554, #10109, #85146, #27309, #89175, #49596, #96746, #41488, #88166, #4498, #3037, #4002, #74428, #80551, #10612, #58195, #12619, #82044, #96244, #35394, #87681, #56700, #57688, #95760, #97236, #19722, #34888, #18216 ),
 .UNSPECIFIED., .F., .F.,
 ( 4, 2, 2, 2, 2, 2, 2, 2, 2, 2, 2, 2, 2, 2, 2, 2, 2, 2, 2, 2, 2, 2, 2, 2, 4 ),
 ( 0.002713875006044959379, 0.003119435521400706294, 0.003220825650239643456, 0.003322215779078580618, 0.003423605907917517781, 0.003524996036756454943, 0.003727776294434217812, 0.003930556552111981114, 0.004336117067467507719, 0.005147238098178560928, 0.005958359128889613270, 0.006769480159600665611, 0.007580601190311718821, 0.007681991319150647743, 0.007732686383570167715, 0.007783381447989689422, 0.007834076512409211129, 0.007884771576828731102, 0.007986161705667788394, 0.008188941963345904712, 0.008391722221024021031, 0.008594502478702137349, 0.008797282736380253668, 0.009000062994058369986, 0.009202843251736486305 ),
 .UNSPECIFIED. ) ;
#69661 = CARTESIAN_POINT ( 'NONE',  ( 175.2129986207789329, 281.2675690177629804, -15.37069089762922225 ) ) ;
#69662 = CARTESIAN_POINT ( 'NONE',  ( 78.86219776201926379, 59.55369065033505649, 16.50996775951927020 ) ) ;
#69663 = B_SPLINE_CURVE_WITH_KNOTS ( 'NONE', 3,
 ( #6104, #98828, #84638, #69398, #7597, #36999, #60279, #54172, #45099, #54675, #52688, #61290, #8110, #15178, #29410, #85659, #93230, #61786, #83649, #91237, #67910, #76512, #21802, #62276, #23790, #38484, #84155, #14208, #29900, #92254, #77518, #501, #14701, #76034, #46079, #31390, #6612, #7096, #37485, #44585, #37977, #15688, #68395, #75520, #14, #68888 ),
 .UNSPECIFIED., .F., .F.,
 ( 4, 1, 2, 2, 1, 2, 2, 1, 1, 2, 2, 1, 1, 2, 2, 1, 1, 2, 2, 1, 1, 1, 2, 2, 1, 1, 1, 2, 2, 4 ),
 ( 0.000000000000000000, 0.06249999999998147315, 0.09374999999997439548, 0.1249999999999673317, 0.1874999999999541755, 0.2187499999999455991, 0.2499999999999369948, 0.3124999999999205635, 0.3437499999999136802, 0.3593749999999097944, 0.3749999999999058531, 0.4374999999999018563, 0.4687499999998997469, 0.4843749999999002465, 0.4999999999999008571, 0.5624999999998997469, 0.5937499999998977485, 0.6093749999998983036, 0.6249999999998988587, 0.6874999999999000799, 0.7187499999999023004, 0.7343749999999018563, 0.7421874999999029665, 0.7499999999999040767, 0.8124999999999173994, 0.8437499999999240607, 0.8593749999999276135, 0.8671874999999309441, 0.8749999999999341638, 1.000000000000000000 ),
 .UNSPECIFIED. ) ;
#69664 = CARTESIAN_POINT ( 'NONE',  ( -22.42236680055709641, 157.8615022471902591, 0.000000000000000000 ) ) ;
#69665 = CARTESIAN_POINT ( 'NONE',  ( -16.76269525828470464, 104.2312461070085021, 12.63376007436041171 ) ) ;
#69666 = CARTESIAN_POINT ( 'NONE',  ( 207.5785076975260779, 271.1104734389944042, -6.824813054587777650 ) ) ;
#69667 = DIRECTION ( 'NONE',  ( -1.000000000000000000, 0.000000000000000000, 0.000000000000000000 ) ) ;
#69668 = CARTESIAN_POINT ( 'NONE',  ( 194.1852025340051284, 294.3083584634874796, -15.46421316575964688 ) ) ;
#69669 = CARTESIAN_POINT ( 'NONE',  ( 71.54829379733448036, 63.11566098394168023, 14.24659271140924055 ) ) ;
#69670 = CARTESIAN_POINT ( 'NONE',  ( 167.7619341864813975, 278.3484540127419109, 14.70418198314342462 ) ) ;
#69671 = DIRECTION ( 'NONE',  ( 0.000000000000000000, 0.000000000000000000, 1.000000000000000000 ) ) ;
#69672 = CARTESIAN_POINT ( 'NONE',  ( 68.17950952005891452, 67.62522511356370103, 7.807613421983940150 ) ) ;
#69673 = CARTESIAN_POINT ( 'NONE',  ( 190.6071113721798156, 300.5057941498820924, -0.4754021072632813594 ) ) ;
#69674 = DIRECTION ( 'NONE',  ( -0.5891075386695857619, -0.8080546441192343332, 0.000000000000000000 ) ) ;
#69675 = ORIENTED_EDGE ( 'NONE', *, *, #58439, .F. ) ;
#69676 = DIRECTION ( 'NONE',  ( -0.000000000000000000, -0.000000000000000000, -1.000000000000000000 ) ) ;
#69677 = AXIS2_PLACEMENT_3D ( 'NONE', #48808, #16885, #32594 ) ;
#69678 = CARTESIAN_POINT ( 'NONE',  ( 163.7595992360150490, 247.0070492265414828, -6.976205010573520049 ) ) ;
#69679 = CARTESIAN_POINT ( 'NONE',  ( 184.8703512676141827, 269.6233871522278491, 15.48342133112897123 ) ) ;
#69680 = CARTESIAN_POINT ( 'NONE',  ( 107.7791399978856930, 233.0333772461660828, 9.188101187500095079 ) ) ;
#69681 = CARTESIAN_POINT ( 'NONE',  ( 16.72130706672765754, 10.44966523072493203, -2.296566073217252530E-15 ) ) ;
#69682 = CARTESIAN_POINT ( 'NONE',  ( 191.4484954869714954, 299.0484741143815199, 8.684991747358081327 ) ) ;
#69683 = FACE_OUTER_BOUND ( 'NONE', #61772, .T. ) ;
#69685 = CARTESIAN_POINT ( 'NONE',  ( 195.3919583724417635, 278.7998134803532935, 16.31606295574663434 ) ) ;
#69684 = LINE ( 'NONE', #289, #29053 ) ;
#69686 = DIRECTION ( 'NONE',  ( -0.8660254037844387076, -0.4999999999999998890, -0.000000000000000000 ) ) ;
#69687 = CARTESIAN_POINT ( 'NONE',  ( 198.7829547491859330, 286.3448180261817129, -18.59838968157616179 ) ) ;
#69688 = CARTESIAN_POINT ( 'NONE',  ( 139.4522149234842061, 257.9865022471903444, -10.00000000000009592 ) ) ;
#69689 = CARTESIAN_POINT ( 'NONE',  ( -65.13399084342830747, 55.99333101439553673, 59.99999999999999289 ) ) ;
#69690 = CARTESIAN_POINT ( 'NONE',  ( 36.72872667615778397, 36.90829794293883737, 10.00000000000000355 ) ) ;
#69691 = CARTESIAN_POINT ( 'NONE',  ( 20.94669640352213236, 37.57748520232516398, -10.00000000000000000 ) ) ;
#69692 = ORIENTED_EDGE ( 'NONE', *, *, #72194, .T. ) ;
#69693 = CARTESIAN_POINT ( 'NONE',  ( 193.0262541023288918, 267.0219039627663165, 11.38476112752691982 ) ) ;
#69694 = CARTESIAN_POINT ( 'NONE',  ( 26.34264212020660167, 36.18502408145594273, 5.678558825948277544 ) ) ;
#69695 = CARTESIAN_POINT ( 'NONE',  ( 77.16259408558386212, 62.51244760150711954, -15.78298705770125920 ) ) ;
#69696 = CARTESIAN_POINT ( 'NONE',  ( 81.83903537127142158, 50.54224542843174106, 14.83243049913419753 ) ) ;
#69697 = CARTESIAN_POINT ( 'NONE',  ( 196.8363552541316324, 289.7164272536036265, -17.80258609350122967 ) ) ;
#69698 = ORIENTED_EDGE ( 'NONE', *, *, #21324, .T. ) ;
#69699 = CARTESIAN_POINT ( 'NONE',  ( 84.64469814230420752, 50.57817590239302064, -14.03985074783417630 ) ) ;
#69700 = CARTESIAN_POINT ( 'NONE',  ( 75.65276086696347591, 65.13941327059393416, -14.42100060933655570 ) ) ;
#69701 = CARTESIAN_POINT ( 'NONE',  ( -21.74822063352838697, 40.08241122545509683, 59.99999999999999289 ) ) ;
#69702 = CARTESIAN_POINT ( 'NONE',  ( 15.67199189347853761, 32.63213790969699346, 177.5919119679930134 ) ) ;
#69703 = CARTESIAN_POINT ( 'NONE',  ( 192.4202172926039793, 297.3654025762033370, 10.98569444949570872 ) ) ;
#69704 = ORIENTED_EDGE ( 'NONE', *, *, #37494, .F. ) ;
#69705 = CARTESIAN_POINT ( 'NONE',  ( 190.0593414272333064, 280.4258356288787013, 16.63430549608987263 ) ) ;
#69706 = CARTESIAN_POINT ( 'NONE',  ( 33.95706010830453181, 41.64646525600393545, -2.839279412974133887 ) ) ;
#69707 = ORIENTED_EDGE ( 'NONE', *, *, #16550, .T. ) ;
#69708 = CARTESIAN_POINT ( 'NONE',  ( 166.6597750968865057, 249.2737811707126241, 6.985541172388376019 ) ) ;
#69709 = CARTESIAN_POINT ( 'NONE',  ( 166.6845710576681654, 267.6039330892615453, -17.82176506903607915 ) ) ;
#69711 = EDGE_CURVE ( 'NONE', #31470, #22323, #64845, .T. ) ;
#69710 = VERTEX_POINT ( 'NONE', #65336 ) ;
#69712 = CARTESIAN_POINT ( 'NONE',  ( 86.42645758268480449, 47.01732744055364321, -10.52632212332719064 ) ) ;
#69713 = CARTESIAN_POINT ( 'NONE',  ( 206.1870820878973518, 273.5204932898241168, 12.10889776728465961 ) ) ;
#69714 = CARTESIAN_POINT ( 'NONE',  ( 153.3174834103889168, 265.0933243750448582, -17.43849572736497322 ) ) ;
#69715 = B_SPLINE_CURVE_WITH_KNOTS ( 'NONE', 3,
 ( #16002, #16993, #94540, #79356, #47883, #92546, #78321, #17503, #798, #94045, #84941, #39771, #38794, #69201, #31680, #63099 ),
 .UNSPECIFIED., .F., .F.,
 ( 4, 1, 2, 2, 2, 1, 2, 2, 4 ),
 ( 0.000000000000000000, 0.1249999999999995004, 0.1874999999999998335, 0.2500000000000001665, 0.5000000000000008882, 0.6250000000000018874, 0.6875000000000016653, 0.7500000000000014433, 1.000000000000000000 ),
 .UNSPECIFIED. ) ;
#69716 = CARTESIAN_POINT ( 'NONE',  ( 81.90730358699052260, 44.58729832355561484, -10.71401170549568427 ) ) ;
#69717 = CARTESIAN_POINT ( 'NONE',  ( 45.46674490716588224, 28.11110640527296312, -2.839279412974138328 ) ) ;
#69718 = CARTESIAN_POINT ( 'NONE',  ( 84.88788782112796127, 50.10586950722157695, -13.27192515002011497 ) ) ;
#69719 = CARTESIAN_POINT ( 'NONE',  ( -65.10162659358719850, 39.48459004765182812, 10.00000000000000000 ) ) ;
#69720 = ADVANCED_FACE ( 'NONE', ( #63834 ), #48651, .F. ) ;
#69721 = VERTEX_POINT ( 'NONE', #87217 ) ;
#69722 = CARTESIAN_POINT ( 'NONE',  ( 162.6827909417944227, 249.2597063335634004, 10.48648004974573311 ) ) ;
#69723 = EDGE_CURVE ( 'NONE', #76194, #89530, #49629, .T. ) ;
#69724 = ORIENTED_EDGE ( 'NONE', *, *, #58243, .T. ) ;
#69725 = CARTESIAN_POINT ( 'NONE',  ( 81.54419519852100962, 59.48562949720209048, 0.3078307376628255376 ) ) ;
#69726 = ORIENTED_EDGE ( 'NONE', *, *, #89366, .T. ) ;
#69727 = CARTESIAN_POINT ( 'NONE',  ( 170.6801095655508220, 269.8234966757721622, 16.62812258642549068 ) ) ;
#69728 = EDGE_LOOP ( 'NONE', ( #56396, #62208, #13764, #4511 ) ) ;
#69729 = PLANE ( 'NONE',  #10373 ) ;
#69730 = CARTESIAN_POINT ( 'NONE',  ( 163.2919429874875448, 247.8170536094679903, 9.876785378511263147 ) ) ;
#69731 = CARTESIAN_POINT ( 'NONE',  ( 32.62753302031853053, 27.03677371833804344, 10.00000000000000533 ) ) ;
#69732 = CARTESIAN_POINT ( 'NONE',  ( 17.38248943320504836, 35.13769309531819829, 10.00000000000000000 ) ) ;
#69733 = CARTESIAN_POINT ( 'NONE',  ( 192.6679047218190135, 296.9363953644068488, -13.34486378385621386 ) ) ;
#69734 = CARTESIAN_POINT ( 'NONE',  ( 167.7899786429152584, 249.3113210190526559, -5.466766185341908724 ) ) ;
#69735 = LINE ( 'NONE', #31232, #45295 ) ;
#69736 = CARTESIAN_POINT ( 'NONE',  ( 183.4965467059954278, 284.4269586455677086, -15.20610756331047142 ) ) ;
#69737 = CARTESIAN_POINT ( 'NONE',  ( 110.3232631693849726, 228.3768266524160140, 9.188101187500098632 ) ) ;
#69738 = FACE_OUTER_BOUND ( 'NONE', #41423, .T. ) ;
#69739 = CARTESIAN_POINT ( 'NONE',  ( 40.50696180670117741, 29.10170272979929962, -7.433330006724141015 ) ) ;
#69740 = FACE_OUTER_BOUND ( 'NONE', #70896, .T. ) ;
#69741 = ORIENTED_EDGE ( 'NONE', *, *, #91300, .T. ) ;
#69742 = ORIENTED_EDGE ( 'NONE', *, *, #5521, .F. ) ;
#69743 = CARTESIAN_POINT ( 'NONE',  ( 74.09829895435802882, 68.37032454858436381, -11.67432565205426620 ) ) ;
#69744 = CARTESIAN_POINT ( 'NONE',  ( 76.92921310806362101, 62.30676013583172335, -15.39267375184458153 ) ) ;
#69745 = CARTESIAN_POINT ( 'NONE',  ( 171.1034016855470554, 287.7520123759660464, -4.697436788832531462 ) ) ;
#69746 = CARTESIAN_POINT ( 'NONE',  ( 157.6286460899086137, 257.6261715744221306, 18.25526781158026779 ) ) ;
#69747 = CARTESIAN_POINT ( 'NONE',  ( 73.47311079653673005, 67.27134392232589732, 11.78844781490330185 ) ) ;
#69748 = CARTESIAN_POINT ( 'NONE',  ( 153.4361244163197000, 264.8878321249116539, -17.23169627811277493 ) ) ;
#69749 = CARTESIAN_POINT ( 'NONE',  ( 177.2134584772402093, 288.8126101685933236, -9.294799257062784648 ) ) ;
#69750 = VERTEX_POINT ( 'NONE', #79586 ) ;
#69751 = CARTESIAN_POINT ( 'NONE',  ( 153.4281311866982946, 266.9016768047333130, 16.59090889036721350 ) ) ;
#69752 = AXIS2_PLACEMENT_3D ( 'NONE', #93921, #63477, #9282 ) ;
#69753 = CARTESIAN_POINT ( 'NONE',  ( 76.94285302476421862, 54.04301539206709037, -16.48480982881932988 ) ) ;
#69754 = ORIENTED_EDGE ( 'NONE', *, *, #13245, .F. ) ;
#69756 = ADVANCED_FACE ( 'NONE', ( #56733 ), #48134, .F. ) ;
#69755 = CARTESIAN_POINT ( 'NONE',  ( 200.4592083165572092, 283.0503611105633013, -16.74591048218803735 ) ) ;
#69757 = DIRECTION ( 'NONE',  ( 0.000000000000000000, 0.000000000000000000, 1.000000000000000000 ) ) ;
#69758 = ORIENTED_EDGE ( 'NONE', *, *, #54391, .T. ) ;
#69759 = DIRECTION ( 'NONE',  ( 0.5000000000000014433, -0.8660254037844378194, 0.000000000000000000 ) ) ;
#69760 = EDGE_CURVE ( 'NONE', #69588, #47527, #23536, .T. ) ;
#69761 = CARTESIAN_POINT ( 'NONE',  ( 158.7649833156394550, 277.6848923185260105, 10.28015389956229342 ) ) ;
#69762 = CARTESIAN_POINT ( 'NONE',  ( 193.0608394500619056, 263.6465134353720714, 4.469366988433737475 ) ) ;
#69763 = CARTESIAN_POINT ( 'NONE',  ( 164.8705138155180521, 286.2009910768602481, -3.373684704351256780 ) ) ;
#69764 = CARTESIAN_POINT ( 'NONE',  ( 165.8382246003566820, 285.1844245935532740, 7.589631688483079230 ) ) ;
#69766 = CARTESIAN_POINT ( 'NONE',  ( 160.8333331388420504, 281.5850016983533806, 5.638315465617829148 ) ) ;
#69765 = CARTESIAN_POINT ( 'NONE',  ( 163.7170172071680554, 282.9345500121884811, -6.650731061596685478 ) ) ;
#69767 = CARTESIAN_POINT ( 'NONE',  ( 152.7375212135632125, 266.0978483664162582, -16.47968945089317572 ) ) ;
#69768 = ORIENTED_EDGE ( 'NONE', *, *, #11902, .F. ) ;
#69769 = CARTESIAN_POINT ( 'NONE',  ( 146.9376205018946848, 276.1435710778808925, 5.066564108429441937 ) ) ;
#69770 = CARTESIAN_POINT ( 'NONE',  ( 71.75782458564195565, 63.63093110014494869, 13.49702202809486984 ) ) ;
#69771 = CARTESIAN_POINT ( 'NONE',  ( 187.0789047048238558, 262.1108460767160295, -8.681453026525897343 ) ) ;
#69772 = EDGE_CURVE ( 'NONE', #20413, #16667, #88199, .T. ) ;
#69773 = CARTESIAN_POINT ( 'NONE',  ( -13.11024591527723615, 27.99999999999999645, -32.50000000000017053 ) ) ;
#69774 = CARTESIAN_POINT ( 'NONE',  ( 24.59328401069779702, 196.5530062829863311, -4.648177544792955347E-16 ) ) ;
#69775 = CARTESIAN_POINT ( 'NONE',  ( 188.5791505740767491, 298.5695105480600660, -4.259152367848529686 ) ) ;
#69776 = CYLINDRICAL_SURFACE ( 'NONE', #30716, 70.00000000000002842 ) ;
#69777 = CARTESIAN_POINT ( 'NONE',  ( 155.3017250444513024, 261.6565170503553190, 18.58368563027307374 ) ) ;
#69778 = CARTESIAN_POINT ( 'NONE',  ( 191.1544238276611054, 283.3818065463574953, -16.58314240119747751 ) ) ;
#69779 = CARTESIAN_POINT ( 'NONE',  ( 74.78835937171426451, 65.46884208322394727, -13.99351343922952218 ) ) ;
#69780 = CARTESIAN_POINT ( 'NONE',  ( 81.12205585946965414, 208.4548013555409796, -4.594050593750042211 ) ) ;
#69781 = DIRECTION ( 'NONE',  ( -0.6270036013472530811, -0.3336146661356822474, -0.7039657224870768948 ) ) ;
#69782 = CARTESIAN_POINT ( 'NONE',  ( 93.96857342517719758, 4.999999999999999112, 0.000000000000000000 ) ) ;
#69783 = CARTESIAN_POINT ( 'NONE',  ( 60.73642589098854216, 194.3262482093457777, 3.021315404115420679E-15 ) ) ;
#69784 = CARTESIAN_POINT ( 'NONE',  ( 203.3041373168503299, 278.5139001086923827, -16.61929732091214973 ) ) ;
#69785 = DIRECTION ( 'NONE',  ( -0.8660254037844387076, -0.4999999999999998890, -0.000000000000000000 ) ) ;
#69786 = CARTESIAN_POINT ( 'NONE',  ( 84.88524026444144965, 50.15864675185714106, -13.30353507586484163 ) ) ;
#69787 = DIRECTION ( 'NONE',  ( 0.000000000000000000, 0.000000000000000000, 1.000000000000000000 ) ) ;
#69789 = CARTESIAN_POINT ( 'NONE',  ( 75.83926582415926987, 51.72761679342552554, 15.75719939435382955 ) ) ;
#69788 = CARTESIAN_POINT ( 'NONE',  ( 73.43716180859617282, 69.78348016549323063, -9.856747356917667346 ) ) ;
#69790 = CARTESIAN_POINT ( 'NONE',  ( 36.10619739613039769, 52.83927550304669296, 10.00000000000000000 ) ) ;
#69791 = CARTESIAN_POINT ( 'NONE',  ( 168.3799552507776696, 251.5246230850010534, -8.803241810830677139 ) ) ;
#69792 = CARTESIAN_POINT ( 'NONE',  ( 164.0559412503519070, 246.4937698012927285, -5.533805667793892269 ) ) ;
#69793 = CARTESIAN_POINT ( 'NONE',  ( 196.2048238403250764, 290.8102717488927169, 17.53926796892840656 ) ) ;
#69794 = CARTESIAN_POINT ( 'NONE',  ( -58.00277386063315532, 34.50477571329874138, -10.00000000000000000 ) ) ;
#69795 = EDGE_CURVE ( 'NONE', #26008, #68209, #26843, .T. ) ;
#69796 = CARTESIAN_POINT ( 'NONE',  ( 47.67182463829572470, 189.1423013555410080, -4.594050593750043987 ) ) ;
#69797 = ADVANCED_FACE ( 'NONE', ( #12144 ), #34922, .F. ) ;
#69798 = CARTESIAN_POINT ( 'NONE',  ( 57.27886009182306282, 210.0024278399160949, -9.188101187500093303 ) ) ;
#69799 = CARTESIAN_POINT ( 'NONE',  ( 163.9339498312803585, 247.2367830492466112, -6.562094630368194181 ) ) ;
#69800 = CARTESIAN_POINT ( 'NONE',  ( 88.31461815508600921, 44.17477163632586468, -0.1894090640934013026 ) ) ;
#69801 = CARTESIAN_POINT ( 'NONE',  ( 164.8422622293784627, 258.6706822939664789, 15.55324439361764277 ) ) ;
#69802 = CARTESIAN_POINT ( 'NONE',  ( 141.5809337175232940, 261.7369531367911009, -4.594050593750048428 ) ) ;
#69803 = CARTESIAN_POINT ( 'NONE',  ( 43.53192288983093761, 62.93782412512172186, 177.5919119679930134 ) ) ;
#69804 = CARTESIAN_POINT ( 'NONE',  ( 196.3172732138167191, 269.3125600491860041, -10.61832308323725549 ) ) ;
#69805 = CARTESIAN_POINT ( 'NONE',  ( 28.18775043786755319, 21.98920272979927759, 7.433330006724137462 ) ) ;
#69806 = CARTESIAN_POINT ( 'NONE',  ( 135.5370584069941913, 242.3927522451417360, -10.00000000000009237 ) ) ;
#69807 = CARTESIAN_POINT ( 'NONE',  ( 79.71556424985024591, 47.75035343155403211, -13.49447772176174531 ) ) ;
#69808 = CARTESIAN_POINT ( 'NONE',  ( 7.926391159377050855, 27.68290643055185285, 3.479690158560446702E-15 ) ) ;
#69809 = CARTESIAN_POINT ( 'NONE',  ( 61.04057116557046925, 215.2369531367911009, -4.594050593750048428 ) ) ;
#69810 = CARTESIAN_POINT ( 'NONE',  ( 77.10487046911684672, 63.70698652748915691, 15.00300083360309067 ) ) ;
#69811 = CARTESIAN_POINT ( 'NONE',  ( 154.8545429534089237, 262.4310591522755089, -17.81746354318405778 ) ) ;
#69812 = CARTESIAN_POINT ( 'NONE',  ( 197.8977219949227049, 287.8780861330898801, 17.48564646125164046 ) ) ;
#69813 = CARTESIAN_POINT ( 'NONE',  ( 59.15898261476995401, 193.4155109091896065, 2.679491924311254714 ) ) ;
#69814 = CARTESIAN_POINT ( 'NONE',  ( 153.1683959517632729, 276.7515984265086786, 7.179112260468418327 ) ) ;
#69815 = VECTOR ( 'NONE', #555, 1000.000000000000000 ) ;
#69816 = CARTESIAN_POINT ( 'NONE',  ( 77.94754277669224507, 55.87611658206658660, -16.15100785399431160 ) ) ;
#69817 = CARTESIAN_POINT ( 'NONE',  ( 87.71125355519491507, 45.00661457325054471, -6.624481356856373182 ) ) ;
#69818 = CARTESIAN_POINT ( 'NONE',  ( 103.2234855318351947, 243.7365022471903444, 2.944929066748280225E-16 ) ) ;
#69819 = CARTESIAN_POINT ( 'NONE',  ( -19.65615963453818082, 92.92325100318677755, 59.99999999999999289 ) ) ;
#69820 = CARTESIAN_POINT ( 'NONE',  ( 206.9059968923335475, 272.2752963222270068, 6.902135944297345560 ) ) ;
#69821 = ORIENTED_EDGE ( 'NONE', *, *, #55656, .F. ) ;
#69822 = DIRECTION ( 'NONE',  ( -0.9689885751534038638, -0.2471055264905585858, 0.000000000000000000 ) ) ;
#69823 = CARTESIAN_POINT ( 'NONE',  ( 82.83837546952335629, 53.74639695667534056, 15.76443799962147452 ) ) ;
#69824 = ORIENTED_EDGE ( 'NONE', *, *, #86864, .T. ) ;
#69825 = CARTESIAN_POINT ( 'NONE',  ( 206.4484807199597753, 273.0677375780628608, -9.220527398138528952 ) ) ;
#69826 = CARTESIAN_POINT ( 'NONE',  ( 188.1954655760533797, 277.4481781369921123, -16.60034468329214263 ) ) ;
#69827 = DIRECTION ( 'NONE',  ( -0.8660254037844387076, -0.4999999999999998890, -0.000000000000000000 ) ) ;
#69828 = ORIENTED_EDGE ( 'NONE', *, *, #69358, .T. ) ;
#69829 = DIRECTION ( 'NONE',  ( 1.000000000000000000, 0.000000000000000000, 0.000000000000000000 ) ) ;
#69830 = VERTEX_POINT ( 'NONE', #89204 ) ;
#69831 = CARTESIAN_POINT ( 'NONE',  ( 79.52155086799245964, 46.24721992604344223, -13.21381413403579863 ) ) ;
#69832 = CARTESIAN_POINT ( 'NONE',  ( 194.9757425430702824, 292.9391030023704161, -15.21392314336593365 ) ) ;
#69833 = CARTESIAN_POINT ( 'NONE',  ( 82.86586985908988368, 152.2544130683315871, 0.000000000000000000 ) ) ;
#69834 = VERTEX_POINT ( 'NONE', #81572 ) ;
#69835 = CARTESIAN_POINT ( 'NONE',  ( 26.72152145096863762, 27.37878583063842086, 9.188101187500006262 ) ) ;
#69836 = CARTESIAN_POINT ( 'NONE',  ( 79.76359975193354046, 44.98417069036880633, 11.54310746654911135 ) ) ;
#69837 = LINE ( 'NONE', #23233, #9624 ) ;
#69838 = CARTESIAN_POINT ( 'NONE',  ( 75.07571136114331978, 67.05229642490535014, -13.12030194816077788 ) ) ;
#69839 = ORIENTED_EDGE ( 'NONE', *, *, #75240, .T. ) ;
#69840 = EDGE_CURVE ( 'NONE', #15205, #97002, #96783, .T. ) ;
#69841 = CARTESIAN_POINT ( 'NONE',  ( 159.7692415128758228, 253.9185515433934768, -16.85856106119654285 ) ) ;
#69842 = EDGE_CURVE ( 'NONE', #95622, #9585, #96846, .T. ) ;
#69843 = VERTEX_POINT ( 'NONE', #54318 ) ;
#69844 = CARTESIAN_POINT ( 'NONE',  ( 174.2237003172097332, 285.9827261121123456, 10.49758392901496329 ) ) ;
#69846 = CARTESIAN_POINT ( 'NONE',  ( 68.07222591375136744, 65.60410304735803777, -10.28098472668225050 ) ) ;
#69845 = CARTESIAN_POINT ( 'NONE',  ( 67.97956794376455036, 65.69536696150683497, 10.87159683219886297 ) ) ;
#69847 = CARTESIAN_POINT ( 'NONE',  ( 81.69437891932362561, 55.22934985428000232, -15.91580060879360659 ) ) ;
#69848 = CARTESIAN_POINT ( 'NONE',  ( 164.4294002498235159, 245.8469198396639399, 6.098783631055905374 ) ) ;
#69849 = EDGE_CURVE ( 'NONE', #6423, #55638, #57890, .T. ) ;
#69850 = CARTESIAN_POINT ( 'NONE',  ( 71.98264401366868981, 72.39816763649429276, -2.869464145551836598 ) ) ;
#69851 = CARTESIAN_POINT ( 'NONE',  ( 204.9184781223158609, 275.7177798128946620, -12.59106622113254126 ) ) ;
#69852 = CARTESIAN_POINT ( 'NONE',  ( 141.2025682470151366, 243.1423013555409796, -4.594050593750043987 ) ) ;
#69853 = CARTESIAN_POINT ( 'NONE',  ( 206.5477884165873377, 270.4809506326999440, 3.067131091788421582 ) ) ;
#69854 = CARTESIAN_POINT ( 'NONE',  ( 181.6318543639017662, 260.2046728290346209, 9.493342775386514276 ) ) ;
#69855 = CARTESIAN_POINT ( 'NONE',  ( 68.21243081460160340, 216.3149278399160664, 9.188101187500093303 ) ) ;
#69856 = ORIENTED_EDGE ( 'NONE', *, *, #71939, .F. ) ;
#69857 = CARTESIAN_POINT ( 'NONE',  ( 190.9907605556751093, 299.8412942717858414, 8.799173206188184437 ) ) ;
#69858 = CARTESIAN_POINT ( 'NONE',  ( 199.5820190223589066, 281.0610403850588455, -17.29246150691365358 ) ) ;
#69859 = DIRECTION ( 'NONE',  ( 0.5000000000000002220, -0.8660254037844387076, -0.000000000000000000 ) ) ;
#69860 = EDGE_LOOP ( 'NONE', ( #13952, #25676, #88274, #7308 ) ) ;
#69861 = CARTESIAN_POINT ( 'NONE',  ( 157.2289892027454528, 258.3183976085836662, -18.38247659754729924 ) ) ;
#69862 = ORIENTED_EDGE ( 'NONE', *, *, #14654, .T. ) ;
#69863 = CARTESIAN_POINT ( 'NONE',  ( 66.77969908731566306, 67.50642965742754598, 6.591304754949472766 ) ) ;
#69864 = CARTESIAN_POINT ( 'NONE',  ( 32.24342178309110096, 47.97677246190463052, -10.00000000000000000 ) ) ;
#69866 = B_SPLINE_SURFACE_WITH_KNOTS ( 'NONE', 3, 1, ( 
 ( #31365, #16173 ),
 ( #30874, #62249 ),
 ( #47069, #77985 ),
 ( #8580, #39445 ),
 ( #98804, #37458 ),
 ( #95729, #72398 ),
 ( #40456, #11092 ),
 ( #70366, #24276 ),
 ( #63271, #33370 ),
 ( #25790, #10081 ),
 ( #17164, #976 ),
 ( #87651, #16668 ),
 ( #1489, #55152 ),
 ( #25267, #64783 ),
 ( #17680, #39946 ),
 ( #71391, #88136 ),
 ( #32370, #80013 ),
 ( #94705, #56151 ),
 ( #40945, #47563 ),
 ( #31855, #1980 ),
 ( #64273, #87148 ),
 ( #49565, #78490 ),
 ( #62757, #26279 ),
 ( #70883, #80516 ),
 ( #57155, #95224 ),
 ( #94211, #56667 ),
 ( #48064, #18682 ),
 ( #49080, #41455 ),
 ( #71892, #32866 ),
 ( #93714, #79006 ),
 ( #2488, #48580 ) ),
 .UNSPECIFIED., .F., .F., .F.,
 ( 4, 3, 3, 3, 3, 3, 3, 3, 3, 3, 4 ),
 ( 2, 2 ),
 ( 0.000000000000000000, 0.1122669598086694226, 0.2243161639709572996, 0.3396355846219043517, 0.4553962076585063579, 0.5677860799922249679, 0.6749047109689459978, 0.7773884377078082997, 0.8775581155834093483, 0.9782364162377646943, 1.000000000000000000 ),
 ( 0.000000000000000000, 1.000000000000000000 ),
 .UNSPECIFIED. ) ;
#69865 = CARTESIAN_POINT ( 'NONE',  ( 191.8232488616404225, 298.3993822291468518, -9.342381338555176384 ) ) ;
#69867 = CARTESIAN_POINT ( 'NONE',  ( 11.80767242186427879, 30.53330575246455325, 177.5919119679930134 ) ) ;
#69868 = CARTESIAN_POINT ( 'NONE',  ( 56.67693180720107193, 191.9824982072973967, 3.021315404115420679E-15 ) ) ;
#69869 = CARTESIAN_POINT ( 'NONE',  ( 71.45638833778239984, 66.77805383252390925, 11.11285407077601306 ) ) ;
#69870 = CARTESIAN_POINT ( 'NONE',  ( 77.38680066200176100, 224.6744531367911293, 4.594050593750047540 ) ) ;
#69871 = VERTEX_POINT ( 'NONE', #47727 ) ;
#69872 = EDGE_LOOP ( 'NONE', ( #54737, #65022, #19061, #54904 ) ) ;
#69873 = EDGE_CURVE ( 'NONE', #1725, #70239, #7747, .T. ) ;
#69874 = CARTESIAN_POINT ( 'NONE',  ( 200.3340733048875393, 283.6582018791440873, -17.27431918982609460 ) ) ;
#69875 = ORIENTED_EDGE ( 'NONE', *, *, #31857, .T. ) ;
#69876 = CARTESIAN_POINT ( 'NONE',  ( 76.34612012204810583, 51.62224941536150880, -15.67199456353200127 ) ) ;
#69877 = CARTESIAN_POINT ( 'NONE',  ( 76.04102746794296763, 65.42908112640478180, -14.38850911432199098 ) ) ;
#69878 = CARTESIAN_POINT ( 'NONE',  ( 164.3754245770190039, 245.9404084473339083, 1.667926061651832992 ) ) ;
#69879 = CARTESIAN_POINT ( 'NONE',  ( 162.2653288181836047, 284.9971543465875925, 0.5418273949422370839 ) ) ;
#69880 = DIRECTION ( 'NONE',  ( -0.8660254037844382635, -0.5000000000000006661, 0.000000000000000000 ) ) ;
#69882 = B_SPLINE_CURVE_WITH_KNOTS ( 'NONE', 3,
 ( #95189, #85601, #25761, #41426, #444, #62220, #93172, #80998, #26743, #4436, #41939, #95704, #89592, #58617, #3466, #74373 ),
 .UNSPECIFIED., .F., .F.,
 ( 4, 1, 2, 2, 2, 1, 2, 2, 4 ),
 ( 0.000000000000000000, 0.1250000000000004441, 0.1875000000000006661, 0.2500000000000008882, 0.5000000000000014433, 0.6250000000000022204, 0.6875000000000012212, 0.7500000000000002220, 1.000000000000000000 ),
 .UNSPECIFIED. ) ;
#69881 = CARTESIAN_POINT ( 'NONE',  ( 160.2559598273567190, 260.1138223702041614, 16.66839514798089184 ) ) ;
#69883 = ORIENTED_EDGE ( 'NONE', *, *, #15702, .F. ) ;
#69884 = CARTESIAN_POINT ( 'NONE',  ( 188.8294196202719206, 294.9100790419620921, 11.53803975672503235 ) ) ;
#69885 = CARTESIAN_POINT ( 'NONE',  ( 185.3082215061529325, 260.2536058253289752, 6.219936519710626222 ) ) ;
#69886 = CARTESIAN_POINT ( 'NONE',  ( 80.51198428680065433, 43.68793065238016737, 9.861687463089015893 ) ) ;
#69887 = CARTESIAN_POINT ( 'NONE',  ( 152.6692142062575499, 266.2161595735824449, -16.77985299603479419 ) ) ;
#69888 = CARTESIAN_POINT ( 'NONE',  ( 72.48986692580926672, 70.61770627562482616, 7.247109231847176147 ) ) ;
#69889 = DIRECTION ( 'NONE',  ( 0.7278481391575630788, -0.6857383512134002101, 0.000000000000000000 ) ) ;
#69890 = ORIENTED_EDGE ( 'NONE', *, *, #16924, .T. ) ;
#69891 = FACE_OUTER_BOUND ( 'NONE', #59952, .T. ) ;
#69892 = DIRECTION ( 'NONE',  ( -0.000000000000000000, -0.000000000000000000, 1.000000000000000000 ) ) ;
#69893 = CARTESIAN_POINT ( 'NONE',  ( 82.52387326870589845, 41.00991866554480225, 1.047277955764182700 ) ) ;
#69894 = CARTESIAN_POINT ( 'NONE',  ( 187.2381800466000925, 265.7314477490792797, -11.83692723186113938 ) ) ;
#69895 = CARTESIAN_POINT ( 'NONE',  ( 198.5136947552106221, 266.2255384214813603, 1.040791414451307295 ) ) ;
#69896 = CARTESIAN_POINT ( 'NONE',  ( 152.8435137206748777, 271.1131880070238935, 14.11897916978259993 ) ) ;
#69897 = ORIENTED_EDGE ( 'NONE', *, *, #72885, .F. ) ;
#69898 = DIRECTION ( 'NONE',  ( -5.984665299743594308E-16, 0.000000000000000000, -1.000000000000000000 ) ) ;
#69899 = CARTESIAN_POINT ( 'NONE',  ( -14.00244190342910144, 103.2482637300012698, 44.08288450968263561 ) ) ;
#69900 = EDGE_CURVE ( 'NONE', #86369, #23627, #78661, .T. ) ;
#69901 = CARTESIAN_POINT ( 'NONE',  ( -19.65312891409030271, 93.06504152958497400, -40.00000000000000000 ) ) ;
#69903 = FACE_BOUND ( 'NONE', #89843, .T. ) ;
#69902 = CARTESIAN_POINT ( 'NONE',  ( 155.6559071247401960, 261.0430556921643870, 17.79853447468815375 ) ) ;
#69904 = CARTESIAN_POINT ( 'NONE',  ( 176.1208302163809662, 285.3140190418353086, -12.11730431473343295 ) ) ;
#69905 = CARTESIAN_POINT ( 'NONE',  ( 30.45164419685804091, 25.78052372038641948, -10.00000000000000355 ) ) ;
#69906 = CARTESIAN_POINT ( 'NONE',  ( 188.0775634319173832, 267.1413101313072502, 14.31780989748781252 ) ) ;
#69907 = CARTESIAN_POINT ( 'NONE',  ( 79.14312167556931854, 57.64441083166269664, 0.000000000000000000 ) ) ;
#69908 = CARTESIAN_POINT ( 'NONE',  ( 190.6996816925783946, 262.0116268005010056, 2.896814088563383294 ) ) ;
#69909 = CARTESIAN_POINT ( 'NONE',  ( 148.5274394637607998, 249.8927522451418213, -10.00000000000009059 ) ) ;
#69910 = DIRECTION ( 'NONE',  ( 0.8660254037844385966, 0.4999999999999999445, 0.000000000000000000 ) ) ;
#69911 = VERTEX_POINT ( 'NONE', #39616 ) ;
#69912 = FACE_OUTER_BOUND ( 'NONE', #9094, .T. ) ;
#69913 = DIRECTION ( 'NONE',  ( 1.000000000000000000, -1.066607120086310925E-13, 0.000000000000000000 ) ) ;
#69914 = FACE_OUTER_BOUND ( 'NONE', #77499, .T. ) ;
#69915 = DIRECTION ( 'NONE',  ( 0.5000000000000011102, 0.8660254037844380415, 0.000000000000000000 ) ) ;
#69916 = CARTESIAN_POINT ( 'NONE',  ( 20.41882739113040302, 182.5958772461660544, -9.188101187500095079 ) ) ;
#69917 = AXIS2_PLACEMENT_3D ( 'NONE', #30349, #61235, #92199 ) ;
#69918 = CARTESIAN_POINT ( 'NONE',  ( 181.9536094017156813, 275.8212133861905500, -16.44258783804268376 ) ) ;
#69919 = CARTESIAN_POINT ( 'NONE',  ( 24.32480936679734640, 35.81751292744057480, -6.180339887498951690 ) ) ;
#69920 = CARTESIAN_POINT ( 'NONE',  ( 82.54706635703216477, 41.64549635078170553, -4.312970195963365505 ) ) ;
#69921 = CARTESIAN_POINT ( 'NONE',  ( 173.4026771546767804, 273.2456497557084845, -17.70700034978624515 ) ) ;
#69922 = CARTESIAN_POINT ( 'NONE',  ( 72.27059105936884009, 62.71376582020941726, 14.64825672156503522 ) ) ;
#69923 = CARTESIAN_POINT ( 'NONE',  ( 186.8262740501982080, 295.8231315473516929, -8.285001673899497376 ) ) ;
#69924 = LINE ( 'NONE', #16735, #6417 ) ;
#69925 = CARTESIAN_POINT ( 'NONE',  ( 183.0976892694797868, 295.7619773535599279, 1.283268163629483816 ) ) ;
#69926 = CARTESIAN_POINT ( 'NONE',  ( 62.88113547221012567, 207.1115022471902307, 10.00000000000009592 ) ) ;
#69927 = CARTESIAN_POINT ( 'NONE',  ( 71.70518999464594856, 66.55211070663439443, -11.44409006190726608 ) ) ;
#69928 = CARTESIAN_POINT ( 'NONE',  ( 205.1661410800912506, 270.9228951919408814, 6.078262840308254589 ) ) ;
#69929 = CARTESIAN_POINT ( 'NONE',  ( 28.37526224051743284, 193.3149278399160949, -9.188101187500095079 ) ) ;
#69930 = CARTESIAN_POINT ( 'NONE',  ( 72.71813417941989144, 70.76084006159408091, -7.966439650937871875 ) ) ;
#69931 = CARTESIAN_POINT ( 'NONE',  ( 79.14312167556931854, 57.64441083166269664, 0.000000000000000000 ) ) ;
#69932 = CARTESIAN_POINT ( 'NONE',  ( 151.0013883899287066, 269.1049186256390726, -14.25461351222133466 ) ) ;
#69933 = FACE_OUTER_BOUND ( 'NONE', #6613, .T. ) ;
#69934 = CARTESIAN_POINT ( 'NONE',  ( 193.9966098916996771, 294.6350105018939871, 13.97117019253516013 ) ) ;
#69936 = CARTESIAN_POINT ( 'NONE',  ( 88.42888488385111145, 211.8615022471902023, 5.000000000000051514 ) ) ;
#69935 = AXIS2_PLACEMENT_3D ( 'NONE', #33654, #9861, #94980 ) ;
#69937 = CARTESIAN_POINT ( 'NONE',  ( 159.9066067912097537, 278.3881009423306523, -10.16859343533022120 ) ) ;
#69938 = LINE ( 'NONE', #86709, #69815 ) ;
#69939 = CONTEXT_DEPENDENT_SHAPE_REPRESENTATION ( #19839, #96955 ) ;
#69940 = CARTESIAN_POINT ( 'NONE',  ( 26.24098094315136009, 17.01110640527292972, 2.839279412974134775 ) ) ;
#69941 = CARTESIAN_POINT ( 'NONE',  ( 10.99774771173347432, 18.30066082961419838, -10.00000000000000533 ) ) ;
#69942 = CARTESIAN_POINT ( 'NONE',  ( 99.93749413994396491, 240.0530062829862743, -4.648177544792955347E-16 ) ) ;
#69943 = CARTESIAN_POINT ( 'NONE',  ( -19.65312891409030271, 93.06504152958497400, 177.5919119679930134 ) ) ;
#69944 = ORIENTED_EDGE ( 'NONE', *, *, #7592, .F. ) ;
#69945 = CARTESIAN_POINT ( 'NONE',  ( 43.91732790946529263, 25.75978393459167748, -1.583844403245362020 ) ) ;
#69946 = CARTESIAN_POINT ( 'NONE',  ( 7.976297994771393896, 26.64646525600388571, -2.839279412974133887 ) ) ;
#69947 = CARTESIAN_POINT ( 'NONE',  ( 72.40192626949962573, 60.07796831195529563, -15.19260960954916584 ) ) ;
#69948 = CARTESIAN_POINT ( 'NONE',  ( 88.28941560846926961, 44.33790759572318052, 2.269834333188780473 ) ) ;
#69949 = ORIENTED_EDGE ( 'NONE', *, *, #93373, .T. ) ;
#69950 = CARTESIAN_POINT ( 'NONE',  ( 172.4831635826484444, 290.8796410925290843, -1.652085212636280609 ) ) ;
#69952 = EDGE_CURVE ( 'NONE', #37573, #33225, #28814, .T. ) ;
#69951 = CARTESIAN_POINT ( 'NONE',  ( 71.31109310106401722, 71.30997890262395345, -3.879444360706853168 ) ) ;
#69953 = CARTESIAN_POINT ( 'NONE',  ( 77.12096872831645555, 63.68411177576406601, 15.01383154859763280 ) ) ;
#69954 = CARTESIAN_POINT ( 'NONE',  ( 86.21323549116458196, 43.83733327322993745, 5.984240272472757027 ) ) ;
#69955 = EDGE_CURVE ( 'NONE', #95607, #23731, #30667, .T. ) ;
#69956 = EDGE_LOOP ( 'NONE', ( #21189, #30471, #10060, #27374 ) ) ;
#69957 = ORIENTED_EDGE ( 'NONE', *, *, #77543, .F. ) ;
#69959 = CARTESIAN_POINT ( 'NONE',  ( 86.05652331311144110, 43.10072823858845936, -2.262228719805865484 ) ) ;
#69958 = CARTESIAN_POINT ( 'NONE',  ( 186.3691305807677168, 272.1350040206665426, -16.09258582117654868 ) ) ;
#69960 = VERTEX_POINT ( 'NONE', #55325 ) ;
#69961 = CARTESIAN_POINT ( 'NONE',  ( 151.2057546125658973, 268.7509459446807227, 15.78031848731319187 ) ) ;
#69962 = CARTESIAN_POINT ( 'NONE',  ( 29.13110022456613635, 42.86445400964587549, -10.00000000000000000 ) ) ;
#69963 = CARTESIAN_POINT ( 'NONE',  ( 80.28041774221068749, 57.81736701477463924, 16.60186235868147619 ) ) ;
#69964 = CARTESIAN_POINT ( 'NONE',  ( 77.07103148522583069, 63.64506183647083759, 15.39324216548719626 ) ) ;
#69965 = B_SPLINE_CURVE_WITH_KNOTS ( 'NONE', 3,
 ( #74248, #58984, #13433, #59488 ),
 .UNSPECIFIED., .F., .F.,
 ( 4, 4 ),
 ( 0.01596741559801433119, 0.02157542978236621015 ),
 .UNSPECIFIED. ) ;
#69967 = EDGE_CURVE ( 'NONE', #30385, #61372, #9450, .T. ) ;
#69966 = CARTESIAN_POINT ( 'NONE',  ( 148.4016473149517594, 273.6078022540229426, 8.470066617688926769 ) ) ;
#69968 = ORIENTED_EDGE ( 'NONE', *, *, #75861, .F. ) ;
#69969 = DIRECTION ( 'NONE',  ( 0.3213938048432692374, -0.5566703992264209200, -0.7660444431189770143 ) ) ;
#69970 = CARTESIAN_POINT ( 'NONE',  ( -21.58168810074490551, 24.33735145887882112, 10.00000000000000000 ) ) ;
#69971 = VERTEX_POINT ( 'NONE', #92388 ) ;
#69972 = CARTESIAN_POINT ( 'NONE',  ( 28.45357225853751260, 28.37878583063842441, 9.188101187500006262 ) ) ;
#69973 = CARTESIAN_POINT ( 'NONE',  ( 149.6676065383367416, 271.4150965588098074, 11.80358707172367261 ) ) ;
#69974 = FACE_OUTER_BOUND ( 'NONE', #66724, .T. ) ;
#69975 = EDGE_LOOP ( 'NONE', ( #20813, #95982, #60969, #33322 ) ) ;
#69976 = CARTESIAN_POINT ( 'NONE',  ( -18.15312891409030982, 78.55673867226647644, 13.76774301257399458 ) ) ;
#69977 = CARTESIAN_POINT ( 'NONE',  ( 159.9612433783809990, 254.2824735748564535, 15.35173791718965752 ) ) ;
#69978 = CARTESIAN_POINT ( 'NONE',  ( 197.9723018751917039, 287.7489099912414758, 17.92592712455262571 ) ) ;
#69979 = CARTESIAN_POINT ( 'NONE',  ( 83.42767843756884361, 52.41288616963773705, 14.83540219176039798 ) ) ;
#69980 = VERTEX_POINT ( 'NONE', #47239 ) ;
#69981 = VERTEX_POINT ( 'NONE', #86303 ) ;
#69982 =( BOUNDED_CURVE ( )  B_SPLINE_CURVE ( 2, ( #47591, #1519, #17191, #2519, #10609, #33401, #95757, #48092, #9623 ),
 .UNSPECIFIED., .F., .T. ) 
 B_SPLINE_CURVE_WITH_KNOTS ( ( 3, 2, 2, 2, 3 ),
 ( 0.1008064516129032334, 0.1021505376344086086, 0.1048387096774193589, 0.1075268817204301092, 0.1088709677419354843 ),
 .UNSPECIFIED. ) 
 CURVE ( )  GEOMETRIC_REPRESENTATION_ITEM ( )  RATIONAL_B_SPLINE_CURVE ( ( 0.9330127018922192983, 0.9330127018922196314, 1.000000000000000000, 0.8660254037844387076, 1.000000000000000000, 0.8660254037844387076, 1.000000000000000000, 0.9330127018922194093, 0.9330127018922194093 ) ) 
 REPRESENTATION_ITEM ( '' )  );
#69983 = CARTESIAN_POINT ( 'NONE',  ( 25.34687108590969729, 93.06504152958497400, 60.00000000000000000 ) ) ;
#69984 = CARTESIAN_POINT ( 'NONE',  ( 69.13686587061594935, 64.31895405193962745, 11.99662287724232357 ) ) ;
#69985 = CARTESIAN_POINT ( 'NONE',  ( 147.0538900202505488, 275.9421863647172017, 5.192507380313251986 ) ) ;
#69986 = CARTESIAN_POINT ( 'NONE',  ( 148.3707431749605234, 273.6613297946520902, 8.912574527564540716 ) ) ;
#69987 = VERTEX_POINT ( 'NONE', #16837 ) ;
#69988 = CARTESIAN_POINT ( 'NONE',  ( 149.7119746935222793, 271.3382486597900538, 12.05352563709836922 ) ) ;
#69989 = CARTESIAN_POINT ( 'NONE',  ( 157.4655681218829670, 259.9086309006383431, -17.75190047967350893 ) ) ;
#69990 = CARTESIAN_POINT ( 'NONE',  ( 207.1572261440131797, 271.8401544939704877, -5.633070628900782140 ) ) ;
#69991 = CARTESIAN_POINT ( 'NONE',  ( 146.7943851877206214, 276.3916619194686746, -4.608908220452185844 ) ) ;
#69992 = CARTESIAN_POINT ( 'NONE',  ( 160.0211798425829670, 255.5694664316391425, 16.22702261962307091 ) ) ;
#69993 = CIRCLE ( 'NONE', #40917, 0.1418229129683777623 ) ;
#69994 = CARTESIAN_POINT ( 'NONE',  ( 69.69662549137501628, 67.03661573462981949, 9.803235490692268073 ) ) ;
#69995 = DIRECTION ( 'NONE',  ( 0.7253665389804488939, 0.6883628288392138472, 0.000000000000000000 ) ) ;
#69996 = CARTESIAN_POINT ( 'NONE',  ( 67.64562412842587946, 66.75646473445011964, 8.610110601876797887 ) ) ;
#69997 = CARTESIAN_POINT ( 'NONE',  ( 69.28028072256803682, 65.61004360350007403, -10.97831167068993352 ) ) ;
#69998 = CARTESIAN_POINT ( 'NONE',  ( 77.95184231570208055, 47.94166338610092026, 14.11904032283977806 ) ) ;
#69999 = CARTESIAN_POINT ( 'NONE',  ( 104.0442318961827652, 237.0024278399160949, -9.188101187500093303 ) ) ;
#70000 = ORIENTED_EDGE ( 'NONE', *, *, #14542, .F. ) ;
#70001 = CARTESIAN_POINT ( 'NONE',  ( 147.2784190576484491, 275.5532906641692534, 0.2793038414862047958 ) ) ;
#70002 = CARTESIAN_POINT ( 'NONE',  ( 69.83162332184129184, 64.07449313801377855, 12.49715358904647466 ) ) ;
#70003 = CARTESIAN_POINT ( 'NONE',  ( 68.22205435738101187, 65.90345407221148832, 10.80313017757570826 ) ) ;
#70004 = VECTOR ( 'NONE', #59974, 1000.000000000000114 ) ;
#70005 = CARTESIAN_POINT ( 'NONE',  ( 155.2922060645262263, 261.6730044072216401, -16.98884022075611355 ) ) ;
#70006 = CARTESIAN_POINT ( 'NONE',  ( 192.6212972830795707, 296.5656100641699595, 11.48306352210076220 ) ) ;
#70007 = CARTESIAN_POINT ( 'NONE',  ( 83.42542119994749328, 51.64995580955419996, -14.90072893730333270 ) ) ;
#70008 = CARTESIAN_POINT ( 'NONE',  ( 169.0232498750005163, 285.7081439545306694, -7.538763084472316578 ) ) ;
#70009 = ORIENTED_EDGE ( 'NONE', *, *, #71141, .F. ) ;
#70010 = CARTESIAN_POINT ( 'NONE',  ( 162.6757594134126350, 248.8843148665554281, -10.86406770146305867 ) ) ;
#70011 = CARTESIAN_POINT ( 'NONE',  ( 72.11459644421852033, 71.43304111169508985, 5.074525307012419439 ) ) ;
#70012 = CARTESIAN_POINT ( 'NONE',  ( 206.3999048951260136, 272.5212040135120333, 8.078790923728028872 ) ) ;
#70013 = CARTESIAN_POINT ( 'NONE',  ( 129.7002344832967538, 251.8149278399160949, -9.188101187500095079 ) ) ;
#70014 = LINE ( 'NONE', #72042, #51056 ) ;
#70015 = AXIS2_PLACEMENT_3D ( 'NONE', #99063, #6350, #84376 ) ;
#70016 = CARTESIAN_POINT ( 'NONE',  ( 186.1442180010177481, 296.8921586699537443, 4.664459278073469051 ) ) ;
#70017 = CARTESIAN_POINT ( 'NONE',  ( 196.0395593785976018, 291.0965181932902510, 15.97855489120023087 ) ) ;
#70018 = LINE ( 'NONE', #32538, #32062 ) ;
#70019 = CARTESIAN_POINT ( 'NONE',  ( 58.84905177982988533, 192.5327760586659451, 1.948934522072303157E-15 ) ) ;
#70020 = EDGE_CURVE ( 'NONE', #26987, #5926, #85289, .T. ) ;
#70021 = CARTESIAN_POINT ( 'NONE',  ( 69.59316709322138195, 66.26231169737734206, -10.55197826579468057 ) ) ;
#70022 = EDGE_LOOP ( 'NONE', ( #23097, #92236, #80536, #80632 ) ) ;
#70023 = CARTESIAN_POINT ( 'NONE',  ( 72.49757734898066985, 67.98224297600880561, 10.61344264115449576 ) ) ;
#70024 = CARTESIAN_POINT ( 'NONE',  ( 87.97078667614408687, 44.76483236400627419, -4.665040245107967110 ) ) ;
#70025 = DIRECTION ( 'NONE',  ( -1.000000000000000000, 0.000000000000000000, 0.000000000000000000 ) ) ;
#70026 = CARTESIAN_POINT ( 'NONE',  ( 172.4040405218840419, 260.9152829665344484, 14.52276536162257159 ) ) ;
#70027 = LINE ( 'NONE', #22931, #41797 ) ;
#70028 = ADVANCED_FACE ( 'NONE', ( #71063 ), #62421, .T. ) ;
#70029 = DIRECTION ( 'NONE',  ( -0.4831861483251571054, -0.8755176446347036068, 0.000000000000000000 ) ) ;
#70030 = CARTESIAN_POINT ( 'NONE',  ( 81.53115339410011586, 41.92267797703283350, -7.515177224638169839 ) ) ;
#70031 = CARTESIAN_POINT ( 'NONE',  ( 108.1850894041356810, 233.2677522451418497, 10.00000000000009592 ) ) ;
#70032 = CARTESIAN_POINT ( 'NONE',  ( 45.64937871703416761, 26.75978393459169880, -1.583844403245396437 ) ) ;
#70033 = EDGE_LOOP ( 'NONE', ( #33891, #27005, #97653, #99133 ) ) ;
#70034 = EDGE_CURVE ( 'NONE', #66385, #13582, #87185, .T. ) ;
#70035 = CARTESIAN_POINT ( 'NONE',  ( 162.8037981520209314, 248.6625452659484381, 9.809699077002424161 ) ) ;
#70036 = CARTESIAN_POINT ( 'NONE',  ( 9.939249538635717585, 29.23654200823201421, 1.583844403245363353 ) ) ;
#70037 = CARTESIAN_POINT ( 'NONE',  ( 26.45420224557697608, 176.8923013555409796, 4.594050593750050204 ) ) ;
#70038 = CARTESIAN_POINT ( 'NONE',  ( 20.60277255440211164, 12.86426979415089278, -3.090169943749474069 ) ) ;
#70039 = CARTESIAN_POINT ( 'NONE',  ( -25.71980777823813114, 41.69035350511823879, 59.99999999999999289 ) ) ;
#70040 = CYLINDRICAL_SURFACE ( 'NONE', #61025, 60.00000000000002132 ) ;
#70041 = DIRECTION ( 'NONE',  ( 0.8660254037844382635, 0.5000000000000004441, 0.000000000000000000 ) ) ;
#70043 = CARTESIAN_POINT ( 'NONE',  ( 69.94482871793547929, 205.0643266524159856, -9.188101187500093303 ) ) ;
#70042 = CARTESIAN_POINT ( 'NONE',  ( 174.0424481033923314, 287.4814580433055653, 10.99910921803667208 ) ) ;
#70044 = CARTESIAN_POINT ( 'NONE',  ( 161.2313178023453588, 251.3861611254901618, 13.12937145726518473 ) ) ;
#70045 = CARTESIAN_POINT ( 'NONE',  ( 72.90739036693749142, 57.16012815389416346, 15.90261827893724167 ) ) ;
#70046 = CARTESIAN_POINT ( 'NONE',  ( 56.67693180720107193, 191.9824982072973967, 3.021315404115420679E-15 ) ) ;
#70047 = CARTESIAN_POINT ( 'NONE',  ( 66.75732258258473450, 68.40744662148340183, -4.417456331192459729 ) ) ;
#70048 = EDGE_LOOP ( 'NONE', ( #93537, #10454, #53293, #12075 ) ) ;
#70049 = CARTESIAN_POINT ( 'NONE',  ( 29.53915742650918830, 197.8615022471903160, 5.000000000000046185 ) ) ;
#70050 = CARTESIAN_POINT ( 'NONE',  ( 116.9873692804980010, 249.8967562850347122, -4.648177544792955347E-16 ) ) ;
#70051 = CARTESIAN_POINT ( 'NONE',  ( -13.87062626178347813, 171.9869531367911293, 4.594050593750046652 ) ) ;
#70052 = CARTESIAN_POINT ( 'NONE',  ( 32.17146729527596705, 24.28920272979928541, -7.433330006724141015 ) ) ;
#70054 = CARTESIAN_POINT ( 'NONE',  ( -4.170157060006060235, 26.08383846222962887, -10.00000000000000000 ) ) ;
#70053 = DIRECTION ( 'NONE',  ( 1.000000000000000000, 0.000000000000000000, 0.000000000000000000 ) ) ;
#70055 = CARTESIAN_POINT ( 'NONE',  ( 189.2272359299283266, 261.5041717493482452, 6.718889169067000289 ) ) ;
#70056 = CARTESIAN_POINT ( 'NONE',  ( 164.2801755739368446, 246.1053845600426087, 2.518777461081745717 ) ) ;
#70057 = CARTESIAN_POINT ( 'NONE',  ( 183.2104879449952364, 257.6787062734009623, -1.976312334137507287 ) ) ;
#70058 = CARTESIAN_POINT ( 'NONE',  ( 66.10824223320386750, 68.56859800295461582, 2.217169679141618666 ) ) ;
#70059 = EDGE_LOOP ( 'NONE', ( #88526, #50286, #16705, #37344 ) ) ;
#70060 = CARTESIAN_POINT ( 'NONE',  ( 135.1739027599712131, 260.3967562850347122, -4.648177544792955347E-16 ) ) ;
#70061 = CARTESIAN_POINT ( 'NONE',  ( 181.6036457256498693, 287.6251638105166535, 13.44163109634966524 ) ) ;
#70062 = CARTESIAN_POINT ( 'NONE',  ( 196.4935506854234575, 289.8709393705694879, 16.33153036150777737 ) ) ;
#70063 = CARTESIAN_POINT ( 'NONE',  ( 6.332637391379750014, 21.84336893147753855, -7.433330006724137462 ) ) ;
#70064 = VERTEX_POINT ( 'NONE', #45728 ) ;
#70065 = CARTESIAN_POINT ( 'NONE',  ( 159.9379022179727485, 253.6264226329247435, 14.98846149617483192 ) ) ;
#70066 = CARTESIAN_POINT ( 'NONE',  ( 204.6075833744878878, 276.2562653119390461, -13.34672481898815910 ) ) ;
#70067 = EDGE_CURVE ( 'NONE', #41966, #95838, #14841, .T. ) ;
#70068 = AXIS2_PLACEMENT_3D ( 'NONE', #83689, #84194, #53239 ) ;
#70069 = CARTESIAN_POINT ( 'NONE',  ( 71.51113537273405996, 72.37632541024544253, 1.045464050329093286 ) ) ;
#70070 = CARTESIAN_POINT ( 'NONE',  ( 31.08397696812772182, 23.11029122506295863, -8.090169943749478065 ) ) ;
#70071 = CARTESIAN_POINT ( 'NONE',  ( 164.9586510554008782, 244.9302305544571823, -1.717556444319656039 ) ) ;
#70072 = LINE ( 'NONE', #31074, #91421 ) ;
#70073 = CARTESIAN_POINT ( 'NONE',  ( 207.7837159184916231, 270.7550423741513441, -2.369602332675663448 ) ) ;
#70074 = CARTESIAN_POINT ( 'NONE',  ( 201.4520623681621316, 281.7217880192456505, -17.56577389517433119 ) ) ;
#70075 = VERTEX_POINT ( 'NONE', #69544 ) ;
#70076 = ORIENTED_EDGE ( 'NONE', *, *, #96740, .F. ) ;
#70077 = CARTESIAN_POINT ( 'NONE',  ( 191.1055097870458042, 281.0373243973215267, 16.65489552781466287 ) ) ;
#70078 = CARTESIAN_POINT ( 'NONE',  ( 164.2934308416063232, 248.6433794851443793, 10.01835112954314155 ) ) ;
#70079 = ORIENTED_EDGE ( 'NONE', *, *, #23730, .T. ) ;
#70081 = EDGE_CURVE ( 'NONE', #65113, #53392, #64393, .T. ) ;
#70080 = CARTESIAN_POINT ( 'NONE',  ( 71.59728507587232116, 70.99594489426432631, 6.387564926741087667 ) ) ;
#70082 = DIRECTION ( 'NONE',  ( 0.000000000000000000, 1.000000000000000000, 0.000000000000000000 ) ) ;
#70083 = ORIENTED_EDGE ( 'NONE', *, *, #53495, .F. ) ;
#70085 = ADVANCED_FACE ( 'NONE', ( #56833 ), #87818, .T. ) ;
#70084 = PLANE ( 'NONE',  #81502 ) ;
#70086 = CARTESIAN_POINT ( 'NONE',  ( 79.46674400240780756, 59.17914826126551731, -16.22576502784502139 ) ) ;
#70087 = CIRCLE ( 'NONE', #6966, 0.1418229129680828593 ) ;
#70088 = B_SPLINE_CURVE_WITH_KNOTS ( 'NONE', 3,
 ( #19231, #50586, #20209, #27803, #51081, #82043, #66792, #12108, #12618, #42968, #89174, #28796, #59675, #36381, #96745, #4497 ),
 .UNSPECIFIED., .F., .F.,
 ( 4, 2, 2, 2, 2, 2, 2, 4 ),
 ( 0.0006989770276497502596, 0.0009902908671597099310, 0.001281604706669669603, 0.001572918546179629274, 0.001864232385689588945, 0.002155546225199548617, 0.002446860064709508072, 0.003029487743729583106 ),
 .UNSPECIFIED. ) ;
#70089 = CARTESIAN_POINT ( 'NONE',  ( 149.6230451358742926, 271.4922791719315001, -12.72565967355361671 ) ) ;
#70090 = CARTESIAN_POINT ( 'NONE',  ( 69.71741781551351380, 62.54328943123160656, 13.41580856235687769 ) ) ;
#70091 = ORIENTED_EDGE ( 'NONE', *, *, #31583, .T. ) ;
#70092 = CARTESIAN_POINT ( 'NONE',  ( 155.3513056799751553, 261.5706408705564741, 18.59020393050806064 ) ) ;
#70093 = CARTESIAN_POINT ( 'NONE',  ( 150.0879970963906374, 274.3151389057389906, -8.688618402280457786 ) ) ;
#70094 = B_SPLINE_SURFACE_WITH_KNOTS ( 'NONE', 3, 1, ( 
 ( #72489, #41035 ),
 ( #64356, #95320 ),
 ( #25877, #3091 ),
 ( #33982, #64866 ),
 ( #18769, #70200 ),
 ( #59218, #5060 ),
 ( #90193, #811 ),
 ( #75460, #53140 ),
 ( #74482, #31690 ),
 ( #6553, #28340 ),
 ( #51138, #75979 ),
 ( #8418, #89704 ),
 ( #98267, #35941 ),
 ( #20768, #22239 ),
 ( #66843, #97770 ),
 ( #28855, #99260 ),
 ( #83585, #39290 ),
 ( #60714, #12673 ),
 ( #52629, #68335 ),
 ( #51656, #82605 ),
 ( #84097, #13171 ),
 ( #82101, #29845 ),
 ( #37426, #44025 ),
 ( #20264, #67341 ),
 ( #74968, #43541 ),
 ( #5549, #91678 ),
 ( #36434, #14148 ),
 ( #45035, #21744 ),
 ( #59734, #90702 ),
 ( #14649, #46914 ),
 ( #13657, #77836 ),
 ( #21257, #52136 ),
 ( #29355, #83086 ),
 ( #44528, #91183 ) ),
 .UNSPECIFIED., .T., .F., .F.,
 ( 4, 2, 2, 2, 2, 2, 2, 2, 2, 2, 2, 2, 2, 2, 2, 2, 4 ),
 ( 2, 2 ),
 ( 0.000000000000000000, 0.06250000000000000000, 0.1250000000000000000, 0.1875000000000000000, 0.2500000000000000000, 0.3125000000000000000, 0.3750000000000000000, 0.4375000000000000000, 0.5000000000000000000, 0.5625000000000000000, 0.6250000000000000000, 0.6875000000000000000, 0.7500000000000000000, 0.8125000000000000000, 0.8750000000000000000, 0.9375000000000000000, 1.000000000000000000 ),
 ( 0.000000000000000000, 1.000000000000000000 ),
 .UNSPECIFIED. ) ;
#70095 = EDGE_LOOP ( 'NONE', ( #79498, #90479, #31398, #44534 ) ) ;
#70096 = ORIENTED_EDGE ( 'NONE', *, *, #43547, .T. ) ;
#70097 = ORIENTED_EDGE ( 'NONE', *, *, #24989, .F. ) ;
#70098 = CARTESIAN_POINT ( 'NONE',  ( 74.45444392623342367, 66.27966151248681115, 12.94663026855831411 ) ) ;
#70099 = VERTEX_POINT ( 'NONE', #33040 ) ;
#70100 = CARTESIAN_POINT ( 'NONE',  ( -18.45562326176556311, 23.07528527759725634, 177.5919119679930134 ) ) ;
#70101 = ORIENTED_EDGE ( 'NONE', *, *, #87641, .T. ) ;
#70102 = CARTESIAN_POINT ( 'NONE',  ( 208.0692320075777957, 270.2605140014760536, 2.043861372130216569 ) ) ;
#70103 = CARTESIAN_POINT ( 'NONE',  ( 83.35356881092343428, 49.56826083113291759, 13.41475373279179095 ) ) ;
#70104 = CARTESIAN_POINT ( 'NONE',  ( 165.0778591066108163, 270.9504257995093326, 16.70825090401362090 ) ) ;
#70105 = CARTESIAN_POINT ( 'NONE',  ( 167.5814449122423753, 281.2627869255007340, 11.46311708006829200 ) ) ;
#70106 = CARTESIAN_POINT ( 'NONE',  ( 194.3442947553755005, 294.0328026529847421, -15.97648891113594871 ) ) ;
#70107 = CARTESIAN_POINT ( 'NONE',  ( 175.0270463369839149, 289.9902377644656895, 6.217893157806833493 ) ) ;
#70108 = CARTESIAN_POINT ( 'NONE',  ( -69.61464189717713680, 45.83092310410447112, -10.00000000000000000 ) ) ;
#70109 = CARTESIAN_POINT ( 'NONE',  ( 79.49634071307748684, 55.47133629792779175, -16.47986696218380587 ) ) ;
#70110 = CARTESIAN_POINT ( 'NONE',  ( 21.21803360120161486, 14.11110640527291871, -2.839279412974138328 ) ) ;
#70111 = CARTESIAN_POINT ( 'NONE',  ( 198.7717544147009789, 276.5896982162381050, -15.52327009455605022 ) ) ;
#70112 = CARTESIAN_POINT ( 'NONE',  ( 80.03994542435373205, 57.65115798690545290, 16.60126445886217539 ) ) ;
#70114 = ORIENTED_EDGE ( 'NONE', *, *, #95300, .F. ) ;
#70113 = CARTESIAN_POINT ( 'NONE',  ( 159.6978881494930249, 254.0421391940632532, 15.34888828951022610 ) ) ;
#70115 = LINE ( 'NONE', #32632, #44738 ) ;
#70116 = CARTESIAN_POINT ( 'NONE',  ( 206.5081929095101998, 272.9643130319303737, -9.215516226794479238 ) ) ;
#70117 = DIRECTION ( 'NONE',  ( 0.000000000000000000, 0.000000000000000000, 1.000000000000000000 ) ) ;
#70118 = CARTESIAN_POINT ( 'NONE',  ( 68.31414817410238527, 198.7012482093460335, 5.278111984874363062E-14 ) ) ;
#70119 = CARTESIAN_POINT ( 'NONE',  ( 178.0302064638906074, 292.4640037680099454, 7.106335582765731296 ) ) ;
#70120 = FACE_OUTER_BOUND ( 'NONE', #488, .T. ) ;
#70121 = EDGE_LOOP ( 'NONE', ( #24893, #846, #68115, #76585 ) ) ;
#70122 = CARTESIAN_POINT ( 'NONE',  ( 155.2374724870715568, 261.7678057442532804, -17.06470218616315648 ) ) ;
#70123 = DIRECTION ( 'NONE',  ( -0.8660254037844387076, -0.4999999999999998890, -0.000000000000000000 ) ) ;
#70124 = CARTESIAN_POINT ( 'NONE',  ( 162.5887743522035294, 284.9919049736276975, -2.844505511527740005 ) ) ;
#70125 = CARTESIAN_POINT ( 'NONE',  ( 14.22133309352410002, 169.0177522451418213, 5.000000000000051514 ) ) ;
#70126 = CARTESIAN_POINT ( 'NONE',  ( 81.82518085639701155, 227.2369531367911293, -4.594050593750048428 ) ) ;
#70127 = PLANE ( 'NONE',  #23562 ) ;
#70128 = CARTESIAN_POINT ( 'NONE',  ( 16.16012747849099540, 9.734156793818206310, 1.333680081654574804E-15 ) ) ;
#70129 = CARTESIAN_POINT ( 'NONE',  ( 169.3174896907622156, 279.7497339657720090, -13.49786840205827509 ) ) ;
#70130 = CARTESIAN_POINT ( 'NONE',  ( 7.094665711762558225, 168.2365022471902023, -10.00000000000009237 ) ) ;
#70132 = CARTESIAN_POINT ( 'NONE',  ( 75.74251350868291865, 65.46771939187904366, 14.28157630633085518 ) ) ;
#70131 = CARTESIAN_POINT ( 'NONE',  ( 10.18872876104421366, 182.8149278399160949, -9.188101187500095079 ) ) ;
#70133 = EDGE_CURVE ( 'NONE', #86521, #38635, #14284, .T. ) ;
#70134 = CARTESIAN_POINT ( 'NONE',  ( 200.2690241097007799, 283.7708703901988656, 16.96680019208369927 ) ) ;
#70135 = ORIENTED_EDGE ( 'NONE', *, *, #19596, .F. ) ;
#70136 = ORIENTED_EDGE ( 'NONE', *, *, #67929, .F. ) ;
#70137 = CARTESIAN_POINT ( 'NONE',  ( 164.9043417134678577, 286.5925546497160212, 0.04530247668140159611 ) ) ;
#70138 = CARTESIAN_POINT ( 'NONE',  ( 189.0937190564843604, 261.2781646461646687, -6.128236982588672888 ) ) ;
#70139 = EDGE_CURVE ( 'NONE', #58975, #39044, #60183, .T. ) ;
#70140 = CARTESIAN_POINT ( 'NONE',  ( 85.97138696049607631, 45.97668872975567211, -9.009752818326484558 ) ) ;
#70141 = CARTESIAN_POINT ( 'NONE',  ( 202.4709886568992943, 279.9569559179853400, -17.37304959755336853 ) ) ;
#70142 = CARTESIAN_POINT ( 'NONE',  ( 85.69442934047377491, 231.8297689869269220, -2.679491924311252493 ) ) ;
#70143 = FACE_OUTER_BOUND ( 'NONE', #51287, .T. ) ;
#70144 = CARTESIAN_POINT ( 'NONE',  ( 36.84650709099022947, 182.8923013555409796, 4.594050593750050204 ) ) ;
#70145 = VECTOR ( 'NONE', #75206, 1000.000000000000227 ) ;
#70146 = CARTESIAN_POINT ( 'NONE',  ( 196.0366049223029563, 275.3890784149895694, 15.51794149486366159 ) ) ;
#70147 = EDGE_LOOP ( 'NONE', ( #2908, #16998, #93212, #53128 ) ) ;
#70149 = EDGE_CURVE ( 'NONE', #68627, #47421, #12251, .T. ) ;
#70148 = B_SPLINE_CURVE_WITH_KNOTS ( 'NONE', 3,
 ( #52721, #60809, #77551, #37521, #21836, #23320, #91769, #83174, #84185, #14734, #22830, #7126, #91271, #85176, #83681, #15720, #68426, #59828, #53233, #46621, #45617, #76546, #77024, #53715, #38009, #8140, #75551, #99848, #84673, #15215, #67430, #47622, #24826, #17746, #71450, #78047, #54713, #47124, #48646, #40515, #2040, #8636, #79581, #71949, #10142, #39503, #1040, #69921 ),
 .UNSPECIFIED., .F., .F.,
 ( 4, 2, 2, 2, 2, 2, 2, 2, 2, 2, 2, 2, 2, 2, 2, 2, 2, 2, 2, 2, 2, 2, 2, 4 ),
 ( 0.0001670487744419399021, 0.0006556382875749478499, 0.001144227800707955933, 0.001388522557274385165, 0.001632817313840814397, 0.001754964692124029229, 0.001877112070407243845, 0.001999259448690458244, 0.002121406826973672860, 0.002365701583540164975, 0.002609996340106656657, 0.003098585853239643490, 0.004075764879505538660, 0.005052943905771435130, 0.005541533418904341299, 0.005785828175470836450, 0.006030122932037331601, 0.006091196621178905299, 0.006152270310320478129, 0.006274417688603629861, 0.006518712445170039144, 0.007007301958302823881, 0.007495891471435606884, 0.007984480984568392489 ),
 .UNSPECIFIED. ) ;
#70150 = CARTESIAN_POINT ( 'NONE',  ( 88.22000632671871756, 44.27423112938743088, 4.003506518527984781 ) ) ;
#70151 = VECTOR ( 'NONE', #52353, 1000.000000000000114 ) ;
#70152 = CARTESIAN_POINT ( 'NONE',  ( 182.4282706175910391, 260.3850099854238920, -10.97823297164843126 ) ) ;
#70153 = CARTESIAN_POINT ( 'NONE',  ( 80.65296072109273950, 57.47057263566300378, -16.23811142086485759 ) ) ;
#70154 = DIRECTION ( 'NONE',  ( 0.03277852384265245167, -0.9994626398093610087, 0.000000000000000000 ) ) ;
#70155 = CARTESIAN_POINT ( 'NONE',  ( 161.8153478334749877, 250.3745914384277285, -14.21120979595050215 ) ) ;
#70156 = DIRECTION ( 'NONE',  ( 0.4999999999999998890, -0.8660254037844385966, 0.000000000000000000 ) ) ;
#70157 = CARTESIAN_POINT ( 'NONE',  ( 147.7785919239399846, 274.6869658471848652, -7.924750738206837397 ) ) ;
#70158 = B_SPLINE_CURVE_WITH_KNOTS ( 'NONE', 3,
 ( #87803, #10739, #81175, #57318 ),
 .UNSPECIFIED., .F., .F.,
 ( 4, 4 ),
 ( 1.962615573354718958E-17, 0.0005839710162101796522 ),
 .UNSPECIFIED. ) ;
#70159 = EDGE_CURVE ( 'NONE', #38705, #72251, #91262, .T. ) ;
#70160 = CARTESIAN_POINT ( 'NONE',  ( 192.4516364921933018, 265.1256046145381902, 7.763685239252594350 ) ) ;
#70161 = CARTESIAN_POINT ( 'NONE',  ( 163.6414931044696175, 249.4718858119513527, -10.35415494711363849 ) ) ;
#70162 = CARTESIAN_POINT ( 'NONE',  ( 192.5623620705172527, 265.1981932100166546, 8.541982082413346333 ) ) ;
#70163 = CARTESIAN_POINT ( 'NONE',  ( 191.3041230083617563, 299.2985345825480863, -9.819045872446528378 ) ) ;
#70164 = CARTESIAN_POINT ( 'NONE',  ( 148.2159754900428936, 273.9293952882992471, 9.267836332806297150 ) ) ;
#70165 = CARTESIAN_POINT ( 'NONE',  ( 181.2668321688125843, 265.9111225571392083, -15.67575644871175022 ) ) ;
#70166 = EDGE_CURVE ( 'NONE', #20148, #41802, #48201, .T. ) ;
#70167 = ORIENTED_EDGE ( 'NONE', *, *, #19104, .T. ) ;
#70168 = LINE ( 'NONE', #7895, #36771 ) ;
#70169 = CARTESIAN_POINT ( 'NONE',  ( 163.7323023463233937, 247.0543288263758086, -6.244751637846886361 ) ) ;
#70170 = CARTESIAN_POINT ( 'NONE',  ( 182.3665809609293547, 271.4228521140648809, 17.36529365643261968 ) ) ;
#70171 = CARTESIAN_POINT ( 'NONE',  ( 113.7334117446687145, 224.2202760586659736, -5.415160957724236172E-17 ) ) ;
#70172 = CARTESIAN_POINT ( 'NONE',  ( 16.50122538818396478, 18.03085787977762422, 9.188101187500006262 ) ) ;
#70173 = CARTESIAN_POINT ( 'NONE',  ( 151.0099717111976076, 269.0900518771037468, 15.84752309685681659 ) ) ;
#70174 = DIRECTION ( 'NONE',  ( -0.8660254037844387076, -0.4999999999999998890, -0.000000000000000000 ) ) ;
#70176 = CARTESIAN_POINT ( 'NONE',  ( 195.1258871920489071, 279.1051608108670621, 16.30780866269864049 ) ) ;
#70175 = CARTESIAN_POINT ( 'NONE',  ( 196.0355168007595523, 291.1035201434990540, 17.55377893960077884 ) ) ;
#70177 = CARTESIAN_POINT ( 'NONE',  ( 204.6375318825442946, 272.9465897887138226, -9.753471222488339976 ) ) ;
#70178 = CARTESIAN_POINT ( 'NONE',  ( 161.5977722445767313, 278.0340992893568455, 13.12270833059843156 ) ) ;
#70179 = DIRECTION ( 'NONE',  ( -1.000000000000000000, 0.000000000000000000, 0.000000000000000000 ) ) ;
#70180 = CARTESIAN_POINT ( 'NONE',  ( 107.6799079185947221, 239.6427522451419350, 10.00000000000009415 ) ) ;
#70181 = CARTESIAN_POINT ( 'NONE',  ( 33.33823495471120424, 42.18080186712595747, 3.090169943749475401 ) ) ;
#70182 = CARTESIAN_POINT ( 'NONE',  ( 86.31939919580703702, 47.65601329950942500, 10.71069801041972447 ) ) ;
#70183 = ORIENTED_EDGE ( 'NONE', *, *, #72666, .T. ) ;
#70184 = CARTESIAN_POINT ( 'NONE',  ( -68.10632939235270555, 44.28490124273476880, -10.00000000000000000 ) ) ;
#70185 = CARTESIAN_POINT ( 'NONE',  ( 178.7992128730961952, 280.7823504994489667, 16.46972532697894565 ) ) ;
#70186 = CARTESIAN_POINT ( 'NONE',  ( 200.1132727327846226, 269.8987286879626026, 8.973240105661503208 ) ) ;
#70187 = ADVANCED_FACE ( 'NONE', ( #34091 ), #22337, .F. ) ;
#70188 = ORIENTED_EDGE ( 'NONE', *, *, #59842, .T. ) ;
#70189 = DIRECTION ( 'NONE',  ( -0.8660254037844387076, -0.4999999999999998890, -0.000000000000000000 ) ) ;
#70190 = CARTESIAN_POINT ( 'NONE',  ( 183.6876657337322172, 264.4717431763341438, -13.48096450996037632 ) ) ;
#70191 = CARTESIAN_POINT ( 'NONE',  ( 72.39195994751899832, 71.88450172447629427, -5.391213119607743742 ) ) ;
#70192 = CARTESIAN_POINT ( 'NONE',  ( 141.2564345147017946, 262.3615022471902876, 5.000000000000046185 ) ) ;
#70193 = ADVANCED_FACE ( 'NONE', ( #13753 ), #67956, .T. ) ;
#70194 = ORIENTED_EDGE ( 'NONE', *, *, #81348, .T. ) ;
#70195 = CARTESIAN_POINT ( 'NONE',  ( 187.7551830709135174, 279.0899711224498105, 17.74026388000889654 ) ) ;
#70196 = CARTESIAN_POINT ( 'NONE',  ( 40.27059248445925732, 25.11110640527295601, -2.839279412974138328 ) ) ;
#70197 = ORIENTED_EDGE ( 'NONE', *, *, #96350, .F. ) ;
#70198 = CARTESIAN_POINT ( 'NONE',  ( 167.6110149314430942, 249.8830905776618181, 6.925631721972418831 ) ) ;
#70199 = DIRECTION ( 'NONE',  ( 0.4535245244745221282, -0.8912437970051507730, 0.000000000000000000 ) ) ;
#70200 = CARTESIAN_POINT ( 'NONE',  ( 156.9196333786560160, 258.8542176135235877, 18.37000459710097644 ) ) ;
#70201 = ORIENTED_EDGE ( 'NONE', *, *, #23089, .T. ) ;
#70203 = EDGE_CURVE ( 'NONE', #55881, #67265, #75075, .T. ) ;
#70202 = CARTESIAN_POINT ( 'NONE',  ( 79.58936028502597537, 59.22294857574253513, 16.56770033466461811 ) ) ;
#70204 = CARTESIAN_POINT ( 'NONE',  ( 159.2101406416221892, 256.7198602926216608, 16.95745424613295071 ) ) ;
#70205 = B_SPLINE_CURVE_WITH_KNOTS ( 'NONE', 3,
 ( #79405, #2377, #4871, #42829, #19082, #49959, #98065, #59524, #81893, #51445, #74287, #89037, #43339, #73763, #20070, #59020 ),
 .UNSPECIFIED., .F., .F.,
 ( 4, 1, 2, 2, 2, 1, 2, 2, 4 ),
 ( 0.000000000000000000, 0.1249999999999980016, 0.1874999999999987232, 0.2499999999999994449, 0.4999999999999982236, 0.6249999999999958922, 0.6874999999999965583, 0.7499999999999972244, 1.000000000000000000 ),
 .UNSPECIFIED. ) ;
#70206 = CARTESIAN_POINT ( 'NONE',  ( 192.5090254847960693, 297.2115822751985093, -12.59048664097589487 ) ) ;
#70207 = CARTESIAN_POINT ( 'NONE',  ( 83.31676998715261107, 44.47964662621878063, -9.710295204768222277 ) ) ;
#70208 = CARTESIAN_POINT ( 'NONE',  ( -19.65312891409030271, 93.06504152958497400, 59.99999999999999289 ) ) ;
#70209 = EDGE_CURVE ( 'NONE', #76847, #98779, #91286, .T. ) ;
#70210 = CARTESIAN_POINT ( 'NONE',  ( 43.97106342183892735, 31.10170272979931028, -7.433330006724141015 ) ) ;
#70211 = CARTESIAN_POINT ( 'NONE',  ( 80.44421536292240660, 44.39010815972903146, 11.34380831960723945 ) ) ;
#70212 = CARTESIAN_POINT ( 'NONE',  ( 84.79901702372750094, 50.05075620941028092, -13.68787013058487290 ) ) ;
#70213 = CARTESIAN_POINT ( 'NONE',  ( -19.65312891409030271, 93.06504152958497400, -10.00000000000000888 ) ) ;
#70214 = EDGE_CURVE ( 'NONE', #92543, #54381, #44633, .T. ) ;
#70215 = EDGE_LOOP ( 'NONE', ( #6819, #80896, #14517, #64301 ) ) ;
#70216 = ADVANCED_FACE ( 'NONE', ( #61831 ), #60330, .T. ) ;
#70217 = VERTEX_POINT ( 'NONE', #87228 ) ;
#70218 = CARTESIAN_POINT ( 'NONE',  ( 175.6456982650794885, 258.5815163761128019, 13.11329590940762202 ) ) ;
#70219 = ORIENTED_EDGE ( 'NONE', *, *, #10692, .F. ) ;
#70220 = CARTESIAN_POINT ( 'NONE',  ( 77.14916621374221961, 49.44515670615653136, -15.44477560956883799 ) ) ;
#70221 = VECTOR ( 'NONE', #11139, 1000.000000000000227 ) ;
#70222 = EDGE_LOOP ( 'NONE', ( #21946, #96474, #2639, #23862 ) ) ;
#70223 = CARTESIAN_POINT ( 'NONE',  ( 87.00169912441755571, 45.80253757415765392, -8.636720921146656238 ) ) ;
#70224 = CARTESIAN_POINT ( 'NONE',  ( 78.92544819766602870, 51.82601731205822659, 15.40366229040229484 ) ) ;
#70225 = VERTEX_POINT ( 'NONE', #32940 ) ;
#70226 = LINE ( 'NONE', #99155, #41072 ) ;
#70227 = CARTESIAN_POINT ( 'NONE',  ( 206.6347703933553532, 272.7450743988160866, -10.98802705318387574 ) ) ;
#70228 = CARTESIAN_POINT ( 'NONE',  ( 190.7101769558895512, 300.3272793223849249, 2.683020982371553398 ) ) ;
#70229 = CARTESIAN_POINT ( 'NONE',  ( 148.9266665119372703, 272.6984423298952152, 12.06339424062075061 ) ) ;
#70230 = CARTESIAN_POINT ( 'NONE',  ( 82.81737761417261368, 40.62361263855670046, 0.9906565628550747515 ) ) ;
#70231 = LINE ( 'NONE', #99660, #62437 ) ;
#70232 = CARTESIAN_POINT ( 'NONE',  ( 44.35726076638960080, 207.9637435831424455, 2.679491924311251605 ) ) ;
#70233 = CIRCLE ( 'NONE', #21657, 10.00000000000007816 ) ;
#70234 = CARTESIAN_POINT ( 'NONE',  ( 186.8168172874784716, 287.0359679780673332, -15.71538299017341522 ) ) ;
#70235 = CARTESIAN_POINT ( 'NONE',  ( 123.0428377395863890, 241.8458772461660544, 9.188101187500095079 ) ) ;
#70236 = CARTESIAN_POINT ( 'NONE',  ( 70.67277294938870114, 60.56909423328382047, -14.64600609532338993 ) ) ;
#70237 = CARTESIAN_POINT ( 'NONE',  ( 36.06377727768691699, 41.79752408145595410, -5.678558825948271327 ) ) ;
#70238 = CARTESIAN_POINT ( 'NONE',  ( 177.1851276373975566, 289.0245988117038110, -10.43460913673951218 ) ) ;
#70239 = VERTEX_POINT ( 'NONE', #47137 ) ;
#70241 = ORIENTED_EDGE ( 'NONE', *, *, #54380, .T. ) ;
#70240 = CARTESIAN_POINT ( 'NONE',  ( 29.12701137275935181, 44.61184105132205957, -10.00000000000000000 ) ) ;
#70242 = CARTESIAN_POINT ( 'NONE',  ( 200.0814620334770098, 273.7332971121043101, 13.81105051205792122 ) ) ;
#70243 = CARTESIAN_POINT ( 'NONE',  ( 177.6597045081098827, 253.3888418680545556, 1.386942453458301250 ) ) ;
#70244 = DIRECTION ( 'NONE',  ( -0.000000000000000000, 0.000000000000000000, -1.000000000000000000 ) ) ;
#70245 = CARTESIAN_POINT ( 'NONE',  ( 146.9460647107688658, 276.1289452790811652, 2.604800266209711168 ) ) ;
#70246 = CARTESIAN_POINT ( 'NONE',  ( 71.75200176415748388, 60.74830010697920812, 14.83125165669016177 ) ) ;
#70247 = CARTESIAN_POINT ( 'NONE',  ( 66.51217979237357270, 68.21896002327083863, 4.555124048972479578 ) ) ;
#70248 = CARTESIAN_POINT ( 'NONE',  ( 174.4665098196985298, 288.5002641398569949, -10.08633113632384237 ) ) ;
#70249 = CARTESIAN_POINT ( 'NONE',  ( 36.94473716931751284, 21.73415679381824361, -6.890680421881970419E-14 ) ) ;
#70250 = DIRECTION ( 'NONE',  ( 0.000000000000000000, 0.000000000000000000, 1.000000000000000000 ) ) ;
#70251 = ORIENTED_EDGE ( 'NONE', *, *, #7239, .F. ) ;
#70252 = CARTESIAN_POINT ( 'NONE',  ( 148.1829914015846157, 273.9865254053503349, -9.304102644963160529 ) ) ;
#70253 = CARTESIAN_POINT ( 'NONE',  ( 12.50963621419470329, 166.4824982072973967, 3.021315404115420679E-15 ) ) ;
#70254 = ORIENTED_EDGE ( 'NONE', *, *, #97232, .F. ) ;
#70255 = DIRECTION ( 'NONE',  ( -0.000000000000000000, -0.000000000000000000, -1.000000000000000000 ) ) ;
#70256 = CARTESIAN_POINT ( 'NONE',  ( 160.2824175349068412, 279.0229062109438587, 10.59256730584001716 ) ) ;
#70257 = CARTESIAN_POINT ( 'NONE',  ( 180.4572463832561482, 261.7460625851787199, -13.63662180976220384 ) ) ;
#70258 = CARTESIAN_POINT ( 'NONE',  ( 190.0226014859668453, 301.5181949703289774, 3.835066345245774500 ) ) ;
#70259 = CARTESIAN_POINT ( 'NONE',  ( 13.42747647338834760, 171.8927522451418213, -10.00000000000009237 ) ) ;
#70261 = CARTESIAN_POINT ( 'NONE',  ( 160.8788117166195661, 281.5922145059649893, 5.693820771016479654 ) ) ;
#70260 = CARTESIAN_POINT ( 'NONE',  ( 153.3273301907053394, 270.2101081292901767, 14.04008172480431327 ) ) ;
#70262 = CARTESIAN_POINT ( 'NONE',  ( -17.42236680055705023, 149.2012482093457777, 0.000000000000000000 ) ) ;
#70263 = ORIENTED_EDGE ( 'NONE', *, *, #4583, .T. ) ;
#70264 = CARTESIAN_POINT ( 'NONE',  ( 190.9335643195044838, 299.9403610588350944, -4.692880224846124548 ) ) ;
#70265 = CARTESIAN_POINT ( 'NONE',  ( 73.25245674375855742, 68.31447868205536622, 10.71232302521148405 ) ) ;
#70266 = CARTESIAN_POINT ( 'NONE',  ( 72.15234558402282516, 59.70125055744302500, 15.74980178838212730 ) ) ;
#70267 = CARTESIAN_POINT ( 'NONE',  ( 193.5643139362479701, 276.1245741781895617, -16.51112113933535497 ) ) ;
#70268 = CARTESIAN_POINT ( 'NONE',  ( 31.61400995286156501, 182.3927522451417644, -10.00000000000009237 ) ) ;
#70269 = CARTESIAN_POINT ( 'NONE',  ( 184.5863935663384154, 297.1395876791133333, -4.463175273155427725 ) ) ;
#70270 = CARTESIAN_POINT ( 'NONE',  ( 192.4202172926039793, 297.3654025762033370, 10.98569444949570872 ) ) ;
#70271 = CARTESIAN_POINT ( 'NONE',  ( 58.82164138842269097, 194.7677522451418213, -5.000000000000041744 ) ) ;
#70272 = CARTESIAN_POINT ( 'NONE',  ( 74.11561865490956791, 68.62363639872573629, 10.95723244528671714 ) ) ;
#70273 = CARTESIAN_POINT ( 'NONE',  ( 71.85042758235270810, 71.69843285251393183, -3.789477364735254650 ) ) ;
#70274 = CARTESIAN_POINT ( 'NONE',  ( -1.691623377417284635, 160.6423013555410080, -4.594050593750043987 ) ) ;
#70275 = CARTESIAN_POINT ( 'NONE',  ( 95.22211873877630239, 213.5327760586659451, 1.948934522072303157E-15 ) ) ;
#70276 = CARTESIAN_POINT ( 'NONE',  ( 203.3041373168503299, 278.5139001086923827, -16.61929732091214973 ) ) ;
#70277 = CARTESIAN_POINT ( 'NONE',  ( 193.0065576635309412, 296.3498312632291913, -11.90044991639595295 ) ) ;
#70278 = DIRECTION ( 'NONE',  ( -0.9756173257765569096, -0.2194785493951510180, 0.000000000000000000 ) ) ;
#70279 = EDGE_CURVE ( 'NONE', #5574, #79014, #552, .T. ) ;
#70280 = DIRECTION ( 'NONE',  ( -0.000000000000000000, -0.000000000000000000, 1.000000000000000000 ) ) ;
#70281 = CARTESIAN_POINT ( 'NONE',  ( 78.30031128316109346, 56.39945258195061228, 16.19534353207165012 ) ) ;
#70282 = CARTESIAN_POINT ( 'NONE',  ( 84.88560255493293027, 50.09086853330895650, -13.26386351457619206 ) ) ;
#70283 = CARTESIAN_POINT ( 'NONE',  ( 47.99632384111720995, 188.5177522451417929, 5.000000000000051514 ) ) ;
#70285 = CARTESIAN_POINT ( 'NONE',  ( 76.18389692386300283, 51.34301906948758187, 15.63209118771619366 ) ) ;
#70284 = DIRECTION ( 'NONE',  ( -0.000000000000000000, -0.000000000000000000, -1.000000000000000000 ) ) ;
#70286 = CARTESIAN_POINT ( 'NONE',  ( 207.7086642703471568, 270.8850356419295053, 6.393550561233467100 ) ) ;
#70287 = EDGE_CURVE ( 'NONE', #4641, #72984, #94783, .T. ) ;
#70288 = CARTESIAN_POINT ( 'NONE',  ( 168.1679099710297578, 251.3796770727044247, -8.814879634955225640 ) ) ;
#70289 = CARTESIAN_POINT ( 'NONE',  ( 164.1514344399216725, 246.3283707451809903, -4.343706172463206450 ) ) ;
#70290 =( BOUNDED_SURFACE ( )  B_SPLINE_SURFACE ( 1, 2, ( 
 ( #20612, #81937, #51493, #52987, #67189, #91036, #92044, #35798, #13515, #83432, #6886, #60074, #83935, #66692, #68678, #13998, #44877, #75817, #6402, #12515, #90550, #98624, #59575, #43387, #82462, #60569, #37286, #36787, #13024, #74329, #43887, #68181, #99110, #4918, #29693, #36290, #98113, #99609, #91525, #22089, #45381, #30187, #97628, #28192, #74826, #28698, #21122, #51998, #75316, #67696, #16483, #61574, #14975, #84922, #62063, #69681, #8884, #47865, #32682, #39752, #45862, #779, #78802, #93012, #47377, #38269, #31666, #92525, #63582, #23566, #85956, #31173, #69180, #7900, #39260, #55462, #9390, #54457, #100110, #93525, #40266, #76787, #1798, #24579, #85436, #22589, #15985, #62562, #16974, #53479, #71206, #70172, #46884, #78302, #24082, #30694, #84430, #54978, #70681, #285, #1295, #77809, #8392, #32180, #7380, #63083, #94028, #86449, #23071, #53965, #15468, #46363, #77292, #38775, #64087, #57470, #25595, #88453, #26596, #2306, #33703, #27098, #65580, #79830, #41267, #18501, #10398, #49387, #25076, #34678, #55956, #33187, #86951, #3313, #80332, #17484, #9905, #50378, #48896, #56481, #34193, #19012, #49886, #48392, #87956, #95031, #64596, #4276, #87469, #10900, #57981, #65084, #79335, #35175, #42760, #11415, #80845, #18004, #42269, #96528, #73202, #3797, #72210, #73692, #95549, #81331, #88964, #11903, #94524, #19518, #40763, #71714, #2814, #72722, #26097, #56971, #41776, #96035, #91405, #75688, #37169, #89439, #52863, #29091, #36165, #12398, #43264, #21970, #83813, #75197, #44755, #67568, #82338, #36661, #67068, #13394, #52367, #20498, #97992, #21004, #51370, #6274, #14380, #5772, #66581, #97505, #6774, #74209, #66086, #21479, #45264, #98991, #59451, #51885, #68067, #44265, #83312, #76198, #35680, #90929, #90432, #29574, #13874, #5286, #97032, #4799, #60452, #58467, #59957, #27601, #98501, #19995, #12906, #50874, #81823, #74709, #28075, #58947, #28571, #89918, #43765, #82826, #31552, #78685, #15345, #99489, #8769, #77691, #8274, #47748, #22470, #172, #39139, #62963, #15858, #70560, #53364, #55347, #70052, #667, #62441, #46765, #37653, #77167, #85312, #46241, #68564, #76673, #47259, #93408, #92897, #7260, #30067, #38143, #23957, #54860, #60956, #85838, #92408, #22956, #93913, #16368, #78180, #1177, #16861, #39638, #32051, #91915, #24467, #86324, #84314, #14861, #69565, #45748, #69060, #99989, #30573, #7769, #84805, #61458, #53845, #38662, #31056, #61945, #23450, #54340, #48781, #34085, #24958, #87840, #48269, #50257, #79713, #72596, #17883, #55834, #94902, #25984, #42153, #65461, #10276, #86829, #80211, #96403, #63468, #88834, #11294, #41146, #19398, #72084, #49274, #3682, #9274, #34561, #56854, #2685, #3201, #10779, #17362, #40147, #18379, #64975, #87354, #41654, #33576, #64471, #95918, #26972, #95431, #26478, #73088, #79216, #71088, #1687, #88330, #32572, #57354, #9790, #18885, #40650, #49765, #80720, #71588, #2183, #33066, #57854, #94404, #63960, #25465, #56354, #47437, #78870, #8946, #9455, #49442, #63645, #25661, #40326, #39814, #87016, #41331, #17544, #94088, #32740, #64146, #80397, #3377, #48453, #55521, #64658, #65146, #63143, #70746, #10967, #79396, #71266, #40824, #57032, #25137, #71768, #2368 ),
 ( #88015, #33245, #95097, #56540, #18564, #59516, #75256, #59011, #19577, #50438, #60019, #27158, #19074, #74769, #67630, #51944, #12460, #4861, #28631, #97569, #36228, #36725, #89027, #43829, #43331, #21067, #5347, #58529, #49948, #96595, #90494, #11478, #12968, #5836, #51436, #82883, #35241, #89978, #20557, #27661, #82402, #98563, #50934, #81393, #13458, #11959, #67133, #80906, #97092, #42332, #44324, #98055, #20061, #29148, #73259, #66145, #81883, #74277, #35743, #66639, #3854, #34738, #65639, #58045, #42821, #28138, #73752, #52426, #6337, #46824, #45321, #52926, #30633, #15406, #53906, #83373, #84368, #29636, #61009, #719, #99054, #76729, #54397, #61519, #75753, #31607, #39198, #7833, #77226, #60509, #46300, #99544, #92465, #77747, #22531, #68622, #92952, #91466, #90983, #13937, #69620, #21543, #38714, #22026, #84864, #83878, #227, #23011, #14440, #76256, #37228, #31112, #62000, #23505, #30126, #91981, #70110, #6828, #44817, #37713, #85374, #53419, #15918, #68126, #14916, #45805, #8330, #7322, #69120, #38201, #100047, #80273, #64027, #2247, #94968, #40712, #3256, #1747, #9853, #71148, #62497, #1231, #72147, #33126, #17423, #32113, #93467, #63023, #25533, #56420, #72661, #17945, #16918, #47806, #18444, #87417, #48844, #95491, #41715, #71655, #26043, #24019, #49333, #79776, #87900, #10341, #94463, #41207, #93968, #54917, #24521, #32626, #9330, #2750, #10837, #85896, #33641, #16421, #64533, #47316, #63524, #56913, #78241, #8822, #55400, #39690, #25016, #70619, #55896, #86385, #78741, #79279, #40202, #86889, #48332, #26540, #96470, #11843, #95978, #42701, #50318, #42212, #73633, #73148, #65520, #81269, #34138, #65032, #57920, #27035, #57413, #19461, #49827, #88394, #18948, #80784, #88899, #11358, #3745, #34620, #17800, #63385, #71508, #16281, #71006, #1608, #39556, #94325, #10199, #62876, #586, #32979, #23873, #24880, #72000, #8687, #92817, #2099, #32494, #70480, #63884, #94820, #47175, #78096, #55261, #1094, #86243, #61866, #25384, #23371, #69972, #54257, #40064, #16779, #85228, #46680, #87269, #85752, #93319, #55754, #86747, #17281, #15774, #24388, #31471, #31971, #41063, #39059, #47671, #56272, #48185, #77606, #30979, #79633, #79131, #9711, #62362, #40568, #48699, #8191, #54773, #93834, #78603, #9189, #91095, #73997, #60135, #83494, #34971, #49199, #65873, #21663, #81136, #34010, #18797, #14060, #98685, #29265, #12193, #5960, #25907, #52543, #96829, #73011, #80133, #10696, #44941, #2605, #11702, #81620, #4079, #49679, #73496, #3603, #50182, #89251, #57273, #34482, #57772, #88249, #43052, #33493, #42562, #3125, #64895, #64388, #41575, #95352, #58275, #56779, #36851, #96324, #88746, #67760, #27392, #19801, #87762, #72516, #50668, #26894, #18301, #95841, #42079, #26396, #80635, #11212, #65381, #19319, #8450, #55033, #23130, #39321, #16542, #62626, #54025, #841, #46427, #7441, #69739, #14564, #68244, #37837, #15034, #22657, #62122, #31722, #86015, #93070, #99168, #84980, #93581, #45926, #348, #91582, #15526, #45439, #75885, #76843, #38833, #84491, #22156, #61135, #92587, #70237, #24148, #38333, #53046, #77352, #6463, #29756, #37342, #77864, #69241, #60628, #100171, #7959, #84003, #76374, #6945, #31236, #30757 ) ),
 .UNSPECIFIED., .F., .F., .T. ) 
 B_SPLINE_SURFACE_WITH_KNOTS ( ( 2, 2 ),
 ( 3, 2, 2, 2, 2, 2, 2, 2, 2, 2, 2, 2, 2, 2, 2, 2, 2, 2, 2, 2, 2, 2, 2, 2, 2, 2, 2, 2, 2, 2, 2, 2, 2, 2, 2, 2, 2, 2, 2, 2, 2, 2, 2, 2, 2, 2, 2, 2, 2, 2, 2, 2, 2, 2, 2, 2, 2, 2, 2, 2, 2, 2, 2, 2, 2, 2, 2, 2, 2, 2, 2, 2, 2, 2, 2, 2, 2, 2, 2, 2, 2, 2, 2, 2, 2, 2, 2, 2, 2, 2, 2, 2, 2, 2, 2, 2, 2, 2, 2, 2, 2, 2, 2, 2, 2, 2, 2, 2, 2, 2, 2, 2, 2, 2, 2, 2, 2, 2, 2, 2, 2, 2, 2, 2, 2, 2, 2, 2, 2, 2, 2, 2, 2, 2, 2, 2, 2, 2, 2, 2, 2, 2, 2, 2, 2, 2, 2, 2, 2, 2, 2, 2, 2, 2, 2, 2, 2, 2, 2, 2, 2, 2, 2, 2, 2, 2, 2, 2, 2, 2, 2, 2, 2, 2, 2, 2, 2, 2, 2, 2, 2, 2, 2, 2, 2, 2, 2, 2, 2, 2, 2, 2, 2, 2, 2, 2, 2, 2, 2, 2, 3 ),
 ( 0.000000000000000000, 1.000000000000000000 ),
 ( 0.000000000000000000, 0.005000000000000000104, 0.01000000000000000021, 0.01499999999999999944, 0.02000000000000000042, 0.02500000000000000139, 0.02999999999999999889, 0.03500000000000000333, 0.04000000000000000083, 0.04499999999999999833, 0.05000000000000000278, 0.05500000000000000028, 0.05999999999999999778, 0.06500000000000000222, 0.07000000000000000666, 0.07499999999999999722, 0.08000000000000000167, 0.08500000000000000611, 0.08999999999999999667, 0.09500000000000000111, 0.1000000000000000056, 0.1049999999999999961, 0.1100000000000000006, 0.1150000000000000050, 0.1199999999999999956, 0.1250000000000000000, 0.1300000000000000044, 0.1350000000000000089, 0.1400000000000000133, 0.1449999999999999900, 0.1499999999999999944, 0.1549999999999999989, 0.1600000000000000033, 0.1650000000000000078, 0.1700000000000000122, 0.1749999999999999889, 0.1799999999999999933, 0.1849999999999999978, 0.1900000000000000022, 0.1950000000000000067, 0.2000000000000000111, 0.2049999999999999878, 0.2099999999999999922, 0.2149999999999999967, 0.2200000000000000011, 0.2250000000000000056, 0.2300000000000000100, 0.2349999999999999867, 0.2399999999999999911, 0.2449999999999999956, 0.2500000000000000000, 0.2550000000000000044, 0.2600000000000000089, 0.2650000000000000133, 0.2700000000000000178, 0.2750000000000000222, 0.2800000000000000266, 0.2849999999999999756, 0.2899999999999999800, 0.2949999999999999845, 0.2999999999999999889, 0.3049999999999999933, 0.3099999999999999978, 0.3150000000000000022, 0.3200000000000000067, 0.3250000000000000111, 0.3300000000000000155, 0.3350000000000000200, 0.3400000000000000244, 0.3449999999999999734, 0.3499999999999999778, 0.3549999999999999822, 0.3599999999999999867, 0.3649999999999999911, 0.3699999999999999956, 0.3750000000000000000, 0.3800000000000000044, 0.3850000000000000089, 0.3900000000000000133, 0.3950000000000000178, 0.4000000000000000222, 0.4050000000000000266, 0.4099999999999999756, 0.4149999999999999800, 0.4199999999999999845, 0.4249999999999999889, 0.4299999999999999933, 0.4349999999999999978, 0.4400000000000000022, 0.4450000000000000067, 0.4500000000000000111, 0.4550000000000000155, 0.4600000000000000200, 0.4650000000000000244, 0.4699999999999999734, 0.4749999999999999778, 0.4799999999999999822, 0.4849999999999999867, 0.4899999999999999911, 0.4949999999999999956, 0.5000000000000000000, 0.5050000000000000044, 0.5100000000000000089, 0.5150000000000000133, 0.5200000000000000178, 0.5250000000000000222, 0.5300000000000000266, 0.5350000000000000311, 0.5400000000000000355, 0.5450000000000000400, 0.5500000000000000444, 0.5550000000000000488, 0.5600000000000000533, 0.5649999999999999467, 0.5699999999999999512, 0.5749999999999999556, 0.5799999999999999600, 0.5849999999999999645, 0.5899999999999999689, 0.5949999999999999734, 0.5999999999999999778, 0.6049999999999999822, 0.6099999999999999867, 0.6149999999999999911, 0.6199999999999999956, 0.6250000000000000000, 0.6300000000000000044, 0.6350000000000000089, 0.6400000000000000133, 0.6450000000000000178, 0.6500000000000000222, 0.6550000000000000266, 0.6600000000000000311, 0.6650000000000000355, 0.6700000000000000400, 0.6750000000000000444, 0.6800000000000000488, 0.6850000000000000533, 0.6899999999999999467, 0.6949999999999999512, 0.6999999999999999556, 0.7049999999999999600, 0.7099999999999999645, 0.7149999999999999689, 0.7199999999999999734, 0.7249999999999999778, 0.7299999999999999822, 0.7349999999999999867, 0.7399999999999999911, 0.7449999999999999956, 0.7500000000000000000, 0.7550000000000000044, 0.7600000000000000089, 0.7650000000000000133, 0.7700000000000000178, 0.7750000000000000222, 0.7800000000000000266, 0.7850000000000000311, 0.7900000000000000355, 0.7950000000000000400, 0.8000000000000000444, 0.8050000000000000488, 0.8100000000000000533, 0.8149999999999999467, 0.8199999999999999512, 0.8249999999999999556, 0.8299999999999999600, 0.8349999999999999645, 0.8399999999999999689, 0.8449999999999999734, 0.8499999999999999778, 0.8549999999999999822, 0.8599999999999999867, 0.8649999999999999911, 0.8699999999999999956, 0.8750000000000000000, 0.8800000000000000044, 0.8850000000000000089, 0.8900000000000000133, 0.8950000000000000178, 0.9000000000000000222, 0.9050000000000000266, 0.9100000000000000311, 0.9150000000000000355, 0.9200000000000000400, 0.9250000000000000444, 0.9300000000000000488, 0.9350000000000000533, 0.9399999999999999467, 0.9449999999999999512, 0.9499999999999999556, 0.9549999999999999600, 0.9599999999999999645, 0.9649999999999999689, 0.9699999999999999734, 0.9749999999999999778, 0.9799999999999999822, 0.9849999999999999867, 0.9899999999999999911, 0.9949999999999999956, 1.000000000000000000 ),
 .UNSPECIFIED. ) 
 GEOMETRIC_REPRESENTATION_ITEM ( )  RATIONAL_B_SPLINE_SURFACE ( (
 ( 1.000000000000000000, 0.9510565162951535312, 1.000000000000000000, 0.9510565162951535312, 1.000000000000000000, 0.9510565162951535312, 1.000000000000000000, 0.9510565162951535312, 1.000000000000000000, 0.9510565162951535312, 1.000000000000000000, 0.9510565162951535312, 1.000000000000000000, 0.9510565162951535312, 1.000000000000000000, 0.9510565162951535312, 1.000000000000000000, 0.9510565162951535312, 1.000000000000000000, 0.9510565162951535312, 1.000000000000000000, 0.9510565162951535312, 1.000000000000000000, 0.9510565162951535312, 1.000000000000000000, 0.9510565162951535312, 1.000000000000000000, 0.9510565162951535312, 1.000000000000000000, 0.9510565162951535312, 1.000000000000000000, 0.9510565162951535312, 1.000000000000000000, 0.9510565162951535312, 1.000000000000000000, 0.9510565162951535312, 1.000000000000000000, 0.9510565162951535312, 1.000000000000000000, 0.9510565162951535312, 1.000000000000000000, 0.9510565162951535312, 1.000000000000000000, 0.9510565162951535312, 1.000000000000000000, 0.9510565162951535312, 1.000000000000000000, 0.9510565162951535312, 1.000000000000000000, 0.9510565162951535312, 1.000000000000000000, 0.9510565162951535312, 1.000000000000000000, 0.9510565162951535312, 1.000000000000000000, 0.9510565162951535312, 1.000000000000000000, 0.9510565162951535312, 1.000000000000000000, 0.9510565162951535312, 1.000000000000000000, 0.9510565162951535312, 1.000000000000000000, 0.9510565162951535312, 1.000000000000000000, 0.9510565162951535312, 1.000000000000000000, 0.9510565162951535312, 1.000000000000000000, 0.9510565162951535312, 1.000000000000000000, 0.9510565162951535312, 1.000000000000000000, 0.9510565162951535312, 1.000000000000000000, 0.9510565162951535312, 1.000000000000000000, 0.9510565162951535312, 1.000000000000000000, 0.9510565162951535312, 1.000000000000000000, 0.9510565162951535312, 1.000000000000000000, 0.9510565162951535312, 1.000000000000000000, 0.9510565162951535312, 1.000000000000000000, 0.9510565162951535312, 1.000000000000000000, 0.9510565162951535312, 1.000000000000000000, 0.9510565162951535312, 1.000000000000000000, 0.9510565162951535312, 1.000000000000000000, 0.9510565162951535312, 1.000000000000000000, 0.9510565162951535312, 1.000000000000000000, 0.9510565162951535312, 1.000000000000000000, 0.9510565162951535312, 1.000000000000000000, 0.9510565162951535312, 1.000000000000000000, 0.9510565162951535312, 1.000000000000000000, 0.9510565162951535312, 1.000000000000000000, 0.9510565162951535312, 1.000000000000000000, 0.9510565162951535312, 1.000000000000000000, 0.9510565162951535312, 1.000000000000000000, 0.9510565162951535312, 1.000000000000000000, 0.9510565162951535312, 1.000000000000000000, 0.9510565162951535312, 1.000000000000000000, 0.9510565162951535312, 1.000000000000000000, 0.9510565162951535312, 1.000000000000000000, 0.9510565162951535312, 1.000000000000000000, 0.9510565162951535312, 1.000000000000000000, 0.9510565162951535312, 1.000000000000000000, 0.9510565162951535312, 1.000000000000000000, 0.9510565162951535312, 1.000000000000000000, 0.9510565162951535312, 1.000000000000000000, 0.9510565162951535312, 1.000000000000000000, 0.9510565162951535312, 1.000000000000000000, 0.9510565162951535312, 1.000000000000000000, 0.9510565162951535312, 1.000000000000000000, 0.9510565162951535312, 1.000000000000000000, 0.9510565162951535312, 1.000000000000000000, 0.9510565162951535312, 1.000000000000000000, 0.9510565162951535312, 1.000000000000000000, 0.9510565162951535312, 1.000000000000000000, 0.9510565162951535312, 1.000000000000000000, 0.9510565162951535312, 1.000000000000000000, 0.9510565162951535312, 1.000000000000000000, 0.9510565162951535312, 1.000000000000000000, 0.9510565162951535312, 1.000000000000000000, 0.9510565162951535312, 1.000000000000000000, 0.9510565162951535312, 1.000000000000000000, 0.9510565162951535312, 1.000000000000000000, 0.9510565162951535312, 1.000000000000000000, 0.9510565162951535312, 1.000000000000000000, 0.9510565162951535312, 1.000000000000000000, 0.9510565162951535312, 1.000000000000000000, 0.9510565162951535312, 1.000000000000000000, 0.9510565162951535312, 1.000000000000000000, 0.9510565162951535312, 1.000000000000000000, 0.9510565162951535312, 1.000000000000000000, 0.9510565162951535312, 1.000000000000000000, 0.9510565162951535312, 1.000000000000000000, 0.9510565162951535312, 1.000000000000000000, 0.9510565162951535312, 1.000000000000000000, 0.9510565162951535312, 1.000000000000000000, 0.9510565162951535312, 1.000000000000000000, 0.9510565162951535312, 1.000000000000000000, 0.9510565162951535312, 1.000000000000000000, 0.9510565162951535312, 1.000000000000000000, 0.9510565162951535312, 1.000000000000000000, 0.9510565162951535312, 1.000000000000000000, 0.9510565162951535312, 1.000000000000000000, 0.9510565162951535312, 1.000000000000000000, 0.9510565162951535312, 1.000000000000000000, 0.9510565162951535312, 1.000000000000000000, 0.9510565162951535312, 1.000000000000000000, 0.9510565162951535312, 1.000000000000000000, 0.9510565162951535312, 1.000000000000000000, 0.9510565162951535312, 1.000000000000000000, 0.9510565162951535312, 1.000000000000000000, 0.9510565162951535312, 1.000000000000000000, 0.9510565162951535312, 1.000000000000000000, 0.9510565162951535312, 1.000000000000000000, 0.9510565162951535312, 1.000000000000000000, 0.9510565162951535312, 1.000000000000000000, 0.9510565162951535312, 1.000000000000000000, 0.9510565162951535312, 1.000000000000000000, 0.9510565162951535312, 1.000000000000000000, 0.9510565162951535312, 1.000000000000000000, 0.9510565162951535312, 1.000000000000000000, 0.9510565162951535312, 1.000000000000000000, 0.9510565162951535312, 1.000000000000000000, 0.9510565162951535312, 1.000000000000000000, 0.9510565162951535312, 1.000000000000000000, 0.9510565162951535312, 1.000000000000000000, 0.9510565162951535312, 1.000000000000000000, 0.9510565162951535312, 1.000000000000000000, 0.9510565162951535312, 1.000000000000000000, 0.9510565162951535312, 1.000000000000000000, 0.9510565162951535312, 1.000000000000000000, 0.9510565162951535312, 1.000000000000000000, 0.9510565162951535312, 1.000000000000000000, 0.9510565162951535312, 1.000000000000000000, 0.9510565162951535312, 1.000000000000000000, 0.9510565162951535312, 1.000000000000000000, 0.9510565162951535312, 1.000000000000000000, 0.9510565162951535312, 1.000000000000000000, 0.9510565162951535312, 1.000000000000000000, 0.9510565162951535312, 1.000000000000000000, 0.9510565162951535312, 1.000000000000000000, 0.9510565162951535312, 1.000000000000000000, 0.9510565162951535312, 1.000000000000000000, 0.9510565162951535312, 1.000000000000000000, 0.9510565162951535312, 1.000000000000000000, 0.9510565162951535312, 1.000000000000000000, 0.9510565162951535312, 1.000000000000000000, 0.9510565162951535312, 1.000000000000000000, 0.9510565162951535312, 1.000000000000000000, 0.9510565162951535312, 1.000000000000000000, 0.9510565162951535312, 1.000000000000000000, 0.9510565162951535312, 1.000000000000000000, 0.9510565162951535312, 1.000000000000000000, 0.9510565162951535312, 1.000000000000000000, 0.9510565162951535312, 1.000000000000000000, 0.9510565162951535312, 1.000000000000000000, 0.9510565162951535312, 1.000000000000000000, 0.9510565162951535312, 1.000000000000000000, 0.9510565162951535312, 1.000000000000000000, 0.9510565162951535312, 1.000000000000000000, 0.9510565162951535312, 1.000000000000000000, 0.9510565162951535312, 1.000000000000000000, 0.9510565162951535312, 1.000000000000000000, 0.9510565162951535312, 1.000000000000000000, 0.9510565162951535312, 1.000000000000000000, 0.9510565162951535312, 1.000000000000000000, 0.9510565162951535312, 1.000000000000000000, 0.9510565162951535312, 1.000000000000000000, 0.9510565162951535312, 1.000000000000000000, 0.9510565162951535312, 1.000000000000000000, 0.9510565162951535312, 1.000000000000000000, 0.9510565162951535312, 1.000000000000000000, 0.9510565162951535312, 1.000000000000000000, 0.9510565162951535312, 1.000000000000000000, 0.9510565162951535312, 1.000000000000000000, 0.9510565162951535312, 1.000000000000000000, 0.9510565162951535312, 1.000000000000000000, 0.9510565162951535312, 1.000000000000000000, 0.9510565162951535312, 1.000000000000000000, 0.9510565162951535312, 1.000000000000000000, 0.9510565162951535312, 1.000000000000000000, 0.9510565162951535312, 1.000000000000000000, 0.9510565162951535312, 1.000000000000000000, 0.9510565162951535312, 1.000000000000000000, 0.9510565162951535312, 1.000000000000000000, 0.9510565162951535312, 1.000000000000000000, 0.9510565162951535312, 1.000000000000000000, 0.9510565162951535312, 1.000000000000000000, 0.9510565162951535312, 1.000000000000000000, 0.9510565162951535312, 1.000000000000000000, 0.9510565162951535312, 1.000000000000000000, 0.9510565162951535312, 1.000000000000000000, 0.9510565162951535312, 1.000000000000000000, 0.9510565162951535312, 1.000000000000000000, 0.9510565162951535312, 1.000000000000000000, 0.9510565162951535312, 1.000000000000000000, 0.9510565162951535312, 1.000000000000000000, 0.9510565162951535312, 1.000000000000000000),
 ( 1.000000000000000000, 0.9510565162951535312, 1.000000000000000000, 0.9510565162951535312, 1.000000000000000000, 0.9510565162951535312, 1.000000000000000000, 0.9510565162951535312, 1.000000000000000000, 0.9510565162951535312, 1.000000000000000000, 0.9510565162951535312, 1.000000000000000000, 0.9510565162951535312, 1.000000000000000000, 0.9510565162951535312, 1.000000000000000000, 0.9510565162951535312, 1.000000000000000000, 0.9510565162951535312, 1.000000000000000000, 0.9510565162951535312, 1.000000000000000000, 0.9510565162951535312, 1.000000000000000000, 0.9510565162951535312, 1.000000000000000000, 0.9510565162951535312, 1.000000000000000000, 0.9510565162951535312, 1.000000000000000000, 0.9510565162951535312, 1.000000000000000000, 0.9510565162951535312, 1.000000000000000000, 0.9510565162951535312, 1.000000000000000000, 0.9510565162951535312, 1.000000000000000000, 0.9510565162951535312, 1.000000000000000000, 0.9510565162951535312, 1.000000000000000000, 0.9510565162951535312, 1.000000000000000000, 0.9510565162951535312, 1.000000000000000000, 0.9510565162951535312, 1.000000000000000000, 0.9510565162951535312, 1.000000000000000000, 0.9510565162951535312, 1.000000000000000000, 0.9510565162951535312, 1.000000000000000000, 0.9510565162951535312, 1.000000000000000000, 0.9510565162951535312, 1.000000000000000000, 0.9510565162951535312, 1.000000000000000000, 0.9510565162951535312, 1.000000000000000000, 0.9510565162951535312, 1.000000000000000000, 0.9510565162951535312, 1.000000000000000000, 0.9510565162951535312, 1.000000000000000000, 0.9510565162951535312, 1.000000000000000000, 0.9510565162951535312, 1.000000000000000000, 0.9510565162951535312, 1.000000000000000000, 0.9510565162951535312, 1.000000000000000000, 0.9510565162951535312, 1.000000000000000000, 0.9510565162951535312, 1.000000000000000000, 0.9510565162951535312, 1.000000000000000000, 0.9510565162951535312, 1.000000000000000000, 0.9510565162951535312, 1.000000000000000000, 0.9510565162951535312, 1.000000000000000000, 0.9510565162951535312, 1.000000000000000000, 0.9510565162951535312, 1.000000000000000000, 0.9510565162951535312, 1.000000000000000000, 0.9510565162951535312, 1.000000000000000000, 0.9510565162951535312, 1.000000000000000000, 0.9510565162951535312, 1.000000000000000000, 0.9510565162951535312, 1.000000000000000000, 0.9510565162951535312, 1.000000000000000000, 0.9510565162951535312, 1.000000000000000000, 0.9510565162951535312, 1.000000000000000000, 0.9510565162951535312, 1.000000000000000000, 0.9510565162951535312, 1.000000000000000000, 0.9510565162951535312, 1.000000000000000000, 0.9510565162951535312, 1.000000000000000000, 0.9510565162951535312, 1.000000000000000000, 0.9510565162951535312, 1.000000000000000000, 0.9510565162951535312, 1.000000000000000000, 0.9510565162951535312, 1.000000000000000000, 0.9510565162951535312, 1.000000000000000000, 0.9510565162951535312, 1.000000000000000000, 0.9510565162951535312, 1.000000000000000000, 0.9510565162951535312, 1.000000000000000000, 0.9510565162951535312, 1.000000000000000000, 0.9510565162951535312, 1.000000000000000000, 0.9510565162951535312, 1.000000000000000000, 0.9510565162951535312, 1.000000000000000000, 0.9510565162951535312, 1.000000000000000000, 0.9510565162951535312, 1.000000000000000000, 0.9510565162951535312, 1.000000000000000000, 0.9510565162951535312, 1.000000000000000000, 0.9510565162951535312, 1.000000000000000000, 0.9510565162951535312, 1.000000000000000000, 0.9510565162951535312, 1.000000000000000000, 0.9510565162951535312, 1.000000000000000000, 0.9510565162951535312, 1.000000000000000000, 0.9510565162951535312, 1.000000000000000000, 0.9510565162951535312, 1.000000000000000000, 0.9510565162951535312, 1.000000000000000000, 0.9510565162951535312, 1.000000000000000000, 0.9510565162951535312, 1.000000000000000000, 0.9510565162951535312, 1.000000000000000000, 0.9510565162951535312, 1.000000000000000000, 0.9510565162951535312, 1.000000000000000000, 0.9510565162951535312, 1.000000000000000000, 0.9510565162951535312, 1.000000000000000000, 0.9510565162951535312, 1.000000000000000000, 0.9510565162951535312, 1.000000000000000000, 0.9510565162951535312, 1.000000000000000000, 0.9510565162951535312, 1.000000000000000000, 0.9510565162951535312, 1.000000000000000000, 0.9510565162951535312, 1.000000000000000000, 0.9510565162951535312, 1.000000000000000000, 0.9510565162951535312, 1.000000000000000000, 0.9510565162951535312, 1.000000000000000000, 0.9510565162951535312, 1.000000000000000000, 0.9510565162951535312, 1.000000000000000000, 0.9510565162951535312, 1.000000000000000000, 0.9510565162951535312, 1.000000000000000000, 0.9510565162951535312, 1.000000000000000000, 0.9510565162951535312, 1.000000000000000000, 0.9510565162951535312, 1.000000000000000000, 0.9510565162951535312, 1.000000000000000000, 0.9510565162951535312, 1.000000000000000000, 0.9510565162951535312, 1.000000000000000000, 0.9510565162951535312, 1.000000000000000000, 0.9510565162951535312, 1.000000000000000000, 0.9510565162951535312, 1.000000000000000000, 0.9510565162951535312, 1.000000000000000000, 0.9510565162951535312, 1.000000000000000000, 0.9510565162951535312, 1.000000000000000000, 0.9510565162951535312, 1.000000000000000000, 0.9510565162951535312, 1.000000000000000000, 0.9510565162951535312, 1.000000000000000000, 0.9510565162951535312, 1.000000000000000000, 0.9510565162951535312, 1.000000000000000000, 0.9510565162951535312, 1.000000000000000000, 0.9510565162951535312, 1.000000000000000000, 0.9510565162951535312, 1.000000000000000000, 0.9510565162951535312, 1.000000000000000000, 0.9510565162951535312, 1.000000000000000000, 0.9510565162951535312, 1.000000000000000000, 0.9510565162951535312, 1.000000000000000000, 0.9510565162951535312, 1.000000000000000000, 0.9510565162951535312, 1.000000000000000000, 0.9510565162951535312, 1.000000000000000000, 0.9510565162951535312, 1.000000000000000000, 0.9510565162951535312, 1.000000000000000000, 0.9510565162951535312, 1.000000000000000000, 0.9510565162951535312, 1.000000000000000000, 0.9510565162951535312, 1.000000000000000000, 0.9510565162951535312, 1.000000000000000000, 0.9510565162951535312, 1.000000000000000000, 0.9510565162951535312, 1.000000000000000000, 0.9510565162951535312, 1.000000000000000000, 0.9510565162951535312, 1.000000000000000000, 0.9510565162951535312, 1.000000000000000000, 0.9510565162951535312, 1.000000000000000000, 0.9510565162951535312, 1.000000000000000000, 0.9510565162951535312, 1.000000000000000000, 0.9510565162951535312, 1.000000000000000000, 0.9510565162951535312, 1.000000000000000000, 0.9510565162951535312, 1.000000000000000000, 0.9510565162951535312, 1.000000000000000000, 0.9510565162951535312, 1.000000000000000000, 0.9510565162951535312, 1.000000000000000000, 0.9510565162951535312, 1.000000000000000000, 0.9510565162951535312, 1.000000000000000000, 0.9510565162951535312, 1.000000000000000000, 0.9510565162951535312, 1.000000000000000000, 0.9510565162951535312, 1.000000000000000000, 0.9510565162951535312, 1.000000000000000000, 0.9510565162951535312, 1.000000000000000000, 0.9510565162951535312, 1.000000000000000000, 0.9510565162951535312, 1.000000000000000000, 0.9510565162951535312, 1.000000000000000000, 0.9510565162951535312, 1.000000000000000000, 0.9510565162951535312, 1.000000000000000000, 0.9510565162951535312, 1.000000000000000000, 0.9510565162951535312, 1.000000000000000000, 0.9510565162951535312, 1.000000000000000000, 0.9510565162951535312, 1.000000000000000000, 0.9510565162951535312, 1.000000000000000000, 0.9510565162951535312, 1.000000000000000000, 0.9510565162951535312, 1.000000000000000000, 0.9510565162951535312, 1.000000000000000000, 0.9510565162951535312, 1.000000000000000000, 0.9510565162951535312, 1.000000000000000000, 0.9510565162951535312, 1.000000000000000000, 0.9510565162951535312, 1.000000000000000000, 0.9510565162951535312, 1.000000000000000000, 0.9510565162951535312, 1.000000000000000000, 0.9510565162951535312, 1.000000000000000000, 0.9510565162951535312, 1.000000000000000000, 0.9510565162951535312, 1.000000000000000000, 0.9510565162951535312, 1.000000000000000000, 0.9510565162951535312, 1.000000000000000000, 0.9510565162951535312, 1.000000000000000000, 0.9510565162951535312, 1.000000000000000000, 0.9510565162951535312, 1.000000000000000000, 0.9510565162951535312, 1.000000000000000000, 0.9510565162951535312, 1.000000000000000000, 0.9510565162951535312, 1.000000000000000000, 0.9510565162951535312, 1.000000000000000000, 0.9510565162951535312, 1.000000000000000000, 0.9510565162951535312, 1.000000000000000000, 0.9510565162951535312, 1.000000000000000000, 0.9510565162951535312, 1.000000000000000000, 0.9510565162951535312, 1.000000000000000000, 0.9510565162951535312, 1.000000000000000000, 0.9510565162951535312, 1.000000000000000000, 0.9510565162951535312, 1.000000000000000000, 0.9510565162951535312, 1.000000000000000000, 0.9510565162951535312, 1.000000000000000000, 0.9510565162951535312, 1.000000000000000000, 0.9510565162951535312, 1.000000000000000000, 0.9510565162951535312, 1.000000000000000000) ) ) 
 REPRESENTATION_ITEM ( '' )  SURFACE ( )  );
#70291 = CARTESIAN_POINT ( 'NONE',  ( 196.4982648257524147, 290.3020170531091821, 16.69353242256149628 ) ) ;
#70292 = DIRECTION ( 'NONE',  ( 0.000000000000000000, 0.000000000000000000, 1.000000000000000000 ) ) ;
#70293 = EDGE_CURVE ( 'NONE', #44322, #21282, #23836, .T. ) ;
#70294 = CARTESIAN_POINT ( 'NONE',  ( 72.95830788359974406, 56.77128196665827176, -15.96545419981962333 ) ) ;
#70295 = CARTESIAN_POINT ( 'NONE',  ( 42.47567221558909267, 186.1423013555410080, -4.594050593750043987 ) ) ;
#70296 = CARTESIAN_POINT ( 'NONE',  ( 79.95842099707557793, 204.7202760586659167, -5.415160957724236172E-17 ) ) ;
#70297 = CARTESIAN_POINT ( 'NONE',  ( 177.9714937548455680, 255.7189482022137383, 8.882064279750110813 ) ) ;
#70299 = CARTESIAN_POINT ( 'NONE',  ( 88.49101168009576668, 43.86507591752568658, 0.01250564173601438969 ) ) ;
#70298 = CIRCLE ( 'NONE', #21790, 7.298499999999999766 ) ;
#70300 = CARTESIAN_POINT ( 'NONE',  ( 5.272250483539713706, 24.81751292744053217, -6.180339887498951690 ) ) ;
#70301 = CARTESIAN_POINT ( 'NONE',  ( 140.4712518949831974, 264.1589784336661637, -6.496448406907675876E-16 ) ) ;
#70303 = CARTESIAN_POINT ( 'NONE',  ( -22.42236680055709641, 157.8615022471902591, 0.000000000000000000 ) ) ;
#70302 = CARTESIAN_POINT ( 'NONE',  ( 4.781100836665275189, 70.53751509772452266, -10.00000000000000000 ) ) ;
#70304 = CARTESIAN_POINT ( 'NONE',  ( 22.44857442947627035, 173.7677522451417929, -5.000000000000041744 ) ) ;
#70305 = CARTESIAN_POINT ( 'NONE',  ( 32.94607225727562394, 21.94754757982091320, 5.678558825948272215 ) ) ;
#70306 = CARTESIAN_POINT ( 'NONE',  ( 150.9584389135710865, 269.1793093008492406, -15.82751450793727699 ) ) ;
#70307 = CARTESIAN_POINT ( 'NONE',  ( 81.09489198153239897, 47.45865598376690997, -12.84490686960000794 ) ) ;
#70308 = CARTESIAN_POINT ( 'NONE',  ( 13.11890841201833169, 13.28920272979925166, -7.433330006724141015 ) ) ;
#70309 = CARTESIAN_POINT ( 'NONE',  ( 58.44249495421716745, 213.7369531367911293, -4.594050593750048428 ) ) ;
#70310 = CARTESIAN_POINT ( 'NONE',  ( 76.83059214691050443, 63.69233987691562504, 15.32693845983791547 ) ) ;
#70311 = CARTESIAN_POINT ( 'NONE',  ( 155.3250150347760723, 261.6161776038049425, -18.57420904020362684 ) ) ;
#70312 = CARTESIAN_POINT ( 'NONE',  ( 198.1230806404959139, 287.4877535090322453, 17.00698319228197164 ) ) ;
#70313 = CARTESIAN_POINT ( 'NONE',  ( 69.49445684968409864, 63.05235503358468208, -13.61616618888627883 ) ) ;
#70314 = CARTESIAN_POINT ( 'NONE',  ( 153.3535503493361887, 265.0308546043145270, 16.96417449729259630 ) ) ;
#70315 = CARTESIAN_POINT ( 'NONE',  ( 79.03501320358060411, 55.48393193879000762, -16.09017401043118056 ) ) ;
#70316 = CARTESIAN_POINT ( 'NONE',  ( 87.62838477539726512, 44.93552847577709031, -6.577990587745525808 ) ) ;
#70317 = CARTESIAN_POINT ( 'NONE',  ( 107.0484310652164481, 242.6115022471903160, -5.000000000000047962 ) ) ;
#70318 = ADVANCED_FACE ( 'NONE', ( #1568 ), #31933, .F. ) ;
#70319 = CARTESIAN_POINT ( 'NONE',  ( 207.2383675728608239, 271.6996134166075763, 7.873592648726489784 ) ) ;
#70320 = EDGE_LOOP ( 'NONE', ( #34367, #43677, #63129, #15179 ) ) ;
#70321 = CARTESIAN_POINT ( 'NONE',  ( 77.41302249286091808, 49.21411113510112045, 15.30941459159846119 ) ) ;
#70322 = CARTESIAN_POINT ( 'NONE',  ( 184.9087269013485013, 271.1903322944930892, 16.55683110539250436 ) ) ;
#70323 = VERTEX_POINT ( 'NONE', #63844 ) ;
#70324 = CARTESIAN_POINT ( 'NONE',  ( 206.1615484827472358, 273.5647187912443314, -9.556459874778100883 ) ) ;
#70325 = CARTESIAN_POINT ( 'NONE',  ( 190.2191487900553852, 279.1426948662232803, -16.69313596982519243 ) ) ;
#70326 = CARTESIAN_POINT ( 'NONE',  ( -22.42236680055709641, 157.8615022471902591, 0.000000000000000000 ) ) ;
#70327 = ORIENTED_EDGE ( 'NONE', *, *, #90949, .F. ) ;
#70329 = ADVANCED_FACE ( 'NONE', ( #25342 ), #25657, .T. ) ;
#70328 = CARTESIAN_POINT ( 'NONE',  ( 173.6323106214142626, 251.0528461505140285, 0.5214956749697322591 ) ) ;
#70330 = ORIENTED_EDGE ( 'NONE', *, *, #97235, .F. ) ;
#70332 = EDGE_CURVE ( 'NONE', #25048, #17411, #71963, .T. ) ;
#70331 = CARTESIAN_POINT ( 'NONE',  ( -19.65009819364242105, 93.20683205598336940, 59.99999999999999289 ) ) ;
#70333 = CARTESIAN_POINT ( 'NONE',  ( 147.8819534105757043, 274.5079385007862811, -9.338341377131436971 ) ) ;
#70334 = B_SPLINE_CURVE_WITH_KNOTS ( 'NONE', 3,
 ( #67508, #98439, #81270, #27541 ),
 .UNSPECIFIED., .F., .F.,
 ( 4, 4 ),
 ( 0.000000000000000000, 0.002378078545638787674 ),
 .UNSPECIFIED. ) ;
#70335 = CARTESIAN_POINT ( 'NONE',  ( 148.5942620090405342, 274.9790495171396856, 7.678286107965337948 ) ) ;
#70336 = EDGE_LOOP ( 'NONE', ( #71110, #61916, #90252, #51131 ) ) ;
#70337 = CARTESIAN_POINT ( 'NONE',  ( 33.71705561599726053, 20.26216523072496045, -2.296566073217252530E-15 ) ) ;
#70338 = DIRECTION ( 'NONE',  ( -0.5951734788405910193, 0.8035972437015875824, 0.000000000000000000 ) ) ;
#70339 = CARTESIAN_POINT ( 'NONE',  ( 74.96814850772595662, 66.86370092720997604, -13.20453066047569024 ) ) ;
#70340 = ADVANCED_FACE ( 'NONE', ( #86704 ), #62837, .T. ) ;
#70341 = EDGE_CURVE ( 'NONE', #20756, #59093, #10159, .T. ) ;
#70342 = ORIENTED_EDGE ( 'NONE', *, *, #40586, .F. ) ;
#70343 = LINE ( 'NONE', #61736, #88710 ) ;
#70344 = CARTESIAN_POINT ( 'NONE',  ( 170.8805640699686990, 257.7213711969266114, 14.63406020945912367 ) ) ;
#70345 = ORIENTED_EDGE ( 'NONE', *, *, #23704, .F. ) ;
#70346 = CARTESIAN_POINT ( 'NONE',  ( 171.5339044271115370, 285.5759136860501144, 11.31677738237828557 ) ) ;
#70348 = CARTESIAN_POINT ( 'NONE',  ( 67.93422661307175758, 66.05804427658543432, -10.47009145265134933 ) ) ;
#70347 = CARTESIAN_POINT ( 'NONE',  ( 67.97326575654918202, 65.43911154409434516, 10.39403152487275506 ) ) ;
#70349 = CARTESIAN_POINT ( 'NONE',  ( 208.0421103033489771, 270.3074901711881353, -2.473242163239977476 ) ) ;
#70350 = CARTESIAN_POINT ( 'NONE',  ( 193.7275870247597425, 295.1009717758319084, 14.48058678254265885 ) ) ;
#70351 = CARTESIAN_POINT ( 'NONE',  ( 158.3585752585947262, 263.3710999200782226, 17.79390465796247156 ) ) ;
#70352 = CARTESIAN_POINT ( 'NONE',  ( 204.8385597977314490, 275.8562024115307167, -12.64672659107585240 ) ) ;
#70353 = CARTESIAN_POINT ( 'NONE',  ( 145.2890388471816721, 248.5643266524160424, -9.188101187500093303 ) ) ;
#70354 = CARTESIAN_POINT ( 'NONE',  ( 206.4643841499645305, 270.6241384910937882, 2.661278798003872570 ) ) ;
#70355 = CARTESIAN_POINT ( 'NONE',  ( 178.7344501488548758, 257.7588143725840837, 9.974505692861084682 ) ) ;
#70356 = CARTESIAN_POINT ( 'NONE',  ( 96.27750042569734035, 217.2048013555409796, 4.594050593750051981 ) ) ;
#70357 = ORIENTED_EDGE ( 'NONE', *, *, #51075, .T. ) ;
#70359 = B_SPLINE_CURVE_WITH_KNOTS ( 'NONE', 3,
 ( #82713, #75076, #5657, #52735, #29457, #99371, #6660, #13281, #45147, #52250, #7140, #60331, #83698, #14258, #83192, #76559, #7647, #30448, #61338, #38027, #68938, #67452, #92296, #37050, #15230, #59847, #76086, #53730, #98380, #22847, #13754, #90311, #20883, #53248, #67957, #68443, #37537, #91288, #44634, #91786, #90810, #21364, #46126, #75567, #77040, #29950, #69445, #59331, #45631, #6156, #21854, #51772 ),
 .UNSPECIFIED., .F., .F.,
 ( 4, 2, 2, 2, 2, 2, 2, 2, 2, 2, 2, 2, 2, 2, 2, 2, 2, 2, 2, 2, 2, 2, 2, 2, 2, 4 ),
 ( 0.0001254446608424856873, 0.0006176921519154450479, 0.001109939642988404382, 0.001356063388524914081, 0.001602187134061423997, 0.001725249006829678846, 0.001848310879597933913, 0.001971372752366188329, 0.002094434625134443395, 0.002340558370670906690, 0.002586682116207370419, 0.003078929607280350787, 0.004063424589426311954, 0.005047919571572273556, 0.005540167062645214892, 0.005786290808181685993, 0.006032414553718157095, 0.006093945490102312817, 0.006155476426486468540, 0.006278538299254766974, 0.006524662044791365578, 0.006770785790327965049, 0.007016909535864564521, 0.007263033281401164859, 0.007509157026937763463, 0.008001404518010932915 ),
 .UNSPECIFIED. ) ;
#70358 = CARTESIAN_POINT ( 'NONE',  ( 191.4922467593309250, 298.9726946877590876, 7.604184559945784017 ) ) ;
#70360 = CARTESIAN_POINT ( 'NONE',  ( 193.0512205562391159, 275.6825563886401369, -16.88465587640301280 ) ) ;
#70361 = DIRECTION ( 'NONE',  ( 0.5000000000000009992, -0.8660254037844380415, 0.000000000000000000 ) ) ;
#70362 = ORIENTED_EDGE ( 'NONE', *, *, #12211, .F. ) ;
#70363 = CARTESIAN_POINT ( 'NONE',  ( 157.0384757953324595, 258.6483765097458445, -16.84863706481609569 ) ) ;
#70364 = ORIENTED_EDGE ( 'NONE', *, *, #17040, .T. ) ;
#70365 = B_SPLINE_CURVE_WITH_KNOTS ( 'NONE', 3,
 ( #36247, #67152, #98073, #99070, #28650, #6358, #52442, #83389, #37244, #29651, #89047, #19594, #81407, #42836, #4363, #35259 ),
 .UNSPECIFIED., .F., .F.,
 ( 4, 2, 2, 2, 2, 2, 2, 4 ),
 ( 3.688072698881470622E-17, 0.0004627479835026719417, 0.0006941219752539907551, 0.0009254959670053095142, 0.001156869958756628165, 0.001388243950507947033, 0.001619617942259265683, 0.001850991934010584551 ),
 .UNSPECIFIED. ) ;
#70366 = CARTESIAN_POINT ( 'NONE',  ( 80.03788392018469722, 44.31502134952003757, -11.48980017305513179 ) ) ;
#70367 = DIRECTION ( 'NONE',  ( -0.000000000000000000, -0.000000000000000000, -1.000000000000000000 ) ) ;
#70368 = CARTESIAN_POINT ( 'NONE',  ( 191.2211340522693774, 299.4422756709672626, -8.405362570633277741 ) ) ;
#70369 = CARTESIAN_POINT ( 'NONE',  ( 81.17232691891707930, 55.55242957854174080, 16.36487835605631602 ) ) ;
#70370 = CARTESIAN_POINT ( 'NONE',  ( 82.74137886417670984, 47.78502673368306120, -12.47258107324418930 ) ) ;
#70371 = FACE_OUTER_BOUND ( 'NONE', #19543, .T. ) ;
#70372 = CARTESIAN_POINT ( 'NONE',  ( 88.80803131805656392, 212.8923013555409796, 4.594050593750050204 ) ) ;
#70373 = ORIENTED_EDGE ( 'NONE', *, *, #13487, .T. ) ;
#70374 = VECTOR ( 'NONE', #43425, 1000.000000000000114 ) ;
#70375 = EDGE_LOOP ( 'NONE', ( #69741, #11800, #31038, #84854, #57730 ) ) ;
#70376 = DIRECTION ( 'NONE',  ( 0.7059494278973771353, -0.7082622432767159415, 0.000000000000000000 ) ) ;
#70377 = B_SPLINE_SURFACE_WITH_KNOTS ( 'NONE', 3, 1, ( 
 ( #53613, #84570 ),
 ( #15108, #98250 ),
 ( #13154, #68816 ),
 ( #83070, #46001 ),
 ( #74951, #21730 ),
 ( #92661, #83572 ),
 ( #14133, #52614 ),
 ( #67327, #98757 ),
 ( #76919, #7518 ),
 ( #45019, #28840 ),
 ( #82589, #7021 ),
 ( #13641, #38411 ),
 ( #99244, #37413 ),
 ( #69326, #29340 ),
 ( #91662, #29829 ),
 ( #22225, #75962 ),
 ( #53126, #100247 ),
 ( #59720, #68319 ),
 ( #84082, #30829 ),
 ( #21243, #44514 ),
 ( #14633, #45514 ),
 ( #75445, #36923 ),
 ( #67837, #37906 ),
 ( #64226, #40902 ),
 ( #932, #10039 ),
 ( #71344, #25222 ),
 ( #1444, #16622 ),
 ( #430, #55601 ),
 ( #31808, #46507 ),
 ( #78446, #38914 ),
 ( #23214, #9027 ),
 ( #15609, #77445 ),
 ( #32821, #77942 ),
 ( #62708, #32324 ) ),
 .UNSPECIFIED., .T., .F., .F.,
 ( 4, 2, 2, 2, 2, 2, 2, 2, 2, 2, 2, 2, 2, 2, 2, 2, 4 ),
 ( 2, 2 ),
 ( 0.000000000000000000, 0.06250000000000000000, 0.1250000000000000000, 0.1875000000000000000, 0.2500000000000000000, 0.3125000000000000000, 0.3750000000000000000, 0.4375000000000000000, 0.5000000000000000000, 0.5625000000000000000, 0.6250000000000000000, 0.6875000000000000000, 0.7500000000000000000, 0.8125000000000000000, 0.8750000000000000000, 0.9375000000000000000, 1.000000000000000000 ),
 ( 0.000000000000000000, 1.000000000000000000 ),
 .UNSPECIFIED. ) ;
#70378 = CARTESIAN_POINT ( 'NONE',  ( 208.3682389855799499, 269.7426187237583690, -1.431169231381201890 ) ) ;
#70379 = ORIENTED_EDGE ( 'NONE', *, *, #26204, .T. ) ;
#70380 = EDGE_CURVE ( 'NONE', #26607, #13801, #49944, .T. ) ;
#70381 = CARTESIAN_POINT ( 'NONE',  ( 15.66455532895297331, 30.81751292744056059, -6.180339887498951690 ) ) ;
#70382 = VECTOR ( 'NONE', #78615, 1000.000000000000000 ) ;
#70383 = CARTESIAN_POINT ( 'NONE',  ( 184.1072502077840909, 275.2075811318409819, 16.36983495193582172 ) ) ;
#70384 = CARTESIAN_POINT ( 'NONE',  ( 162.3887597439333774, 285.1017702274234580, 0.5428779426774286154 ) ) ;
#70385 = CARTESIAN_POINT ( 'NONE',  ( 98.91686120480925126, 239.4637435831424739, 2.679491924311251605 ) ) ;
#70386 = CARTESIAN_POINT ( 'NONE',  ( 88.10887562929657690, 44.41668309952778060, 4.665177569529613599 ) ) ;
#70387 = ORIENTED_EDGE ( 'NONE', *, *, #93410, .F. ) ;
#70388 = CARTESIAN_POINT ( 'NONE',  ( 81.04961468568201610, 43.68546784643918812, -9.492462169003031747 ) ) ;
#70389 = CARTESIAN_POINT ( 'NONE',  ( 185.9605642706161746, 259.1549715882831606, 6.130847983954422986 ) ) ;
#70390 = CARTESIAN_POINT ( 'NONE',  ( 40.48539884740146277, 126.3902902409112556, -10.00000000000000000 ) ) ;
#70391 = CARTESIAN_POINT ( 'NONE',  ( 201.0356089830534643, 282.4431064412383989, -18.18835788025466371 ) ) ;
#70392 = CARTESIAN_POINT ( 'NONE',  ( 72.55393231385352237, 70.87694079910581024, 7.622851120052408724 ) ) ;
#70393 = CARTESIAN_POINT ( 'NONE',  ( 149.3118911495987788, 247.0312136851381126, 5.028230608967417581 ) ) ;
#70394 = VERTEX_POINT ( 'NONE', #79596 ) ;
#70395 = PLANE ( 'NONE',  #62357 ) ;
#70396 = CARTESIAN_POINT ( 'NONE',  ( 161.4396252346964218, 251.0253620690641299, 14.51972485405798885 ) ) ;
#70397 = FACE_OUTER_BOUND ( 'NONE', #31830, .T. ) ;
#70398 = CARTESIAN_POINT ( 'NONE',  ( 187.5257214801813461, 265.9040347152727009, -11.83413594510077260 ) ) ;
#70399 = CARTESIAN_POINT ( 'NONE',  ( -22.42236680055709641, 157.8615022471902591, 0.000000000000000000 ) ) ;
#70400 = CARTESIAN_POINT ( 'NONE',  ( 153.5335373734693576, 270.3435883613224178, 14.01947500330756391 ) ) ;
#70401 = ORIENTED_EDGE ( 'NONE', *, *, #85332, .T. ) ;
#70402 = ADVANCED_FACE ( 'NONE', ( #86207 ), #15734, .T. ) ;
#70403 = DIRECTION ( 'NONE',  ( 0.4999999999999998890, -0.8660254037844385966, 0.000000000000000000 ) ) ;
#70404 = B_SPLINE_CURVE_WITH_KNOTS ( 'NONE', 3,
 ( #40564, #48695, #23868, #40060 ),
 .UNSPECIFIED., .F., .F.,
 ( 4, 4 ),
 ( 0.008181640604905312045, 0.01326458609140142818 ),
 .UNSPECIFIED. ) ;
#70405 = CARTESIAN_POINT ( 'NONE',  ( 202.4943568615953779, 279.9164810001701085, 17.09064351659286984 ) ) ;
#70406 = AXIS2_PLACEMENT_3D ( 'NONE', #29110, #90453, #59976 ) ;
#70407 = DIRECTION ( 'NONE',  ( 1.000000000000000000, 0.000000000000000000, 0.000000000000000000 ) ) ;
#70409 = CARTESIAN_POINT ( 'NONE',  ( 73.60933432321982650, 55.64367109616565443, 16.10230547196764661 ) ) ;
#70408 = CARTESIAN_POINT ( 'NONE',  ( 177.4749804298298272, 264.4991266834069279, -15.68007347713953514 ) ) ;
#70410 = CARTESIAN_POINT ( 'NONE',  ( 199.1402566354874750, 281.8950033040109133, -16.59982190247651346 ) ) ;
#70411 = ADVANCED_FACE ( 'NONE', ( #48145 ), #77565, .F. ) ;
#70412 = CARTESIAN_POINT ( 'NONE',  ( 26.23682664367882111, 38.08080186712594184, -3.090169943749475845 ) ) ;
#70413 = CARTESIAN_POINT ( 'NONE',  ( 168.4187099521293760, 273.5093150913818363, 16.15648551869223937 ) ) ;
#70414 = CARTESIAN_POINT ( 'NONE',  ( 163.3291633122615849, 283.7466658353214939, -3.311912926934972301 ) ) ;
#70415 = DIRECTION ( 'NONE',  ( -0.8660254037844377084, -0.5000000000000014433, -0.000000000000000000 ) ) ;
#70416 = CARTESIAN_POINT ( 'NONE',  ( 191.3487518683689359, 261.0470579585651194, 3.102467918029140126 ) ) ;
#70417 = ADVANCED_FACE ( 'NONE', ( #69933 ), #6975, .T. ) ;
#70418 = DIRECTION ( 'NONE',  ( -0.9404163354663408469, -0.3400251696390412803, 0.000000000000000000 ) ) ;
#70419 = CARTESIAN_POINT ( 'NONE',  ( 2.016134656476094023, 159.7202760586659736, -5.415160957724236172E-17 ) ) ;
#70420 = CARTESIAN_POINT ( 'NONE',  ( 82.93017357788667709, 175.3855496052738374, 36.50000000000000000 ) ) ;
#70421 = EDGE_LOOP ( 'NONE', ( #52782, #38194, #58159, #86607, #19056 ) ) ;
#70422 = CARTESIAN_POINT ( 'NONE',  ( 174.8562727840514412, 255.3278782549236894, 8.725767214627929036 ) ) ;
#70423 = CARTESIAN_POINT ( 'NONE',  ( 68.68909986782581711, 64.16576715805911135, -12.55144644517788777 ) ) ;
#70424 = PLANE ( 'NONE',  #82061 ) ;
#70425 = DIRECTION ( 'NONE',  ( 1.000000000000000000, 0.000000000000000000, 0.000000000000000000 ) ) ;
#70426 = CARTESIAN_POINT ( 'NONE',  ( 16.52171307410043255, 180.3458772461660544, 9.188101187500095079 ) ) ;
#70427 = LINE ( 'NONE', #62307, #97678 ) ;
#70428 = CARTESIAN_POINT ( 'NONE',  ( 34.54807858326547176, 25.11029122506296929, -8.090169943749478065 ) ) ;
#70429 = CARTESIAN_POINT ( 'NONE',  ( 77.17250858205457575, 53.66386925528713192, 16.42442879155417756 ) ) ;
#70430 = CARTESIAN_POINT ( 'NONE',  ( 100.4810717531844659, 235.4865022471902876, -10.00000000000009592 ) ) ;
#70431 = CARTESIAN_POINT ( 'NONE',  ( 81.46466179813324970, 56.08326244678959682, 16.06754189170436575 ) ) ;
#70432 = CARTESIAN_POINT ( 'NONE',  ( 186.7314779716672888, 295.9876638862722871, -8.607072244006850781 ) ) ;
#70433 = CARTESIAN_POINT ( 'NONE',  ( 189.8800752008499160, 261.4572743640761701, -0.7539990698043521622 ) ) ;
#70434 = VECTOR ( 'NONE', #9540, 1000.000000000000114 ) ;
#70435 = CARTESIAN_POINT ( 'NONE',  ( 67.57210640937580592, 216.4865022471902876, 10.00000000000009237 ) ) ;
#70436 = CARTESIAN_POINT ( 'NONE',  ( 72.84204051986223760, 66.34192636652406350, -12.17031965754431866 ) ) ;
#70437 = EDGE_CURVE ( 'NONE', #63662, #21425, #89696, .T. ) ;
#70438 = CARTESIAN_POINT ( 'NONE',  ( 167.6502826215564994, 287.3877002845107995, 4.891367078714356609 ) ) ;
#70439 = CARTESIAN_POINT ( 'NONE',  ( 37.57712925149210292, 186.3768266524160140, 9.188101187500098632 ) ) ;
#70440 = CARTESIAN_POINT ( 'NONE',  ( 48.77433535142598231, 99.76555324011610537, 10.00000000000000000 ) ) ;
#70441 = CARTESIAN_POINT ( 'NONE',  ( 35.14347105191519205, 25.45404122711135741, -8.090169943749478065 ) ) ;
#70442 = CARTESIAN_POINT ( 'NONE',  ( 203.0352482185525389, 270.0697959434764925, -6.424953051763736767 ) ) ;
#70443 = CARTESIAN_POINT ( 'NONE',  ( 44.85937643310611378, 116.8208962945185050, -10.00000000000000000 ) ) ;
#70444 =( GEOMETRIC_REPRESENTATION_CONTEXT ( 3 ) GLOBAL_UNCERTAINTY_ASSIGNED_CONTEXT ( ( #56450 ) ) GLOBAL_UNIT_ASSIGNED_CONTEXT ( ( #72094, #78695, #56863 ) ) REPRESENTATION_CONTEXT ( 'NONE', 'WORKASPACE' ) );
#70445 = CARTESIAN_POINT ( 'NONE',  ( 67.08714283343131513, 66.81104840727229544, -8.985171576933360882 ) ) ;
#70446 = DIRECTION ( 'NONE',  ( 0.8261602328994307465, -0.5634352399127678934, 0.000000000000000000 ) ) ;
#70447 = CARTESIAN_POINT ( 'NONE',  ( 160.2764658979060926, 278.7662822791168651, -9.787372777049167638 ) ) ;
#70448 = CARTESIAN_POINT ( 'NONE',  ( 205.7570824856458103, 269.1293880245460173, -1.352896656403272946 ) ) ;
#70449 = CARTESIAN_POINT ( 'NONE',  ( 24.91850453858129910, 20.10170272979927475, -7.433330006724141015 ) ) ;
#70450 = CARTESIAN_POINT ( 'NONE',  ( 202.3425522658138505, 280.1794142728863903, 15.86053073629060961 ) ) ;
#70451 = CARTESIAN_POINT ( 'NONE',  ( 196.6800254274587019, 289.9871984561398222, -17.90749311895638129 ) ) ;
#70452 = CARTESIAN_POINT ( 'NONE',  ( 175.1308103651610963, 256.9497360334458449, 11.89887680739436071 ) ) ;
#70453 = ORIENTED_EDGE ( 'NONE', *, *, #57987, .T. ) ;
#70454 = CARTESIAN_POINT ( 'NONE',  ( 5.233272902960924178, 23.99752408145589655, 5.678558825948276656 ) ) ;
#70455 = CYLINDRICAL_SURFACE ( 'NONE', #10646, 10.00000000000010658 ) ;
#70456 = CARTESIAN_POINT ( 'NONE',  ( 79.35086191672368727, 57.56414197016153622, -16.24676580536099735 ) ) ;
#70457 = CARTESIAN_POINT ( 'NONE',  ( 88.08794642153516463, 44.30065689091529890, 2.777777743264004506 ) ) ;
#70458 = DIRECTION ( 'NONE',  ( -0.8660254037844387076, -0.4999999999999998890, -0.000000000000000000 ) ) ;
#70459 = CARTESIAN_POINT ( 'NONE',  ( 69.45630962237427752, 70.64887205696791739, -1.534870757239616301 ) ) ;
#70460 = CARTESIAN_POINT ( 'NONE',  ( 190.9061255863007318, 299.9878863388391892, 7.497146773253707153 ) ) ;
#70461 = CARTESIAN_POINT ( 'NONE',  ( 155.5066938333533528, 261.3015006940112244, -18.40036130547566273 ) ) ;
#70462 = EDGE_LOOP ( 'NONE', ( #56664, #51560, #34114, #85610 ) ) ;
#70463 = VERTEX_POINT ( 'NONE', #26357 ) ;
#70465 = CARTESIAN_POINT ( 'NONE',  ( 82.42451625089289280, 42.32467009663571389, -6.203346966617362845 ) ) ;
#70464 = DIRECTION ( 'NONE',  ( -0.8660254037844387076, -0.4999999999999998890, -0.000000000000000000 ) ) ;
#70466 = ORIENTED_EDGE ( 'NONE', *, *, #9616, .F. ) ;
#70467 = CARTESIAN_POINT ( 'NONE',  ( 201.3053499423511425, 281.9759013948520874, -16.75960365258566398 ) ) ;
#70468 = CARTESIAN_POINT ( 'NONE',  ( 71.78553924664423391, 72.10835861452468976, -3.632824164035485470 ) ) ;
#70469 = CARTESIAN_POINT ( 'NONE',  ( 203.5726949774746117, 269.0034548673361883, -6.096665150295551783 ) ) ;
#70470 = PLANE ( 'NONE',  #79141 ) ;
#70471 = CARTESIAN_POINT ( 'NONE',  ( 189.8147415777049218, 301.8782188922952514, -0.5019643756309712934 ) ) ;
#70472 = CARTESIAN_POINT ( 'NONE',  ( 196.2878005184348353, 290.6665519265632724, -16.69183432842427806 ) ) ;
#70473 = ADVANCED_FACE ( 'NONE', ( #56743 ), #12154, .F. ) ;
#70474 = LINE ( 'NONE', #9707, #93287 ) ;
#70475 = VECTOR ( 'NONE', #58543, 1000.000000000000114 ) ;
#70476 = ORIENTED_EDGE ( 'NONE', *, *, #96210, .F. ) ;
#70477 = CARTESIAN_POINT ( 'NONE',  ( 178.8595466249924755, 265.0989930076032124, -16.03772641351113748 ) ) ;
#70478 = CARTESIAN_POINT ( 'NONE',  ( 161.6952081746299825, 267.0400630579588892, 16.50188533208787334 ) ) ;
#70479 = ORIENTED_EDGE ( 'NONE', *, *, #99162, .F. ) ;
#70480 = CARTESIAN_POINT ( 'NONE',  ( 28.99364183777449000, 25.24335787977764767, -9.188101187500008038 ) ) ;
#70481 = DIRECTION ( 'NONE',  ( 0.1039558454088763267, -0.1800568059919503139, 0.9781476007338069101 ) ) ;
#70482 = CARTESIAN_POINT ( 'NONE',  ( 78.29365456329206552, 47.43229965770008505, -13.76414149961745714 ) ) ;
#70483 = CARTESIAN_POINT ( 'NONE',  ( 58.14488549560751807, 210.5024278399160949, 9.188101187500095079 ) ) ;
#70484 = ORIENTED_EDGE ( 'NONE', *, *, #51003, .T. ) ;
#70485 = CARTESIAN_POINT ( 'NONE',  ( -14.65312891409034535, 84.40478749174073414, 0.000000000000000000 ) ) ;
#70486 = CARTESIAN_POINT ( 'NONE',  ( -19.65312891409030271, 93.06504152958497400, -10.00000000000000000 ) ) ;
#70487 = VECTOR ( 'NONE', #60390, 1000.000000000000000 ) ;
#70488 = CARTESIAN_POINT ( 'NONE',  ( 172.5948319566698501, 271.8727042802207734, 17.20912629143206374 ) ) ;
#70489 = ORIENTED_EDGE ( 'NONE', *, *, #62571, .F. ) ;
#70490 = CARTESIAN_POINT ( 'NONE',  ( 87.12872031379318116, 46.22333408697501511, 8.447664276980741960 ) ) ;
#70491 = CARTESIAN_POINT ( 'NONE',  ( 165.0735250206753619, 246.7312630101393722, 5.989302113854410692 ) ) ;
#70492 = CARTESIAN_POINT ( 'NONE',  ( 147.6121581866023007, 274.9752375363476631, 8.700660424766859080 ) ) ;
#70493 = ORIENTED_EDGE ( 'NONE', *, *, #2303, .T. ) ;
#70494 = CARTESIAN_POINT ( 'NONE',  ( 175.3681337606042803, 261.2921292801445929, -14.32318010708709544 ) ) ;
#70495 = DIRECTION ( 'NONE',  ( -0.8660254037844378194, -0.5000000000000013323, -0.000000000000000000 ) ) ;
#70496 = DIRECTION ( 'NONE',  ( 0.6600842437418872333, -0.7511915808658273797, 0.000000000000000000 ) ) ;
#70497 = CARTESIAN_POINT ( 'NONE',  ( 146.8868584395697781, 276.2314935489248455, -3.891417269505058396 ) ) ;
#70498 = CARTESIAN_POINT ( 'NONE',  ( 31.12960416526798824, 44.88710030135629836, -10.00000000000000000 ) ) ;
#70499 = CARTESIAN_POINT ( 'NONE',  ( -48.92208041226317050, 108.8082784536894110, -10.00000000000000000 ) ) ;
#70500 = CARTESIAN_POINT ( 'NONE',  ( 164.2801755739368446, 246.1053845600426087, 2.518777461081745717 ) ) ;
#70501 = CARTESIAN_POINT ( 'NONE',  ( 76.20608723644332372, 65.18883345732480450, 14.14645056589919214 ) ) ;
#70502 = CARTESIAN_POINT ( 'NONE',  ( 70.44493300807654634, 65.46586672381103256, -11.71043221882291263 ) ) ;
#70503 = CARTESIAN_POINT ( 'NONE',  ( 38.67262647093125594, 99.46401760883253473, 59.99999999999999289 ) ) ;
#70504 = CARTESIAN_POINT ( 'NONE',  ( 113.7334117446687145, 224.2202760586659736, -5.415160957724236172E-17 ) ) ;
#70505 = VERTEX_POINT ( 'NONE', #18759 ) ;
#70506 = AXIS2_PLACEMENT_3D ( 'NONE', #95123, #47465, #23653 ) ;
#70507 = CARTESIAN_POINT ( 'NONE',  ( 190.1981067718782015, 301.2142108981337287, -4.661316250821958995 ) ) ;
#70508 = CARTESIAN_POINT ( 'NONE',  ( 77.93017357788674815, 184.0458036431181768, 30.52142883766498116 ) ) ;
#70509 = CARTESIAN_POINT ( 'NONE',  ( 87.67135465677671391, 44.96834575157770075, -6.594061650049633627 ) ) ;
#70510 = CARTESIAN_POINT ( 'NONE',  ( 154.9048824156581361, 262.3438686460345366, -17.40627786727128168 ) ) ;
#70511 = CIRCLE ( 'NONE', #26845, 70.00000000000001421 ) ;
#70512 = CARTESIAN_POINT ( 'NONE',  ( 164.2413944571582078, 246.1725554246774834, 7.304616466633322425 ) ) ;
#70513 = CARTESIAN_POINT ( 'NONE',  ( 83.70911819089758410, 52.26791303372475994, -15.08805761434582848 ) ) ;
#70514 = CARTESIAN_POINT ( 'NONE',  ( 69.38297557973733376, 65.04212082436336573, -11.54860170590457180 ) ) ;
#70515 = EDGE_LOOP ( 'NONE', ( #4935, #22301, #72789, #31702, #12811, #88354, #34625, #99502, #75257, #71423, #30462, #83907, #59654, #34142, #53753, #14320, #89031, #54922, #3106, #828, #86666 ) ) ;
#70516 = LINE ( 'NONE', #76628, #96418 ) ;
#70517 = CARTESIAN_POINT ( 'NONE',  ( 185.9527541470076812, 261.9448596265605715, 9.964853131083170723 ) ) ;
#70518 = CARTESIAN_POINT ( 'NONE',  ( 206.1020338308353530, 272.8276230067459096, 9.011824622212118996 ) ) ;
#70519 = CARTESIAN_POINT ( 'NONE',  ( 130.4855038751826726, 236.9548013555409796, -4.594050593750042211 ) ) ;
#70520 = CARTESIAN_POINT ( 'NONE',  ( 150.7691137448031213, 269.5072301123068428, -15.63821625702598084 ) ) ;
#70521 = CARTESIAN_POINT ( 'NONE',  ( 185.8363103352124881, 296.8156583057766511, 4.440193935637427813 ) ) ;
#70522 = CARTESIAN_POINT ( 'NONE',  ( 157.7233946900069839, 257.4620621851055375, 16.86796251324260254 ) ) ;
#70523 = FACE_OUTER_BOUND ( 'NONE', #35206, .T. ) ;
#70524 = CARTESIAN_POINT ( 'NONE',  ( 55.14129374593650113, 193.4548013555410080, -4.594050593750042211 ) ) ;
#70525 = CARTESIAN_POINT ( 'NONE',  ( 69.61542750552385428, 62.56132062511080250, -13.94275833699888345 ) ) ;
#70526 = ORIENTED_EDGE ( 'NONE', *, *, #34499, .T. ) ;
#70527 = LINE ( 'NONE', #1144, #39788 ) ;
#70528 = CARTESIAN_POINT ( 'NONE',  ( 50.00170217996129907, 86.12209509027381671, 10.00000000000000000 ) ) ;
#70529 = EDGE_CURVE ( 'NONE', #70099, #35311, #11174, .T. ) ;
#70530 = CARTESIAN_POINT ( 'NONE',  ( 71.50069359034532113, 71.04066487116593009, -5.105904657311576500 ) ) ;
#70531 = CARTESIAN_POINT ( 'NONE',  ( 173.9473224539459579, 261.8997203040686941, 14.37357808391092284 ) ) ;
#70532 = LINE ( 'NONE', #7742, #100039 ) ;
#70533 = CARTESIAN_POINT ( 'NONE',  ( 202.7973612924478743, 279.3916619310153919, -15.54732529288344089 ) ) ;
#70534 = EDGE_CURVE ( 'NONE', #65714, #76666, #42041, .T. ) ;
#70535 = CARTESIAN_POINT ( 'NONE',  ( 153.8789445373735418, 269.2372782055974767, -15.31005183354254129 ) ) ;
#70536 = CARTESIAN_POINT ( 'NONE',  ( 122.5466773502276254, 234.8927522451417360, -10.00000000000009059 ) ) ;
#70537 = ADVANCED_FACE ( 'NONE', ( #73460 ), #75452, .T. ) ;
#70538 = ORIENTED_EDGE ( 'NONE', *, *, #29795, .F. ) ;
#70539 = EDGE_CURVE ( 'NONE', #62627, #74024, #99252, .T. ) ;
#70540 = CARTESIAN_POINT ( 'NONE',  ( 202.2712651538608668, 280.3028871727136675, 16.13191389836473988 ) ) ;
#70541 = CARTESIAN_POINT ( 'NONE',  ( 176.6558404752379090, 252.2237374370411942, -0.2705739152901737166 ) ) ;
#70542 = AXIS2_PLACEMENT_3D ( 'NONE', #5990, #58190, #5495 ) ;
#70543 = CARTESIAN_POINT ( 'NONE',  ( 29.83685365728618066, 188.0333772461660544, 9.188101187500095079 ) ) ;
#70544 = CARTESIAN_POINT ( 'NONE',  ( 20.18734655506498754, 13.78380873178786636, -6.180339887498949025 ) ) ;
#70545 = CARTESIAN_POINT ( 'NONE',  ( 83.68959111172128473, 48.84214776367139166, -13.33749660644718205 ) ) ;
#70546 = CARTESIAN_POINT ( 'NONE',  ( 47.66616421796179992, 112.2513067263565034, 177.5919119679930134 ) ) ;
#70547 = CARTESIAN_POINT ( 'NONE',  ( 66.54034002427947314, 67.76616102596386781, -6.984587242053489575 ) ) ;
#70549 = CARTESIAN_POINT ( 'NONE',  ( 63.61184440487929947, 207.5333772461660544, 9.188101187500095079 ) ) ;
#70548 = FACE_OUTER_BOUND ( 'NONE', #69728, .T. ) ;
#70550 = CARTESIAN_POINT ( 'NONE',  ( 173.3964598228361353, 287.9493122502211691, 7.531884089513041225 ) ) ;
#70551 = CARTESIAN_POINT ( 'NONE',  ( 163.0344181721474968, 256.4022621988681863, -15.46606454548692788 ) ) ;
#70552 = CARTESIAN_POINT ( 'NONE',  ( 157.0978663001774862, 258.5455091378672137, -17.31223197570816552 ) ) ;
#70553 = CARTESIAN_POINT ( 'NONE',  ( 18.69751666607634988, 11.76426979415088958, 3.090169943749476733 ) ) ;
#70554 = ORIENTED_EDGE ( 'NONE', *, *, #47342, .T. ) ;
#70555 = VECTOR ( 'NONE', #38370, 1000.000000000000000 ) ;
#70556 = CARTESIAN_POINT ( 'NONE',  ( 24.34300500380255983, 194.8615022471903160, 5.000000000000046185 ) ) ;
#70557 = CARTESIAN_POINT ( 'NONE',  ( 186.1263547150109900, 286.8862237501084564, -16.18252752151998308 ) ) ;
#70558 = CARTESIAN_POINT ( 'NONE',  ( 202.3894997978090373, 280.0980987621804275, 16.95659012541789323 ) ) ;
#70559 = CARTESIAN_POINT ( 'NONE',  ( -2.016382903836450691, 160.4548013555409796, -4.594050593750042211 ) ) ;
#70560 = CARTESIAN_POINT ( 'NONE',  ( 34.04181514241641082, 20.44966523072496756, -2.296566073217252530E-15 ) ) ;
#70562 = CARTESIAN_POINT ( 'NONE',  ( 170.9167832255728285, 262.8446361638572739, 16.75413523746211908 ) ) ;
#70561 = CARTESIAN_POINT ( 'NONE',  ( 167.3620191591094510, 262.1387632814340236, -17.17666365667549755 ) ) ;
#70563 = CARTESIAN_POINT ( 'NONE',  ( 189.2895335294923029, 261.7382647175048760, 6.647372333888422524 ) ) ;
#70564 = DIRECTION ( 'NONE',  ( -0.8660254037844359321, -0.5000000000000051070, -0.000000000000000000 ) ) ;
#70565 = CARTESIAN_POINT ( 'NONE',  ( 87.97782240006738164, 43.76496563450900368, 2.369043524150745927 ) ) ;
#70566 = CARTESIAN_POINT ( 'NONE',  ( 66.53847098313150354, 68.80888956264922740, 2.264020422531420440 ) ) ;
#70567 = ORIENTED_EDGE ( 'NONE', *, *, #97843, .F. ) ;
#70568 = CARTESIAN_POINT ( 'NONE',  ( 57.45043449909725553, 210.6427522451419634, -10.00000000000009592 ) ) ;
#70569 = CARTESIAN_POINT ( 'NONE',  ( 178.2990217061593228, 285.7009041265487213, 12.88278519312938286 ) ) ;
#70570 = CARTESIAN_POINT ( 'NONE',  ( 167.7231831693838728, 286.7520842802292691, 0.5032469995052184508 ) ) ;
#70571 = CARTESIAN_POINT ( 'NONE',  ( 9.796739006517501736, 23.84336893147754566, -7.433330006724137462 ) ) ;
#70572 = CARTESIAN_POINT ( 'NONE',  ( 159.0402943516375274, 259.3997371224696735, 16.69638147318008947 ) ) ;
#70573 = CIRCLE ( 'NONE', #73850, 70.00000000000001421 ) ;
#70574 = CARTESIAN_POINT ( 'NONE',  ( 206.6298919378964740, 272.7535241315335384, -9.267551915974392429 ) ) ;
#70575 = CARTESIAN_POINT ( 'NONE',  ( 58.98402115518014455, 204.8615022471902307, -10.00000000000009592 ) ) ;
#70576 = CARTESIAN_POINT ( 'NONE',  ( 192.1640094933931096, 297.8091675017319062, 12.36911124822534447 ) ) ;
#70577 = CARTESIAN_POINT ( 'NONE',  ( 80.49827691776714289, 228.8297689869269220, -2.679491924311252493 ) ) ;
#70578 = AXIS2_PLACEMENT_3D ( 'NONE', #95891, #26452, #4129 ) ;
#70579 = CARTESIAN_POINT ( 'NONE',  ( 190.7405042774493324, 298.2747508605859821, 9.591131971744578877 ) ) ;
#70580 = CARTESIAN_POINT ( 'NONE',  ( 87.63119364650853527, 45.29408460765225897, 6.394950601605620122 ) ) ;
#70581 = CARTESIAN_POINT ( 'NONE',  ( 193.7114073116034945, 295.1289958610702797, 14.86160832869823345 ) ) ;
#70582 = ORIENTED_EDGE ( 'NONE', *, *, #98914, .F. ) ;
#70583 =( BOUNDED_CURVE ( )  B_SPLINE_CURVE ( 2, ( #83528, #68776, #70271, #7996, #99698, #22693, #99201, #14092, #54553 ),
 .UNSPECIFIED., .F., .T. ) 
 B_SPLINE_CURVE_WITH_KNOTS ( ( 3, 2, 2, 2, 3 ),
 ( 0.4153225806451613100, 0.4166666666666666852, 0.4193548387096774355, 0.4220430107526881858, 0.4233870967741935609 ),
 .UNSPECIFIED. ) 
 CURVE ( )  GEOMETRIC_REPRESENTATION_ITEM ( )  RATIONAL_B_SPLINE_CURVE ( ( 0.9330127018922194093, 0.9330127018922194093, 1.000000000000000000, 0.8660254037844387076, 1.000000000000000000, 0.8660254037844387076, 1.000000000000000000, 0.9330127018922194093, 0.9330127018922194093 ) ) 
 REPRESENTATION_ITEM ( '' )  );
#70584 = VERTEX_POINT ( 'NONE', #92189 ) ;
#70585 = CARTESIAN_POINT ( 'NONE',  ( 156.6183249201009176, 277.0683422884322340, -10.04461592201575648 ) ) ;
#70586 = CARTESIAN_POINT ( 'NONE',  ( 73.06253000732938574, 70.71164709794337000, 7.625195754903023371 ) ) ;
#70587 = ORIENTED_EDGE ( 'NONE', *, *, #23073, .T. ) ;
#70588 = CARTESIAN_POINT ( 'NONE',  ( 32.51871346713573274, 102.5332718713895588, 59.99999999999999289 ) ) ;
#70589 = CARTESIAN_POINT ( 'NONE',  ( 188.4805308512120234, 298.0761574053781828, 7.892637567094712203 ) ) ;
#70590 = ORIENTED_EDGE ( 'NONE', *, *, #44364, .T. ) ;
#70591 = CARTESIAN_POINT ( 'NONE',  ( 151.3542526322075901, 269.2885850756041464, -14.28695254860580199 ) ) ;
#70592 = CARTESIAN_POINT ( 'NONE',  ( 79.25000469529436486, 59.07415148808540550, -16.22410911865845762 ) ) ;
#70593 = B_SPLINE_CURVE_WITH_KNOTS ( 'NONE', 3,
 ( #58809, #12757, #36018, #51743, #21823, #36518, #14231, #52709, #67927, #39372, #43620, #82183, #83162, #20852, #23678, #83668, #29427, #74561, #98851, #52216, #45118, #76053, #90782, #66920 ),
 .UNSPECIFIED., .F., .F.,
 ( 4, 2, 2, 2, 2, 2, 2, 2, 2, 2, 2, 4 ),
 ( 0.000000000000000000, 0.1250000000000000833, 0.2500000000000001665, 0.3750000000000002220, 0.4375000000000002776, 0.5000000000000003331, 0.5625000000000003331, 0.6250000000000004441, 0.6875000000000004441, 0.7500000000000004441, 0.8750000000000005551, 1.000000000000000000 ),
 .UNSPECIFIED. ) ;
#70594 = B_SPLINE_CURVE_WITH_KNOTS ( 'NONE', 3,
 ( #73613, #25507, #89362, #65499, #3236, #48820, #79753, #27519, #87393, #96953, #41186, #2728, #18422, #73129, #34120, #49803, #19440, #56892, #65013, #57395, #87876, #10317, #43176, #64002, #81249, #12314, #50295, #72123, #96447, #3722, #58388, #80764, #35094, #17922, #19918, #34600, #42194, #27014, #11335, #2224, #41693, #33105, #80250, #94943, #4194, #57898, #95957, #66001, #50789, #49312, #10817, #26518, #88370, #18928, #56398, #42681 ),
 .UNSPECIFIED., .F., .F.,
 ( 4, 2, 2, 2, 2, 2, 2, 2, 2, 2, 2, 2, 2, 2, 2, 2, 2, 2, 2, 2, 2, 2, 2, 2, 2, 2, 2, 4 ),
 ( 0.0009471700189065799689, 0.001428333720301369712, 0.001909497421696159779, 0.002150079272393554813, 0.002390661123090949414, 0.002510952048439690082, 0.002631242973788430750, 0.002751533899137171418, 0.002871824824485912087, 0.003112406675183393423, 0.003352988525880874759, 0.003834152227275901183, 0.004796479630065955332, 0.005758807032856009915, 0.006239970734251036773, 0.006480552584948509436, 0.006721134435645980364, 0.006781279898320428760, 0.006841425360994876290, 0.006901570823669324686, 0.006961716286343772216, 0.007082007211692641253, 0.007202298137041510291, 0.007442879987739348113, 0.007683461838437184201, 0.007924043689135020288, 0.008164625539832857243, 0.008645789241228626562 ),
 .UNSPECIFIED. ) ;
#70595 = CARTESIAN_POINT ( 'NONE',  ( 149.4908848037268001, 271.7211875819559737, -12.92288068979413573 ) ) ;
#70596 = CARTESIAN_POINT ( 'NONE',  ( 78.21454416846142976, 48.89259193441272089, -15.02001292579780234 ) ) ;
#70597 = ADVANCED_FACE ( 'NONE', ( #14641 ), #44521, .T. ) ;
#70598 = CARTESIAN_POINT ( 'NONE',  ( 80.58471728211203811, 43.44896785130639927, 9.531559131089510473 ) ) ;
#70599 = VERTEX_POINT ( 'NONE', #38419 ) ;
#70600 = CARTESIAN_POINT ( 'NONE',  ( 155.7792811089228735, 260.8293656832279908, 18.01238576999985952 ) ) ;
#70601 = CARTESIAN_POINT ( 'NONE',  ( 191.0816511748900268, 299.6838671013740623, 7.311127128005925790 ) ) ;
#70602 = CARTESIAN_POINT ( 'NONE',  ( 74.14312167556930433, 66.30466486950707861, 1.224646799147354045E-15 ) ) ;
#70603 = ORIENTED_EDGE ( 'NONE', *, *, #23962, .T. ) ;
#70604 = ORIENTED_EDGE ( 'NONE', *, *, #7079, .T. ) ;
#70605 = ORIENTED_EDGE ( 'NONE', *, *, #1768, .T. ) ;
#70606 = CARTESIAN_POINT ( 'NONE',  ( 73.46883546717839408, 61.70975325623787455, 14.87585405357015844 ) ) ;
#70607 = ORIENTED_EDGE ( 'NONE', *, *, #32862, .T. ) ;
#70608 = CARTESIAN_POINT ( 'NONE',  ( 159.4238121903318017, 269.8920955656249134, 15.66160391340022606 ) ) ;
#70609 = EDGE_LOOP ( 'NONE', ( #11193, #36865, #88760, #78085 ) ) ;
#70610 = CARTESIAN_POINT ( 'NONE',  ( 208.2939409893161553, 269.8713066281881083, 2.523744790997269227 ) ) ;
#70611 = CARTESIAN_POINT ( 'NONE',  ( 83.50408885241421331, 50.19109076061639030, 13.73202446986405612 ) ) ;
#70613 = ADVANCED_FACE ( 'NONE', ( #36931 ), #67334, .T. ) ;
#70612 = CARTESIAN_POINT ( 'NONE',  ( 168.2234495781609667, 281.3103526383414419, 11.64684307458802870 ) ) ;
#70614 = CARTESIAN_POINT ( 'NONE',  ( 194.4666154385731431, 293.8209370148700827, -14.56896502715340702 ) ) ;
#70615 = LINE ( 'NONE', #33635, #25662 ) ;
#70616 = CARTESIAN_POINT ( 'NONE',  ( 47.78135487164287554, 106.4364430393875267, -10.00000000000000000 ) ) ;
#70617 = EDGE_LOOP ( 'NONE', ( #79013, #4778, #45045, #76248 ) ) ;
#70618 = CARTESIAN_POINT ( 'NONE',  ( 158.6532760188547400, 266.7985734874461627, -17.41301857359564309 ) ) ;
#70619 = CARTESIAN_POINT ( 'NONE',  ( 19.08967936351193373, 31.99752408145592497, 5.678558825948277544 ) ) ;
#70620 = VECTOR ( 'NONE', #7456, 1000.000000000000114 ) ;
#70621 = CARTESIAN_POINT ( 'NONE',  ( 198.4152875795883801, 277.4255225366634932, -15.34652983819002792 ) ) ;
#70622 = LINE ( 'NONE', #26543, #100063 ) ;
#70624 = ORIENTED_EDGE ( 'NONE', *, *, #70870, .T. ) ;
#70623 = CARTESIAN_POINT ( 'NONE',  ( 159.4230536986738400, 254.5181664265525683, 16.83068086755798376 ) ) ;
#70625 = AXIS2_PLACEMENT_3D ( 'NONE', #72919, #58176, #57672 ) ;
#70626 = CARTESIAN_POINT ( 'NONE',  ( 190.4035152335380019, 300.8584330062341792, 5.540201033361155325 ) ) ;
#70627 = DIRECTION ( 'NONE',  ( -0.9184028970038772277, -0.3956464567955659817, 0.000000000000000000 ) ) ;
#70628 = CARTESIAN_POINT ( 'NONE',  ( 159.3237119419271437, 254.6902313965507858, -15.56765445935501191 ) ) ;
#70629 = CYLINDRICAL_SURFACE ( 'NONE', #69935, 10.00000000000001066 ) ;
#70630 = AXIS2_PLACEMENT_3D ( 'NONE', #92951, #54916, #7832 ) ;
#70631 = CARTESIAN_POINT ( 'NONE',  ( 85.27809249074009301, 45.59539938871965603, -8.958021638074621151 ) ) ;
#70632 = CARTESIAN_POINT ( 'NONE',  ( 161.6256441450323678, 250.7031678651938762, 14.48526717260977037 ) ) ;
#70633 = CARTESIAN_POINT ( 'NONE',  ( 114.4096469973842858, 226.8615022471902023, 5.000000000000051514 ) ) ;
#70634 = ORIENTED_EDGE ( 'NONE', *, *, #65564, .T. ) ;
#70635 = FACE_OUTER_BOUND ( 'NONE', #11973, .T. ) ;
#70636 = DIRECTION ( 'NONE',  ( -1.000000000000000000, 0.000000000000000000, 0.000000000000000000 ) ) ;
#70637 = CARTESIAN_POINT ( 'NONE',  ( 182.5291792280718823, 296.7636338796572204, 0.3805386115670883473 ) ) ;
#70638 = CARTESIAN_POINT ( 'NONE',  ( 9.458193372709603253, 186.2677522451419065, -5.000000000000047962 ) ) ;
#70639 = CARTESIAN_POINT ( 'NONE',  ( 87.80660267098954819, 215.3768266524160424, -9.188101187500093303 ) ) ;
#70640 = CARTESIAN_POINT ( 'NONE',  ( 82.32795736216652926, 40.34849779494332012, -1.094049968420492513 ) ) ;
#70641 = CARTESIAN_POINT ( 'NONE',  ( 13.13113612116928763, 15.78052372038639106, -10.00000000000000355 ) ) ;
#70642 = CARTESIAN_POINT ( 'NONE',  ( 167.0433667443437287, 277.9948742561587665, -14.29907309580385188 ) ) ;
#70644 = CARTESIAN_POINT ( 'NONE',  ( 75.82286285680700644, 65.49053554218845363, 14.29367836297803329 ) ) ;
#70643 = CARTESIAN_POINT ( 'NONE',  ( 18.33521408509785644, 172.2048013555409796, 4.594050593750051981 ) ) ;
#70645 = CARTESIAN_POINT ( 'NONE',  ( 161.7101619467568980, 250.5567787384628389, 13.05644392949610655 ) ) ;
#70646 = VERTEX_POINT ( 'NONE', #82597 ) ;
#70647 = CIRCLE ( 'NONE', #80468, 17.82106496071138224 ) ;
#70648 = ORIENTED_EDGE ( 'NONE', *, *, #42069, .T. ) ;
#70649 = CARTESIAN_POINT ( 'NONE',  ( -58.62427208439002158, 70.56504152958493137, 60.00000000000000000 ) ) ;
#70650 = CARTESIAN_POINT ( 'NONE',  ( 189.0990418739154961, 261.3597260687160428, -6.102409993698818980 ) ) ;
#70651 = EDGE_CURVE ( 'NONE', #8402, #61894, #29348, .T. ) ;
#70652 = CARTESIAN_POINT ( 'NONE',  ( 84.27726345673161745, 46.24452505070916430, -10.39517579047728013 ) ) ;
#70653 = AXIS2_PLACEMENT_3D ( 'NONE', #97203, #20179, #82004 ) ;
#70654 = CARTESIAN_POINT ( 'NONE',  ( 24.93549151006825326, 33.13478043621389446, 8.090169943749478065 ) ) ;
#70655 = CARTESIAN_POINT ( 'NONE',  ( 161.8150574665248200, 250.3750943687383881, -13.25074899737357903 ) ) ;
#70656 = CARTESIAN_POINT ( 'NONE',  ( 87.49069069641790009, 227.9865022471902876, -10.00000000000009592 ) ) ;
#70657 = CARTESIAN_POINT ( 'NONE',  ( 180.6066648745947134, 283.7006809008031496, -16.18202752516933174 ) ) ;
#70658 = CARTESIAN_POINT ( 'NONE',  ( 41.36599039304902448, 188.5643266524159571, -9.188101187500093303 ) ) ;
#70659 = CARTESIAN_POINT ( 'NONE',  ( 197.4319809672400652, 276.3590923837395508, 15.22116115860616503 ) ) ;
#70660 = ORIENTED_EDGE ( 'NONE', *, *, #51004, .T. ) ;
#70661 = CARTESIAN_POINT ( 'NONE',  ( 34.30229714732369217, 180.6115022471902023, -5.000000000000041744 ) ) ;
#70662 = ADVANCED_FACE ( 'NONE', ( #90184 ), #74958, .T. ) ;
#70663 = CARTESIAN_POINT ( 'NONE',  ( 175.2487935740293779, 281.5086999169899968, -14.18879801599889490 ) ) ;
#70664 = PLANE ( 'NONE',  #94355 ) ;
#70665 = CARTESIAN_POINT ( 'NONE',  ( 195.9359860111818250, 291.2759125279654882, 17.49638312768267312 ) ) ;
#70666 = CARTESIAN_POINT ( 'NONE',  ( 68.65502763568917999, 64.17108234953235524, -12.53269806771906580 ) ) ;
#70667 = CARTESIAN_POINT ( 'NONE',  ( 65.98439316910436503, 202.2365022471902307, 10.00000000000009948 ) ) ;
#70668 = CARTESIAN_POINT ( 'NONE',  ( 186.5665755256727039, 282.6830977147599810, 16.17162702254794482 ) ) ;
#70669 = CARTESIAN_POINT ( 'NONE',  ( 194.5252985417586729, 293.7192948986070178, -14.54632727629426370 ) ) ;
#70670 = CARTESIAN_POINT ( 'NONE',  ( 71.60580622982271848, 63.30568055998580945, 14.16434923562446535 ) ) ;
#70671 = CARTESIAN_POINT ( 'NONE',  ( 204.2129321040862919, 276.9398213635460024, 14.41515352680879758 ) ) ;
#70672 = CARTESIAN_POINT ( 'NONE',  ( 188.4708381935227521, 298.8780472021338710, 6.289082596400687564 ) ) ;
#70673 = CARTESIAN_POINT ( 'NONE',  ( 68.31449789920554849, 67.83967261433821250, 7.597146809165362669 ) ) ;
#70674 = CARTESIAN_POINT ( 'NONE',  ( 147.6220714307702622, 274.9580672937808572, 8.392894244419288441 ) ) ;
#70675 = CARTESIAN_POINT ( 'NONE',  ( 180.8071464327592253, 266.9085124479379942, -14.75290084666368351 ) ) ;
#70676 = VERTEX_POINT ( 'NONE', #46010 ) ;
#70677 = CARTESIAN_POINT ( 'NONE',  ( 153.2593913506692616, 267.1939427739956727, -16.45456985337825984 ) ) ;
#70678 = CARTESIAN_POINT ( 'NONE',  ( 207.5290616128274337, 271.1961165699281651, 2.604679844609484984 ) ) ;
#70679 = CARTESIAN_POINT ( 'NONE',  ( 79.36263291408793918, 45.67866562566761957, -12.88899626193393821 ) ) ;
#70680 = CARTESIAN_POINT ( 'NONE',  ( 103.8820256808556906, 230.7833772461660544, -9.188101187500095079 ) ) ;
#70681 = CARTESIAN_POINT ( 'NONE',  ( 18.31506083472495661, 16.28920272979926054, -7.433330006724141015 ) ) ;
#70682 = CARTESIAN_POINT ( 'NONE',  ( -15.51451749852110495, 173.3967562850347406, 6.972266317189433612E-15 ) ) ;
#70683 = DIRECTION ( 'NONE',  ( 0.4999999999999998890, -0.8660254037844385966, 0.000000000000000000 ) ) ;
#70685 = CARTESIAN_POINT ( 'NONE',  ( 195.6664450926536460, 278.3245960621525796, 17.18455885460583232 ) ) ;
#70684 = CARTESIAN_POINT ( 'NONE',  ( 175.3074307085254020, 254.5436327766159650, 9.407465564047683415 ) ) ;
#70686 = CARTESIAN_POINT ( 'NONE',  ( -24.63924516542737919, 141.7012482093459766, -37.49999999999996447 ) ) ;
#70687 = CARTESIAN_POINT ( 'NONE',  ( 25.44954664093420149, 26.64441083166262203, -10.00000000000000533 ) ) ;
#70688 = DIRECTION ( 'NONE',  ( 1.000000000000000000, 0.000000000000000000, 0.000000000000000000 ) ) ;
#70689 = VECTOR ( 'NONE', #79001, 1000.000000000000227 ) ;
#70690 = CARTESIAN_POINT ( 'NONE',  ( 116.4326846683273544, 226.4824982072973683, 3.021315404115420679E-15 ) ) ;
#70691 = CARTESIAN_POINT ( 'NONE',  ( 110.0998739067015606, 222.8262482093458061, 3.021315404115420679E-15 ) ) ;
#70692 = CARTESIAN_POINT ( 'NONE',  ( 85.99011874742393502, 47.63415234044297364, 10.88239874243195260 ) ) ;
#70693 = ORIENTED_EDGE ( 'NONE', *, *, #80791, .T. ) ;
#70694 = CARTESIAN_POINT ( 'NONE',  ( 189.8711135266105146, 266.0314335071855112, 10.76611041489257836 ) ) ;
#70695 = LINE ( 'NONE', #46377, #7006 ) ;
#70696 = AXIS2_PLACEMENT_3D ( 'NONE', #23742, #50541, #12066 ) ;
#70697 = CARTESIAN_POINT ( 'NONE',  ( 196.5244701160910665, 267.6823335762956049, 9.543964429419004247 ) ) ;
#70698 = ORIENTED_EDGE ( 'NONE', *, *, #42609, .T. ) ;
#70699 = B_SPLINE_SURFACE_WITH_KNOTS ( 'NONE', 3, 1, ( 
 ( #1767, #32647 ),
 ( #86912, #9351 ),
 ( #25042, #48356 ),
 ( #9874, #79305 ),
 ( #40731, #33150 ),
 ( #87924, #2777 ),
 ( #64050, #56939 ),
 ( #72171, #94994 ),
 ( #56444, #10364 ),
 ( #33665, #64556 ),
 ( #95516, #26062 ),
 ( #77768, #19486 ),
 ( #10865, #65545 ),
 ( #12870, #27061 ),
 ( #89884, #18975 ),
 ( #50342, #88415 ),
 ( #96491, #36129 ),
 ( #42723, #57437 ),
 ( #19959, #97472 ),
 ( #57943, #65052 ),
 ( #18466, #49849 ),
 ( #81294, #11867 ),
 ( #72684, #51332 ),
 ( #88926, #96002 ),
 ( #73661, #34160 ),
 ( #66050, #80294 ),
 ( #20458, #82300 ),
 ( #43729, #49354 ),
 ( #97957, #4239 ),
 ( #26562, #50836 ),
 ( #28038, #4761 ),
 ( #59414, #35139 ),
 ( #80810, #35643 ),
 ( #74672, #5249 ) ),
 .UNSPECIFIED., .T., .F., .F.,
 ( 4, 2, 2, 2, 2, 2, 2, 2, 2, 2, 2, 2, 2, 2, 2, 2, 4 ),
 ( 2, 2 ),
 ( 0.000000000000000000, 0.06250000000000000000, 0.1250000000000000000, 0.1875000000000000000, 0.2500000000000000000, 0.3125000000000000000, 0.3750000000000000000, 0.4375000000000000000, 0.5000000000000000000, 0.5625000000000000000, 0.6250000000000000000, 0.6875000000000000000, 0.7500000000000000000, 0.8125000000000000000, 0.8750000000000000000, 0.9375000000000000000, 1.000000000000000000 ),
 ( 0.000000000000000000, 1.000000000000000000 ),
 .UNSPECIFIED. ) ;
#70700 = CARTESIAN_POINT ( 'NONE',  ( 79.24868352219918677, 50.32229833407618713, 14.83203819062691764 ) ) ;
#70701 = B_SPLINE_CURVE_WITH_KNOTS ( 'NONE', 3,
 ( #99874, #90821, #68949, #92790 ),
 .UNSPECIFIED., .F., .F.,
 ( 4, 4 ),
 ( 0.01073252529666175389, 0.01912580236392939434 ),
 .UNSPECIFIED. ) ;
#70702 = DIRECTION ( 'NONE',  ( -0.8560416229147732592, -0.5169068966820244970, 0.000000000000000000 ) ) ;
#70703 = CARTESIAN_POINT ( 'NONE',  ( 82.28003896795380001, 40.62557011406286733, -3.142018250819523129 ) ) ;
#70704 = CARTESIAN_POINT ( 'NONE',  ( 152.4425959802508999, 245.4865022471901739, 1.119607411625061291E-15 ) ) ;
#70705 = AXIS2_PLACEMENT_3D ( 'NONE', #55667, #24301, #63292 ) ;
#70706 = ORIENTED_EDGE ( 'NONE', *, *, #2322, .T. ) ;
#70707 = FACE_OUTER_BOUND ( 'NONE', #96540, .T. ) ;
#70708 = CARTESIAN_POINT ( 'NONE',  ( 34.24030602833327208, 37.95586893147758900, 7.433330006724141015 ) ) ;
#70709 = CARTESIAN_POINT ( 'NONE',  ( 72.75811361349980189, 70.26368998748593242, -8.075100041229438474 ) ) ;
#70710 = ORIENTED_EDGE ( 'NONE', *, *, #27580, .F. ) ;
#70711 = CARTESIAN_POINT ( 'NONE',  ( 167.4640110857230582, 280.8630760984805192, 11.65775015378388169 ) ) ;
#70712 = CARTESIAN_POINT ( 'NONE',  ( 166.0506673010352472, 274.1027903476490337, -16.62009509085023851 ) ) ;
#70713 = CARTESIAN_POINT ( 'NONE',  ( 114.7524487161677058, 230.3927522451417929, -10.00000000000009237 ) ) ;
#70714 = ORIENTED_EDGE ( 'NONE', *, *, #5220, .T. ) ;
#70715 = CARTESIAN_POINT ( 'NONE',  ( 86.54479369881731543, 47.18726309986306688, -10.63286291588202204 ) ) ;
#70716 = DIRECTION ( 'NONE',  ( 0.9563064286990893281, -0.2923662333936556945, 0.000000000000000000 ) ) ;
#70717 = CARTESIAN_POINT ( 'NONE',  ( 204.1953342137782954, 276.9703018036655067, 13.84727111424505885 ) ) ;
#70718 = CARTESIAN_POINT ( 'NONE',  ( 199.9502294570856407, 265.6703872523112295, 6.360370400932541246E-13 ) ) ;
#70719 = CARTESIAN_POINT ( 'NONE',  ( -52.57320609282758994, 32.70376883311633520, -10.00000000000000000 ) ) ;
#70720 = EDGE_CURVE ( 'NONE', #62347, #100289, #37420, .T. ) ;
#70721 = CYLINDRICAL_SURFACE ( 'NONE', #4901, 10.00000000000010658 ) ;
#70722 = AXIS2_PLACEMENT_3D ( 'NONE', #36841, #60123, #75875 ) ;
#70723 = CARTESIAN_POINT ( 'NONE',  ( 35.00594278435062989, 181.0177522451417929, 5.000000000000051514 ) ) ;
#70724 = VERTEX_POINT ( 'NONE', #28332 ) ;
#70725 = EDGE_CURVE ( 'NONE', #80478, #41871, #9446, .T. ) ;
#70726 = VERTEX_POINT ( 'NONE', #45521 ) ;
#70727 = CARTESIAN_POINT ( 'NONE',  ( 163.3548548005089174, 249.5016276120636860, 11.44428125521734962 ) ) ;
#70728 = ORIENTED_EDGE ( 'NONE', *, *, #47722, .F. ) ;
#70729 = CARTESIAN_POINT ( 'NONE',  ( 77.16668814154863298, 49.29486154796829567, -15.38919878964156496 ) ) ;
#70730 = ORIENTED_EDGE ( 'NONE', *, *, #6026, .F. ) ;
#70731 = CARTESIAN_POINT ( 'NONE',  ( 74.54670819670354831, 56.70307473271788723, 16.07195883519789703 ) ) ;
#70732 = CARTESIAN_POINT ( 'NONE',  ( 79.39877852727147456, 54.29655282685389039, 15.92112751935395920 ) ) ;
#70733 = VERTEX_POINT ( 'NONE', #67845 ) ;
#70734 = CARTESIAN_POINT ( 'NONE',  ( 183.7658459069459695, 280.9060072218711639, -16.15935528051975467 ) ) ;
#70735 = CARTESIAN_POINT ( 'NONE',  ( 206.2880451275741223, 273.3456201754175368, -11.28869033117385534 ) ) ;
#70736 = CARTESIAN_POINT ( 'NONE',  ( 190.1806134411257290, 301.2445102357908127, 1.963143373670005243 ) ) ;
#70737 = CARTESIAN_POINT ( 'NONE',  ( -10.80656490723494123, 24.88181024604956804, 10.00000000000000000 ) ) ;
#70738 = CARTESIAN_POINT ( 'NONE',  ( 79.41088169706156918, 46.22695399816395678, 12.63871909588431564 ) ) ;
#70740 = EDGE_CURVE ( 'NONE', #74234, #21771, #76452, .T. ) ;
#70739 = CARTESIAN_POINT ( 'NONE',  ( 169.4595697446889631, 250.2531843026321496, -5.478044125683344312 ) ) ;
#70741 = DIRECTION ( 'NONE',  ( -0.000000000000000000, -0.000000000000000000, 1.000000000000000000 ) ) ;
#70742 = CARTESIAN_POINT ( 'NONE',  ( 157.7939826016823304, 280.9050555316971440, 2.087917227061603320 ) ) ;
#70743 = CARTESIAN_POINT ( 'NONE',  ( 133.0835800865360170, 238.4548013555409796, -4.594050593750042211 ) ) ;
#70744 = EDGE_LOOP ( 'NONE', ( #95460, #43743 ) ) ;
#70745 = CARTESIAN_POINT ( 'NONE',  ( 185.1104244301751578, 261.7904637200641673, -9.069498223535303438 ) ) ;
#70746 = CARTESIAN_POINT ( 'NONE',  ( 43.77620770598743150, 30.98920272979930601, 7.433330006724137462 ) ) ;
#70747 = ORIENTED_EDGE ( 'NONE', *, *, #48508, .F. ) ;
#70749 = ORIENTED_EDGE ( 'NONE', *, *, #88057, .T. ) ;
#70748 = CARTESIAN_POINT ( 'NONE',  ( 85.74825148587619594, 48.61567592689142003, -12.33318615817161934 ) ) ;
#70750 = CARTESIAN_POINT ( 'NONE',  ( 202.8857220437332955, 275.8096136465296695, 13.30856319272651511 ) ) ;
#70751 = CARTESIAN_POINT ( 'NONE',  ( 180.7946767411322355, 256.2352744486502161, 1.150915517461931659 ) ) ;
#70752 = CARTESIAN_POINT ( 'NONE',  ( 174.2171726394180666, 290.5684288936432154, -4.877197793559998829 ) ) ;
#70753 = CARTESIAN_POINT ( 'NONE',  ( 147.4643594168521474, 275.2312325148511718, 3.404945201207095540 ) ) ;
#70754 = CARTESIAN_POINT ( 'NONE',  ( 71.92913702268965892, 61.41965493978950263, 14.61815708677550418 ) ) ;
#70755 = CARTESIAN_POINT ( 'NONE',  ( 164.2897805489690768, 249.8104079013010335, 11.36607573508163505 ) ) ;
#70756 = CARTESIAN_POINT ( 'NONE',  ( 78.72526120150082818, 53.56602875328650981, 16.28398236204086302 ) ) ;
#70757 = ADVANCED_FACE ( 'NONE', ( #28847 ), #51648, .F. ) ;
#70758 = CARTESIAN_POINT ( 'NONE',  ( 174.9303175201940803, 282.4108518568261843, 14.59670604635778979 ) ) ;
#70759 = CARTESIAN_POINT ( 'NONE',  ( 177.7342311040593756, 255.2532439957012684, -8.367404576774948310 ) ) ;
#70760 = ORIENTED_EDGE ( 'NONE', *, *, #46855, .T. ) ;
#70761 = CARTESIAN_POINT ( 'NONE',  ( 148.1004780136491377, 274.1294427855589788, -7.811560775291159331 ) ) ;
#70762 = CARTESIAN_POINT ( 'NONE',  ( 66.01919585322798412, 68.69228577893747456, -0.4091825812074046942 ) ) ;
#70763 = ORIENTED_EDGE ( 'NONE', *, *, #59425, .F. ) ;
#70764 = CARTESIAN_POINT ( 'NONE',  ( -19.65312891409030271, 93.06504152958497400, -10.00000000000000888 ) ) ;
#70765 = CARTESIAN_POINT ( 'NONE',  ( 190.6453411250757313, 284.1316474202013183, -17.46766191648467625 ) ) ;
#70766 = CARTESIAN_POINT ( 'NONE',  ( 191.9852310057781040, 298.1188209255817014, -9.473644331849939704 ) ) ;
#70767 = CARTESIAN_POINT ( 'NONE',  ( 149.6036070299368532, 271.5259469590175740, 11.63513718912356865 ) ) ;
#70768 = VECTOR ( 'NONE', #99433, 1000.000000000000114 ) ;
#70769 = CARTESIAN_POINT ( 'NONE',  ( 204.6288132990387965, 273.0563504000126045, -9.947042290372426265 ) ) ;
#70771 = CARTESIAN_POINT ( 'NONE',  ( 151.4859849967579919, 274.9594807944311015, -8.716721077935043027 ) ) ;
#70770 = CARTESIAN_POINT ( 'NONE',  ( 164.7092427929301550, 283.9547367519082854, -6.819220165404522582 ) ) ;
#70772 = DIRECTION ( 'NONE',  ( 0.4999999999999998890, -0.8660254037844385966, 0.000000000000000000 ) ) ;
#70773 = ORIENTED_EDGE ( 'NONE', *, *, #20301, .T. ) ;
#70775 = CARTESIAN_POINT ( 'NONE',  ( 147.5177358149801421, 275.1387818813681179, 4.867883209065928085 ) ) ;
#70774 = VECTOR ( 'NONE', #33842, 1000.000000000000114 ) ;
#70776 = EDGE_CURVE ( 'NONE', #86172, #32812, #86830, .T. ) ;
#70777 = CARTESIAN_POINT ( 'NONE',  ( 66.17343954913512505, 68.52301864461630032, -2.711686016849372827 ) ) ;
#70778 = CARTESIAN_POINT ( 'NONE',  ( 193.5405458432471164, 276.0738629501939272, -16.60598989773238188 ) ) ;
#70779 = CARTESIAN_POINT ( 'NONE',  ( 149.0710170770012724, 245.3262482093457777, 3.021315404115420679E-15 ) ) ;
#70780 = EDGE_CURVE ( 'NONE', #826, #50951, #5542, .T. ) ;
#70781 = CARTESIAN_POINT ( 'NONE',  ( 188.5029508706952015, 298.7682505406680775, -3.886380934741553883 ) ) ;
#70782 = B_SPLINE_CURVE_WITH_KNOTS ( 'NONE', 3,
 ( #83234, #97434, #82264, #82759, #83742, #14305, #97922, #91837, #28004, #5214, #43697, #66508, #98924, #51817, #59891, #45191, #75613, #12836, #58882, #51292, #76130, #35610, #89850, #36095, #6705, #28498 ),
 .UNSPECIFIED., .F., .F.,
 ( 4, 2, 2, 2, 2, 2, 2, 2, 2, 2, 2, 2, 4 ),
 ( 0.0004635842473323659716, 0.001626875584096156924, 0.002790166920859947931, 0.003371812589241843759, 0.003517224006337276842, 0.003662635423432709925, 0.003735341131980426683, 0.003808046840528143441, 0.003953458257623576957, 0.004244281091814402357, 0.004535103926005227756, 0.004825926760196054023, 0.005116749594386879423 ),
 .UNSPECIFIED. ) ;
#70783 = CARTESIAN_POINT ( 'NONE',  ( 85.68485941944550177, 48.66523437743575187, 11.91861461389294163 ) ) ;
#70784 = CARTESIAN_POINT ( 'NONE',  ( 74.40608543823466903, 68.34271654374390437, 11.85151599582641424 ) ) ;
#70785 = EDGE_CURVE ( 'NONE', #6903, #37817, #36427, .T. ) ;
#70786=STYLED_ITEM('',(#100338),#76056);
#70787 = CARTESIAN_POINT ( 'NONE',  ( -5.895715345004023611, 160.7365022471902023, -10.00000000000009237 ) ) ;
#70788 = CARTESIAN_POINT ( 'NONE',  ( 68.56904214663958896, 70.19644423968159686, 0.8067628227658676376 ) ) ;
#70789 = CARTESIAN_POINT ( 'NONE',  ( -11.73236572436687730, 164.0333772461660544, 9.188101187500095079 ) ) ;
#70790 = CARTESIAN_POINT ( 'NONE',  ( 92.21748570181026139, 233.2369531367911009, -4.594050593750048428 ) ) ;
#70791 = DIRECTION ( 'NONE',  ( 0.1162373735601320568, 0.9932214622066130039, 0.000000000000000000 ) ) ;
#70792 = CARTESIAN_POINT ( 'NONE',  ( 192.4743214706506365, 297.2716913909250707, -12.17804856100553046 ) ) ;
#70793 = CARTESIAN_POINT ( 'NONE',  ( 182.2991478702006134, 275.2734891516705034, -17.80812521087705846 ) ) ;
#70794 = CARTESIAN_POINT ( 'NONE',  ( 155.1601726304954809, 261.9016930232608615, -18.56587418422714464 ) ) ;
#70795 = EDGE_CURVE ( 'NONE', #14672, #67236, #94174, .T. ) ;
#70796 = B_SPLINE_CURVE_WITH_KNOTS ( 'NONE', 3,
 ( #61237, #37433, #84103, #68343 ),
 .UNSPECIFIED., .F., .F.,
 ( 4, 4 ),
 ( 0.03983647665132224180, 0.04828245132308466026 ),
 .UNSPECIFIED. ) ;
#70797 = CARTESIAN_POINT ( 'NONE',  ( 78.07803331781863676, 55.04206026085086023, 16.09808790484326835 ) ) ;
#70798 = CARTESIAN_POINT ( 'NONE',  ( 84.72317995036203797, 49.82855470703300682, -13.16391237593562025 ) ) ;
#70799 = VECTOR ( 'NONE', #84856, 1000.000000000000114 ) ;
#70800 = CARTESIAN_POINT ( 'NONE',  ( 77.95473461231914314, 62.00593549909827118, 15.66743434672346424 ) ) ;
#70802 = CARTESIAN_POINT ( 'NONE',  ( 76.04288044954796533, 51.24135356845017242, 16.11949329745968384 ) ) ;
#70801 = CARTESIAN_POINT ( 'NONE',  ( 66.95957972044308804, 66.97324061659901417, 8.659915215018605394 ) ) ;
#70803 = EDGE_CURVE ( 'NONE', #23380, #50052, #11977, .T. ) ;
#70804 = CARTESIAN_POINT ( 'NONE',  ( 161.3538429669452512, 251.1739413151977089, 12.93463751804771533 ) ) ;
#70805 = EDGE_CURVE ( 'NONE', #20627, #11925, #99750, .T. ) ;
#70806 = CARTESIAN_POINT ( 'NONE',  ( 165.9674733710236296, 249.3024098291379289, -9.244165487746641929 ) ) ;
#70807 = CARTESIAN_POINT ( 'NONE',  ( 164.7631898711947827, 245.2687792564100562, -5.064413554850759169 ) ) ;
#70808 = CARTESIAN_POINT ( 'NONE',  ( 195.7291850945597957, 291.6341022226063160, 17.08310330964873813 ) ) ;
#70809 = CARTESIAN_POINT ( 'NONE',  ( 32.30839531297598910, 123.0650415295850593, -25.00000000000000000 ) ) ;
#70810 = CARTESIAN_POINT ( 'NONE',  ( 73.03680373040982943, 57.44200512075386911, -15.87150009157571873 ) ) ;
#70811 = CARTESIAN_POINT ( 'NONE',  ( 31.67681054456310008, 201.3464784336661353, 1.353441290958777327E-15 ) ) ;
#70812 = VECTOR ( 'NONE', #83422, 1000.000000000000114 ) ;
#70813 = CARTESIAN_POINT ( 'NONE',  ( 68.53719034102077501, 216.5024278399160664, 9.188101187500095079 ) ) ;
#70814 = PLANE ( 'NONE',  #74141 ) ;
#70815 = CARTESIAN_POINT ( 'NONE',  ( 88.54549197286583251, 43.89854493182281203, -0.2370037879772141087 ) ) ;
#70816 = CARTESIAN_POINT ( 'NONE',  ( 84.44366846031314822, 49.29134167535947597, -12.87259635285258952 ) ) ;
#70818 = CARTESIAN_POINT ( 'NONE',  ( 72.17108608572740991, 71.17802923003300464, -6.704596218806396557 ) ) ;
#70817 = DIRECTION ( 'NONE',  ( -0.8660254037844378194, -0.5000000000000014433, -0.000000000000000000 ) ) ;
#70819 = CARTESIAN_POINT ( 'NONE',  ( 200.2320358376919103, 270.9633186839029690, -11.45871590196247070 ) ) ;
#70820 = CARTESIAN_POINT ( 'NONE',  ( 22.15746398174156440, 34.83396525600390703, -2.839279412974133887 ) ) ;
#70821 = CYLINDRICAL_SURFACE ( 'NONE', #98427, 16.60714546451156792 ) ;
#70822 = CARTESIAN_POINT ( 'NONE',  ( 79.94121550646556784, 47.70160699126887494, -13.39487937175259091 ) ) ;
#70823 = CARTESIAN_POINT ( 'NONE',  ( 13.03712377304622194, 16.03085787977761356, 9.188101187500006262 ) ) ;
#70824 = CARTESIAN_POINT ( 'NONE',  ( 64.58612298413676456, 208.0958772461660544, -9.188101187500095079 ) ) ;
#70825 = FACE_OUTER_BOUND ( 'NONE', #49310, .T. ) ;
#70826 = CARTESIAN_POINT ( 'NONE',  ( 202.7602807045765019, 279.4558873931827065, -15.90558713185497020 ) ) ;
#70827 = CARTESIAN_POINT ( 'NONE',  ( 198.2114954873088948, 287.3346145022089786, 18.52864136173620935 ) ) ;
#70828 = CARTESIAN_POINT ( 'NONE',  ( 73.83071771892932134, 66.06232275870847559, 12.79940641639033672 ) ) ;
#70829 = CARTESIAN_POINT ( 'NONE',  ( 153.8947951769603719, 264.0933910635359325, 16.60696150718446518 ) ) ;
#70830 = CARTESIAN_POINT ( 'NONE',  ( 76.63808522071934703, 56.32536596566799858, -16.16213633644409242 ) ) ;
#70831 = CARTESIAN_POINT ( 'NONE',  ( 115.3478411848173835, 230.7365022471902023, 10.00000000000009592 ) ) ;
#70832 = DIRECTION ( 'NONE',  ( -0.9974094913373522386, -0.07193265315671491800, 0.000000000000000000 ) ) ;
#70833 = CARTESIAN_POINT ( 'NONE',  ( 164.2953672501826929, 246.0790718049323687, -2.576662677987826111 ) ) ;
#70834 = ORIENTED_EDGE ( 'NONE', *, *, #99971, .T. ) ;
#70835 = CARTESIAN_POINT ( 'NONE',  ( 77.49963593495350267, 49.62430142007526257, 14.92239454847386959 ) ) ;
#70836 = VECTOR ( 'NONE', #40761, 1000.000000000000114 ) ;
#70837 = CARTESIAN_POINT ( 'NONE',  ( 82.30387339498274457, 53.64944443644737504, 15.82386716188995734 ) ) ;
#70838 = ORIENTED_EDGE ( 'NONE', *, *, #55531, .T. ) ;
#70839 = CARTESIAN_POINT ( 'NONE',  ( 159.3995226465659982, 254.5589234043588078, -16.81133486613867234 ) ) ;
#70840 = CARTESIAN_POINT ( 'NONE',  ( 194.2428668711552007, 293.6808394427342819, 14.33833691752719375 ) ) ;
#70841 = CARTESIAN_POINT ( 'NONE',  ( 72.54644133328486078, 68.79346617608341319, -9.755494697606795995 ) ) ;
#70842 = ORIENTED_EDGE ( 'NONE', *, *, #39180, .T. ) ;
#70843 = DIRECTION ( 'NONE',  ( -0.1654779384134575648, 0.9862134920484671996, 0.000000000000000000 ) ) ;
#70844 = ORIENTED_EDGE ( 'NONE', *, *, #29406, .F. ) ;
#70845 = LINE ( 'NONE', #85599, #74960 ) ;
#70846 = CARTESIAN_POINT ( 'NONE',  ( 167.4264173877831468, 247.7494294226382294, 3.562207888615490425 ) ) ;
#70847 = DIRECTION ( 'NONE',  ( -0.5344452582589588330, 0.8452030915256492083, 0.000000000000000000 ) ) ;
#70848 = VECTOR ( 'NONE', #15078, 1000.000000000000000 ) ;
#70849 = VERTEX_POINT ( 'NONE', #1943 ) ;
#70850 = ADVANCED_FACE ( 'NONE', ( #87107 ), #17645, .T. ) ;
#70851 = AXIS2_PLACEMENT_3D ( 'NONE', #20026, #59985, #50900 ) ;
#70852 = CARTESIAN_POINT ( 'NONE',  ( 27.26159103020561147, 24.24335787977764767, -9.188101187500008038 ) ) ;
#70853 = CARTESIAN_POINT ( 'NONE',  ( 21.87918239556003641, 194.9860189848785410, -2.679491924311252493 ) ) ;
#70854 = CARTESIAN_POINT ( 'NONE',  ( 75.09735448162263083, 66.37212636226136908, -13.14697353001001545 ) ) ;
#70855 = CARTESIAN_POINT ( 'NONE',  ( 79.90451369755943745, 49.15256129334691337, -14.17871552535267909 ) ) ;
#70856 = ADVANCED_FACE ( 'NONE', ( #23223 ), #63233, .T. ) ;
#70857 = ORIENTED_EDGE ( 'NONE', *, *, #96425, .T. ) ;
#70858 = DIRECTION ( 'NONE',  ( -0.8660254037844377084, -0.5000000000000014433, -0.000000000000000000 ) ) ;
#70859 = DIRECTION ( 'NONE',  ( 0.3002896333693371722, 0.9538480676139722281, 0.000000000000000000 ) ) ;
#70860 = ORIENTED_EDGE ( 'NONE', *, *, #44476, .F. ) ;
#70861 = CARTESIAN_POINT ( 'NONE',  ( 170.8150813163964585, 284.7511851418007609, 11.02223257947848012 ) ) ;
#70862 = AXIS2_PLACEMENT_3D ( 'NONE', #56197, #3536, #64823 ) ;
#70864 = CARTESIAN_POINT ( 'NONE',  ( 68.09452353918298684, 66.09134662472550303, -10.53294727184536406 ) ) ;
#70863 = CARTESIAN_POINT ( 'NONE',  ( 162.9111130980074620, 284.4370125796830848, -2.463596310689824875 ) ) ;
#70865 = CARTESIAN_POINT ( 'NONE',  ( 81.77434258213597218, 55.39018043030689853, -15.93420164564364150 ) ) ;
#70866 = CARTESIAN_POINT ( 'NONE',  ( 194.2764122224708103, 294.1503786489221284, 15.46903869661980835 ) ) ;
#70867 = CARTESIAN_POINT ( 'NONE',  ( 160.8753431536632945, 265.5703843255740253, 17.74957321532883014 ) ) ;
#70868 = CARTESIAN_POINT ( 'NONE',  ( 164.3157126687612504, 265.7538407082229241, -17.18074097244921816 ) ) ;
#70870 = EDGE_CURVE ( 'NONE', #18263, #18179, #18967, .T. ) ;
#70869 = CARTESIAN_POINT ( 'NONE',  ( 133.4890956248536895, 254.0024278399161233, 9.188101187500095079 ) ) ;
#70871 = CARTESIAN_POINT ( 'NONE',  ( 206.8217325168575371, 270.0045844243117017, 3.350393751014514532 ) ) ;
#70872 = VECTOR ( 'NONE', #9290, 1000.000000000000000 ) ;
#70873 = CARTESIAN_POINT ( 'NONE',  ( 79.09523395582193928, 59.82262253747457237, 16.49691284064748231 ) ) ;
#70874 = CARTESIAN_POINT ( 'NONE',  ( 77.73871025623044773, 221.8149278399160949, -9.188101187500095079 ) ) ;
#70875 = VERTEX_POINT ( 'NONE', #438 ) ;
#70876 = CARTESIAN_POINT ( 'NONE',  ( 34.73896580337741113, 43.55466486950702887, 7.012934429366973338E-14 ) ) ;
#70877 = CARTESIAN_POINT ( 'NONE',  ( 78.08878743907096975, 62.01730706715306951, -16.03713534414099939 ) ) ;
#70878 = VERTEX_POINT ( 'NONE', #16630 ) ;
#70879 = CARTESIAN_POINT ( 'NONE',  ( 195.6782192648066427, 291.7223776291889408, -15.68068164243272022 ) ) ;
#70880 = ORIENTED_EDGE ( 'NONE', *, *, #33162, .T. ) ;
#70881 = B_SPLINE_CURVE_WITH_KNOTS ( 'NONE', 3,
 ( #50451, #90505, #12981, #66652 ),
 .UNSPECIFIED., .F., .F.,
 ( 4, 4 ),
 ( 0.04313187872937399719, 0.04472034873244652015 ),
 .UNSPECIFIED. ) ;
#70882 = ORIENTED_EDGE ( 'NONE', *, *, #2733, .T. ) ;
#70883 = CARTESIAN_POINT ( 'NONE',  ( 80.29316516335838116, 44.72160512723912973, -11.71951212942682119 ) ) ;
#70884 = PLANE ( 'NONE',  #81819 ) ;
#70885 = EDGE_CURVE ( 'NONE', #93322, #62754, #2091, .T. ) ;
#70886 = FACE_OUTER_BOUND ( 'NONE', #31485, .T. ) ;
#70887 = CARTESIAN_POINT ( 'NONE',  ( 67.76563652183371289, 65.64620069392987034, 10.05537879187873074 ) ) ;
#70888 = CARTESIAN_POINT ( 'NONE',  ( 47.85994450909318232, 209.9860189848785410, -2.679491924311201423 ) ) ;
#70889 = CARTESIAN_POINT ( 'NONE',  ( 207.5492168967516875, 271.1612065941299079, 2.279797467183042325 ) ) ;
#70890 = EDGE_CURVE ( 'NONE', #99040, #47742, #15940, .T. ) ;
#70891 = CARTESIAN_POINT ( 'NONE',  ( 79.20030167299918844, 216.5333772461660544, 9.188101187500095079 ) ) ;
#70892 = ORIENTED_EDGE ( 'NONE', *, *, #67438, .F. ) ;
#70893 = VERTEX_POINT ( 'NONE', #88101 ) ;
#70894 = LINE ( 'NONE', #63279, #39897 ) ;
#70895 = CARTESIAN_POINT ( 'NONE',  ( 163.2742264920156572, 247.8477394797576778, -9.850275379362519956 ) ) ;
#70896 = EDGE_LOOP ( 'NONE', ( #94897, #97897, #93553, #80023 ) ) ;
#70897 = CARTESIAN_POINT ( 'NONE',  ( 75.93601443309867705, 65.18730796954976370, -14.47772449952195117 ) ) ;
#70898 = DIRECTION ( 'NONE',  ( -0.8660254037844369313, -0.5000000000000029976, -0.000000000000000000 ) ) ;
#70899 = DIRECTION ( 'NONE',  ( 1.000000000000000000, 0.000000000000000000, 0.000000000000000000 ) ) ;
#70900 = CARTESIAN_POINT ( 'NONE',  ( 87.75230366022445594, 44.21248639555269477, 4.670146826978180954 ) ) ;
#70901 = VERTEX_POINT ( 'NONE', #72867 ) ;
#70902 = CARTESIAN_POINT ( 'NONE',  ( 83.07363809413841693, 43.66347682277865516, -7.925384865395641576 ) ) ;
#70903 = CARTESIAN_POINT ( 'NONE',  ( 184.7820298688179719, 260.0036009586479508, 6.327424396724815381 ) ) ;
#70904 = CARTESIAN_POINT ( 'NONE',  ( 206.3454060440500086, 273.2462681537123785, -9.268083217908118954 ) ) ;
#70905 = CARTESIAN_POINT ( 'NONE',  ( 193.9866089479436368, 275.7653998617566913, 16.75281791482838400 ) ) ;
#70906 = CARTESIAN_POINT ( 'NONE',  ( 174.6633675210554486, 283.9072383021423320, 13.76783388809871056 ) ) ;
#70907 =( BOUNDED_CURVE ( )  B_SPLINE_CURVE ( 2, ( #70779, #38363, #69273, #62156, #47472, #93103, #30787 ),
 .UNSPECIFIED., .F., .T. ) 
 B_SPLINE_CURVE_WITH_KNOTS ( ( 3, 2, 2, 3 ),
 ( 0.9798387096774193727, 0.9811827956989247479, 0.9838709677419354982, 0.9855294979220013962 ),
 .UNSPECIFIED. ) 
 CURVE ( )  GEOMETRIC_REPRESENTATION_ITEM ( )  RATIONAL_B_SPLINE_CURVE ( ( 0.9330127018922194093, 0.9330127018922194093, 1.000000000000000000, 0.8660254037844387076, 1.000000000000000000, 0.9173412610389377608, 0.9366789799084298540 ) ) 
 REPRESENTATION_ITEM ( '' )  );
#70908 = CYLINDRICAL_SURFACE ( 'NONE', #93732, 10.00000000000010658 ) ;
#70909 = B_SPLINE_CURVE_WITH_KNOTS ( 'NONE', 3,
 ( #49820, #56415, #4212, #71647, #64528, #34133, #88893, #18943, #11351, #72141, #50311, #10336, #73142, #42207 ),
 .UNSPECIFIED., .F., .F.,
 ( 4, 2, 2, 2, 2, 2, 4 ),
 ( 0.0007774119382052871018, 0.001058953235776235405, 0.001340494533347183926, 0.001622035830918132230, 0.001903577128489080750, 0.002466659723631069515, 0.003029742318773058496 ),
 .UNSPECIFIED. ) ;
#70910 = CARTESIAN_POINT ( 'NONE',  ( 195.5865870811380205, 279.6577477989692397, -17.40305323361667433 ) ) ;
#70911 = VERTEX_POINT ( 'NONE', #57620 ) ;
#70912 = CARTESIAN_POINT ( 'NONE',  ( 203.3892195006453107, 277.9383451777727032, -14.51582383987914149 ) ) ;
#70913 = EDGE_CURVE ( 'NONE', #71581, #21771, #90456, .T. ) ;
#70914 = CARTESIAN_POINT ( 'NONE',  ( 181.1156277128715431, 292.7914473640799997, 9.490545386343454126 ) ) ;
#70915 = CARTESIAN_POINT ( 'NONE',  ( 83.94554275650895647, 42.35676708697683068, 4.096087114950127450 ) ) ;
#70916 = CARTESIAN_POINT ( 'NONE',  ( 185.5597808477625961, 264.6293126611748789, -11.95344273703673466 ) ) ;
#70917 = CARTESIAN_POINT ( 'NONE',  ( 83.82333528792250377, 52.03156133651413739, 14.57194887151437968 ) ) ;
#70918 = CARTESIAN_POINT ( 'NONE',  ( 153.7922915876480090, 270.4832132560703712, 14.01318345560697765 ) ) ;
#70919 = ORIENTED_EDGE ( 'NONE', *, *, #45650, .T. ) ;
#70920 = AXIS2_PLACEMENT_3D ( 'NONE', #750, #62534, #24052 ) ;
#70921 = EDGE_CURVE ( 'NONE', #45184, #58863, #88599, .T. ) ;
#70922 = CARTESIAN_POINT ( 'NONE',  ( -15.11550709823832861, 102.3030086117089752, 44.38387608498982928 ) ) ;
#70923 = VECTOR ( 'NONE', #53286, 1000.000000000000227 ) ;
#70924 = CIRCLE ( 'NONE', #79045, 17.82106496071138935 ) ;
#70925 = EDGE_CURVE ( 'NONE', #57797, #34618, #93983, .T. ) ;
#70926 = CARTESIAN_POINT ( 'NONE',  ( 165.0509870607838252, 244.7702999017660375, -2.356357909806504392 ) ) ;
#70928 = CARTESIAN_POINT ( 'NONE',  ( 73.74393169614602073, 55.22324961333944060, 16.59624740907808871 ) ) ;
#70927 = CARTESIAN_POINT ( 'NONE',  ( 180.2669822489033322, 266.6255696747526258, -14.77114471355729108 ) ) ;
#70929 = CARTESIAN_POINT ( 'NONE',  ( 70.01283242295176024, 62.80173547756309915, -13.36538303052352283 ) ) ;
#70930 = CARTESIAN_POINT ( 'NONE',  ( 34.29273532275193759, 21.92755873383628185, 6.180339887498953466 ) ) ;
#70931 = CARTESIAN_POINT ( 'NONE',  ( 162.8496566865346438, 284.5585608631904506, -4.049346908545373047 ) ) ;
#70932 = CARTESIAN_POINT ( 'NONE',  ( 160.1969820541083607, 255.1776831935258372, -16.37528374203482073 ) ) ;
#70933 = CARTESIAN_POINT ( 'NONE',  ( 188.3509091528505905, 260.8885577967712379, 2.876703767957366598 ) ) ;
#70934 = CARTESIAN_POINT ( 'NONE',  ( 195.3381664883222300, 265.3235058747017092, -7.510424545325947498 ) ) ;
#70935 = VECTOR ( 'NONE', #97516, 1000.000000000000114 ) ;
#70936 = CARTESIAN_POINT ( 'NONE',  ( 6.102605256642664067, 165.1423013555410080, -4.594050593750043987 ) ) ;
#70937 = CARTESIAN_POINT ( 'NONE',  ( -27.42236680055714260, 166.5217562850347406, 1.224646799147364892E-15 ) ) ;
#70938 = VERTEX_POINT ( 'NONE', #59979 ) ;
#70939 = VECTOR ( 'NONE', #55582, 1000.000000000000000 ) ;
#70941 = CARTESIAN_POINT ( 'NONE',  ( 160.2340067623557616, 254.0231382518209386, -15.28591403396486470 ) ) ;
#70940 = B_SPLINE_CURVE_WITH_KNOTS ( 'NONE', 3,
 ( #79398, #24151, #86017, #88017, #49446, #47931, #72273, #80399, #78368, #39817, #70748, #9964, #63145, #40826, #86510, #71772, #33248, #41842, #73262, #80909, #34251, #20064, #73756, #4348, #58049, #11481, #3856, #35244, #19579, #66151, #57536 ),
 .UNSPECIFIED., .F., .F.,
 ( 4, 3, 3, 3, 3, 3, 3, 3, 3, 3, 4 ),
 ( 0.000000000000000000, 0.1333490885032397044, 0.3007194338854659588, 0.4699862290245639951, 0.5844252810809660303, 0.6686540514503046539, 0.7354980260655714641, 0.8028463152565815664, 0.8633854507757389163, 0.9437142632667553377, 1.000000000000000000 ),
 .UNSPECIFIED. ) ;
#70942 = DIRECTION ( 'NONE',  ( -0.8660254037844387076, -0.4999999999999998890, -0.000000000000000000 ) ) ;
#70943 = CARTESIAN_POINT ( 'NONE',  ( 81.87359138905077316, 41.32955797133629972, 5.976920566261187950 ) ) ;
#70944 = CARTESIAN_POINT ( 'NONE',  ( 13.16551753867071461, 190.6589784336661637, -6.496448406907676862E-16 ) ) ;
#70945 = CARTESIAN_POINT ( 'NONE',  ( 173.2322951681075551, 290.9646578649885669, 3.668310523228456965 ) ) ;
#70946 = CARTESIAN_POINT ( 'NONE',  ( 34.45917901495312208, 20.86426979415091765, -3.090169943749474069 ) ) ;
#70947 = B_SPLINE_CURVE_WITH_KNOTS ( 'NONE', 3,
 ( #11246, #33526, #63421, #72035, #1128, #56813, #49714, #64928, #94854, #87302 ),
 .UNSPECIFIED., .F., .F.,
 ( 4, 2, 2, 2, 4 ),
 ( 0.000000000000000000, 0.2500000000000000000, 0.5000000000000000000, 0.7500000000000000000, 1.000000000000000000 ),
 .UNSPECIFIED. ) ;
#70948 = CARTESIAN_POINT ( 'NONE',  ( 189.4090321304425970, 263.6681562366250091, -10.67085280218717003 ) ) ;
#70949 = CARTESIAN_POINT ( 'NONE',  ( 147.2592533090473239, 275.5864867145116932, -0.3770461397900867762 ) ) ;
#70950 = DIRECTION ( 'NONE',  ( 0.000000000000000000, 0.000000000000000000, 1.000000000000000000 ) ) ;
#70951 = CARTESIAN_POINT ( 'NONE',  ( 81.64195525244801388, 42.01227061513564109, 7.558743156282623055 ) ) ;
#70952 = B_SPLINE_SURFACE_WITH_KNOTS ( 'NONE', 3, 1, ( 
 ( #21949, #22449 ),
 ( #53345, #76652 ),
 ( #45730, #7241 ),
 ( #44732, #28055 ),
 ( #58930, #20479 ),
 ( #82318, #43746 ),
 ( #5268, #13375 ),
 ( #67051, #97974 ),
 ( #20986, #51869 ),
 ( #29073, #59938 ),
 ( #75668, #68050 ),
 ( #6252, #16347 ),
 ( #70540, #46743 ),
 ( #40127, #8748 ),
 ( #71066, #70035 ),
 ( #15837, #93384 ),
 ( #23937, #55328 ),
 ( #86305, #84787 ),
 ( #78160, #54835 ),
 ( #648, #16839 ),
 ( #47241, #94385 ),
 ( #61437, #15326 ),
 ( #69546, #79195 ),
 ( #85818, #32551 ),
 ( #53827, #9769 ),
 ( #47730, #7749 ),
 ( #30554, #78663 ),
 ( #77670, #151 ),
 ( #31535, #55815 ),
 ( #24938, #93893 ),
 ( #39619, #69039 ),
 ( #86808, #22937 ),
 ( #31040, #99969 ),
 ( #1668, #92391 ) ),
 .UNSPECIFIED., .T., .F., .F.,
 ( 4, 2, 2, 2, 2, 2, 2, 2, 2, 2, 2, 2, 2, 2, 2, 2, 4 ),
 ( 2, 2 ),
 ( 0.000000000000000000, 0.06250000000000000000, 0.1250000000000000000, 0.1875000000000000000, 0.2500000000000000000, 0.3125000000000000000, 0.3750000000000000000, 0.4375000000000000000, 0.5000000000000000000, 0.5625000000000000000, 0.6250000000000000000, 0.6875000000000000000, 0.7500000000000000000, 0.8125000000000000000, 0.8750000000000000000, 0.9375000000000000000, 1.000000000000000000 ),
 ( 0.000000000000000000, 1.000000000000000000 ),
 .UNSPECIFIED. ) ;
#70953 = CARTESIAN_POINT ( 'NONE',  ( 186.9530661741948450, 295.9748403543025574, -7.697179163675227365 ) ) ;
#70954 = CARTESIAN_POINT ( 'NONE',  ( 190.7500944235871998, 261.9717678648361812, -0.8447403391411513196 ) ) ;
#70955 = CARTESIAN_POINT ( 'NONE',  ( 74.64464720694877542, 207.2365022471902023, -10.00000000000009059 ) ) ;
#70956 = CARTESIAN_POINT ( 'NONE',  ( 68.63741997012778029, 66.83210094663463963, -9.273233233882304916 ) ) ;
#70957 = CIRCLE ( 'NONE', #83932, 12.50000000000000000 ) ;
#70958 = DIRECTION ( 'NONE',  ( -0.4999999999999987788, 0.8660254037844392627, 0.000000000000000000 ) ) ;
#70959 = B_SPLINE_CURVE_WITH_KNOTS ( 'NONE', 3,
 ( #51468, #59042, #12999, #81419 ),
 .UNSPECIFIED., .F., .F.,
 ( 4, 4 ),
 ( 0.03583253215054491014, 0.04455304000076568821 ),
 .UNSPECIFIED. ) ;
#70960 = FACE_OUTER_BOUND ( 'NONE', #12933, .T. ) ;
#70961 = CARTESIAN_POINT ( 'NONE',  ( 29.51209413086700906, 187.8458772461660544, 9.188101187500095079 ) ) ;
#70962 = CARTESIAN_POINT ( 'NONE',  ( 159.2303255284352304, 254.8519814094557603, 16.39103317446447150 ) ) ;
#70963 = EDGE_CURVE ( 'NONE', #45691, #35211, #29885, .T. ) ;
#70964 = DIRECTION ( 'NONE',  ( -0.8660254037844377084, -0.5000000000000014433, -0.000000000000000000 ) ) ;
#70965 = CARTESIAN_POINT ( 'NONE',  ( 45.88188149789386472, 72.29567966924399514, 10.00000000000000000 ) ) ;
#70966 = DIRECTION ( 'NONE',  ( -0.9957145386939475484, -0.09248003802712848054, 0.000000000000000000 ) ) ;
#70967 = VERTEX_POINT ( 'NONE', #33863 ) ;
#70968 = CARTESIAN_POINT ( 'NONE',  ( 80.56248746614238598, 223.9865022471902876, 10.00000000000009415 ) ) ;
#70969 = CYLINDRICAL_SURFACE ( 'NONE', #63585, 70.00000000000002842 ) ;
#70970 = CARTESIAN_POINT ( 'NONE',  ( 163.2169812233754840, 281.0183292176826626, -10.13472441872696805 ) ) ;
#70971 = LINE ( 'NONE', #62841, #61712 ) ;
#70972 = CARTESIAN_POINT ( 'NONE',  ( 28.14623683147711830, 18.11110640527293114, -2.839279412974138328 ) ) ;
#70973 = CARTESIAN_POINT ( 'NONE',  ( 163.2437751800324293, 247.9004826992694461, 9.806027032984305336 ) ) ;
#70974 = CARTESIAN_POINT ( 'NONE',  ( 197.0226655822963551, 289.3937282992477549, -17.28982543158101493 ) ) ;
#70975 = VECTOR ( 'NONE', #34289, 1000.000000000000000 ) ;
#70976 = CARTESIAN_POINT ( 'NONE',  ( 185.5122645235197467, 267.6225438542603570, -14.65295725662480386 ) ) ;
#70977 = ORIENTED_EDGE ( 'NONE', *, *, #11405, .T. ) ;
#70978 = CARTESIAN_POINT ( 'NONE',  ( 185.5535017383455454, 290.7975388464344064, 12.55098773011679469 ) ) ;
#70979 = CARTESIAN_POINT ( 'NONE',  ( 9.553764119070450533, 20.91421378149917132, 9.188101187500008038 ) ) ;
#70980 = CARTESIAN_POINT ( 'NONE',  ( 78.13494257139964816, 58.08983479524191296, -16.20152750994855495 ) ) ;
#70981 = CARTESIAN_POINT ( 'NONE',  ( 71.85962433970722429, 72.56121191805073067, -1.249447308665279088 ) ) ;
#70982 = ORIENTED_EDGE ( 'NONE', *, *, #59092, .T. ) ;
#70983 = CARTESIAN_POINT ( 'NONE',  ( 25.50001727096127979, 173.9824982072973967, 3.021315404115420679E-15 ) ) ;
#70984 = CARTESIAN_POINT ( 'NONE',  ( 71.98137461515177904, 71.49844079294172161, -5.753101040561137580 ) ) ;
#70985 = CARTESIAN_POINT ( 'NONE',  ( 191.4044787581200069, 299.1247133251352466, 7.435199718141230818 ) ) ;
#70986 = CARTESIAN_POINT ( 'NONE',  ( 181.0633185409454597, 257.6960604115657816, -7.513758380418855687 ) ) ;
#70987 = ORIENTED_EDGE ( 'NONE', *, *, #5083, .F. ) ;
#70988 = ORIENTED_EDGE ( 'NONE', *, *, #50326, .F. ) ;
#70990 = CARTESIAN_POINT ( 'NONE',  ( 81.35748880148537410, 42.22347387491733173, -7.155507324468848296 ) ) ;
#70989 = CARTESIAN_POINT ( 'NONE',  ( 148.3010860587701814, 276.5068540982774721, -3.904121881399305050 ) ) ;
#70991 = ORIENTED_EDGE ( 'NONE', *, *, #20153, .T. ) ;
#70992 = CARTESIAN_POINT ( 'NONE',  ( 200.9445292274600092, 282.6008612054670266, -16.62830946367346741 ) ) ;
#70993 = AXIS2_PLACEMENT_3D ( 'NONE', #52795, #31000, #29517 ) ;
#70994 = DIRECTION ( 'NONE',  ( 0.8755176446346986108, -0.4831861483251663203, 0.000000000000000000 ) ) ;
#70995 = CARTESIAN_POINT ( 'NONE',  ( 79.95899844298520520, 58.10650356627559887, 16.26824798947572148 ) ) ;
#70996 = DIRECTION ( 'NONE',  ( 0.000000000000000000, 0.000000000000000000, 1.000000000000000000 ) ) ;
#70997 = CARTESIAN_POINT ( 'NONE',  ( 204.9658583905037688, 275.6357147811169170, -12.57240504404813564 ) ) ;
#70999 = EDGE_CURVE ( 'NONE', #65627, #33084, #9527, .T. ) ;
#70998 = CARTESIAN_POINT ( 'NONE',  ( 100.7430306879021060, 216.7202760586659167, -5.415160957724236172E-17 ) ) ;
#71000 = AXIS2_PLACEMENT_3D ( 'NONE', #9151, #17239, #2567 ) ;
#71001 = CARTESIAN_POINT ( 'NONE',  ( 181.5074763156532072, 287.3577042999648370, -13.30743195732708450 ) ) ;
#71002 = ORIENTED_EDGE ( 'NONE', *, *, #74554, .T. ) ;
#71003 = VECTOR ( 'NONE', #94551, 1000.000000000000000 ) ;
#71004 = CARTESIAN_POINT ( 'NONE',  ( 162.1885223555109974, 266.5710106843741869, 17.09332258216276657 ) ) ;
#71005 = EDGE_LOOP ( 'NONE', ( #75112, #93549, #67487, #27348 ) ) ;
#71006 = CARTESIAN_POINT ( 'NONE',  ( 21.83270445532239989, 34.64646525600390703, -2.839279412974133887 ) ) ;
#71007 = CARTESIAN_POINT ( 'NONE',  ( 157.2469855225926381, 258.6801040481246332, 16.82957450039010538 ) ) ;
#71008 = CARTESIAN_POINT ( 'NONE',  ( 78.54120617833643792, 48.00853119821599790, -13.98189004695917959 ) ) ;
#71009 = CARTESIAN_POINT ( 'NONE',  ( 59.17381130624904984, 192.7202760586659451, -5.415160957724236172E-17 ) ) ;
#71010 = ADVANCED_FACE ( 'NONE', ( #95697 ), #26244, .F. ) ;
#71011 = CARTESIAN_POINT ( 'NONE',  ( 74.01669459151050035, 68.61891074470059948, 10.90943161386742055 ) ) ;
#71012 = CARTESIAN_POINT ( 'NONE',  ( 35.16829885187633664, 20.70852965304481685, 1.583844403245364907 ) ) ;
#71013 = CARTESIAN_POINT ( 'NONE',  ( 150.2982063762752603, 270.3228656002555681, 14.90512853129094495 ) ) ;
#71014 = CARTESIAN_POINT ( 'NONE',  ( 176.6036273517752875, 273.2589018324615608, 17.10821691637876540 ) ) ;
#71015 = EDGE_CURVE ( 'NONE', #74234, #77633, #29112, .T. ) ;
#71016 = ORIENTED_EDGE ( 'NONE', *, *, #27450, .F. ) ;
#71017 = AXIS2_PLACEMENT_3D ( 'NONE', #94812, #54246, #40055 ) ;
#71018 = CARTESIAN_POINT ( 'NONE',  ( 190.7573459890224683, 299.4656496600463242, 6.232719852847871778 ) ) ;
#71019 = CARTESIAN_POINT ( 'NONE',  ( 86.05859607216220297, 43.31872955745066633, -3.244090947481843568 ) ) ;
#71020 = CARTESIAN_POINT ( 'NONE',  ( 147.2443490232117256, 275.6123016948292275, 5.226063659459642352 ) ) ;
#71021 = FACE_OUTER_BOUND ( 'NONE', #66868, .T. ) ;
#71022 = EDGE_LOOP ( 'NONE', ( #82995, #47784, #4859, #58721, #65020, #4319 ) ) ;
#71023 = CARTESIAN_POINT ( 'NONE',  ( 174.5672763864540968, 261.0320004397244702, -14.05403048710671854 ) ) ;
#71024 = CARTESIAN_POINT ( 'NONE',  ( 170.6811438746260592, 275.2999556018212388, -16.27734202032215904 ) ) ;
#71025 = CARTESIAN_POINT ( 'NONE',  ( 207.7320178805681508, 270.8445860024863237, -5.379955943374661764 ) ) ;
#71026 = CARTESIAN_POINT ( 'NONE',  ( 147.4824818982269790, 275.1998434563504929, -4.972419998968698351 ) ) ;
#71027 = CARTESIAN_POINT ( 'NONE',  ( 190.8138402884741254, 300.1477291634665789, 4.037153726988762514 ) ) ;
#71028 = CARTESIAN_POINT ( 'NONE',  ( 180.5385023393456834, 271.2514381441214368, 16.52379068675051599 ) ) ;
#71029 = CYLINDRICAL_SURFACE ( 'NONE', #9445, 17.82106496071139645 ) ;
#71030 = CARTESIAN_POINT ( 'NONE',  ( 67.34387953621143197, 66.59329343503119958, 8.595237674194807553 ) ) ;
#71031 = CARTESIAN_POINT ( 'NONE',  ( 72.42134570124093784, 65.10669864484587777, -12.85055710188708566 ) ) ;
#71032 = CARTESIAN_POINT ( 'NONE',  ( 163.7038023771459052, 247.1036922210055025, -6.448491958542482472 ) ) ;
#71033 = CARTESIAN_POINT ( 'NONE',  ( 112.2171730965159071, 247.8464784336661353, 1.353441290958777327E-15 ) ) ;
#71034 = ORIENTED_EDGE ( 'NONE', *, *, #98607, .F. ) ;
#71035 = CARTESIAN_POINT ( 'NONE',  ( 191.2111338740054975, 299.4595964878050154, -9.718193530796334301 ) ) ;
#71036 = CARTESIAN_POINT ( 'NONE',  ( 84.09826433023697234, 41.84909642707336985, -0.5111001068266544101 ) ) ;
#71037 = CARTESIAN_POINT ( 'NONE',  ( 155.6281496932864457, 261.0911329737299980, -18.07904265579665548 ) ) ;
#71038 = CARTESIAN_POINT ( 'NONE',  ( 163.7239493340838123, 247.0687966679708438, 6.286946239157660266 ) ) ;
#71039 = DIRECTION ( 'NONE',  ( -0.8660254037844387076, -0.4999999999999998890, -0.000000000000000000 ) ) ;
#71040 = CARTESIAN_POINT ( 'NONE',  ( 177.9425579050794965, 255.3610639913140972, 4.864846912946482860 ) ) ;
#71041 = EDGE_LOOP ( 'NONE', ( #29608, #84322, #75851, #79756 ) ) ;
#71042 = CARTESIAN_POINT ( 'NONE',  ( 207.5959034698703078, 271.0803430774575418, -1.830000129038042544 ) ) ;
#71043 = ADVANCED_FACE ( 'NONE', ( #52391 ), #82848, .T. ) ;
#71044 = CARTESIAN_POINT ( 'NONE',  ( 158.4807356281016553, 274.9683795502273824, -12.52945643738231674 ) ) ;
#71045 = CARTESIAN_POINT ( 'NONE',  ( 182.4400702163412404, 260.6821622823035227, 9.500263120530494376 ) ) ;
#71046 = CARTESIAN_POINT ( 'NONE',  ( 206.4738852556816369, 273.0237356314501085, -9.746110091792012042 ) ) ;
#71047 = CARTESIAN_POINT ( 'NONE',  ( 134.7341806906763395, 248.5958772461660544, -9.188101187500095079 ) ) ;
#71048 = CARTESIAN_POINT ( 'NONE',  ( 189.8764391022526183, 294.5890629899907935, -12.42416005126432310 ) ) ;
#71049 = CARTESIAN_POINT ( 'NONE',  ( -22.42236680055709641, 157.8615022471902591, 0.000000000000000000 ) ) ;
#71050 = CARTESIAN_POINT ( 'NONE',  ( 196.3341081413628899, 290.5863447708742342, 16.12390540996472410 ) ) ;
#71051 = CYLINDRICAL_SURFACE ( 'NONE', #9456, 10.00000000000010658 ) ;
#71052 = CARTESIAN_POINT ( 'NONE',  ( 51.43353571204313823, 194.3768266524159856, -9.188101187500091527 ) ) ;
#71053 = CARTESIAN_POINT ( 'NONE',  ( 85.60276959248551520, 48.33120518904961926, -11.70778487545583602 ) ) ;
#71054 = CARTESIAN_POINT ( 'NONE',  ( 88.07430803657909735, 44.66886354398342007, -4.226991484831405188 ) ) ;
#71055 = ADVANCED_FACE ( 'NONE', ( #26736 ), #1390, .F. ) ;
#71056 = CARTESIAN_POINT ( 'NONE',  ( 80.36752454425955250, 44.74486481172305474, -11.70255150684123002 ) ) ;
#71057 = CARTESIAN_POINT ( 'NONE',  ( 171.5539035853818746, 260.2959543727399705, 14.72132304298182248 ) ) ;
#71058 = CARTESIAN_POINT ( 'NONE',  ( 151.4588969340128983, 278.2628330447197982, -1.654564867966292319 ) ) ;
#71059 = CARTESIAN_POINT ( 'NONE',  ( 178.8787720380167912, 291.7606112093855018, -6.206199073717809434 ) ) ;
#71060 = DIRECTION ( 'NONE',  ( 1.000000000000000000, -1.070572202317114942E-14, 0.000000000000000000 ) ) ;
#71061 = CARTESIAN_POINT ( 'NONE',  ( 153.7185388398659711, 269.2090732872851504, -15.41358683631291271 ) ) ;
#71062 = CARTESIAN_POINT ( 'NONE',  ( 127.5984922056368731, 231.1427522451417360, 1.119607411625061291E-15 ) ) ;
#71063 = FACE_OUTER_BOUND ( 'NONE', #43455, .T. ) ;
#71064 = VERTEX_POINT ( 'NONE', #38679 ) ;
#71065 = AXIS2_PLACEMENT_3D ( 'NONE', #94631, #63695, #56070 ) ;
#71066 = CARTESIAN_POINT ( 'NONE',  ( 202.3425522658138505, 280.1794142728863903, 15.86053073629060961 ) ) ;
#71067 = CARTESIAN_POINT ( 'NONE',  ( 12.21574338843640284, 25.79103043416548147, 8.090169943749478065 ) ) ;
#71068 = CARTESIAN_POINT ( 'NONE',  ( 18.68642948779652002, 193.8464784336661637, 1.353441290958777327E-15 ) ) ;
#71069 = AXIS2_PLACEMENT_3D ( 'NONE', #88788, #73047, #49718 ) ;
#71070 = CARTESIAN_POINT ( 'NONE',  ( 18.45529574749610902, 12.78380873178786281, -6.180339887498949025 ) ) ;
#71071 = CARTESIAN_POINT ( 'NONE',  ( 188.7203383489409134, 290.4861718803290955, -14.87964105563550277 ) ) ;
#71072 = CARTESIAN_POINT ( 'NONE',  ( -19.52403302344049507, 93.00632194460597191, 59.99999999999999289 ) ) ;
#71073 = CARTESIAN_POINT ( 'NONE',  ( 42.25626477193290498, 60.39660150822810891, 177.5919119679930134 ) ) ;
#71075 = CARTESIAN_POINT ( 'NONE',  ( 58.38862868653046689, 194.5177522451417929, 5.000000000000051514 ) ) ;
#71074 = CARTESIAN_POINT ( 'NONE',  ( 177.1262862392189845, 269.6057104283654553, 17.56656865388298172 ) ) ;
#71076 = CARTESIAN_POINT ( 'NONE',  ( 6.591042624459347188, 19.50829794293877839, -10.00000000000000355 ) ) ;
#71077 = CARTESIAN_POINT ( 'NONE',  ( 184.2320252568399894, 257.8019328292739374, 1.345153837617685255 ) ) ;
#71078 = CARTESIAN_POINT ( 'NONE',  ( 204.9184781223158609, 275.7177798128946620, -12.59106622113254126 ) ) ;
#71079 = CARTESIAN_POINT ( 'NONE',  ( 66.45302924825351454, 68.82209965975525279, -4.357771214034995566 ) ) ;
#71080 = ORIENTED_EDGE ( 'NONE', *, *, #16047, .T. ) ;
#71081 = EDGE_CURVE ( 'NONE', #81724, #45554, #52887, .T. ) ;
#71082 = AXIS2_PLACEMENT_3D ( 'NONE', #99875, #42781, #4297 ) ;
#71083 = CARTESIAN_POINT ( 'NONE',  ( 161.4250356354754672, 267.9004136800010656, 17.49898951125957680 ) ) ;
#71084 = CARTESIAN_POINT ( 'NONE',  ( 28.60096323907606219, 193.9865022471902876, 10.00000000000009237 ) ) ;
#71085 = CARTESIAN_POINT ( 'NONE',  ( 39.40823858692152015, 186.8927522451417929, -10.00000000000009237 ) ) ;
#71086 = CARTESIAN_POINT ( 'NONE',  ( 162.6626107288841467, 248.9070890562113902, 10.12509462564867313 ) ) ;
#71087 = CARTESIAN_POINT ( 'NONE',  ( -7.997804718428996651, 172.3149278399160949, -9.188101187500095079 ) ) ;
#71088 = CARTESIAN_POINT ( 'NONE',  ( 40.31210609084968866, 28.98920272979929535, 7.433330006724137462 ) ) ;
#71091 = EDGE_CURVE ( 'NONE', #50887, #11410, #7793, .T. ) ;
#71090 = CARTESIAN_POINT ( 'NONE',  ( 181.2305971022323661, 265.9781236237157032, -15.82518789413146010 ) ) ;
#71089 = CARTESIAN_POINT ( 'NONE',  ( 80.32771389996757705, 57.94408260071153194, -16.24746918486169633 ) ) ;
#71092 = CARTESIAN_POINT ( 'NONE',  ( 187.8353293621520663, 261.5626033622391446, 6.406781397797947086 ) ) ;
#71093 = CARTESIAN_POINT ( 'NONE',  ( 205.7829192689729325, 274.2205238267313234, 11.21202327925415254 ) ) ;
#71094 = CARTESIAN_POINT ( 'NONE',  ( 187.1283629995790250, 258.9907284234702161, -2.438144316879867990 ) ) ;
#71095 = CARTESIAN_POINT ( 'NONE',  ( 65.83313805523765438, 68.98304839603784444, 2.094471952982813523 ) ) ;
#71096 = EDGE_LOOP ( 'NONE', ( #90696, #87396, #28003, #71202 ) ) ;
#71097 = CYLINDRICAL_SURFACE ( 'NONE', #17999, 17.82106496071139645 ) ;
#71098 = SHAPE_REPRESENTATION_RELATIONSHIP ( 'NONE' , 'NONE' ,  #77412, #29552 ) ;
#71099 = CARTESIAN_POINT ( 'NONE',  ( 178.4448961284112158, 285.5018398465763312, 12.98938652614517153 ) ) ;
#71100 = CARTESIAN_POINT ( 'NONE',  ( 153.2952765687912802, 277.6672861512745385, -5.343879082789506185 ) ) ;
#71101 = CARTESIAN_POINT ( 'NONE',  ( 8.584303441219292452, 23.14336893147753571, 7.433330006724141015 ) ) ;
#71102 = AXIS2_PLACEMENT_3D ( 'NONE', #27100, #10400, #64598 ) ;
#71103 = CARTESIAN_POINT ( 'NONE',  ( 160.6541084136885615, 252.3859171132495476, 15.19188851725936118 ) ) ;
#71104 = CARTESIAN_POINT ( 'NONE',  ( 159.2713554375903300, 254.7809155221686410, -15.70062444474382168 ) ) ;
#71105 = CARTESIAN_POINT ( 'NONE',  ( 63.33450210234187239, 195.8262482093458061, 3.021315404115420679E-15 ) ) ;
#71106 = CARTESIAN_POINT ( 'NONE',  ( 23.46864935082055581, 158.3759306620404743, -30.52142883766493853 ) ) ;
#71107 = CARTESIAN_POINT ( 'NONE',  ( 104.7876960802104946, 219.7592609112380160, 2.679491924311254714 ) ) ;
#71108 = CARTESIAN_POINT ( 'NONE',  ( 87.66825142739060084, 45.41049311418420587, 6.595692451674659118 ) ) ;
#71109 = DIRECTION ( 'NONE',  ( -0.5000000000000012212, 0.8660254037844378194, -0.000000000000000000 ) ) ;
#71110 = ORIENTED_EDGE ( 'NONE', *, *, #12345, .F. ) ;
#71111 = CARTESIAN_POINT ( 'NONE',  ( 155.7862279768771714, 277.0639705730557694, -10.34674495731000654 ) ) ;
#71112 = FACE_OUTER_BOUND ( 'NONE', #1940, .T. ) ;
#71113 = ORIENTED_EDGE ( 'NONE', *, *, #96152, .T. ) ;
#71114 = DIRECTION ( 'NONE',  ( 0.4803199113995043623, -0.8770933717188679202, 0.000000000000000000 ) ) ;
#71115 = LINE ( 'NONE', #87385, #66160 ) ;
#71116 = ORIENTED_EDGE ( 'NONE', *, *, #67438, .T. ) ;
#71117 = CARTESIAN_POINT ( 'NONE',  ( 146.5046981847821428, 276.8934145268504494, 0.02269072295920678689 ) ) ;
#71118 = CARTESIAN_POINT ( 'NONE',  ( 79.38384574407295702, 59.10269726290196246, -16.22807843983317255 ) ) ;
#71119 = LINE ( 'NONE', #10813, #90149 ) ;
#71120 = CARTESIAN_POINT ( 'NONE',  ( 176.0798903307563990, 267.4715319269637916, 17.29251186195777379 ) ) ;
#71121 = ORIENTED_EDGE ( 'NONE', *, *, #64706, .T. ) ;
#71122 = CARTESIAN_POINT ( 'NONE',  ( 161.0952649348064938, 251.6218116045831437, 13.81854265722852482 ) ) ;
#71123 = DIRECTION ( 'NONE',  ( 1.000000000000000000, 0.000000000000000000, 0.000000000000000000 ) ) ;
#71124 = CARTESIAN_POINT ( 'NONE',  ( 177.3946647576825910, 293.3261284689752415, 3.859629117064975468 ) ) ;
#71125 = CARTESIAN_POINT ( 'NONE',  ( 66.59506449235166770, 69.13094975345107684, 3.575540226172965408 ) ) ;
#71126 = CARTESIAN_POINT ( 'NONE',  ( 151.3579658450212264, 274.9463947945409359, -8.627328198253888303 ) ) ;
#71127 = ORIENTED_EDGE ( 'NONE', *, *, #33879, .F. ) ;
#71128 = CARTESIAN_POINT ( 'NONE',  ( 193.2752197284765998, 263.9480352582601768, 7.898392093415175452 ) ) ;
#71129 = ORIENTED_EDGE ( 'NONE', *, *, #75925, .T. ) ;
#71130 = ADVANCED_FACE ( 'NONE', ( #53385, #31076 ), #23470, .F. ) ;
#71131 = ORIENTED_EDGE ( 'NONE', *, *, #85646, .T. ) ;
#71132 = CARTESIAN_POINT ( 'NONE',  ( 73.81332162787411733, 63.24887547442293112, 14.34933433100697009 ) ) ;
#71133 = EDGE_LOOP ( 'NONE', ( #67725, #66495, #76001, #24362 ) ) ;
#71134 = EDGE_CURVE ( 'NONE', #4349, #8776, #48296, .T. ) ;
#71135 = CARTESIAN_POINT ( 'NONE',  ( 19.39999966495784989, 36.48715600906563594, -10.00000000000000000 ) ) ;
#71136 = ORIENTED_EDGE ( 'NONE', *, *, #3307, .F. ) ;
#71137 = CARTESIAN_POINT ( 'NONE',  ( 81.52669532789981588, 44.57943870447123658, 10.20249863168784721 ) ) ;
#71138 = EDGE_CURVE ( 'NONE', #75897, #42311, #9814, .T. ) ;
#71139 = CARTESIAN_POINT ( 'NONE',  ( 166.8502408137956081, 271.8018640180155217, 16.11660651124998367 ) ) ;
#71140 = CARTESIAN_POINT ( 'NONE',  ( 71.47986246715085201, 69.49463484872732977, 7.994332015353252885 ) ) ;
#71141 = EDGE_CURVE ( 'NONE', #99910, #6796, #26007, .T. ) ;
#71142 = CARTESIAN_POINT ( 'NONE',  ( 194.3177355571849318, 294.0788045336591381, -15.93712594727561616 ) ) ;
#71144 = CARTESIAN_POINT ( 'NONE',  ( 82.65877604426773928, 53.27536003831319533, -15.29495776700401954 ) ) ;
#71143 = CIRCLE ( 'NONE', #27455, 7.499999999999996447 ) ;
#71145 = CARTESIAN_POINT ( 'NONE',  ( 197.7108840479781122, 288.2016989499799138, -17.75818441575643902 ) ) ;
#71146 = ORIENTED_EDGE ( 'NONE', *, *, #47881, .T. ) ;
#71147 = DIRECTION ( 'NONE',  ( -0.7280311630581435267, -0.6855440362341479466, 0.000000000000000000 ) ) ;
#71148 = CARTESIAN_POINT ( 'NONE',  ( 20.33338779993010803, 20.24335787977762990, -9.188101187500008038 ) ) ;
#71149 = CARTESIAN_POINT ( 'NONE',  ( 205.7867067512454184, 274.2139637150027056, 10.62737868262404106 ) ) ;
#71150 = CARTESIAN_POINT ( 'NONE',  ( 190.7404869014439726, 298.2747809567102308, -9.591077548819823662 ) ) ;
#71151 = AXIS2_PLACEMENT_3D ( 'NONE', #99082, #29664, #60541 ) ;
#71153 = VERTEX_POINT ( 'NONE', #8789 ) ;
#71152 = CARTESIAN_POINT ( 'NONE',  ( -19.65312891409030271, 93.06504152958497400, 10.00000000000000888 ) ) ;
#71154 = CARTESIAN_POINT ( 'NONE',  ( 190.9873456450184506, 299.8472090705463984, 5.391280221519696880 ) ) ;
#71155 = CARTESIAN_POINT ( 'NONE',  ( 154.1396649810517090, 268.6945475872249744, 16.07262325421418936 ) ) ;
#71156 = CARTESIAN_POINT ( 'NONE',  ( 159.7692415128758228, 253.9185515433934768, -16.85856106119654285 ) ) ;
#71157 = DIRECTION ( 'NONE',  ( -0.8660254037844387076, -0.4999999999999998890, -0.000000000000000000 ) ) ;
#71158 = CARTESIAN_POINT ( 'NONE',  ( 200.9111546617170916, 282.6586676490145464, 17.66063511622358106 ) ) ;
#71159 = CARTESIAN_POINT ( 'NONE',  ( 112.7497649734640959, 229.2365022471902307, 10.00000000000009948 ) ) ;
#71160 = VECTOR ( 'NONE', #98715, 1000.000000000000114 ) ;
#71161 = ORIENTED_EDGE ( 'NONE', *, *, #10728, .F. ) ;
#71162 = CARTESIAN_POINT ( 'NONE',  ( 190.7982574810033611, 262.8194055429554510, 8.405793748174573921 ) ) ;
#71163 = CYLINDRICAL_SURFACE ( 'NONE', #3122, 70.00000000000002842 ) ;
#71164 = B_SPLINE_CURVE_WITH_KNOTS ( 'NONE', 3,
 ( #24215, #85567, #16112, #84556, #914, #8026, #1425, #94151, #9010, #31302 ),
 .UNSPECIFIED., .F., .F.,
 ( 4, 2, 2, 2, 4 ),
 ( 0.000000000000000000, 0.0002622400424273183960, 0.0005244800848546367919, 0.0007867201272819552421, 0.001048960169709273584 ),
 .UNSPECIFIED. ) ;
#71165 = CARTESIAN_POINT ( 'NONE',  ( 126.0342816572616016, 255.1199935810940929, 2.679491924311251605 ) ) ;
#71166 = DIRECTION ( 'NONE',  ( -0.9606745773021557744, 0.2776767122488390527, 0.000000000000000000 ) ) ;
#71167 = CARTESIAN_POINT ( 'NONE',  ( 9.891206074601820220, 186.5177522451419065, 5.000000000000046185 ) ) ;
#71168 = CARTESIAN_POINT ( 'NONE',  ( 86.94057726720511425, 214.8768266524160140, 9.188101187500096856 ) ) ;
#71169 = CARTESIAN_POINT ( 'NONE',  ( 72.44129552685039641, 70.67501955208014408, -7.848061272651214004 ) ) ;
#71170 = FACE_OUTER_BOUND ( 'NONE', #72014, .T. ) ;
#71171 = FACE_OUTER_BOUND ( 'NONE', #13085, .T. ) ;
#71173 = CARTESIAN_POINT ( 'NONE',  ( -44.49648453423614569, 28.96346851210257967, 10.00000000000000000 ) ) ;
#71172 = CARTESIAN_POINT ( 'NONE',  ( 8.727484440040480962, 175.8458772461660828, 9.188101187500095079 ) ) ;
#71174 = VECTOR ( 'NONE', #18283, 1000.000000000000000 ) ;
#71175 = CARTESIAN_POINT ( 'NONE',  ( 161.5504728662519369, 250.8333683393111926, 12.94300825113363373 ) ) ;
#71176 = ORIENTED_EDGE ( 'NONE', *, *, #42942, .T. ) ;
#71177 = VERTEX_POINT ( 'NONE', #39658 ) ;
#71178 = CARTESIAN_POINT ( 'NONE',  ( 197.5198955408084487, 265.2020030822665717, -2.944437631376198183 ) ) ;
#71179 = VECTOR ( 'NONE', #32420, 1000.000000000000000 ) ;
#71180 = CARTESIAN_POINT ( 'NONE',  ( 69.06100142215747439, 70.44252798373366886, 1.237476299740512431 ) ) ;
#71181 = CARTESIAN_POINT ( 'NONE',  ( 83.26693017028203769, 42.57865931657983083, 5.729871548751052757 ) ) ;
#71182 = CARTESIAN_POINT ( 'NONE',  ( -19.51454890667437425, 93.09519646595313702, 59.99999999999999289 ) ) ;
#71183 = CARTESIAN_POINT ( 'NONE',  ( 105.5870131927823081, 241.7677522451419065, -5.000000000000047962 ) ) ;
#71184 = CARTESIAN_POINT ( 'NONE',  ( 74.09769653082098273, 68.87686179987508694, -11.21282387169916284 ) ) ;
#71185 = CARTESIAN_POINT ( 'NONE',  ( 37.63108229134613225, 192.5333772461660544, 9.188101187500095079 ) ) ;
#71186 = CARTESIAN_POINT ( 'NONE',  ( 73.90491717100159974, 220.1427522451418781, 10.00000000000009237 ) ) ;
#71187 = CARTESIAN_POINT ( 'NONE',  ( 199.4661499282636044, 277.5283185301939284, 15.18718668142867934 ) ) ;
#71188 = VERTEX_POINT ( 'NONE', #16387 ) ;
#71189 = CARTESIAN_POINT ( 'NONE',  ( 152.1915498382297471, 272.9642279343270275, -11.71006468322317140 ) ) ;
#71190 = CARTESIAN_POINT ( 'NONE',  ( 175.2874222581449430, 281.1428048220561777, -14.59610539211987401 ) ) ;
#71191 = ADVANCED_FACE ( 'NONE', ( #86349 ), #54715, .F. ) ;
#71192 = CARTESIAN_POINT ( 'NONE',  ( -13.97887943725652882, 171.9244531367911293, -4.594050593750046652 ) ) ;
#71193 = CARTESIAN_POINT ( 'NONE',  ( 196.0395593785976018, 291.0965181932902510, 15.97855489120023087 ) ) ;
#71194 = CARTESIAN_POINT ( 'NONE',  ( 68.56886429688491091, 64.21317091390413623, -12.46312428434479358 ) ) ;
#71195 = CARTESIAN_POINT ( 'NONE',  ( 151.2567985338353935, 268.6625352796243646, -15.71756535662528798 ) ) ;
#71196 = CARTESIAN_POINT ( 'NONE',  ( 186.9138942552878575, 282.8138041189644696, 16.19480528300033839 ) ) ;
#71197 = CARTESIAN_POINT ( 'NONE',  ( 194.9385458806846430, 293.0035295114944347, -15.70518692812489192 ) ) ;
#71198 = CARTESIAN_POINT ( 'NONE',  ( 192.6098662181048553, 265.0933516837970956, 7.612540007641825035 ) ) ;
#71199 = CARTESIAN_POINT ( 'NONE',  ( 204.3951397407346064, 276.6242284793436852, 14.79595971842109137 ) ) ;
#71200 = CARTESIAN_POINT ( 'NONE',  ( 76.37669801451765750, 208.2365022471902023, 10.00000000000009948 ) ) ;
#71201 = CARTESIAN_POINT ( 'NONE',  ( 190.5154909595809727, 300.6644853595138329, -0.04129855346138300298 ) ) ;
#71202 = ORIENTED_EDGE ( 'NONE', *, *, #51635, .T. ) ;
#71203 =( BOUNDED_CURVE ( )  B_SPLINE_CURVE ( 2, ( #14577, #46441, #29768, #99182, #83012, #61653, #60641, #91597, #75389 ),
 .UNSPECIFIED., .F., .T. ) 
 B_SPLINE_CURVE_WITH_KNOTS ( ( 3, 2, 2, 2, 3 ),
 ( 0.3346774193548386900, 0.3360215053763440651, 0.3387096774193548154, 0.3413978494623655657, 0.3427419354838709964 ),
 .UNSPECIFIED. ) 
 CURVE ( )  GEOMETRIC_REPRESENTATION_ITEM ( )  RATIONAL_B_SPLINE_CURVE ( ( 0.9330127018922194093, 0.9330127018922194093, 1.000000000000000000, 0.8660254037844387076, 1.000000000000000000, 0.8660254037844387076, 1.000000000000000000, 0.9330127018922179660, 0.9330127018922194093 ) ) 
 REPRESENTATION_ITEM ( '' )  );
#71204 = CARTESIAN_POINT ( 'NONE',  ( 12.21864935082045456, 177.8615022471902591, -10.00000000000009592 ) ) ;
#71205 = CARTESIAN_POINT ( 'NONE',  ( 100.3364738622893810, 237.9244531367911009, -4.594050593750046652 ) ) ;
#71206 = CARTESIAN_POINT ( 'NONE',  ( 14.92192532440567199, 20.56628583063839955, 9.188101187500006262 ) ) ;
#71207 = CARTESIAN_POINT ( 'NONE',  ( 71.21816854543845920, 61.31929265152032826, -14.99493774206449359 ) ) ;
#71208 = VECTOR ( 'NONE', #25527, 1000.000000000000000 ) ;
#71209 = CARTESIAN_POINT ( 'NONE',  ( 71.98264401366868981, 72.39816763649429276, -2.869464145551836598 ) ) ;
#71211 = CARTESIAN_POINT ( 'NONE',  ( 150.0916500121360286, 245.9155109091895781, 2.679491924311254714 ) ) ;
#71210 = CARTESIAN_POINT ( 'NONE',  ( 9.242171499132833645, 29.30720582267293750, 10.00000000000000000 ) ) ;
#71212 = CARTESIAN_POINT ( 'NONE',  ( 204.5701216393242987, 272.9108463828269464, -9.751758126869200183 ) ) ;
#71213 = CARTESIAN_POINT ( 'NONE',  ( 21.04067422097218909, 35.08080186712593473, -3.090169943749475845 ) ) ;
#71214 = CARTESIAN_POINT ( 'NONE',  ( 196.9319848161575806, 289.5507919934690335, -17.64330560362266453 ) ) ;
#71215 = CARTESIAN_POINT ( 'NONE',  ( 82.00597693497557827, 40.98120758155860699, -2.954347521771857554 ) ) ;
#71216 = CARTESIAN_POINT ( 'NONE',  ( 173.0532909196153071, 289.8873365335254562, -1.653350512543673378 ) ) ;
#71217 = CARTESIAN_POINT ( 'NONE',  ( 93.96857342517719758, 0.000000000000000000, 0.000000000000000000 ) ) ;
#71218 = ORIENTED_EDGE ( 'NONE', *, *, #34950, .T. ) ;
#71219 = CARTESIAN_POINT ( 'NONE',  ( 131.1144086761837571, 258.0530062829863027, -4.648177544792955347E-16 ) ) ;
#71220 = CARTESIAN_POINT ( 'NONE',  ( 200.5914588262792222, 282.7033700937254821, -16.73555027083989444 ) ) ;
#71221 = CARTESIAN_POINT ( 'NONE',  ( 156.1857201963304362, 277.6936791020598889, 10.39727624116721749 ) ) ;
#71222 = ORIENTED_EDGE ( 'NONE', *, *, #28134, .F. ) ;
#71223 = CARTESIAN_POINT ( 'NONE',  ( 78.87602572105338083, 48.98972573457342605, 14.36228915801518369 ) ) ;
#71224 = CARTESIAN_POINT ( 'NONE',  ( 83.87863349871378205, 51.97949305273395737, -14.54186584096833279 ) ) ;
#71225 = CARTESIAN_POINT ( 'NONE',  ( -19.65312891409030271, 93.06504152958497400, -10.00000000000000888 ) ) ;
#71227 = CARTESIAN_POINT ( 'NONE',  ( 74.91412036032340893, 53.21648545400848462, -16.51781489608933384 ) ) ;
#71226 = VECTOR ( 'NONE', #57436, 1000.000000000000000 ) ;
#71228 = CARTESIAN_POINT ( 'NONE',  ( 153.3100492430090753, 265.1062007306585997, 16.32434963471121492 ) ) ;
#71229 = VERTEX_POINT ( 'NONE', #99828 ) ;
#71230 = DIRECTION ( 'NONE',  ( -0.6363689690731114679, -0.7713848165480219343, 0.000000000000000000 ) ) ;
#71231 = B_SPLINE_SURFACE_WITH_KNOTS ( 'NONE', 3, 1, ( 
 ( #12020, #87082 ),
 ( #89085, #27220 ),
 ( #19634, #49504 ),
 ( #3912, #80459 ),
 ( #79458, #65209 ),
 ( #96150, #57594 ),
 ( #4403, #50494 ),
 ( #34793, #10023 ),
 ( #88575, #19137 ),
 ( #65696, #73809 ),
 ( #41396, #50010 ),
 ( #40885, #96650 ),
 ( #35300, #94649 ),
 ( #25204, #18117 ),
 ( #2432, #79953 ),
 ( #33308, #95160 ),
 ( #10520, #68185 ),
 ( #59579, #89559 ),
 ( #51497, #74334 ),
 ( #13518, #74830 ),
 ( #98629, #35801 ),
 ( #21608, #43891 ),
 ( #21125, #36293 ),
 ( #20616, #52488 ),
 ( #29209, #5410 ),
 ( #67194, #59072 ),
 ( #66695, #5899 ),
 ( #98117, #4922 ),
 ( #99115, #22093 ),
 ( #82945, #45386 ),
 ( #97631, #36790 ),
 ( #90043, #28196 ),
 ( #28703, #67701 ),
 ( #83436, #60078 ) ),
 .UNSPECIFIED., .T., .F., .F.,
 ( 4, 2, 2, 2, 2, 2, 2, 2, 2, 2, 2, 2, 2, 2, 2, 2, 4 ),
 ( 2, 2 ),
 ( 0.000000000000000000, 0.06250000000000000000, 0.1250000000000000000, 0.1875000000000000000, 0.2500000000000000000, 0.3125000000000000000, 0.3750000000000000000, 0.4375000000000000000, 0.5000000000000000000, 0.5625000000000000000, 0.6250000000000000000, 0.6875000000000000000, 0.7500000000000000000, 0.8125000000000000000, 0.8750000000000000000, 0.9375000000000000000, 1.000000000000000000 ),
 ( 0.000000000000000000, 1.000000000000000000 ),
 .UNSPECIFIED. ) ;
#71232 = CARTESIAN_POINT ( 'NONE',  ( 35.45274159363147959, 38.65586893147759184, -7.433330006724137462 ) ) ;
#71233 = CARTESIAN_POINT ( 'NONE',  ( 195.1200766625154017, 290.1138218968723663, -16.44780575384534771 ) ) ;
#71234 = ORIENTED_EDGE ( 'NONE', *, *, #77063, .T. ) ;
#71235 = CARTESIAN_POINT ( 'NONE',  ( 163.9638979413247171, 279.3640461705110738, 12.10115734641663821 ) ) ;
#71236 = DIRECTION ( 'NONE',  ( 0.5864613938488598688, -0.8099771808667527440, 0.000000000000000000 ) ) ;
#71237 = CARTESIAN_POINT ( 'NONE',  ( 196.5144060520763105, 263.7350746926370562, -1.323704968039587815 ) ) ;
#71238 = ORIENTED_EDGE ( 'NONE', *, *, #476, .T. ) ;
#71239 = CARTESIAN_POINT ( 'NONE',  ( 79.39869110645544481, 59.73379174629956623, 16.16845418028724524 ) ) ;
#71240 = CARTESIAN_POINT ( 'NONE',  ( 188.7230124823968254, 293.4391532799720608, 12.65699786571403784 ) ) ;
#71241 = CARTESIAN_POINT ( 'NONE',  ( 204.3951397407346064, 276.6242284793436852, 14.79595971842109137 ) ) ;
#71242 = CARTESIAN_POINT ( 'NONE',  ( 24.56267145112387240, 22.38052372038641735, 10.00000000000000533 ) ) ;
#71243 = CARTESIAN_POINT ( 'NONE',  ( 155.3513572141771704, 261.5705516107003064, -17.00592413546589299 ) ) ;
#71244 = ORIENTED_EDGE ( 'NONE', *, *, #24790, .F. ) ;
#71245 = B_SPLINE_CURVE_WITH_KNOTS ( 'NONE', 3,
 ( #46653, #30955, #68952, #77580, #69948, #67968, #98889, #29468, #60343, #37548, #31448, #68454, #62340, #13767, #99383, #93806, #70457, #47150, #8660, #1068, #64361, #9166, #94797, #87738 ),
 .UNSPECIFIED., .F., .F.,
 ( 4, 2, 2, 2, 2, 2, 2, 2, 2, 2, 2, 4 ),
 ( 0.000000000000000000, 0.1250000000000041633, 0.2500000000000083267, 0.3750000000000124900, 0.4375000000000112133, 0.5000000000000099920, 0.5625000000000087708, 0.6250000000000074385, 0.6875000000000062172, 0.7500000000000049960, 0.8750000000000024425, 1.000000000000000000 ),
 .UNSPECIFIED. ) ;
#71246 = ORIENTED_EDGE ( 'NONE', *, *, #66944, .T. ) ;
#71247 = CARTESIAN_POINT ( 'NONE',  ( 103.4941184669699794, 223.8927522451417929, 10.00000000000009948 ) ) ;
#71248 = ORIENTED_EDGE ( 'NONE', *, *, #62730, .F. ) ;
#71249 = CARTESIAN_POINT ( 'NONE',  ( 77.20279821355711647, 49.64797377247255383, -14.99054536557791906 ) ) ;
#71250 = ORIENTED_EDGE ( 'NONE', *, *, #6598, .T. ) ;
#71251 = EDGE_CURVE ( 'NONE', #21258, #88994, #60012, .T. ) ;
#71252 = CARTESIAN_POINT ( 'NONE',  ( 173.1761264927225454, 270.8446349882100321, 16.51755988034715017 ) ) ;
#71253 = DIRECTION ( 'NONE',  ( 0.5102188382608533468, -0.8600446134263879383, 0.000000000000000000 ) ) ;
#71254 = VERTEX_POINT ( 'NONE', #54188 ) ;
#71255 = CARTESIAN_POINT ( 'NONE',  ( 186.0894263339278609, 282.3892669566888571, -16.72715339669124290 ) ) ;
#71256 = CARTESIAN_POINT ( 'NONE',  ( 190.7042836556221062, 300.3374868178723887, 2.564074060554762280 ) ) ;
#71257 = DIRECTION ( 'NONE',  ( -1.000000000000000000, 0.000000000000000000, 0.000000000000000000 ) ) ;
#71258 = CARTESIAN_POINT ( 'NONE',  ( 82.78178186318515941, 40.60033419795881571, 0.9506087024331607571 ) ) ;
#71259 = CARTESIAN_POINT ( 'NONE',  ( 201.4214977800931763, 281.7747274386935601, -17.04225209925078133 ) ) ;
#71260 = EDGE_CURVE ( 'NONE', #76155, #35311, #77530, .T. ) ;
#71261 = DIRECTION ( 'NONE',  ( -0.000000000000000000, 0.000000000000000000, 1.000000000000000000 ) ) ;
#71262 = CARTESIAN_POINT ( 'NONE',  ( -89.11465314115665137, 93.37593066204027537, -37.49999999999999289 ) ) ;
#71263 = CARTESIAN_POINT ( 'NONE',  ( 127.1021582719434662, 250.3149278399161233, -9.188101187500095079 ) ) ;
#71264 = VERTEX_POINT ( 'NONE', #46092 ) ;
#71265 = CARTESIAN_POINT ( 'NONE',  ( 186.8567874311567039, 262.4816910035492015, -10.18088338104968393 ) ) ;
#71266 = CARTESIAN_POINT ( 'NONE',  ( 46.16617079539854984, 27.44966523072498177, -2.296566073217252530E-15 ) ) ;
#71267 = VERTEX_POINT ( 'NONE', #25 ) ;
#71269 = ORIENTED_EDGE ( 'NONE', *, *, #92088, .T. ) ;
#71268 = CARTESIAN_POINT ( 'NONE',  ( 86.32427409670840746, 43.64500876675992203, -5.374088149502346923 ) ) ;
#71270 = B_SPLINE_CURVE_WITH_KNOTS ( 'NONE', 3,
 ( #98336, #7106, #60782, #66912, #75041, #90773, #83152, #82677, #59290, #36009, #28930, #5617, #90269, #45108, #13720, #37987, #91748, #76043, #21323, #61301, #29420, #60289, #20843, #21812, #52698, #13242, #75529, #68899, #99826, #6623, #30410, #59804, #83659, #84648, #67919, #37498, #6114, #68404, #37009, #84165, #22309, #91249, #46089, #99332, #53212, #14711 ),
 .UNSPECIFIED., .F., .F.,
 ( 4, 2, 2, 2, 2, 2, 2, 2, 2, 2, 2, 2, 2, 2, 2, 2, 2, 2, 2, 2, 2, 2, 4 ),
 ( 0.001500548513609991329, 0.001965505369317757569, 0.002430462225025523809, 0.002662940652879392835, 0.002779179866806390665, 0.002895419080733388061, 0.003011658294660385024, 0.003127897508587382854, 0.003360375936441254915, 0.003825332792148934419, 0.004290289647856613056, 0.005220203359271819409, 0.006150117070687024894, 0.006615073926394628503, 0.007080030782102231246, 0.007196269996029148845, 0.007254389602992554302, 0.007312509209955960626, 0.007544987637809759395, 0.008009944493517464487, 0.008474901349225167843, 0.008707379777079013450, 0.008939858204932860791 ),
 .UNSPECIFIED. ) ;
#71271 = CARTESIAN_POINT ( 'NONE',  ( 203.5349748457618944, 276.1682765948387441, 13.32875452130744875 ) ) ;
#71272 = CARTESIAN_POINT ( 'NONE',  ( 181.2270729396664706, 255.5114031541049826, 0.5804978543035055338 ) ) ;
#71273 = CARTESIAN_POINT ( 'NONE',  ( 172.3006544489366263, 288.5207632028400440, -4.638716040452800726 ) ) ;
#71274 = CARTESIAN_POINT ( 'NONE',  ( 192.0554304829709906, 297.9972318644188931, 11.99356102654441614 ) ) ;
#71275 = CARTESIAN_POINT ( 'NONE',  ( 72.06635965893990203, 61.93972394716566043, 14.43705991168542546 ) ) ;
#71276 = CARTESIAN_POINT ( 'NONE',  ( 201.0356089830534643, 282.4431064412383989, -18.18835788025466371 ) ) ;
#71277 = CARTESIAN_POINT ( 'NONE',  ( 173.3498119174590215, 287.3205656585489578, -9.768182251902993940 ) ) ;
#71278 = CARTESIAN_POINT ( 'NONE',  ( 153.5053096856745469, 266.9305189219332419, 16.59624669306388967 ) ) ;
#71279 = LINE ( 'NONE', #9470, #90206 ) ;
#71280 = ORIENTED_EDGE ( 'NONE', *, *, #54719, .T. ) ;
#71281 = CARTESIAN_POINT ( 'NONE',  ( 194.6943296385021824, 293.4265244509877562, -16.10917128197217352 ) ) ;
#71282 = CARTESIAN_POINT ( 'NONE',  ( 164.8489450237687493, 247.1202469751449939, -7.123750760659631531 ) ) ;
#71283 = VERTEX_POINT ( 'NONE', #30911 ) ;
#71284 = DIRECTION ( 'NONE',  ( -0.2938926261462390666, 0.5090369604551334692, 0.8090169943749425663 ) ) ;
#71285 = CARTESIAN_POINT ( 'NONE',  ( 190.9541724464728247, 283.5919873151655679, -16.59114474495747515 ) ) ;
#71286 = CARTESIAN_POINT ( 'NONE',  ( 191.7730772792068308, 298.4862819590180720, -10.97593358402262886 ) ) ;
#71287 = CARTESIAN_POINT ( 'NONE',  ( 190.0896302098338424, 301.4020978150248311, 3.433521196325825642 ) ) ;
#71288 = CARTESIAN_POINT ( 'NONE',  ( 162.7644741734472120, 248.7306563947940958, 9.865755277559742353 ) ) ;
#71290 = CARTESIAN_POINT ( 'NONE',  ( 154.5359630391655514, 276.9837356694303594, -8.741008087266880722 ) ) ;
#71289 = CARTESIAN_POINT ( 'NONE',  ( 153.3780955418828285, 270.1760744682334803, 14.08076314294041964 ) ) ;
#71291 = CARTESIAN_POINT ( 'NONE',  ( 199.9376085384402586, 267.5739236585927188, 6.187416678158419003 ) ) ;
#71292 = EDGE_LOOP ( 'NONE', ( #60841, #60893, #89619, #58473 ) ) ;
#71293 = PRODUCT_DEFINITION ( 'UNKNOWN', '', #60733, #17975 ) ;
#71294 = CARTESIAN_POINT ( 'NONE',  ( 164.0405138800869054, 280.4465961471673836, -11.50895991882478242 ) ) ;
#71295 = CARTESIAN_POINT ( 'NONE',  ( 193.7609008727193043, 262.8443104439116951, 4.759103018491034121 ) ) ;
#71296 = CYLINDRICAL_SURFACE ( 'NONE', #18321, 70.00000000000002842 ) ;
#71297 = CARTESIAN_POINT ( 'NONE',  ( 32.84087927488953085, 179.7677522451417929, -5.000000000000041744 ) ) ;
#71298 = CARTESIAN_POINT ( 'NONE',  ( 165.7068383116082657, 276.7076515144831887, 15.46715011107357718 ) ) ;
#71299 = CARTESIAN_POINT ( 'NONE',  ( 190.0534303668326288, 269.9073674132432643, 15.26070177760127322 ) ) ;
#71300 = CARTESIAN_POINT ( 'NONE',  ( 50.37091257173480585, 98.81520120758277415, -10.00000000000000000 ) ) ;
#71301 = VECTOR ( 'NONE', #20082, 1000.000000000000114 ) ;
#71302 = CARTESIAN_POINT ( 'NONE',  ( 74.28280957949721142, 68.55643958410426819, 11.10420501780135893 ) ) ;
#71303 = DIRECTION ( 'NONE',  ( -0.8660254037844387076, -0.4999999999999998890, -0.000000000000000000 ) ) ;
#71304 = CARTESIAN_POINT ( 'NONE',  ( 1.528821818964843482, 165.5643266524160140, 9.188101187500095079 ) ) ;
#71305 = CARTESIAN_POINT ( 'NONE',  ( 88.50972766791686297, 234.1589784336661637, -6.496448406907675876E-16 ) ) ;
#71306 = CARTESIAN_POINT ( 'NONE',  ( 155.6281496932864457, 261.0911329737299980, -18.07904265579665548 ) ) ;
#71307 = LINE ( 'NONE', #55565, #70975 ) ;
#71308 = CARTESIAN_POINT ( 'NONE',  ( 49.07419501245632176, 91.40403951869188859, -10.00000000000000000 ) ) ;
#71309 = FACE_BOUND ( 'NONE', #8199, .T. ) ;
#71310 = ADVANCED_FACE ( 'NONE', ( #8123 ), #93758, .F. ) ;
#71311 = CARTESIAN_POINT ( 'NONE',  ( 77.59148524364135824, 52.59450808426719703, 15.75520512475421953 ) ) ;
#71312 = CARTESIAN_POINT ( 'NONE',  ( -112.5954152546897262, 74.04580364311806306, 21.50000000000000000 ) ) ;
#71314 = CYLINDRICAL_SURFACE ( 'NONE', #93314, 49.99999999999999289 ) ;
#71313 = DIRECTION ( 'NONE',  ( 0.4999999999999992784, -0.8660254037844390407, 0.000000000000000000 ) ) ;
#71315 = CARTESIAN_POINT ( 'NONE',  ( 178.6117656011147972, 290.0031260663362787, 9.480844723140000596 ) ) ;
#71316 = CARTESIAN_POINT ( 'NONE',  ( 195.3341046825671583, 268.5239226548773104, 12.14968905865328175 ) ) ;
#71317 = CARTESIAN_POINT ( 'NONE',  ( 205.5585585089849303, 274.6091280622553086, -13.37199793655179825 ) ) ;
#71318 = DIRECTION ( 'NONE',  ( -0.000000000000000000, -0.000000000000000000, -1.000000000000000000 ) ) ;
#71319 = DIRECTION ( 'NONE',  ( 0.4999999999999998890, -0.8660254037844385966, 0.000000000000000000 ) ) ;
#71320 = EDGE_CURVE ( 'NONE', #93866, #179, #37991, .T. ) ;
#71321 = CARTESIAN_POINT ( 'NONE',  ( 161.3773209892555371, 251.1332761876949746, -14.50043705923759241 ) ) ;
#71322 = CARTESIAN_POINT ( 'NONE',  ( 37.63108229134613225, 192.5333772461660544, 9.188101187500095079 ) ) ;
#71323 = CARTESIAN_POINT ( 'NONE',  ( 76.86303881961467255, 63.31387137873053916, -15.46595148530503927 ) ) ;
#71324 = EDGE_CURVE ( 'NONE', #83705, #99407, #808, .T. ) ;
#71325 = CARTESIAN_POINT ( 'NONE',  ( 73.21957404993666785, 203.8923013555409796, 4.594050593750050204 ) ) ;
#71326 = CARTESIAN_POINT ( 'NONE',  ( 57.68498304950345812, 214.1115022471903444, -5.000000000000047962 ) ) ;
#71327 = CARTESIAN_POINT ( 'NONE',  ( 88.30697365647166919, 43.76017805630483792, 0.1929712240254208011 ) ) ;
#71328 = CARTESIAN_POINT ( 'NONE',  ( 13.83268420227240014, 8.390406791769812855, -2.889640176918245968E-15 ) ) ;
#71329 = CARTESIAN_POINT ( 'NONE',  ( 85.48636484970303684, 43.17023849599863183, -5.434256565237638448 ) ) ;
#71330 = CARTESIAN_POINT ( 'NONE',  ( 176.6243488689623007, 270.1410765278557164, -16.80516242629813561 ) ) ;
#71331 = CARTESIAN_POINT ( 'NONE',  ( 31.65185205300530313, 23.98920272979928114, 7.433330006724137462 ) ) ;
#71332 = DIRECTION ( 'NONE',  ( 1.000000000000000000, 0.000000000000000000, 0.000000000000000000 ) ) ;
#71333 = CARTESIAN_POINT ( 'NONE',  ( 196.4170778717353585, 290.4426369823788718, -17.78762421190030452 ) ) ;
#71334 = VERTEX_POINT ( 'NONE', #87188 ) ;
#71335 = CARTESIAN_POINT ( 'NONE',  ( 12.13982549814181411, 27.98502408145591502, -5.678558825948271327 ) ) ;
#71336 = CARTESIAN_POINT ( 'NONE',  ( 65.53359859134977228, 199.4548013555410080, -4.594050593750042211 ) ) ;
#71337 = CARTESIAN_POINT ( 'NONE',  ( 28.50765780192512366, 60.84557485627980356, 59.99999999999999289 ) ) ;
#71338 = CARTESIAN_POINT ( 'NONE',  ( 154.9067123643522734, 262.3406990819208886, -18.18534662427576265 ) ) ;
#71339 = CARTESIAN_POINT ( 'NONE',  ( 172.9649338451820029, 290.0245193479112800, -0.4253077601802810470 ) ) ;
#71340 = CARTESIAN_POINT ( 'NONE',  ( -16.99542894172669349, 24.36904009834038476, -10.00000000000000000 ) ) ;
#71341 = CARTESIAN_POINT ( 'NONE',  ( 154.0022440109411832, 263.9072842238671228, 16.76240413822421971 ) ) ;
#71342 = CARTESIAN_POINT ( 'NONE',  ( 189.9590362446921858, 286.5603738525368840, 16.42061212002715465 ) ) ;
#71343 = CARTESIAN_POINT ( 'NONE',  ( 125.2349645446897171, 243.1115022471902591, 10.00000000000009592 ) ) ;
#71344 = CARTESIAN_POINT ( 'NONE',  ( 200.9110265982630779, 282.6588894614233141, 17.52479721249226685 ) ) ;
#71345 = CARTESIAN_POINT ( 'NONE',  ( 207.5686001603237116, 271.1276337968068333, 7.659944433763431704 ) ) ;
#71346 = EDGE_LOOP ( 'NONE', ( #99181, #93258, #99650, #51337 ) ) ;
#71347 = CARTESIAN_POINT ( 'NONE',  ( 149.2522690271913746, 273.6402648190738205, -10.03091955270726032 ) ) ;
#71348 = CARTESIAN_POINT ( 'NONE',  ( 82.10840107674059141, 54.12326372724951540, 15.62324998714231050 ) ) ;
#71349 = VERTEX_POINT ( 'NONE', #89656 ) ;
#71350 = CARTESIAN_POINT ( 'NONE',  ( 206.8317058779879574, 272.4039721336197317, -10.41591514895975834 ) ) ;
#71351 = CARTESIAN_POINT ( 'NONE',  ( 207.3988330342936877, 270.8564699888902396, -1.301389719878858875 ) ) ;
#71352 = CARTESIAN_POINT ( 'NONE',  ( 69.48308982531537481, 68.85812419773016302, -7.057691085508246864 ) ) ;
#71353 = VERTEX_POINT ( 'NONE', #82051 ) ;
#71354 = CARTESIAN_POINT ( 'NONE',  ( 176.8434924416465321, 253.2981294648533606, -0.2582399125330065992 ) ) ;
#71355 = ORIENTED_EDGE ( 'NONE', *, *, #55958, .T. ) ;
#71356 = CARTESIAN_POINT ( 'NONE',  ( 65.81996430066485004, 68.94383839650693346, -2.301213135912207886 ) ) ;
#71357 = CARTESIAN_POINT ( 'NONE',  ( 147.8819534105757043, 274.5079385007862811, -9.338341377131436971 ) ) ;
#71358 = CARTESIAN_POINT ( 'NONE',  ( 148.8636819117637629, 274.0699646975406836, 8.926834414297511344 ) ) ;
#71359 = EDGE_LOOP ( 'NONE', ( #14636, #7682, #9740, #48663 ) ) ;
#71360 = CARTESIAN_POINT ( 'NONE',  ( 26.56877070717806433, 23.84335787977763843, 9.188101187500006262 ) ) ;
#71361 = CARTESIAN_POINT ( 'NONE',  ( 79.97118972361107581, 44.44405107747005701, 11.63932608780695510 ) ) ;
#71362 = CARTESIAN_POINT ( 'NONE',  ( 84.64469814230420752, 50.57817590239302064, -14.03985074783417630 ) ) ;
#71363 = CARTESIAN_POINT ( 'NONE',  ( -27.42236680055714260, 166.5217562850347406, 1.224646799147364892E-15 ) ) ;
#71364 = EDGE_CURVE ( 'NONE', #46853, #29881, #43981, .T. ) ;
#71365 = ADVANCED_FACE ( 'NONE', ( #81544 ), #8638, .T. ) ;
#71366 = ORIENTED_EDGE ( 'NONE', *, *, #96297, .T. ) ;
#71367 = FACE_OUTER_BOUND ( 'NONE', #49918, .T. ) ;
#71368 = CARTESIAN_POINT ( 'NONE',  ( 175.0809028706871118, 261.2525943152746208, 15.25527675994286092 ) ) ;
#71369 = ORIENTED_EDGE ( 'NONE', *, *, #49202, .T. ) ;
#71370 = VECTOR ( 'NONE', #14771, 1000.000000000000000 ) ;
#71371 = ORIENTED_EDGE ( 'NONE', *, *, #54076, .F. ) ;
#71372 = CARTESIAN_POINT ( 'NONE',  ( 183.6038495250667211, 296.0503002337411544, 1.014586387891125652 ) ) ;
#71374 = CARTESIAN_POINT ( 'NONE',  ( 148.3629184514745987, 273.6748826132846375, -8.219814532462343948 ) ) ;
#71373 = CARTESIAN_POINT ( 'NONE',  ( 67.84078594043214139, 65.66857331658644625, 10.81805557313897737 ) ) ;
#71375 = CARTESIAN_POINT ( 'NONE',  ( 208.3764315856425640, 269.7284287242038658, -1.833640725398759441 ) ) ;
#71376 = CARTESIAN_POINT ( 'NONE',  ( 193.8603219414924013, 294.8710681561126989, 15.36476279452078586 ) ) ;
#71377 = CARTESIAN_POINT ( 'NONE',  ( 40.97195624589149077, 25.78380873178789656, -6.180339887498949025 ) ) ;
#71378 = CARTESIAN_POINT ( 'NONE',  ( 157.4805323096970255, 257.8827121670497036, -16.70238855805511591 ) ) ;
#71379 = CARTESIAN_POINT ( 'NONE',  ( 164.7279764954933512, 245.3297706122307034, 5.346914787972785632 ) ) ;
#71380 = EDGE_CURVE ( 'NONE', #47254, #28615, #51601, .T. ) ;
#71381 = CARTESIAN_POINT ( 'NONE',  ( 75.48556727315214232, 61.63299524387726080, -15.75020862335680150 ) ) ;
#71382 = DIRECTION ( 'NONE',  ( -0.1889875038809470109, -0.9819794923402672682, 0.000000000000000000 ) ) ;
#71383 = CARTESIAN_POINT ( 'NONE',  ( 81.47361835793333285, 217.8458772461660544, 9.188101187500095079 ) ) ;
#71384 = EDGE_LOOP ( 'NONE', ( #43623, #54247, #24789, #18906 ) ) ;
#71385 = CARTESIAN_POINT ( 'NONE',  ( 150.6453220160077251, 269.7216436761371483, 14.94145576020818034 ) ) ;
#71386 = DIRECTION ( 'NONE',  ( -0.9042435392811277728, -0.4270171210482544000, 0.000000000000000000 ) ) ;
#71387 = CARTESIAN_POINT ( 'NONE',  ( 78.11917150362724271, 61.95746172053952705, -16.05486485196055568 ) ) ;
#71388 = ORIENTED_EDGE ( 'NONE', *, *, #58430, .T. ) ;
#71389 = CARTESIAN_POINT ( 'NONE',  ( 157.4450252842904092, 257.9442121390794682, -17.98854725065957183 ) ) ;
#71390 = ORIENTED_EDGE ( 'NONE', *, *, #23850, .F. ) ;
#71391 = CARTESIAN_POINT ( 'NONE',  ( 80.06816492365965132, 44.55418465396458316, -11.68679231591616308 ) ) ;
#71392 = CARTESIAN_POINT ( 'NONE',  ( -19.65312891409030271, 93.06504152958497400, 177.5919119679930134 ) ) ;
#71393 = DIRECTION ( 'NONE',  ( -0.4999999999999997224, 0.8660254037844387076, 0.000000000000000000 ) ) ;
#71394 = CARTESIAN_POINT ( 'NONE',  ( 164.1883108770558692, 249.9675975386064692, 10.18338785008276481 ) ) ;
#71395 = CARTESIAN_POINT ( 'NONE',  ( 81.91428016588723438, 47.98820967271630877, -12.92198026695155910 ) ) ;
#71396 = CARTESIAN_POINT ( 'NONE',  ( 207.7679535393632477, 270.7823436156499497, 1.643001479255987274 ) ) ;
#71397 = CARTESIAN_POINT ( 'NONE',  ( 73.73334276372743545, 219.5024278399160664, 9.188101187500095079 ) ) ;
#71398 = ORIENTED_EDGE ( 'NONE', *, *, #89685, .T. ) ;
#71399 = ORIENTED_EDGE ( 'NONE', *, *, #70287, .T. ) ;
#71400 = LINE ( 'NONE', #32875, #52859 ) ;
#71401 = CARTESIAN_POINT ( 'NONE',  ( 161.7973860292566712, 250.4057021959295071, -14.21001024987457484 ) ) ;
#71402 = ORIENTED_EDGE ( 'NONE', *, *, #14495, .T. ) ;
#71403 = CARTESIAN_POINT ( 'NONE',  ( 76.00174837439909936, 64.70029647188280819, -14.33957986251690997 ) ) ;
#71404 = CARTESIAN_POINT ( 'NONE',  ( 68.07113691668065769, 69.08423509312365240, -4.762053786030961966 ) ) ;
#71405 = CARTESIAN_POINT ( 'NONE',  ( 109.9838485029171267, 222.7592609112380160, 2.679491924311254714 ) ) ;
#71406 = CARTESIAN_POINT ( 'NONE',  ( 87.89236927835047197, 44.79168309952778060, 4.915177569529609158 ) ) ;
#71407 = ORIENTED_EDGE ( 'NONE', *, *, #44210, .F. ) ;
#71408 = CARTESIAN_POINT ( 'NONE',  ( 188.7267243920021542, 295.1910411013678299, 11.79826141631466463 ) ) ;
#71409 = CARTESIAN_POINT ( 'NONE',  ( 159.3969902868548161, 275.0432323227933580, 12.88213412656160095 ) ) ;
#71410 = CARTESIAN_POINT ( 'NONE',  ( 159.3237119419271437, 254.6902313965507858, -15.56765445935501191 ) ) ;
#71411 = CARTESIAN_POINT ( 'NONE',  ( 148.1846401255833996, 275.9836697316168284, -5.368268268079755323 ) ) ;
#71412 = CARTESIAN_POINT ( 'NONE',  ( 180.6665526851674599, 287.6815954905284798, 14.11204521094005671 ) ) ;
#71413 = DIRECTION ( 'NONE',  ( -0.8806841296921844586, 0.4737039832092607705, 0.000000000000000000 ) ) ;
#71414 = DIRECTION ( 'NONE',  ( -1.804112415015878984E-15, 1.000000000000000000, -0.000000000000000000 ) ) ;
#71415 = EDGE_LOOP ( 'NONE', ( #82253, #78175, #7693, #58611 ) ) ;
#71416 = CARTESIAN_POINT ( 'NONE',  ( 203.1577047574547805, 277.9875982410399047, -14.81633164762421195 ) ) ;
#71417 = CARTESIAN_POINT ( 'NONE',  ( 200.8551880497955437, 282.7556046643899776, 18.00894873733387058 ) ) ;
#71418 = CARTESIAN_POINT ( 'NONE',  ( 84.22395731584195744, 42.64873031269722503, 4.526430362304276755 ) ) ;
#71419 = CARTESIAN_POINT ( 'NONE',  ( 171.6080846817307872, 251.3649527223411724, 7.288243930487503519 ) ) ;
#71420 = CARTESIAN_POINT ( 'NONE',  ( 83.26710953215496147, 52.37668708275160867, 14.85863008173918942 ) ) ;
#71421 = CARTESIAN_POINT ( 'NONE',  ( 175.0524379492280502, 290.1408238227680272, -6.332636328160596406 ) ) ;
#71422 = CARTESIAN_POINT ( 'NONE',  ( 153.3702792842350107, 270.2708052652295123, 14.01565955641743422 ) ) ;
#71423 = ORIENTED_EDGE ( 'NONE', *, *, #86359, .T. ) ;
#71424 = EDGE_CURVE ( 'NONE', #31631, #82532, #86344, .T. ) ;
#71425 = CARTESIAN_POINT ( 'NONE',  ( 164.4858674010174298, 245.7491158648375347, -2.958464974013825355 ) ) ;
#71427 = FACE_BOUND ( 'NONE', #79606, .T. ) ;
#71426 = CARTESIAN_POINT ( 'NONE',  ( 177.5003341694142307, 264.7901247500786894, -15.18634591033956305 ) ) ;
#71428 = CARTESIAN_POINT ( 'NONE',  ( 176.1768359416886369, 285.1771366315132923, -12.84902834441190755 ) ) ;
#71429 = ADVANCED_FACE ( 'NONE', ( #53583 ), #84537, .T. ) ;
#71430 = CARTESIAN_POINT ( 'NONE',  ( 29.80052344588228408, 32.90829794293883026, 10.00000000000000355 ) ) ;
#71431 = CARTESIAN_POINT ( 'NONE',  ( 78.01406954259199722, 47.82291453140933157, 14.04263472196524098 ) ) ;
#71432 = CARTESIAN_POINT ( 'NONE',  ( 168.7693793741400725, 272.9564462316830600, 15.95584976162842494 ) ) ;
#71433 = CARTESIAN_POINT ( 'NONE',  ( 180.5253698147535317, 273.0125201196690909, 17.27947222482116985 ) ) ;
#71434 = CARTESIAN_POINT ( 'NONE',  ( 36.76746430747500938, 51.63176190406337440, -10.00000000000000000 ) ) ;
#71435 = CARTESIAN_POINT ( 'NONE',  ( 192.2066520969698615, 261.9360867464749276, 3.041693569932921726 ) ) ;
#71436 = VECTOR ( 'NONE', #35847, 1000.000000000000000 ) ;
#71437 = CARTESIAN_POINT ( 'NONE',  ( 195.4436462626574667, 265.1414692012189676, -7.795071168451356058 ) ) ;
#71438 = CARTESIAN_POINT ( 'NONE',  ( 6.724974241671477060, 168.5643266524160424, 9.188101187500095079 ) ) ;
#71439 = CARTESIAN_POINT ( 'NONE',  ( 82.21261018562424283, 47.88076305863328486, 12.73987827041416843 ) ) ;
#71440 = EDGE_LOOP ( 'NONE', ( #64136, #71244, #100257, #82066 ) ) ;
#71441 = ADVANCED_FACE ( 'NONE', ( #25188 ), #9511, .F. ) ;
#71442 = CARTESIAN_POINT ( 'NONE',  ( 175.0454162132552085, 255.3288691254335561, 8.248559459473627342 ) ) ;
#71443 = CARTESIAN_POINT ( 'NONE',  ( 27.87997788293534285, 34.83478043621390441, -8.090169943749479842 ) ) ;
#71444 = CARTESIAN_POINT ( 'NONE',  ( 192.8292865579535658, 291.0864435001786887, 16.05090170841207353 ) ) ;
#71445 = CARTESIAN_POINT ( 'NONE',  ( 82.13419662640586694, 41.24805531849482065, 5.427534581471942232 ) ) ;
#71446 = CARTESIAN_POINT ( 'NONE',  ( 14.70821206310299978, 188.4869531367911293, 4.594050593750046652 ) ) ;
#71447 = CARTESIAN_POINT ( 'NONE',  ( 86.18027666378029039, 49.75620593066999220, -22.49999999999982592 ) ) ;
#71448 = CARTESIAN_POINT ( 'NONE',  ( 35.24645901769773815, 32.30066082961424456, -10.00000000000000533 ) ) ;
#71449 = CARTESIAN_POINT ( 'NONE',  ( 181.7837364184500188, 294.2830797998335584, 6.350600127774545633 ) ) ;
#71450 = CARTESIAN_POINT ( 'NONE',  ( 173.6102056894289660, 272.6920272357795056, -16.35699099929867018 ) ) ;
#71451 = CARTESIAN_POINT ( 'NONE',  ( 197.0456392842824016, 289.3539366801700794, 16.77178551838651188 ) ) ;
#71452 = CARTESIAN_POINT ( 'NONE',  ( 81.44543282719071442, 56.09797068433638145, 16.07152707150316928 ) ) ;
#71453 = CARTESIAN_POINT ( 'NONE',  ( 171.6209549223533770, 276.3359157968284876, 16.92957725593318941 ) ) ;
#71454 = CARTESIAN_POINT ( 'NONE',  ( 186.8199858043552410, 295.8404895034861397, -7.792751730412551758 ) ) ;
#71455 = EDGE_CURVE ( 'NONE', #29993, #15150, #47992, .T. ) ;
#71456 = CARTESIAN_POINT ( 'NONE',  ( 87.56285948006663489, 221.3615022471902591, -10.00000000000009592 ) ) ;
#71457 = EDGE_CURVE ( 'NONE', #38156, #6816, #3421, .T. ) ;
#71458 = CARTESIAN_POINT ( 'NONE',  ( 192.8922210760480311, 295.5150220211069723, -12.92664670631823753 ) ) ;
#71459 = CARTESIAN_POINT ( 'NONE',  ( 70.67536410627012344, 201.6115022471901739, -5.000000000000041744 ) ) ;
#71460 = CARTESIAN_POINT ( 'NONE',  ( 73.79739402942419702, 66.12004107874481917, -12.74733577929619521 ) ) ;
#71461 = CARTESIAN_POINT ( 'NONE',  ( -19.65312891409030271, 93.06504152958497400, 177.5919119679930134 ) ) ;
#71462 = CARTESIAN_POINT ( 'NONE',  ( 203.3512397331466275, 270.1136130142050433, 6.392281993283416952 ) ) ;
#71463 = CARTESIAN_POINT ( 'NONE',  ( 53.65289935712325331, 189.5327760586659451, 1.948934522072303157E-15 ) ) ;
#71464 = CARTESIAN_POINT ( 'NONE',  ( 159.5284711081640125, 254.3355781173132755, 15.34104435652608522 ) ) ;
#71465 = CARTESIAN_POINT ( 'NONE',  ( -5.008551768858394482, 80.94865873146321178, 13.45811050236818396 ) ) ;
#71466 = CARTESIAN_POINT ( 'NONE',  ( 190.8545714895799392, 300.0771806536980648, -5.516553996882049837 ) ) ;
#71467 = CARTESIAN_POINT ( 'NONE',  ( 67.03142477407426725, 66.84972006921925924, -8.889086588726858196 ) ) ;
#71468 = ORIENTED_EDGE ( 'NONE', *, *, #87942, .T. ) ;
#71469 = CARTESIAN_POINT ( 'NONE',  ( 71.94941146435354540, 134.4047874917408478, 22.50000000000001776 ) ) ;
#71470 = CARTESIAN_POINT ( 'NONE',  ( 167.7092726043314315, 282.4287604056521559, -12.24019139390664535 ) ) ;
#71471 = CARTESIAN_POINT ( 'NONE',  ( 193.2853656402591014, 295.8669216819805001, 14.14801835725165091 ) ) ;
#71472 = CARTESIAN_POINT ( 'NONE',  ( 206.1617103877918851, 269.9578652681285575, -1.313740177516645069 ) ) ;
#71473 = CARTESIAN_POINT ( 'NONE',  ( 28.30082151474694641, 24.84335787977763843, 9.188101187500006262 ) ) ;
#71474 = CARTESIAN_POINT ( 'NONE',  ( 162.6774150396764469, 248.8814472377480911, 10.88033986792731689 ) ) ;
#71475 = CARTESIAN_POINT ( 'NONE',  ( 196.9976074755333286, 289.4371302133026802, -16.79549473444794216 ) ) ;
#71476 = CARTESIAN_POINT ( 'NONE',  ( 185.5618649715216861, 267.5775901627870894, -14.75789268656261122 ) ) ;
#71477 = VERTEX_POINT ( 'NONE', #17087 ) ;
#71478 = CARTESIAN_POINT ( 'NONE',  ( 43.87294039959300562, 25.73415679381825427, 1.333680081654574804E-15 ) ) ;
#71479 = CARTESIAN_POINT ( 'NONE',  ( 12.79414888559916719, 13.10170272979925166, -7.433330006724141015 ) ) ;
#71480 = CARTESIAN_POINT ( 'NONE',  ( 74.29045190397653187, 59.50555543665407043, -15.65878564717055177 ) ) ;
#71481 = CARTESIAN_POINT ( 'NONE',  ( 71.90447592081905270, 72.59379857415109427, -1.170934825568553439 ) ) ;
#71482 = EDGE_CURVE ( 'NONE', #89960, #38156, #1906, .T. ) ;
#71483 = ORIENTED_EDGE ( 'NONE', *, *, #32427, .T. ) ;
#71484 = CARTESIAN_POINT ( 'NONE',  ( 72.50273111209941135, 71.24117241184434590, -6.063735550250077821 ) ) ;
#71485 = CARTESIAN_POINT ( 'NONE',  ( 82.18753490691527475, 40.78579184768808830, -0.6546124752527386903 ) ) ;
#71486 = DIRECTION ( 'NONE',  ( -0.000000000000000000, -0.000000000000000000, -1.000000000000000000 ) ) ;
#71487 = CARTESIAN_POINT ( 'NONE',  ( 149.0323968763055689, 272.5153119669064949, 11.64231532207353403 ) ) ;
#71488 = VERTEX_POINT ( 'NONE', #40375 ) ;
#71489 = ORIENTED_EDGE ( 'NONE', *, *, #81177, .F. ) ;
#71490 = ADVANCED_FACE ( 'NONE', ( #72321 ), #41889, .T. ) ;
#71492 = CARTESIAN_POINT ( 'NONE',  ( 161.0515428782683500, 277.3244187559503189, -13.42420650014866368 ) ) ;
#71491 = CARTESIAN_POINT ( 'NONE',  ( 189.7007398628852286, 274.3294530569783660, -15.69864028862395067 ) ) ;
#71493 = VERTEX_POINT ( 'NONE', #95143 ) ;
#71494 = CARTESIAN_POINT ( 'NONE',  ( 201.0356089830534643, 282.4431064412383989, -18.18835788025466371 ) ) ;
#71495 = CARTESIAN_POINT ( 'NONE',  ( 58.29267820409022960, 179.0589433639326558, -17.47570218321535762 ) ) ;
#71496 = CARTESIAN_POINT ( 'NONE',  ( 72.86052486178445520, 57.38405094451463384, -15.86408618498019685 ) ) ;
#71497 = CARTESIAN_POINT ( 'NONE',  ( 76.70982964007059479, 63.62857842591434832, 15.32478313419208149 ) ) ;
#71498 = CARTESIAN_POINT ( 'NONE',  ( 157.8811243250769110, 257.1888664433053009, -17.39256699147873064 ) ) ;
#71499 = ADVANCED_FACE ( 'NONE', ( #11018 ), #34295, .F. ) ;
#71500 = CARTESIAN_POINT ( 'NONE',  ( 104.0442318961827652, 237.0024278399160949, -9.188101187500093303 ) ) ;
#71501 = ADVANCED_FACE ( 'NONE', ( #32787 ), #18609, .T. ) ;
#71502 = CARTESIAN_POINT ( 'NONE',  ( 148.9285945872975390, 272.6951028054104427, -12.01265727652413240 ) ) ;
#71503 = CARTESIAN_POINT ( 'NONE',  ( 180.9558116816610323, 287.1304582847630513, -13.41095839139118695 ) ) ;
#71504 = ORIENTED_EDGE ( 'NONE', *, *, #73449, .F. ) ;
#71505 = CARTESIAN_POINT ( 'NONE',  ( 74.73487060833782891, 53.69418506457893869, 16.08953207461605928 ) ) ;
#71506 = ORIENTED_EDGE ( 'NONE', *, *, #38757, .F. ) ;
#71507 = EDGE_CURVE ( 'NONE', #11479, #63738, #38637, .T. ) ;
#71508 = CARTESIAN_POINT ( 'NONE',  ( 23.32838594064934767, 31.65586893147757408, -7.433330006724137462 ) ) ;
#71509 = LINE ( 'NONE', #63885, #11569 ) ;
#71510 = CARTESIAN_POINT ( 'NONE',  ( 78.35220796506176555, 47.87217679057071251, -14.51592191970564727 ) ) ;
#71511 = CARTESIAN_POINT ( 'NONE',  ( 55.05949644674294774, 214.8464784336662206, 1.353441290958777525E-15 ) ) ;
#71512 = CARTESIAN_POINT ( 'NONE',  ( 74.17419530692131957, 68.61376803465689989, 11.49684454571891479 ) ) ;
#71513 =( BOUNDED_CURVE ( )  B_SPLINE_CURVE ( 1, ( #30985, #22883 ),
 .UNSPECIFIED., .F., .T. ) 
 B_SPLINE_CURVE_WITH_KNOTS ( ( 2, 2 ),
 ( 0.000000000000000000, 0.0009374999959032095671 ),
 .UNSPECIFIED. ) 
 CURVE ( )  GEOMETRIC_REPRESENTATION_ITEM ( )  RATIONAL_B_SPLINE_CURVE ( ( 0.9368410486966849415, 0.9368410486966849415 ) ) 
 REPRESENTATION_ITEM ( '' )  );
#71514 = CARTESIAN_POINT ( 'NONE',  ( 151.3883635558152321, 268.4346579770563608, 15.44343517165679103 ) ) ;
#71515 = CARTESIAN_POINT ( 'NONE',  ( 198.2555168952299027, 287.2583671870688704, 16.98288975666356748 ) ) ;
#71516 = CARTESIAN_POINT ( 'NONE',  ( 172.8453781230440995, 271.4476526176509878, 16.48331706524980333 ) ) ;
#71517 = VERTEX_POINT ( 'NONE', #79442 ) ;
#71518 = CARTESIAN_POINT ( 'NONE',  ( 74.44275639589338311, 58.61260243895608113, -15.83339419040879648 ) ) ;
#71519 = CARTESIAN_POINT ( 'NONE',  ( 85.30525313256302411, 43.13218841966886430, -4.103031163142204285 ) ) ;
#71520 = DIRECTION ( 'NONE',  ( 0.3984034379158949979, -0.9172102815913020235, 0.000000000000000000 ) ) ;
#71521 = CARTESIAN_POINT ( 'NONE',  ( 189.9925954911225290, 301.5701668779311717, 0.1154287172046158938 ) ) ;
#71522 = ORIENTED_EDGE ( 'NONE', *, *, #92720, .F. ) ;
#71523 = CARTESIAN_POINT ( 'NONE',  ( 171.9840958472507566, 258.8842185260619431, -13.78362884886991679 ) ) ;
#71524 = CARTESIAN_POINT ( 'NONE',  ( 69.09727653224064170, 69.59326890348451400, -5.001431338550271555 ) ) ;
#71525 = CARTESIAN_POINT ( 'NONE',  ( 207.8570869662935365, 270.6279599915536664, -5.669188455878507504 ) ) ;
#71526 = DIRECTION ( 'NONE',  ( 0.000000000000000000, 0.000000000000000000, 1.000000000000000000 ) ) ;
#71527 = CARTESIAN_POINT ( 'NONE',  ( 190.5477107455830321, 300.6086790531491033, 3.126266616601216963 ) ) ;
#71528 = CARTESIAN_POINT ( 'NONE',  ( 177.7425752430770274, 269.7382505134228268, 16.10177396393870808 ) ) ;
#71529 = CARTESIAN_POINT ( 'NONE',  ( 188.0757938802393312, 263.1534643581272803, 10.95204294997910033 ) ) ;
#71530 = CARTESIAN_POINT ( 'NONE',  ( 67.66641119600812715, 66.78092416874584103, 8.593359544578680342 ) ) ;
#71531 = CARTESIAN_POINT ( 'NONE',  ( 153.9606011487479122, 264.3624140031040497, -16.52591424867165770 ) ) ;
#71532 = CARTESIAN_POINT ( 'NONE',  ( 174.9193129510662459, 283.1525502601675726, 14.86735122827573718 ) ) ;
#71533 = CARTESIAN_POINT ( 'NONE',  ( 119.3082767336485404, 233.5643266524159856, -9.188101187500093303 ) ) ;
#71534 = EDGE_LOOP ( 'NONE', ( #7520, #93669, #11856, #48182 ) ) ;
#71535 = CARTESIAN_POINT ( 'NONE',  ( 191.8456210280128005, 298.3606325003146367, -9.135603544929113085 ) ) ;
#71536 = DIRECTION ( 'NONE',  ( -0.000000000000000000, -0.000000000000000000, -1.000000000000000000 ) ) ;
#71537 = CARTESIAN_POINT ( 'NONE',  ( 155.6569868912636991, 261.0411854816857158, -17.75433477650897984 ) ) ;
#71538 = CARTESIAN_POINT ( 'NONE',  ( 192.0117586784035097, 296.2629708079742841, 12.42531335008228588 ) ) ;
#71539 = CARTESIAN_POINT ( 'NONE',  ( 83.63875120450398981, 51.47261955259384791, -14.38664681448914884 ) ) ;
#71540 = DIRECTION ( 'NONE',  ( -1.000000000000000000, 0.000000000000000000, 0.000000000000000000 ) ) ;
#71541 = EDGE_LOOP ( 'NONE', ( #18581, #52895, #95635, #16666 ) ) ;
#71542 = CARTESIAN_POINT ( 'NONE',  ( 155.6368094659423207, 263.0761338075079721, 17.69820953191020152 ) ) ;
#71543 = CARTESIAN_POINT ( 'NONE',  ( 158.3005605714957937, 275.4539231493820353, -12.33454573515837893 ) ) ;
#71544 = CARTESIAN_POINT ( 'NONE',  ( 185.6517645066024613, 262.0489465526635513, 9.793930467762132608 ) ) ;
#71545 = CARTESIAN_POINT ( 'NONE',  ( 205.7627300303947209, 272.2554926137148072, 9.584172220806708609 ) ) ;
#71546 = CARTESIAN_POINT ( 'NONE',  ( 130.5662598870812019, 252.3149278399160949, 9.188101187500093303 ) ) ;
#71547 = CARTESIAN_POINT ( 'NONE',  ( 198.7357616895271804, 286.4265588032756114, -17.04018524297827497 ) ) ;
#71548 = CARTESIAN_POINT ( 'NONE',  ( 185.8605417954027530, 296.7763049164376525, 4.522302630076449503 ) ) ;
#71549 = PLANE ( 'NONE',  #41760 ) ;
#71550 = CARTESIAN_POINT ( 'NONE',  ( 67.69866210081085001, 200.7048013555409796, 4.594050593750051981 ) ) ;
#71551 = VECTOR ( 'NONE', #100265, 1000.000000000000000 ) ;
#71552 = CARTESIAN_POINT ( 'NONE',  ( 77.46790047979986582, 60.10606210004741712, -16.34033675906437111 ) ) ;
#71553 = CARTESIAN_POINT ( 'NONE',  ( 157.4805323096970255, 257.8827121670497036, -16.70238855805511591 ) ) ;
#71554 = CARTESIAN_POINT ( 'NONE',  ( 88.00610859356287108, 44.56460208309338356, -4.030656215517964824 ) ) ;
#71555 = B_SPLINE_SURFACE_WITH_KNOTS ( 'NONE', 3, 1, ( 
 ( #65186, #95136 ),
 ( #41374, #1899 ),
 ( #17080, #10001 ),
 ( #24683, #96134 ),
 ( #88549, #32779 ),
 ( #71811, #2407 ),
 ( #57576, #33811 ),
 ( #48996, #94625 ),
 ( #33286, #64695 ),
 ( #88054, #95648 ),
 ( #26195, #79932 ),
 ( #57074, #64187 ),
 ( #40368, #18603 ),
 ( #11011, #19115 ),
 ( #49991, #80946 ),
 ( #87569, #25182 ),
 ( #49482, #18096 ),
 ( #56062, #17590 ),
 ( #11514, #79437 ),
 ( #42368, #63185 ),
 ( #65676, #60056 ),
 ( #89066, #13982 ),
 ( #82444, #97611 ),
 ( #81429, #12000 ),
 ( #74317, #75299 ),
 ( #12501, #44857 ),
 ( #74809, #35282 ),
 ( #59050, #5880 ),
 ( #96630, #43370 ),
 ( #27197, #4899 ),
 ( #28179, #58086 ) ),
 .UNSPECIFIED., .F., .F., .F.,
 ( 4, 3, 3, 3, 3, 3, 3, 3, 3, 3, 4 ),
 ( 2, 2 ),
 ( 0.000000000000000000, 0.1333490885032416196, 0.3007194338854398130, 0.4699862290245220287, 0.5844252810809438259, 0.6686540514502733457, 0.7354980260655562541, 0.8028463152565635808, 0.8633854507757173780, 0.9437142632667323561, 1.000000000000000000 ),
 ( 0.000000000000000000, 1.000000000000000000 ),
 .UNSPECIFIED. ) ;
#71556 = CARTESIAN_POINT ( 'NONE',  ( 71.69160970194380411, 71.06503076016720399, -5.341200118771810779 ) ) ;
#71557 = CARTESIAN_POINT ( 'NONE',  ( 173.8165395728766498, 261.8204000554670188, 14.38043926846092724 ) ) ;
#71558 = CARTESIAN_POINT ( 'NONE',  ( 152.7550266220043511, 278.4983035287039570, -1.611717572787890296 ) ) ;
#71559 = CARTESIAN_POINT ( 'NONE',  ( 180.5721669215874101, 292.9178206186057878, -6.192220326497509753 ) ) ;
#71560 = CARTESIAN_POINT ( 'NONE',  ( 155.5587153255869453, 261.2113968263770971, -18.30500480654006878 ) ) ;
#71561 = CARTESIAN_POINT ( 'NONE',  ( 157.3673062317275537, 270.8922321708535037, -14.72387779267422658 ) ) ;
#71562 = CARTESIAN_POINT ( 'NONE',  ( 128.5366863930700276, 235.0177522451417929, 5.000000000000051514 ) ) ;
#71563 = CARTESIAN_POINT ( 'NONE',  ( 77.82435850266757882, 52.78930163363708061, -15.75762069573296387 ) ) ;
#71564 = EDGE_LOOP ( 'NONE', ( #74884, #92240, #43302, #51811 ) ) ;
#71565 = EDGE_CURVE ( 'NONE', #41961, #20907, #16592, .T. ) ;
#71566 = CARTESIAN_POINT ( 'NONE',  ( 190.3691966041315311, 300.9178746160123410, 0.1783449565851275009 ) ) ;
#71567 = CARTESIAN_POINT ( 'NONE',  ( -13.35616335646270691, 163.0958772461660544, -9.188101187500095079 ) ) ;
#71568 = CARTESIAN_POINT ( 'NONE',  ( 47.67182463829572470, 189.1423013555410080, -4.594050593750043987 ) ) ;
#71569 = CARTESIAN_POINT ( 'NONE',  ( 12.54686387532899516, 29.01751292744055277, 6.180339887498949913 ) ) ;
#71570 = FACE_OUTER_BOUND ( 'NONE', #50779, .T. ) ;
#71571 = CARTESIAN_POINT ( 'NONE',  ( 80.75597752872654667, 49.71520906199375389, -14.73179648239882056 ) ) ;
#71572 = CARTESIAN_POINT ( 'NONE',  ( 72.01517167333473424, 59.31195453282659003, -15.33353692504408272 ) ) ;
#71573 = CARTESIAN_POINT ( 'NONE',  ( 72.25916493420206166, 71.97815949024219151, 3.567716402802650677 ) ) ;
#71575 = CARTESIAN_POINT ( 'NONE',  ( 60.04851071045064970, 192.1427522451417644, 1.119607411625061291E-15 ) ) ;
#71574 = CARTESIAN_POINT ( 'NONE',  ( 198.2717785813136402, 277.4294249212936734, -15.37832795003007114 ) ) ;
#71576 = LINE ( 'NONE', #18370, #61149 ) ;
#71577 = CARTESIAN_POINT ( 'NONE',  ( 183.0365768892434346, 257.4193572625480897, 1.324102024236442965 ) ) ;
#71578 = ADVANCED_FACE ( 'NONE', ( #55079 ), #47487, .F. ) ;
#71579 = CARTESIAN_POINT ( 'NONE',  ( 164.3036517873781008, 252.3706336020835579, 13.60069832213670082 ) ) ;
#71580 = CARTESIAN_POINT ( 'NONE',  ( -13.11024591527734628, 0.000000000000000000, 32.50000000000000000 ) ) ;
#71581 = VERTEX_POINT ( 'NONE', #8993 ) ;
#71582 = EDGE_CURVE ( 'NONE', #38703, #14677, #52843, .T. ) ;
#71583 = CARTESIAN_POINT ( 'NONE',  ( 161.4744130670923994, 267.8122197200463006, 16.81033864343086748 ) ) ;
#71584 = CARTESIAN_POINT ( 'NONE',  ( 31.70422093597033353, 189.1115022471902591, 10.00000000000009592 ) ) ;
#71585 = PLANE ( 'NONE',  #76531 ) ;
#71586 = CARTESIAN_POINT ( 'NONE',  ( 202.3421728196210552, 280.1800714929709670, 16.85915999540957344 ) ) ;
#71587 = CARTESIAN_POINT ( 'NONE',  ( -14.30363896367569509, 171.7369531367911293, -4.594050593750048428 ) ) ;
#71588 = CARTESIAN_POINT ( 'NONE',  ( 35.77750112005064409, 38.84336893147759184, -7.433330006724137462 ) ) ;
#71590 = CARTESIAN_POINT ( 'NONE',  ( 183.1557134058521683, 266.6876041466057927, -15.64491608568827452 ) ) ;
#71589 = DIRECTION ( 'NONE',  ( 0.000000000000000000, 0.000000000000000000, 1.000000000000000000 ) ) ;
#71591 = DIRECTION ( 'NONE',  ( -0.8660254037844377084, -0.5000000000000014433, -0.000000000000000000 ) ) ;
#71592 = CARTESIAN_POINT ( 'NONE',  ( 31.65185205300530313, 23.98920272979928114, 7.433330006724137462 ) ) ;
#71593 = CARTESIAN_POINT ( 'NONE',  ( 205.9240884482826175, 273.9760116357041966, 10.27504561427317142 ) ) ;
#71594 = CARTESIAN_POINT ( 'NONE',  ( 187.0851743399334168, 258.9150848785300809, -2.444460235746602095 ) ) ;
#71595 = CARTESIAN_POINT ( 'NONE',  ( 66.05706222625097723, 68.55736014781324172, 2.107737461089805642 ) ) ;
#71596 = ORIENTED_EDGE ( 'NONE', *, *, #13366, .F. ) ;
#71597 = CARTESIAN_POINT ( 'NONE',  ( 189.8267730604733003, 261.5921186768457574, 7.234476395667181592 ) ) ;
#71598 = CARTESIAN_POINT ( 'NONE',  ( 48.92549481379852949, 97.87922363803308201, -10.00000000000000000 ) ) ;
#71599 = CARTESIAN_POINT ( 'NONE',  ( 10.54248283575963008, 11.80170272979924206, 7.433330006724137462 ) ) ;
#71600 = CARTESIAN_POINT ( 'NONE',  ( 153.2953402526850937, 277.6774005532211049, -5.292706812873809064 ) ) ;
#71601 = CARTESIAN_POINT ( 'NONE',  ( 13.67041502465407277, 29.93396525600389424, 2.839279412974139660 ) ) ;
#71602 = CARTESIAN_POINT ( 'NONE',  ( 207.2815143871675048, 271.6248809420436032, 8.741063757625067154 ) ) ;
#71603 = CARTESIAN_POINT ( 'NONE',  ( 152.8593402092683959, 275.2840601128194749, 10.96293945604634068 ) ) ;
#71604 = CARTESIAN_POINT ( 'NONE',  ( 159.3586121662929713, 254.6297824347537642, -15.50090345830412630 ) ) ;
#71605 = DIRECTION ( 'NONE',  ( 0.000000000000000000, 0.000000000000000000, 1.000000000000000000 ) ) ;
#71606 = ORIENTED_EDGE ( 'NONE', *, *, #65687, .F. ) ;
#71607 = CARTESIAN_POINT ( 'NONE',  ( 23.70688097944214334, 37.18528772668520332, -1.583844403245329602 ) ) ;
#71608 = CARTESIAN_POINT ( 'NONE',  ( 207.0548180518391916, 272.0175305127218053, 7.721676452263806389 ) ) ;
#71609 = B_SPLINE_CURVE_WITH_KNOTS ( 'NONE', 3,
 ( #63700, #79446, #50000, #33296 ),
 .UNSPECIFIED., .F., .F.,
 ( 4, 4 ),
 ( 0.008552533699946726631, 0.01491633745239599393 ),
 .UNSPECIFIED. ) ;
#71610 = CARTESIAN_POINT ( 'NONE',  ( 66.26630907207875509, 68.23277418650276616, 4.087305060687866920 ) ) ;
#71611 = CARTESIAN_POINT ( 'NONE',  ( -65.00000000000000000, 18.66025403784439973, 59.99999999999999289 ) ) ;
#71612 = CARTESIAN_POINT ( 'NONE',  ( -3.153128914090298274, 64.48620320469859735, 0.000000000000000000 ) ) ;
#71613 = ORIENTED_EDGE ( 'NONE', *, *, #14542, .T. ) ;
#71614 = ORIENTED_EDGE ( 'NONE', *, *, #31399, .F. ) ;
#71615 = ADVANCED_FACE ( 'NONE', ( #66194 ), #62824, .F. ) ;
#71616 = CARTESIAN_POINT ( 'NONE',  ( 157.7825643558039417, 277.5034979810923232, -9.893793770821909916 ) ) ;
#71617 = CARTESIAN_POINT ( 'NONE',  ( 86.36983145024699127, 47.62973577336905606, 10.65328243325163804 ) ) ;
#71618 = VERTEX_POINT ( 'NONE', #7368 ) ;
#71619 = CARTESIAN_POINT ( 'NONE',  ( 77.63646380548019010, 56.82889395091936535, 16.18249514420208257 ) ) ;
#71620 = CARTESIAN_POINT ( 'NONE',  ( 189.0276854369573698, 297.1328171424457310, 8.003537747434423366 ) ) ;
#71621 = ORIENTED_EDGE ( 'NONE', *, *, #13600, .T. ) ;
#71622 = CARTESIAN_POINT ( 'NONE',  ( 45.88188149789386472, 72.29567966924399514, -10.00000000000000000 ) ) ;
#71623 = DIRECTION ( 'NONE',  ( -1.000000000000000000, 0.000000000000000000, 0.000000000000000000 ) ) ;
#71624 = EDGE_CURVE ( 'NONE', #37549, #85355, #3370, .T. ) ;
#71626 = CIRCLE ( 'NONE', #61888, 9.999999999999998224 ) ;
#71625 = CARTESIAN_POINT ( 'NONE',  ( 15.92326719930538204, 21.14441083166260071, 10.00000000000000533 ) ) ;
#71627 = ORIENTED_EDGE ( 'NONE', *, *, #34322, .F. ) ;
#71628 = CARTESIAN_POINT ( 'NONE',  ( 200.3765029811139584, 283.5847115241710981, 16.85207472104531590 ) ) ;
#71629 = CARTESIAN_POINT ( 'NONE',  ( 158.4485968073939546, 275.2084588272041401, -13.86993402366507944 ) ) ;
#71630 = CARTESIAN_POINT ( 'NONE',  ( 204.7986527064648214, 275.9253235211867263, 14.74587861556245905 ) ) ;
#71631 = CARTESIAN_POINT ( 'NONE',  ( 151.4212479147002171, 275.0370223182968061, -8.550850240198341723 ) ) ;
#71632 = ORIENTED_EDGE ( 'NONE', *, *, #34989, .T. ) ;
#71633 = EDGE_CURVE ( 'NONE', #82108, #15950, #67684, .T. ) ;
#71634 = DIRECTION ( 'NONE',  ( 0.000000000000000000, 0.000000000000000000, 1.000000000000000000 ) ) ;
#71635 = CARTESIAN_POINT ( 'NONE',  ( 41.56734871454121816, 26.12755873383629535, -6.180339887498949025 ) ) ;
#71636 = AXIS2_PLACEMENT_3D ( 'NONE', #18400, #96932, #4174 ) ;
#71637 = ORIENTED_EDGE ( 'NONE', *, *, #61017, .T. ) ;
#71638 = ORIENTED_EDGE ( 'NONE', *, *, #17605, .F. ) ;
#71639 = CARTESIAN_POINT ( 'NONE',  ( 74.17829915416689346, 64.94294222156766239, 13.63034475538133350 ) ) ;
#71640 = ORIENTED_EDGE ( 'NONE', *, *, #34946, .T. ) ;
#71641 = CARTESIAN_POINT ( 'NONE',  ( 161.0794736472514614, 271.0204982161961880, 16.04590376577446165 ) ) ;
#71642 = ORIENTED_EDGE ( 'NONE', *, *, #90130, .T. ) ;
#71643 = CARTESIAN_POINT ( 'NONE',  ( 76.26946404230703536, 64.97317754398874001, 14.67006731301516176 ) ) ;
#71644 = CARTESIAN_POINT ( 'NONE',  ( 168.4682619938861023, 272.6906211788349310, 15.98134908431772594 ) ) ;
#71645 = LINE ( 'NONE', #89375, #57434 ) ;
#71646 = CARTESIAN_POINT ( 'NONE',  ( 70.74027447083685161, 68.01839942184822974, 9.368956669706040685 ) ) ;
#71647 = CARTESIAN_POINT ( 'NONE',  ( 193.7951232862128848, 294.4761830863158707, 13.69151923843489094 ) ) ;
#71648 = B_SPLINE_CURVE_WITH_KNOTS ( 'NONE', 3,
 ( #1930, #46500, #94658, #77436, #8034, #38907, #23700, #38222, #68641, #99562, #68145, #14459, #92972, #83896, #29653, #99072, #92000, #69137, #75773, #22047, #15424, #23028, #76746, #83391 ),
 .UNSPECIFIED., .F., .F.,
 ( 4, 2, 2, 2, 2, 2, 2, 2, 2, 2, 2, 4 ),
 ( 0.000000000000000000, 0.1250000000000111300, 0.2500000000000222600, 0.3750000000000334177, 0.4375000000000321410, 0.5000000000000308642, 0.5625000000000295319, 0.6250000000000281997, 0.6875000000000268674, 0.7500000000000255351, 0.8750000000000128786, 1.000000000000000000 ),
 .UNSPECIFIED. ) ;
#71649 = CARTESIAN_POINT ( 'NONE',  ( 177.9714937548455680, 255.7189482022137383, 8.882064279750110813 ) ) ;
#71650 = DIRECTION ( 'NONE',  ( -0.8660254037844359321, -0.5000000000000051070, -0.000000000000000000 ) ) ;
#71651 = CIRCLE ( 'NONE', #18264, 0.1418229129681487788 ) ;
#71652 = ORIENTED_EDGE ( 'NONE', *, *, #91677, .T. ) ;
#71653 = CARTESIAN_POINT ( 'NONE',  ( -19.52673012263424113, 93.12936169874843984, 59.99999999999999289 ) ) ;
#71654 = B_SPLINE_CURVE_WITH_KNOTS ( 'NONE', 3,
 ( #91539, #52497, #6418, #37298 ),
 .UNSPECIFIED., .F., .F.,
 ( 4, 4 ),
 ( 0.007320200878984583701, 0.01237002053563545159 ),
 .UNSPECIFIED. ) ;
#71655 = CARTESIAN_POINT ( 'NONE',  ( 22.06543860749898300, 21.24335787977763346, -9.188101187500008038 ) ) ;
#71656 = CARTESIAN_POINT ( 'NONE',  ( 205.7668501412109663, 274.2483563724483133, 11.09689540819876896 ) ) ;
#71657 = CARTESIAN_POINT ( 'NONE',  ( 191.2053780694017462, 298.1875778970886586, -9.406300816995585734 ) ) ;
#71659 = ORIENTED_EDGE ( 'NONE', *, *, #27885, .F. ) ;
#71658 = CARTESIAN_POINT ( 'NONE',  ( 159.2511875226268216, 254.8158473755685520, 15.75855490706745599 ) ) ;
#71660 = ORIENTED_EDGE ( 'NONE', *, *, #42865, .T. ) ;
#71661 = DIRECTION ( 'NONE',  ( 0.4999999999999998890, -0.8660254037844385966, 0.000000000000000000 ) ) ;
#71662 = B_SPLINE_CURVE_WITH_KNOTS ( 'NONE', 3,
 ( #84881, #8838, #93481, #70637 ),
 .UNSPECIFIED., .F., .F.,
 ( 4, 4 ),
 ( 0.03188865644562008383, 0.04088460837272645670 ),
 .UNSPECIFIED. ) ;
#71663 = CARTESIAN_POINT ( 'NONE',  ( 168.5771703487694992, 257.4052341225797704, -14.27990518792410768 ) ) ;
#71664 = CARTESIAN_POINT ( 'NONE',  ( 159.2289198208967775, 254.8544161663325838, -15.88961297684315888 ) ) ;
#71665 = CARTESIAN_POINT ( 'NONE',  ( -68.10632939235270555, 44.28490124273479012, -10.00000000000000000 ) ) ;
#71666 = CARTESIAN_POINT ( 'NONE',  ( 161.8811854682448939, 250.2605573099562264, 13.51112293479948789 ) ) ;
#71667 = LINE ( 'NONE', #39212, #85519 ) ;
#71668 = ORIENTED_EDGE ( 'NONE', *, *, #66674, .F. ) ;
#71669 = DIRECTION ( 'NONE',  ( -0.8660254037844377084, -0.5000000000000014433, -0.000000000000000000 ) ) ;
#71670 = CARTESIAN_POINT ( 'NONE',  ( 74.73078456835840200, 66.79972942087576371, -13.15602295301254543 ) ) ;
#71672 = EDGE_CURVE ( 'NONE', #80413, #10181, #91027, .T. ) ;
#71671 = CARTESIAN_POINT ( 'NONE',  ( 207.1122325394003951, 271.9180857031755636, 7.794245785756032774 ) ) ;
#71673 = CARTESIAN_POINT ( 'NONE',  ( 14.65434579541623172, 189.2677522451419065, -5.000000000000047962 ) ) ;
#71674 = CARTESIAN_POINT ( 'NONE',  ( 85.53293889029039576, 226.3149278399160949, -9.188101187500095079 ) ) ;
#71675 = CARTESIAN_POINT ( 'NONE',  ( 196.2547452604713385, 269.4049120393308385, -11.95081354204263668 ) ) ;
#71676 = CYLINDRICAL_SURFACE ( 'NONE', #53411, 10.00000000000010658 ) ;
#71677 = CARTESIAN_POINT ( 'NONE',  ( 167.2251136787149335, 278.4273091872281043, -13.36331558781519568 ) ) ;
#71679 = CARTESIAN_POINT ( 'NONE',  ( 75.55347530004152645, 65.47672821233528850, 13.82195870221527123 ) ) ;
#71678 = CARTESIAN_POINT ( 'NONE',  ( 7.942909239684589728, 166.2048013555410080, 4.594050593750051981 ) ) ;
#71680 = CARTESIAN_POINT ( 'NONE',  ( 200.8769374536528858, 282.7179335918746688, 17.26928237494566787 ) ) ;
#71681 = VERTEX_POINT ( 'NONE', #77275 ) ;
#71682 = EDGE_LOOP ( 'NONE', ( #34377, #37949, #94361, #77267 ) ) ;
#71683 = CARTESIAN_POINT ( 'NONE',  ( 197.9182972497701769, 265.0047853328303518, -3.008455722180424452 ) ) ;
#71684 = CARTESIAN_POINT ( 'NONE',  ( 78.77678738312307871, 47.31940876559444575, -13.55958224463107165 ) ) ;
#71685 = PLANE ( 'NONE',  #46701 ) ;
#71686 = CARTESIAN_POINT ( 'NONE',  ( 161.6127771116929921, 250.7254542206800352, -12.96229604595372464 ) ) ;
#71687 = CARTESIAN_POINT ( 'NONE',  ( 181.8542211641277788, 285.1504725237182356, 15.60384829402828011 ) ) ;
#71688 = CYLINDRICAL_SURFACE ( 'NONE', #88832, 7.500000000000000000 ) ;
#71689 = CARTESIAN_POINT ( 'NONE',  ( 28.02335264628875677, 196.1744531367911293, 4.594050593750047540 ) ) ;
#71690 = CARTESIAN_POINT ( 'NONE',  ( 83.43119661263050091, 205.6427522451417644, 1.119607411625061291E-15 ) ) ;
#71691 = CARTESIAN_POINT ( 'NONE',  ( 195.9913908494966392, 275.3482408794030221, 15.54441459790748148 ) ) ;
#71692 = ORIENTED_EDGE ( 'NONE', *, *, #4708, .F. ) ;
#71693 = CARTESIAN_POINT ( 'NONE',  ( 84.24277800523259430, 48.02810533160893414, 12.01781408871613266 ) ) ;
#71694 = EDGE_CURVE ( 'NONE', #68946, #31611, #23553, .T. ) ;
#71695 = B_SPLINE_CURVE_WITH_KNOTS ( 'NONE', 3,
 ( #74394, #97687, #83495, #52059, #74880, #29266, #100172, #14565, #6464, #21179 ),
 .UNSPECIFIED., .F., .F.,
 ( 4, 3, 3, 4 ),
 ( 0.001342218634783023945, 0.001498044977018986789, 0.004494154408217571929, 0.006632416054833400326 ),
 .UNSPECIFIED. ) ;
#71696 = B_SPLINE_CURVE_WITH_KNOTS ( 'NONE', 3,
 ( #33395, #35383, #19223, #57679, #11613, #96235, #10102, #88158, #65294, #18706, #40965, #18208, #27301, #42472, #72927, #49100, #71911, #80035, #81530, #12099, #27796, #72425, #80541, #73903, #10604, #2512, #41476, #42961, #11120, #4490, #95246, #25815, #41990, #97227, #3517, #34394, #22184, #5004, #6978, #91124, #29298, #59155, #91611, #82544, #83524, #30278, #67279, #51073 ),
 .UNSPECIFIED., .F., .F.,
 ( 4, 2, 2, 2, 2, 2, 2, 2, 2, 2, 2, 2, 2, 2, 2, 2, 2, 2, 2, 2, 2, 2, 2, 4 ),
 ( 0.001443219783669777217, 0.001907740669036624061, 0.002372261554403471123, 0.002604521997086893786, 0.002720652218428617260, 0.002836782439770340735, 0.002952912661112064643, 0.003069042882453788118, 0.003301303325137235067, 0.003765824210504130701, 0.004230345095871026334, 0.005159386866604723058, 0.006088428637338420650, 0.006552949522705311079, 0.007017470408072201508, 0.007133600629413924116, 0.007191665740084785853, 0.007249730850755647590, 0.007365861072097308615, 0.007481991293438970507, 0.007946512178805745577, 0.008411033064172518045, 0.008643293506855859176, 0.008875553949539200307 ),
 .UNSPECIFIED. ) ;
#71697 = CARTESIAN_POINT ( 'NONE',  ( 198.2505066714982149, 285.2670451491296149, 0.000000000000000000 ) ) ;
#71698 = AXIS2_PLACEMENT_3D ( 'NONE', #33833, #49020, #26714 ) ;
#71699 = CARTESIAN_POINT ( 'NONE',  ( -4.289699588770600869, 159.1423013555410080, -4.594050593750043987 ) ) ;
#71700 = DIRECTION ( 'NONE',  ( -1.000000000000000000, 0.000000000000000000, 0.000000000000000000 ) ) ;
#71701 = CARTESIAN_POINT ( 'NONE',  ( -0.01211276271276783001, 139.0458036431182620, 22.50000000000001776 ) ) ;
#71702 = CARTESIAN_POINT ( 'NONE',  ( -22.42236680055709641, 157.8615022471902591, 0.000000000000000000 ) ) ;
#71703 = CARTESIAN_POINT ( 'NONE',  ( 194.7900911235093133, 293.2606606935473792, -14.66228443412922999 ) ) ;
#71704 = CIRCLE ( 'NONE', #5378, 17.82106496071138224 ) ;
#71705 = DIRECTION ( 'NONE',  ( 1.000000000000000000, 0.000000000000000000, 0.000000000000000000 ) ) ;
#71706 = CARTESIAN_POINT ( 'NONE',  ( 164.0777181605478745, 246.4560510864015441, 5.763760713451748785 ) ) ;
#71707 = ADVANCED_FACE ( 'NONE', ( #60557 ), #52474, .T. ) ;
#71708 = CARTESIAN_POINT ( 'NONE',  ( 191.8456210280128005, 298.3606325003146367, -9.135603544929113085 ) ) ;
#71709 = CARTESIAN_POINT ( 'NONE',  ( 148.2980785574368952, 273.7871886041155562, 9.134436720559454770 ) ) ;
#71710 = ORIENTED_EDGE ( 'NONE', *, *, #33570, .T. ) ;
#71711 = EDGE_CURVE ( 'NONE', #90103, #83863, #32211, .T. ) ;
#71712 = DIRECTION ( 'NONE',  ( 0.8660254037844379305, 0.5000000000000011102, 0.000000000000000000 ) ) ;
#71713 = CARTESIAN_POINT ( 'NONE',  ( 113.2460989071574460, 230.0643266524160140, 9.188101187500095079 ) ) ;
#71714 = CARTESIAN_POINT ( 'NONE',  ( 23.42942861845947178, 22.03085787977762777, 9.188101187500006262 ) ) ;
#71715 = DIRECTION ( 'NONE',  ( -1.000000000000000000, 0.000000000000000000, 0.000000000000000000 ) ) ;
#71716 = CARTESIAN_POINT ( 'NONE',  ( 151.0249774166511827, 270.1664039458447064, 13.81320228137823491 ) ) ;
#71717 = VECTOR ( 'NONE', #42400, 1000.000000000000227 ) ;
#71719 = CARTESIAN_POINT ( 'NONE',  ( 162.2336410148055279, 251.8862672885301492, -14.09881826716025799 ) ) ;
#71718 = CARTESIAN_POINT ( 'NONE',  ( 157.1606030646430554, 258.4368458743103361, 17.96998724893680688 ) ) ;
#71720 = CARTESIAN_POINT ( 'NONE',  ( 191.0684812360443914, 299.7066781045875246, -8.010743411620572019 ) ) ;
#71721 = CARTESIAN_POINT ( 'NONE',  ( 192.8225454482096666, 263.7804965554488490, -4.355381635346724067 ) ) ;
#71722 = CARTESIAN_POINT ( 'NONE',  ( 197.0226655822963551, 289.3937282992477549, -17.28982543158101493 ) ) ;
#71723 = CARTESIAN_POINT ( 'NONE',  ( 175.1758473867431292, 292.4163926228642936, -1.150070930579374151 ) ) ;
#71724 = CARTESIAN_POINT ( 'NONE',  ( 86.41689343025348080, 47.58309788860988476, 10.57565383929702563 ) ) ;
#71725 = ORIENTED_EDGE ( 'NONE', *, *, #36985, .F. ) ;
#71726 = LINE ( 'NONE', #49400, #84584 ) ;
#71727 = CARTESIAN_POINT ( 'NONE',  ( 175.5888903117697453, 278.5951473192365597, 15.44173524372987139 ) ) ;
#71728 = CARTESIAN_POINT ( 'NONE',  ( 165.3957260903385134, 269.6996331764513002, -16.29327252992070996 ) ) ;
#71729 = CARTESIAN_POINT ( 'NONE',  ( 200.1133476818314705, 272.1141633677412415, 12.87458617912082914 ) ) ;
#71730 = CARTESIAN_POINT ( 'NONE',  ( 83.84059829558975707, 51.56187102439434256, -14.37481623513500040 ) ) ;
#71731 = DIRECTION ( 'NONE',  ( 0.000000000000000000, 0.000000000000000000, 1.000000000000000000 ) ) ;
#71732 = CARTESIAN_POINT ( 'NONE',  ( 148.2247184032906375, 275.5581615573433396, 5.963085520373529569 ) ) ;
#71733 = ORIENTED_EDGE ( 'NONE', *, *, #71828, .F. ) ;
#71734 = EDGE_CURVE ( 'NONE', #47543, #66560, #11783, .T. ) ;
#71735 = CARTESIAN_POINT ( 'NONE',  ( 198.9721957120447655, 281.0613474150461570, 17.36564602955951386 ) ) ;
#71736 = CARTESIAN_POINT ( 'NONE',  ( 37.18479240120036167, 39.65586893147759895, -7.433330006724137462 ) ) ;
#71737 = CARTESIAN_POINT ( 'NONE',  ( 174.0223458074996472, 272.1910991151906956, -17.55968156639984556 ) ) ;
#71738 = EDGE_LOOP ( 'NONE', ( #29759, #7097, #3254, #69380 ) ) ;
#71739 = CARTESIAN_POINT ( 'NONE',  ( 78.13090640523601849, 61.76054338150410672, 16.10053832301867516 ) ) ;
#71740 = CARTESIAN_POINT ( 'NONE',  ( 148.1829914015846157, 273.9865254053503349, -9.304102644963160529 ) ) ;
#71741 = CARTESIAN_POINT ( 'NONE',  ( 21.76528272068881265, 171.8262482093457777, 3.021315404115420679E-15 ) ) ;
#71742 = EDGE_LOOP ( 'NONE', ( #92813, #16508, #68620, #83586 ) ) ;
#71743 = CARTESIAN_POINT ( 'NONE',  ( 79.49274628814450239, 59.57836040576013659, 16.53926144102299389 ) ) ;
#71744 = DIRECTION ( 'NONE',  ( -0.9086904199442051855, 0.4174706225611858335, 0.000000000000000000 ) ) ;
#71745 = CARTESIAN_POINT ( 'NONE',  ( 41.47569090598248920, 209.1868197944957899, -17.47570218321533275 ) ) ;
#71746 = CARTESIAN_POINT ( 'NONE',  ( 80.82219357636691370, 51.10915316415084675, -14.83884473207257670 ) ) ;
#71747 = CARTESIAN_POINT ( 'NONE',  ( 80.47142419695269666, 44.41285142414567844, 11.35032686343901354 ) ) ;
#71748 = CARTESIAN_POINT ( 'NONE',  ( 154.9048824156581361, 262.3438686460345366, -17.40627786727128168 ) ) ;
#71749 = ORIENTED_EDGE ( 'NONE', *, *, #22330, .F. ) ;
#71750 = ORIENTED_EDGE ( 'NONE', *, *, #72194, .F. ) ;
#71751 = CARTESIAN_POINT ( 'NONE',  ( 100.3908607700757187, 228.7677522451418497, 10.00000000000009592 ) ) ;
#71752 = ORIENTED_EDGE ( 'NONE', *, *, #88243, .T. ) ;
#71753 = CARTESIAN_POINT ( 'NONE',  ( 81.25645528111445515, 55.75359181263093689, 16.38715272843555226 ) ) ;
#71754 = ORIENTED_EDGE ( 'NONE', *, *, #26528, .T. ) ;
#71755 = LINE ( 'NONE', #40809, #73513 ) ;
#71756 = CARTESIAN_POINT ( 'NONE',  ( 79.50406474403273194, 54.96663328783942148, 16.02396390402955006 ) ) ;
#71757 = ORIENTED_EDGE ( 'NONE', *, *, #29469, .T. ) ;
#71758 = CARTESIAN_POINT ( 'NONE',  ( 185.6868470588481159, 282.1044346093191848, -16.51667675334077501 ) ) ;
#71759 = CARTESIAN_POINT ( 'NONE',  ( 25.81463925578599117, 37.83705186507755514, 3.090169943749475401 ) ) ;
#71760 = CARTESIAN_POINT ( 'NONE',  ( 147.3161703957304667, 275.4879034285576722, -5.959278055987775602 ) ) ;
#71761 = CARTESIAN_POINT ( 'NONE',  ( 196.9911704225566211, 284.9555270314510267, -17.17161694444654785 ) ) ;
#71762 = PLANE ( 'NONE',  #35345 ) ;
#71763 = CARTESIAN_POINT ( 'NONE',  ( 152.9607371460978129, 265.7112270302071124, -16.17698032818104537 ) ) ;
#71764 = DIRECTION ( 'NONE',  ( -0.000000000000000000, 0.000000000000000000, -1.000000000000000000 ) ) ;
#71765 = CARTESIAN_POINT ( 'NONE',  ( 201.3053657339852691, 274.7141922394133076, -14.27644254562359372 ) ) ;
#71766 = CARTESIAN_POINT ( 'NONE',  ( 122.2847184155099995, 253.6589784336661069, -6.496448406907675876E-16 ) ) ;
#71767 = CARTESIAN_POINT ( 'NONE',  ( 70.79886843151163589, 61.41865354507500996, -14.84698767043841627 ) ) ;
#71768 = CARTESIAN_POINT ( 'NONE',  ( 43.17480782474465428, 33.43085787977766898, -9.188101187500008038 ) ) ;
#71769 = ADVANCED_FACE ( 'NONE', ( #93513 ), #24070, .T. ) ;
#71770 = VERTEX_POINT ( 'NONE', #40753 ) ;
#71771 = VECTOR ( 'NONE', #44395, 1000.000000000000114 ) ;
#71772 = CARTESIAN_POINT ( 'NONE',  ( 85.68664465223866955, 48.45350732935998650, -12.23334744974731869 ) ) ;
#71773 = LINE ( 'NONE', #24644, #98337 ) ;
#71774 = CARTESIAN_POINT ( 'NONE',  ( 56.67693180720107193, 191.9824982072973967, 3.021315404115420679E-15 ) ) ;
#71775 = CARTESIAN_POINT ( 'NONE',  ( 173.7213227573953986, 290.5666012884805696, -4.949759831816241906 ) ) ;
#71776 = CARTESIAN_POINT ( 'NONE',  ( 57.60966550219796289, 179.2419560658249225, 18.47570218321542868 ) ) ;
#71777 = CARTESIAN_POINT ( 'NONE',  ( 152.7122812589697958, 277.9324518551267147, 6.933031942251369983 ) ) ;
#71778 = CARTESIAN_POINT ( 'NONE',  ( 80.76436682390523458, 43.05937393749385222, 9.753329205520538281 ) ) ;
#71779 = CARTESIAN_POINT ( 'NONE',  ( 173.6700662098836290, 287.8081707173866448, -9.948204391775917088 ) ) ;
#71780 = CARTESIAN_POINT ( 'NONE',  ( 171.5564966965742997, 280.0145032911023577, 13.85370006234987450 ) ) ;
#71781 = CARTESIAN_POINT ( 'NONE',  ( 176.9521628696608104, 255.8834708374732543, -7.282453275594096276 ) ) ;
#71782 = VERTEX_POINT ( 'NONE', #32167 ) ;
#71783 = CARTESIAN_POINT ( 'NONE',  ( 147.9500839974939197, 274.3899328626944225, -9.375093207164509224 ) ) ;
#71784 = CARTESIAN_POINT ( 'NONE',  ( 65.82437617505169669, 69.12761414359022183, -0.3171011309739659167 ) ) ;
#71785 = ORIENTED_EDGE ( 'NONE', *, *, #95640, .T. ) ;
#71786 = CARTESIAN_POINT ( 'NONE',  ( -59.87889494062799400, 37.30571521936384016, -10.00000000000000000 ) ) ;
#71787 = VECTOR ( 'NONE', #94937, 1000.000000000000000 ) ;
#71788 = CARTESIAN_POINT ( 'NONE',  ( 205.0978449570898476, 268.9670457764514708, -3.035070700556400158 ) ) ;
#71789 = CARTESIAN_POINT ( 'NONE',  ( 152.4585818852530963, 266.5809854552784941, -16.62427189540569117 ) ) ;
#71790 = CARTESIAN_POINT ( 'NONE',  ( 149.7166446726674565, 271.3301600186404698, 12.26048591517335495 ) ) ;
#71791 = CARTESIAN_POINT ( 'NONE',  ( 202.9972156839127990, 279.0455039708822937, 16.77197898838388213 ) ) ;
#71793 = CARTESIAN_POINT ( 'NONE',  ( 160.3733185927383715, 282.5102941377067509, 6.606729549618552078 ) ) ;
#71792 = CARTESIAN_POINT ( 'NONE',  ( 163.1953264782998758, 283.8895661455310915, -7.125257539458086598 ) ) ;
#71794 = CARTESIAN_POINT ( 'NONE',  ( 200.9061540366740246, 282.6673289856585143, -18.13083321883407351 ) ) ;
#71795 = EDGE_LOOP ( 'NONE', ( #46547, #97999, #63511, #22924 ) ) ;
#71796 = CARTESIAN_POINT ( 'NONE',  ( 167.8261084473395499, 282.2036296651569387, -10.70662813516634060 ) ) ;
#71797 = PRODUCT_DEFINITION_SHAPE ( 'NONE', 'NONE',  #80580 ) ;
#71798 = CARTESIAN_POINT ( 'NONE',  ( 9.963374858250592325, 169.8927522451418213, 10.00000000000009948 ) ) ;
#71799 = CARTESIAN_POINT ( 'NONE',  ( 193.1669738419331850, 275.7633846255446315, -16.84869157407539575 ) ) ;
#71800 = CARTESIAN_POINT ( 'NONE',  ( 74.07275743019523873, 225.1199935810941213, 2.679491924311251605 ) ) ;
#71801 = CARTESIAN_POINT ( 'NONE',  ( 74.94581410820386225, 65.07354109301314793, -13.82487701360099486 ) ) ;
#71802 = B_SPLINE_CURVE_WITH_KNOTS ( 'NONE', 3,
 ( #93883, #42976, #10245, #71556, #33032, #70530, #20217, #89179, #55803, #41115, #35401, #50593, #55317, #81543, #16831, #86796, #2152, #12114, #63931, #94870, #17331, #72049, #27807, #58682, #82050, #9241, #47718, #89655, #25432, #12623, #17850, #95398, #1147, #78655, #53582, #60670, #66797, #21701, #74923, #84536, #83541, #29798, #36389, #21215, #5504, #67804 ),
 .UNSPECIFIED., .F., .F.,
 ( 4, 1, 2, 2, 1, 2, 2, 1, 1, 2, 2, 1, 1, 2, 2, 1, 1, 2, 2, 1, 1, 1, 2, 2, 1, 1, 1, 2, 2, 4 ),
 ( 0.000000000000000000, 0.06250000000001508516, 0.09375000000002250977, 0.1250000000000299483, 0.1875000000000420775, 0.2187500000000465739, 0.2500000000000510703, 0.3125000000000602851, 0.3437500000000658362, 0.3593750000000670020, 0.3750000000000681122, 0.4375000000000753841, 0.4687500000000789924, 0.4843750000000808242, 0.5000000000000826006, 0.5625000000000942579, 0.5937500000000983658, 0.6093750000001009193, 0.6250000000001034728, 0.6875000000001139089, 0.7187500000001180167, 0.7343750000001182388, 0.7421875000001172396, 0.7500000000001161293, 0.8125000000000947020, 0.8437500000000832667, 0.8593750000000782707, 0.8671875000000739409, 0.8750000000000696110, 1.000000000000000000 ),
 .UNSPECIFIED. ) ;
#71803 = CARTESIAN_POINT ( 'NONE',  ( 192.0523540417460993, 298.0025604169266558, 12.03387399082417275 ) ) ;
#71804 = CARTESIAN_POINT ( 'NONE',  ( 73.89028189157257032, 68.56231543382321547, 11.39439152759356944 ) ) ;
#71805 =( BOUNDED_CURVE ( )  B_SPLINE_CURVE ( 2, ( #94619, #9997, #78400, #70787, #63180, #17585, #25177, #38872, #56057 ),
 .UNSPECIFIED., .F., .T. ) 
 B_SPLINE_CURVE_WITH_KNOTS ( ( 3, 2, 2, 2, 3 ),
 ( 0.02822580645161290591, 0.02956989247311828106, 0.03225806451612903136, 0.03494623655913978166, 0.03629032258064516375 ),
 .UNSPECIFIED. ) 
 CURVE ( )  GEOMETRIC_REPRESENTATION_ITEM ( )  RATIONAL_B_SPLINE_CURVE ( ( 0.9330127018922192983, 0.9330127018922194093, 1.000000000000000000, 0.8660254037844387076, 1.000000000000000000, 0.8660254037844387076, 1.000000000000000000, 0.9330127018922191873, 0.9330127018922194093 ) ) 
 REPRESENTATION_ITEM ( '' )  );
#71806 = CARTESIAN_POINT ( 'NONE',  ( 194.3799873100184641, 293.9709813348915191, 15.33105633561973669 ) ) ;
#71807 = CARTESIAN_POINT ( 'NONE',  ( 67.68166703610724255, 69.53423434588013663, 2.055755005019128667 ) ) ;
#71808 = CARTESIAN_POINT ( 'NONE',  ( -12.86919761471646773, 169.5024278399161233, -9.188101187500093303 ) ) ;
#71809 = CARTESIAN_POINT ( 'NONE',  ( 93.67942421434402434, 215.7048013555409796, 4.594050593750051981 ) ) ;
#71810 = CARTESIAN_POINT ( 'NONE',  ( 202.7676489560256528, 279.4431252073101746, -16.04062356091568020 ) ) ;
#71811 = CARTESIAN_POINT ( 'NONE',  ( 88.18429177444041045, 44.53138063026126048, -4.871266200417320391 ) ) ;
#71812 = CARTESIAN_POINT ( 'NONE',  ( -17.42236680055705023, 149.2012482093457777, 0.000000000000000000 ) ) ;
#71813 = CARTESIAN_POINT ( 'NONE',  ( -10.37017993122367976, 171.4865022471902876, 10.00000000000009415 ) ) ;
#71814 = CARTESIAN_POINT ( 'NONE',  ( 77.77751611803083165, 53.46578304951030702, 15.90232757848929523 ) ) ;
#71815 = CARTESIAN_POINT ( 'NONE',  ( 160.6677038066905823, 282.0210727026695849, 5.138757052024616634 ) ) ;
#71817 = CARTESIAN_POINT ( 'NONE',  ( 208.3682389855799499, 269.7426187237583690, -1.431169231381201890 ) ) ;
#71816 = CARTESIAN_POINT ( 'NONE',  ( 190.4455119341017451, 300.3931655422463791, -0.7229603976562811729 ) ) ;
#71818 = CARTESIAN_POINT ( 'NONE',  ( 178.5259719646841745, 290.8553054119842045, 10.01277831063413437 ) ) ;
#71819 = EDGE_CURVE ( 'NONE', #46780, #81902, #86941, .T. ) ;
#71820 = CARTESIAN_POINT ( 'NONE',  ( 81.22424941298332612, 53.84597802519924414, -15.65359963525670217 ) ) ;
#71821 = CARTESIAN_POINT ( 'NONE',  ( 79.47466498719533945, 53.91538503943934302, -16.25957047384575915 ) ) ;
#71822 = CARTESIAN_POINT ( 'NONE',  ( 207.2167723318516153, 271.7370174712370954, -6.606038862010207957 ) ) ;
#71824 = EDGE_CURVE ( 'NONE', #4560, #65492, #2804, .T. ) ;
#71823 = CARTESIAN_POINT ( 'NONE',  ( 71.69164292429383067, 72.03424767056361588, -1.595364931656152674 ) ) ;
#71825 = CARTESIAN_POINT ( 'NONE',  ( 48.29419362332453858, 192.5643266524160140, 9.188101187500095079 ) ) ;
#71827 = ADVANCED_FACE ( 'NONE', ( #79820 ), #16962, .T. ) ;
#71826 = CARTESIAN_POINT ( 'NONE',  ( 76.74023481339004604, 63.31925950119924096, -15.43993991125870124 ) ) ;
#71828 = EDGE_CURVE ( 'NONE', #17141, #17498, #33176, .T. ) ;
#71829 = CARTESIAN_POINT ( 'NONE',  ( 72.54290492928882372, 206.5643266524159571, -9.188101187500093303 ) ) ;
#71830 = CARTESIAN_POINT ( 'NONE',  ( 207.1572261440131797, 271.8401544939704877, -5.633070628900782140 ) ) ;
#71831 = CARTESIAN_POINT ( 'NONE',  ( 75.73407124508247534, 53.49751973368108082, -16.50271086146291211 ) ) ;
#71832 = CARTESIAN_POINT ( 'NONE',  ( 164.6052063594347032, 258.5370629776766123, 15.54664782134921097 ) ) ;
#71834 = FACE_OUTER_BOUND ( 'NONE', #47403, .T. ) ;
#71833 = DIRECTION ( 'NONE',  ( 0.000000000000000000, 0.000000000000000000, 1.000000000000000000 ) ) ;
#71835 = CARTESIAN_POINT ( 'NONE',  ( 173.8329535930888881, 268.6061503712382432, -16.29996300370038043 ) ) ;
#71836 = CARTESIAN_POINT ( 'NONE',  ( 28.70736568013821355, 22.28920272979928185, -7.433330006724141015 ) ) ;
#71837 = FACE_OUTER_BOUND ( 'NONE', #72410, .T. ) ;
#71838 = CARTESIAN_POINT ( 'NONE',  ( 196.7130436017243653, 289.9300093007386749, -16.33278734947153765 ) ) ;
#71839 = ORIENTED_EDGE ( 'NONE', *, *, #72475, .T. ) ;
#71840 = CARTESIAN_POINT ( 'NONE',  ( 22.99159801516092472, 18.98920272979926693, 7.433330006724137462 ) ) ;
#71841 = CARTESIAN_POINT ( 'NONE',  ( 80.01237403692960015, 210.8768266524159856, -9.188101187500093303 ) ) ;
#71842 = CYLINDRICAL_SURFACE ( 'NONE', #96708, 15.60714546451156970 ) ;
#71843 = CARTESIAN_POINT ( 'NONE',  ( 173.1031462479762411, 289.7790225637821209, -0.7365366526630715560 ) ) ;
#71844 = CARTESIAN_POINT ( 'NONE',  ( -32.57449995691604272, 93.91662174944717378, 10.44639423499586428 ) ) ;
#71845 = CARTESIAN_POINT ( 'NONE',  ( 50.32263495959776378, 94.90690751109829648, 177.5919119679930134 ) ) ;
#71846 = EDGE_LOOP ( 'NONE', ( #474, #45518, #52911, #13928 ) ) ;
#71847 = DIRECTION ( 'NONE',  ( -0.8434505012732950169, 0.5372068985985076761, 0.000000000000000000 ) ) ;
#71848 = CARTESIAN_POINT ( 'NONE',  ( 189.9889038007835040, 286.7716972915182509, 16.94430205996046013 ) ) ;
#71849 = CARTESIAN_POINT ( 'NONE',  ( 116.2138665886017606, 251.2365022471903444, 2.944929066748280225E-16 ) ) ;
#71850 = LINE ( 'NONE', #94167, #8619 ) ;
#71851 = CARTESIAN_POINT ( 'NONE',  ( 75.32116640173099142, 53.12209477811269664, 16.48561212775914697 ) ) ;
#71852 = ORIENTED_EDGE ( 'NONE', *, *, #53702, .T. ) ;
#71853 = CARTESIAN_POINT ( 'NONE',  ( 188.6960043714797166, 272.5830035644334544, 16.09278530888001413 ) ) ;
#71854 = VERTEX_POINT ( 'NONE', #85942 ) ;
#71855 = CARTESIAN_POINT ( 'NONE',  ( 203.0507839702407580, 278.9527209772879814, 16.21318481136342626 ) ) ;
#71856 = CARTESIAN_POINT ( 'NONE',  ( -19.79442730923454263, 93.05285538284211100, 59.99999999999999289 ) ) ;
#71857 = CARTESIAN_POINT ( 'NONE',  ( 153.2283961777204695, 265.2476279883323400, -17.66880461074566000 ) ) ;
#71858 = ORIENTED_EDGE ( 'NONE', *, *, #19912, .F. ) ;
#71859 = CARTESIAN_POINT ( 'NONE',  ( 174.4814676270071345, 252.3592025919409991, -0.2517021329253662509 ) ) ;
#71861 = ORIENTED_EDGE ( 'NONE', *, *, #79595, .T. ) ;
#71860 = VECTOR ( 'NONE', #84466, 1000.000000000000000 ) ;
#71862 = CARTESIAN_POINT ( 'NONE',  ( 79.11275361910446691, 46.11146926033848104, 13.27945046499836579 ) ) ;
#71863 = CARTESIAN_POINT ( 'NONE',  ( 170.7889457633958727, 250.2325148129452259, 2.962128769278053131 ) ) ;
#71864 = CARTESIAN_POINT ( 'NONE',  ( 206.9220859797902961, 271.2613808489912799, -5.355436660003541682 ) ) ;
#71865 = VERTEX_POINT ( 'NONE', #54963 ) ;
#71866 = CARTESIAN_POINT ( 'NONE',  ( 36.63328578856461348, 23.01110640527294748, 2.839279412974134775 ) ) ;
#71867 = CARTESIAN_POINT ( 'NONE',  ( 79.75726243291551043, 44.80792267523282391, 11.39221341620031502 ) ) ;
#71868 = CARTESIAN_POINT ( 'NONE',  ( 84.77725617564227889, 50.41784377465270950, -13.48640040656236927 ) ) ;
#71869 = CARTESIAN_POINT ( 'NONE',  ( 78.06375342405178230, 49.62358045365419201, -14.80969209974775325 ) ) ;
#71870 = CARTESIAN_POINT ( 'NONE',  ( 168.0746954366166506, 276.8294243769387890, 15.45034248799716714 ) ) ;
#71871 = CARTESIAN_POINT ( 'NONE',  ( 86.71718800452170228, 209.3262482093457493, 3.021315404115420679E-15 ) ) ;
#71872 = VERTEX_POINT ( 'NONE', #78287 ) ;
#71873 = EDGE_LOOP ( 'NONE', ( #98561, #16223, #12339, #31456, #5141, #80381, #76449, #61651, #50160, #48172, #64416, #63797, #72882, #60006, #35844, #1979, #73550, #38956, #84102, #8361 ) ) ;
#71874 = CARTESIAN_POINT ( 'NONE',  ( 184.0405880873563547, 296.3429400402605438, 1.017449987670831169 ) ) ;
#71876 = CARTESIAN_POINT ( 'NONE',  ( 194.4032909867620447, 293.9306181827685123, -16.05392006271526384 ) ) ;
#71875 = CARTESIAN_POINT ( 'NONE',  ( 67.79725476218452229, 65.71048819351142356, 10.00598338191752390 ) ) ;
#71877 = CARTESIAN_POINT ( 'NONE',  ( 208.3586375946586315, 269.7592488206576604, -1.970210487958146128 ) ) ;
#71878 = CARTESIAN_POINT ( 'NONE',  ( 185.4035662733510605, 292.5150471097351783, -10.83705993876271201 ) ) ;
#71879 = CARTESIAN_POINT ( 'NONE',  ( 47.54560441532652959, 78.55524412553474178, 10.00000000000000000 ) ) ;
#71880 = CARTESIAN_POINT ( 'NONE',  ( 78.28621045032348036, 60.56628696945801238, -16.35393821005401804 ) ) ;
#71881 = CARTESIAN_POINT ( 'NONE',  ( 177.5654003108776351, 286.5527965801844630, -13.65658207675519975 ) ) ;
#71882 = CARTESIAN_POINT ( 'NONE',  ( 83.31357524521028779, 231.1589784336661637, -6.496448406907675876E-16 ) ) ;
#71884 = ORIENTED_EDGE ( 'NONE', *, *, #30739, .F. ) ;
#71883 = B_SPLINE_CURVE_WITH_KNOTS ( 'NONE', 3,
 ( #19720, #67284, #20707, #65300, #42479, #89173, #28794, #65785, #59674, #51594, #73413, #82549, #35888, #66301, #97233, #96743, #66790, #4000, #58192, #96242, #4495, #89647, #74425, #27306, #12107, #98211, #26803, #35391, #20208, #90134, #5009, #50585, #52086, #27801, #90648, #97716, #13114, #81535, #28284, #58675, #51080, #82042, #57686, #74914, #5496, #12616 ),
 .UNSPECIFIED., .F., .F.,
 ( 4, 1, 2, 2, 1, 2, 2, 1, 1, 2, 2, 1, 1, 2, 2, 1, 1, 2, 2, 1, 1, 1, 2, 2, 1, 1, 1, 2, 2, 4 ),
 ( 0.000000000000000000, 0.06249999999999761302, 0.09374999999999655831, 0.1249999999999955036, 0.1874999999999933942, 0.2187499999999937550, 0.2499999999999941158, 0.3124999999999954481, 0.3437499999999967248, 0.3593749999999983347, 0.3749999999999998890, 0.4374999999999985012, 0.4687499999999967804, 0.4843749999999955591, 0.4999999999999943379, 0.5624999999999901190, 0.5937499999999876765, 0.6093749999999867883, 0.6249999999999860112, 0.6874999999999786837, 0.7187499999999742428, 0.7343749999999733546, 0.7421874999999722444, 0.7499999999999710232, 0.8124999999999769074, 0.8437499999999799050, 0.8593749999999821254, 0.8671874999999829026, 0.8749999999999835687, 1.000000000000000000 ),
 .UNSPECIFIED. ) ;
#71885 = CARTESIAN_POINT ( 'NONE',  ( 149.9104953625653991, 271.4222773149817840, 11.90972932297161080 ) ) ;
#71886 = CARTESIAN_POINT ( 'NONE',  ( 159.3383002321867821, 278.1316173108193084, 11.89870031586311683 ) ) ;
#71887 = CARTESIAN_POINT ( 'NONE',  ( 78.16855185334185308, 61.58847221756811052, -16.14202726422458767 ) ) ;
#71888 = ADVANCED_FACE ( 'NONE', ( #86436 ), #8871, .F. ) ;
#71889 = EDGE_LOOP ( 'NONE', ( #11841, #24505, #90581, #73818 ) ) ;
#71890 = CARTESIAN_POINT ( 'NONE',  ( 73.67824366217406862, 55.52431661998092238, 16.58293631993679540 ) ) ;
#71891 = ORIENTED_EDGE ( 'NONE', *, *, #18384, .T. ) ;
#71892 = CARTESIAN_POINT ( 'NONE',  ( 80.42973500905783624, 44.73750331184790952, -11.66451360117097558 ) ) ;
#71893 = CARTESIAN_POINT ( 'NONE',  ( 75.36633504343575396, 220.9865022471902876, 10.00000000000009415 ) ) ;
#71894 = PLANE ( 'NONE',  #74062 ) ;
#71895 = CARTESIAN_POINT ( 'NONE',  ( 34.35958382788741261, 28.03677371833804344, 10.00000000000000533 ) ) ;
#71896 = CARTESIAN_POINT ( 'NONE',  ( 182.5291792280718823, 296.7636338796572204, 0.3805386115670883473 ) ) ;
#71897 = CARTESIAN_POINT ( 'NONE',  ( 162.6076392040105816, 249.0023025302617725, 11.70000256607044165 ) ) ;
#71898 = ORIENTED_EDGE ( 'NONE', *, *, #37497, .F. ) ;
#71899 = EDGE_LOOP ( 'NONE', ( #11363, #67619, #19049, #10634 ) ) ;
#71900 = CARTESIAN_POINT ( 'NONE',  ( 163.4055107321044318, 247.6203485056908846, -10.24153090796238530 ) ) ;
#71901 = ORIENTED_EDGE ( 'NONE', *, *, #29907, .T. ) ;
#71902 = EDGE_CURVE ( 'NONE', #49096, #58645, #48383, .T. ) ;
#71903 = CARTESIAN_POINT ( 'NONE',  ( 75.67384099942408682, 65.13299740138256766, -14.43017819244620803 ) ) ;
#71904 = CARTESIAN_POINT ( 'NONE',  ( 71.69170005589681693, 69.37806338950922225, -8.395052771507090839 ) ) ;
#71905 = CARTESIAN_POINT ( 'NONE',  ( -15.15136185149820847, 175.3927522451419350, 2.944929066748280225E-16 ) ) ;
#71906 = CARTESIAN_POINT ( 'NONE',  ( 88.16762080519842470, 44.42520534355205797, 4.589585637743891056 ) ) ;
#71907 = ORIENTED_EDGE ( 'NONE', *, *, #334, .T. ) ;
#71908 = CARTESIAN_POINT ( 'NONE',  ( 87.42460433697408462, 44.12820928407189314, -3.507511662899541527 ) ) ;
#71909 = CARTESIAN_POINT ( 'NONE',  ( 160.1349499500167894, 275.4254527969055744, 12.83854157865886236 ) ) ;
#71910 = CARTESIAN_POINT ( 'NONE',  ( 159.9894443651313338, 253.5371490153152081, -16.36035038356864391 ) ) ;
#71911 = CARTESIAN_POINT ( 'NONE',  ( 188.9935787721526594, 269.7997667481943722, 14.53618363141985448 ) ) ;
#71912 = LINE ( 'NONE', #24302, #1061 ) ;
#71913 = CARTESIAN_POINT ( 'NONE',  ( 198.9561107160696736, 285.0479304499367572, -17.31132130523259960 ) ) ;
#71914 = AXIS2_PLACEMENT_3D ( 'NONE', #72556, #19357, #27436 ) ;
#71915 = DIRECTION ( 'NONE',  ( 0.000000000000000000, -0.000000000000000000, 1.000000000000000000 ) ) ;
#71916 = VERTEX_POINT ( 'NONE', #9895 ) ;
#71917 = CARTESIAN_POINT ( 'NONE',  ( 203.2378153033330932, 277.9981038445823174, -14.71139916435034323 ) ) ;
#71918 = CARTESIAN_POINT ( 'NONE',  ( 161.8811854682448939, 250.2605573099562264, 13.51112293479948789 ) ) ;
#71919 = CARTESIAN_POINT ( 'NONE',  ( 85.59540126815005578, 44.41612895177246401, 6.888311711144287308 ) ) ;
#71920 = DIRECTION ( 'NONE',  ( -0.2588190451025411121, -0.9659258262890628721, -2.299878683274462667E-16 ) ) ;
#71921 = CARTESIAN_POINT ( 'NONE',  ( 77.99842658917772553, 61.99000515389445809, 15.67651427494045890 ) ) ;
#71922 = CARTESIAN_POINT ( 'NONE',  ( 174.8635978287226180, 290.2966283512476480, -6.424262721924552721 ) ) ;
#71923 = DIRECTION ( 'NONE',  ( 0.9985437513708439461, 0.05394790633789421641, 0.000000000000000000 ) ) ;
#71924 = ORIENTED_EDGE ( 'NONE', *, *, #85845, .F. ) ;
#71925 = AXIS2_PLACEMENT_3D ( 'NONE', #58397, #89372, #97432 ) ;
#71926 = CARTESIAN_POINT ( 'NONE',  ( 164.7694554770609159, 245.2579269087094076, -3.003635650077957742 ) ) ;
#71927 = CARTESIAN_POINT ( 'NONE',  ( 74.12482479103741184, 55.26569620697679852, 16.12359666345034626 ) ) ;
#71928 = CARTESIAN_POINT ( 'NONE',  ( 69.59282007774174872, 62.40894646771045018, -13.45448169915730041 ) ) ;
#71929 = CARTESIAN_POINT ( 'NONE',  ( 37.20204829050883433, 21.28848085856233752, 1.475505719884397138E-15 ) ) ;
#71930 = DIRECTION ( 'NONE',  ( -0.000000000000000000, -0.000000000000000000, -1.000000000000000000 ) ) ;
#71931 = CARTESIAN_POINT ( 'NONE',  ( 171.2100401816418298, 274.3227513589740738, 16.12125467595794959 ) ) ;
#71932 = CARTESIAN_POINT ( 'NONE',  ( 181.7118876060299328, 273.6476297288324417, 17.70437625449880414 ) ) ;
#71933 = CARTESIAN_POINT ( 'NONE',  ( 87.73298548431468191, 44.18903561216112763, 4.633618514853090176 ) ) ;
#71934 = CARTESIAN_POINT ( 'NONE',  ( 188.5734885077569629, 260.2193828105671400, 3.781240722223853989 ) ) ;
#71935 = CARTESIAN_POINT ( 'NONE',  ( 207.8718670335145475, 270.6023601641878713, -6.322166851501095586 ) ) ;
#71936 = CARTESIAN_POINT ( 'NONE',  ( 0.4998960083233069396, 183.3464784336661353, 1.353441290958777327E-15 ) ) ;
#71937 = CARTESIAN_POINT ( 'NONE',  ( 82.04497822609438629, 47.34932639374565611, 12.42682962033639527 ) ) ;
#71938 = EDGE_LOOP ( 'NONE', ( #92093, #38701, #63127, #68419 ) ) ;
#71939 = EDGE_CURVE ( 'NONE', #61410, #79692, #28967, .T. ) ;
#71940 = CARTESIAN_POINT ( 'NONE',  ( 178.7827978530413020, 256.8763733133778828, 8.538386915803064525 ) ) ;
#71941 = CARTESIAN_POINT ( 'NONE',  ( 148.4047294057049555, 273.6024639162449716, 0.000000000000000000 ) ) ;
#71942 = CARTESIAN_POINT ( 'NONE',  ( 191.1302745162771259, 290.4652077767679543, 15.89733196130017134 ) ) ;
#71943 = CARTESIAN_POINT ( 'NONE',  ( 82.28113228126468925, 41.34250681205937639, 5.451554181100740415 ) ) ;
#71944 = CARTESIAN_POINT ( 'NONE',  ( 32.89474554257621719, 198.9869531367911293, 4.594050593750046652 ) ) ;
#71945 = CARTESIAN_POINT ( 'NONE',  ( 200.1102648775588193, 284.0458494464393198, 17.54251420653697835 ) ) ;
#71946 = CARTESIAN_POINT ( 'NONE',  ( 190.1693911629507738, 301.2639477917662703, -5.112716700269980485 ) ) ;
#71947 = CARTESIAN_POINT ( 'NONE',  ( 34.38043361391329711, 31.80066082961424812, 10.00000000000000533 ) ) ;
#71948 = CARTESIAN_POINT ( 'NONE',  ( 181.7126073594628224, 294.1164641284040044, 6.307844905921689005 ) ) ;
#71949 = CARTESIAN_POINT ( 'NONE',  ( 173.2870411084388138, 273.4504758881469115, -16.94085204434761494 ) ) ;
#71950 = DIRECTION ( 'NONE',  ( -1.000000000000000000, 0.000000000000000000, 0.000000000000000000 ) ) ;
#71951 = CARTESIAN_POINT ( 'NONE',  ( 5.270092192305421364, 185.3967562850347122, -4.648177544792955347E-16 ) ) ;
#71952 = CARTESIAN_POINT ( 'NONE',  ( 77.46154149802761424, 203.9824982072973967, 3.021315404115420679E-15 ) ) ;
#71953 = CARTESIAN_POINT ( 'NONE',  ( 186.8150228009728835, 295.8650736363334204, -7.734513286467996629 ) ) ;
#71954 = DIRECTION ( 'NONE',  ( -0.1580495287025983631, -0.9874311856918873698, 0.000000000000000000 ) ) ;
#71955 = CARTESIAN_POINT ( 'NONE',  ( 87.63502826371536969, 214.7365022471901739, -10.00000000000009059 ) ) ;
#71956 = CARTESIAN_POINT ( 'NONE',  ( 70.21489987089526608, 66.74148169577378553, -10.42873902553350085 ) ) ;
#71957 = DIRECTION ( 'NONE',  ( -0.000000000000000000, -0.000000000000000000, 1.000000000000000000 ) ) ;
#71958 = CARTESIAN_POINT ( 'NONE',  ( 44.34243207491050498, 208.6589784336661637, -6.496448406907675876E-16 ) ) ;
#71959 = CARTESIAN_POINT ( 'NONE',  ( 159.2111180226792726, 254.8852497853115722, 16.01057445397460910 ) ) ;
#71960 = ORIENTED_EDGE ( 'NONE', *, *, #5199, .T. ) ;
#71961 = CARTESIAN_POINT ( 'NONE',  ( -15.89092471255436401, 83.83718066579119466, 14.94482985791953489 ) ) ;
#71962 = CARTESIAN_POINT ( 'NONE',  ( 198.5511052797322975, 286.7463930869835167, -17.24711022262289006 ) ) ;
#71963 = LINE ( 'NONE', #62327, #61197 ) ;
#71964 = ORIENTED_EDGE ( 'NONE', *, *, #13908, .F. ) ;
#71965 = DIRECTION ( 'NONE',  ( 0.8944271909999156334, 0.000000000000000000, -0.4472135954999582053 ) ) ;
#71966 = CARTESIAN_POINT ( 'NONE',  ( 168.0929298412453079, 282.0018323245688521, -10.93335134749426096 ) ) ;
#71967 = CARTESIAN_POINT ( 'NONE',  ( 81.17232691891707930, 55.55242957854174080, 16.36487835605631602 ) ) ;
#71968 = CARTESIAN_POINT ( 'NONE',  ( -19.79289719785049328, 93.08909491806775804, 59.99999999999999289 ) ) ;
#71969 = CARTESIAN_POINT ( 'NONE',  ( 29.15721111571870594, 19.76004757982090965, 5.678558825948272215 ) ) ;
#71970 = CARTESIAN_POINT ( 'NONE',  ( 162.7644741734472120, 248.7306563947940958, 9.865755277559742353 ) ) ;
#71971 = CARTESIAN_POINT ( 'NONE',  ( 149.1939152435731728, 272.2355539484436235, -11.44223522189843933 ) ) ;
#71972 = CARTESIAN_POINT ( 'NONE',  ( 171.4773364337628152, 255.5008831467121979, 12.42855810394174121 ) ) ;
#71973 = ORIENTED_EDGE ( 'NONE', *, *, #94328, .F. ) ;
#71974 = CARTESIAN_POINT ( 'NONE',  ( 15.84867609773810138, 11.01110640527290840, 2.839279412974134775 ) ) ;
#71975 = CARTESIAN_POINT ( 'NONE',  ( 171.9826536606966272, 253.0931212146789733, 8.466246838993372492 ) ) ;
#71976 = CARTESIAN_POINT ( 'NONE',  ( 71.63329245445480353, 72.42139875791372106, -1.350275132429440861 ) ) ;
#71977 = ORIENTED_EDGE ( 'NONE', *, *, #77665, .T. ) ;
#71978 = LINE ( 'NONE', #25359, #36868 ) ;
#71979 = CARTESIAN_POINT ( 'NONE',  ( 85.07250665400066225, 48.93453557688312117, 12.41781952940225153 ) ) ;
#71980 = CARTESIAN_POINT ( 'NONE',  ( 177.3283375316947286, 255.9921738663651354, -7.116718427656683943 ) ) ;
#71981 = DIRECTION ( 'NONE',  ( -0.5000000000000014433, 0.8660254037844378194, -0.000000000000000000 ) ) ;
#71982 = VECTOR ( 'NONE', #65405, 999.9999999999998863 ) ;
#71983 = ORIENTED_EDGE ( 'NONE', *, *, #68927, .T. ) ;
#71984 = ORIENTED_EDGE ( 'NONE', *, *, #27472, .T. ) ;
#71986 = CARTESIAN_POINT ( 'NONE',  ( 151.0575349784822947, 270.7509268893103354, -13.83753715545528173 ) ) ;
#71985 = CARTESIAN_POINT ( 'NONE',  ( -22.42236680055709641, 157.8615022471902591, 0.000000000000000000 ) ) ;
#71987 = ORIENTED_EDGE ( 'NONE', *, *, #88248, .F. ) ;
#71988 = CARTESIAN_POINT ( 'NONE',  ( 200.6680263064462792, 283.0797783131037022, -17.21821073473145347 ) ) ;
#71989 = CARTESIAN_POINT ( 'NONE',  ( 71.98264401366868981, 72.39816763649429276, -2.869464145551836598 ) ) ;
#71990 = CARTESIAN_POINT ( 'NONE',  ( 72.66110749420992931, 57.51441285064596087, -16.30982310438753657 ) ) ;
#71991 = CARTESIAN_POINT ( 'NONE',  ( 77.33488381500329467, 63.19222936695796733, 15.59520410795408196 ) ) ;
#71992 = CARTESIAN_POINT ( 'NONE',  ( 205.4103625296683617, 274.8658110279089897, -13.38953657917851814 ) ) ;
#71994 = CARTESIAN_POINT ( 'NONE',  ( 108.5637151982415389, 242.6744531367911293, 4.594050593750047540 ) ) ;
#71993 = VECTOR ( 'NONE', #77927, 1000.000000000000000 ) ;
#71995 = CARTESIAN_POINT ( 'NONE',  ( 79.15288444911743682, 228.0530062829863027, -4.648177544792955347E-16 ) ) ;
#71996 = EDGE_CURVE ( 'NONE', #82006, #25263, #11403, .T. ) ;
#71997 = VERTEX_POINT ( 'NONE', #73191 ) ;
#71998 = CARTESIAN_POINT ( 'NONE',  ( 208.1415148974628266, 270.1353163636768500, 3.453641150550738725 ) ) ;
#71999 = ORIENTED_EDGE ( 'NONE', *, *, #57502, .F. ) ;
#72000 = CARTESIAN_POINT ( 'NONE',  ( 31.43713336585798146, 20.01110640527293683, 2.839279412974134775 ) ) ;
#72001 = CARTESIAN_POINT ( 'NONE',  ( 157.1457301079645958, 258.8834783542900482, 16.87614098766286119 ) ) ;
#72002 = CARTESIAN_POINT ( 'NONE',  ( 78.41593629422656875, 47.90319055863865572, -14.51313888544015995 ) ) ;
#72003 = ADVANCED_FACE ( 'NONE', ( #73682 ), #67056, .F. ) ;
#72004 = CARTESIAN_POINT ( 'NONE',  ( 68.02342162723002161, 200.8923013555409796, 4.594050593750050204 ) ) ;
#72005 = CARTESIAN_POINT ( 'NONE',  ( 74.28707621773548908, 68.55768173149772338, 11.10544092197707755 ) ) ;
#72006 = CARTESIAN_POINT ( 'NONE',  ( 191.4922467593309250, 298.9726946877590876, 7.604184559945784017 ) ) ;
#72007 = CARTESIAN_POINT ( 'NONE',  ( 92.59663213601577070, 224.2677522451418497, 10.00000000000009592 ) ) ;
#72009 = B_SPLINE_CURVE_WITH_KNOTS ( 'NONE', 3,
 ( #82055, #5018, #57696, #65311, #12116, #27319 ),
 .UNSPECIFIED., .F., .F.,
 ( 4, 2, 4 ),
 ( 0.01870777577402827491, 0.02322058015305604461, 0.02773338453208381085 ),
 .UNSPECIFIED. ) ;
#72008 = DIRECTION ( 'NONE',  ( 0.02225111142181396620, 0.9997524133706775507, 0.000000000000000000 ) ) ;
#72010 = EDGE_LOOP ( 'NONE', ( #33987, #60228, #64252, #83717 ) ) ;
#72011 = CARTESIAN_POINT ( 'NONE',  ( 156.6812872898450735, 261.2670451491295012, 0.000000000000000000 ) ) ;
#72012 = CARTESIAN_POINT ( 'NONE',  ( 177.8473680943169484, 288.5077986257637122, 10.80235352749306621 ) ) ;
#72013 = CARTESIAN_POINT ( 'NONE',  ( 46.54103524584391494, 115.8319611975524595, 177.5919119679930134 ) ) ;
#72014 = EDGE_LOOP ( 'NONE', ( #47581, #92671, #43077, #3238 ) ) ;
#72015 = CARTESIAN_POINT ( 'NONE',  ( 101.3989120123781191, 240.8967562850346837, -4.648177544792955347E-16 ) ) ;
#72016 = CARTESIAN_POINT ( 'NONE',  ( 173.8371423854052580, 278.0697674778426176, -16.44858265900196770 ) ) ;
#72017 = EDGE_CURVE ( 'NONE', #19430, #54490, #98817, .T. ) ;
#72018 = CARTESIAN_POINT ( 'NONE',  ( 161.0965315767822972, 251.6196177163260188, -13.76772246540905442 ) ) ;
#72019 = CARTESIAN_POINT ( 'NONE',  ( 206.4708747408093643, 270.6173459074702805, 2.419506436698913188 ) ) ;
#72020 = CARTESIAN_POINT ( 'NONE',  ( 149.3883679478359454, 271.8987519849911223, 12.99187507659642371 ) ) ;
#72021 = CARTESIAN_POINT ( 'NONE',  ( 177.2096423064392070, 269.5159051785426527, 16.11451641950014491 ) ) ;
#72022 = VECTOR ( 'NONE', #91163, 1000.000000000000227 ) ;
#72023 = DIRECTION ( 'NONE',  ( -0.8660254037844387076, -0.4999999999999998890, -0.000000000000000000 ) ) ;
#72024 = CARTESIAN_POINT ( 'NONE',  ( 68.91022223105564137, 64.71151235087043574, -12.22836756590942464 ) ) ;
#72025 = CARTESIAN_POINT ( 'NONE',  ( 167.9973872756363562, 255.7907068641800379, 13.67785959516219130 ) ) ;
#72026 = CYLINDRICAL_SURFACE ( 'NONE', #90143, 17.82106496071139645 ) ;
#72027 = CARTESIAN_POINT ( 'NONE',  ( 110.0256537107753161, 225.1423013555409796, -4.594050593750043987 ) ) ;
#72028 = ORIENTED_EDGE ( 'NONE', *, *, #15084, .T. ) ;
#72029 = CARTESIAN_POINT ( 'NONE',  ( 85.05810897262044534, 44.16933612965711831, -6.971008100970949251 ) ) ;
#72030 = CARTESIAN_POINT ( 'NONE',  ( 92.93397336236306217, 212.9155109091896065, 2.679491924311254714 ) ) ;
#72031 = CARTESIAN_POINT ( 'NONE',  ( -79.43448886220070904, 56.15136215343108717, -10.00000000000000000 ) ) ;
#72032 = EDGE_CURVE ( 'NONE', #54142, #62846, #97021, .T. ) ;
#72033 = CARTESIAN_POINT ( 'NONE',  ( 183.2230023984259333, 284.8711938070701990, -14.93434685926643013 ) ) ;
#72034 = CARTESIAN_POINT ( 'NONE',  ( 83.46712633478475141, 51.63463124265641824, -14.88389777197023456 ) ) ;
#72035 = CARTESIAN_POINT ( 'NONE',  ( 76.06472804764035800, 51.19927304191299555, -15.61780489609254197 ) ) ;
#72036 = ORIENTED_EDGE ( 'NONE', *, *, #18521, .F. ) ;
#72037 = CARTESIAN_POINT ( 'NONE',  ( 80.46882139176624094, 57.60428850591405592, -16.59250918983046574 ) ) ;
#72038 = CARTESIAN_POINT ( 'NONE',  ( 157.3661001067102916, 274.3687252322818040, -12.59994636575860838 ) ) ;
#72039 = CARTESIAN_POINT ( 'NONE',  ( 185.8872707255410432, 262.0278434869816238, 9.890274748944476002 ) ) ;
#72040 = LINE ( 'NONE', #10236, #73505 ) ;
#72041 = CARTESIAN_POINT ( 'NONE',  ( 147.1836429658426368, 243.5327760586659451, 1.948934522072302763E-15 ) ) ;
#72042 = CARTESIAN_POINT ( 'NONE',  ( -74.97640825042664403, 52.25402898078436920, -10.00000000000000000 ) ) ;
#72043 = CARTESIAN_POINT ( 'NONE',  ( 24.79662394327660024, 66.59991831601136880, 59.99999999999999289 ) ) ;
#72044 = DIRECTION ( 'NONE',  ( -0.5000000000000006661, 0.8660254037844382635, -1.877843081442121204E-16 ) ) ;
#72045 = CARTESIAN_POINT ( 'NONE',  ( 54.35602435405059651, 208.3149278399161233, -9.188101187500095079 ) ) ;
#72046 = CARTESIAN_POINT ( 'NONE',  ( 164.8670003495851404, 245.0889742334797177, -1.557028074864921674 ) ) ;
#72047 = CARTESIAN_POINT ( 'NONE',  ( 191.5083466856444261, 297.3227120659499292, 10.96045759559922317 ) ) ;
#72048 = EDGE_CURVE ( 'NONE', #95936, #94224, #38300, .T. ) ;
#72049 = CARTESIAN_POINT ( 'NONE',  ( 69.19930876265073039, 70.42046229790001632, -2.224448151379176508 ) ) ;
#72050 = CARTESIAN_POINT ( 'NONE',  ( 199.9134407114337364, 283.6250491837689651, 17.05367660732407842 ) ) ;
#72051 = LINE ( 'NONE', #2654, #49908 ) ;
#72052 = CARTESIAN_POINT ( 'NONE',  ( 169.4088087987535687, 285.0667569032603410, -8.267254425861240819 ) ) ;
#72053 = CARTESIAN_POINT ( 'NONE',  ( 155.2922060645262263, 261.6730044072216401, -16.98884022075611355 ) ) ;
#72054 = LINE ( 'NONE', #33548, #83893 ) ;
#72055 = ADVANCED_FACE ( 'NONE', ( #12894 ), #19508, .T. ) ;
#72056 = CARTESIAN_POINT ( 'NONE',  ( 131.1347626044233152, 236.5177522451417929, 5.000000000000051514 ) ) ;
#72057 = B_SPLINE_SURFACE_WITH_KNOTS ( 'NONE', 3, 1, ( 
 ( #71946, #41516 ),
 ( #79578, #50610 ),
 ( #27826, #58702 ),
 ( #3550, #27337 ),
 ( #12135, #26833 ),
 ( #42997, #4521 ),
 ( #42024, #42506 ),
 ( #73442, #72958 ),
 ( #28312, #81080 ),
 ( #4026, #5033 ),
 ( #34428, #89197 ),
 ( #49623, #95785 ),
 ( #11646, #96267 ),
 ( #26339, #13141 ),
 ( #57215, #96771 ),
 ( #19745, #65328 ),
 ( #72460, #57711 ),
 ( #58218, #88691 ),
 ( #89676, #88190 ),
 ( #34912, #19261 ),
 ( #59190, #43514 ),
 ( #65810, #73935 ),
 ( #20237, #35422 ),
 ( #81564, #50128 ),
 ( #66327, #97259 ),
 ( #51109, #33951 ),
 ( #82074, #12644 ),
 ( #74453, #35915 ),
 ( #66816, #97744 ),
 ( #18739, #90166 ),
 ( #20739, #51626 ),
 ( #82578, #3065 ),
 ( #64838, #80577 ),
 ( #11157, #7504 ) ),
 .UNSPECIFIED., .T., .F., .F.,
 ( 4, 2, 2, 2, 2, 2, 2, 2, 2, 2, 2, 2, 2, 2, 2, 2, 4 ),
 ( 2, 2 ),
 ( 0.000000000000000000, 0.06250000000000000000, 0.1250000000000000000, 0.1875000000000000000, 0.2500000000000000000, 0.3125000000000000000, 0.3750000000000000000, 0.4375000000000000000, 0.5000000000000000000, 0.5625000000000000000, 0.6250000000000000000, 0.6875000000000000000, 0.7500000000000000000, 0.8125000000000000000, 0.8750000000000000000, 0.9375000000000000000, 1.000000000000000000 ),
 ( 0.000000000000000000, 1.000000000000000000 ),
 .UNSPECIFIED. ) ;
#72058 = CARTESIAN_POINT ( 'NONE',  ( 80.74219536503451877, 51.86096535971582000, -15.10915280358188895 ) ) ;
#72059 = ORIENTED_EDGE ( 'NONE', *, *, #95683, .F. ) ;
#72060 = B_SPLINE_CURVE_WITH_KNOTS ( 'NONE', 3,
 ( #64634, #66120, #97069, #27640, #79375, #41811, #34227, #40801, #34715, #42796, #27137, #72759, #57010, #95586, #41304, #35218, #18039, #65615, #71746, #96570, #96070, #11940, #87989, #58022, #25635, #9938, #65123, #89004, #73730, #57512, #18538, #86990, #56517, #19554, #81372, #26628, #19050, #3351, #88488, #50414, #49421, #4314, #3830, #2339, #17520, #33222 ),
 .UNSPECIFIED., .F., .F.,
 ( 4, 1, 2, 2, 1, 2, 2, 1, 1, 2, 2, 1, 1, 2, 2, 1, 1, 2, 2, 1, 1, 1, 2, 2, 1, 1, 1, 2, 2, 4 ),
 ( 0.000000000000000000, 0.06249999999999249212, 0.09374999999998884226, 0.1249999999999852063, 0.1874999999999779066, 0.2187499999999762135, 0.2499999999999745204, 0.3124999999999669709, 0.3437499999999650280, 0.3593749999999655831, 0.3749999999999661382, 0.4374999999999704681, 0.4687499999999723554, 0.4843749999999731881, 0.4999999999999740208, 0.5624999999999785727, 0.5937499999999806821, 0.6093749999999837907, 0.6249999999999868994, 0.6874999999999896749, 0.7187499999999907851, 0.7343749999999892308, 0.7421874999999884537, 0.7499999999999876765, 0.8124999999999982236, 0.8437500000000037748, 0.8593750000000081046, 0.8671875000000084377, 0.8750000000000086597, 1.000000000000000000 ),
 .UNSPECIFIED. ) ;
#72061 = EDGE_CURVE ( 'NONE', #86304, #11813, #80721, .T. ) ;
#72062 = CARTESIAN_POINT ( 'NONE',  ( -15.10528209597770299, 24.46087392797020499, -10.00000000000000000 ) ) ;
#72063 = CARTESIAN_POINT ( 'NONE',  ( 17.03907575219864867, 18.03677371833801146, 10.00000000000000533 ) ) ;
#72064 = B_SPLINE_CURVE_WITH_KNOTS ( 'NONE', 3,
 ( #4666, #66458, #97383, #44628, #27950, #58832, #20372, #51243, #5163, #66943, #28446, #59326, #90306, #16242, #23330, #37531, #93788, #1050, #69930, #39022, #60819, #68436, #30940, #91781, #52730, #92291, #15731, #61331, #99365, #38021, #69439 ),
 .UNSPECIFIED., .F., .F.,
 ( 4, 3, 3, 3, 3, 3, 3, 3, 3, 3, 4 ),
 ( 0.000000000000000000, 0.1333490885032285189, 0.3007194338854188853, 0.4699862290244924967, 0.5844252810809184018, 0.6686540514502693489, 0.7354980260655538116, 0.8028463152565737948, 0.8633854507757268149, 0.9437142632667515629, 1.000000000000000000 ),
 .UNSPECIFIED. ) ;
#72065 = CARTESIAN_POINT ( 'NONE',  ( 43.96406660440233338, 190.0643266524159571, -9.188101187500093303 ) ) ;
#72066 = CARTESIAN_POINT ( 'NONE',  ( 23.96727898247415212, 22.03677371833801857, 10.00000000000000533 ) ) ;
#72067 = CARTESIAN_POINT ( 'NONE',  ( 41.14028939449039513, 187.8927522451418213, 10.00000000000009948 ) ) ;
#72068 = CARTESIAN_POINT ( 'NONE',  ( 82.63770679579928924, 49.15890594283347781, -13.91020417536396003 ) ) ;
#72069 = CARTESIAN_POINT ( 'NONE',  ( 190.8957779480239765, 300.0058089740729770, -4.541438514207768229 ) ) ;
#72070 = CARTESIAN_POINT ( 'NONE',  ( 72.18677484676699407, 72.08588332058079118, 3.002544651710248758 ) ) ;
#72071 = EDGE_CURVE ( 'NONE', #43154, #100075, #35164, .T. ) ;
#72073 = CARTESIAN_POINT ( 'NONE',  ( 53.62548896571601631, 201.7677522451418781, 10.00000000000009592 ) ) ;
#72072 = DIRECTION ( 'NONE',  ( 0.2803049773603249473, -0.9599109957006575211, 0.000000000000000000 ) ) ;
#72074 = ADVANCED_FACE ( 'NONE', ( #19982 ), #65074, .T. ) ;
#72075 = CARTESIAN_POINT ( 'NONE',  ( 174.5898090886373097, 289.3010444735929809, 7.825388048759662318 ) ) ;
#72076 = DIRECTION ( 'NONE',  ( -0.5000000000000019984, 0.8660254037844374864, 0.000000000000000000 ) ) ;
#72077 = CARTESIAN_POINT ( 'NONE',  ( 157.8239779013331372, 257.2878469527003062, -17.92251383114021479 ) ) ;
#72078 = CARTESIAN_POINT ( 'NONE',  ( 162.1762925668143396, 251.9858117565144084, -13.16816576803558014 ) ) ;
#72079 =( BOUNDED_CURVE ( )  B_SPLINE_CURVE ( 2, ( #80553, #42000, #49110, #33406, #46208, #32405, #63804, #3039, #33929 ),
 .UNSPECIFIED., .F., .T. ) 
 B_SPLINE_CURVE_WITH_KNOTS ( ( 3, 2, 2, 2, 3 ),
 ( 0.7862903225806451291, 0.7876344086021505042, 0.7903225806451612545, 0.7930107526881720048, 0.7943548387096773800 ),
 .UNSPECIFIED. ) 
 CURVE ( )  GEOMETRIC_REPRESENTATION_ITEM ( )  RATIONAL_B_SPLINE_CURVE ( ( 0.9330127018922194093, 0.9330127018922194093, 1.000000000000000000, 0.8660254037844387076, 1.000000000000000000, 0.8660254037844387076, 1.000000000000000000, 0.9330127018922194093, 0.9330127018922194093 ) ) 
 REPRESENTATION_ITEM ( '' )  );
#72080 = CARTESIAN_POINT ( 'NONE',  ( 38.99326808448932979, 199.9865022471902876, 10.00000000000009237 ) ) ;
#72081 = CARTESIAN_POINT ( 'NONE',  ( 156.6812872898450735, 261.2670451491295012, 0.000000000000000000 ) ) ;
#72082 = CARTESIAN_POINT ( 'NONE',  ( 202.5245888501533216, 279.8641176599742266, 15.60152447840272494 ) ) ;
#72083 = CARTESIAN_POINT ( 'NONE',  ( -7.619092152155812592, 178.6589784336661637, -6.496448406907675876E-16 ) ) ;
#72084 = CARTESIAN_POINT ( 'NONE',  ( 34.12723495145388597, 35.10171378149922106, 9.188101187500008038 ) ) ;
#72086 = CARTESIAN_POINT ( 'NONE',  ( 200.4065898033495046, 283.0201594895918333, 16.80763448860258791 ) ) ;
#72085 = CARTESIAN_POINT ( 'NONE',  ( -61.68394390806074057, 53.17837850769589636, 59.99999999999999289 ) ) ;
#72087 = CARTESIAN_POINT ( 'NONE',  ( 192.0331311261993790, 298.0358554833232461, 11.82583305898340953 ) ) ;
#72088 = CARTESIAN_POINT ( 'NONE',  ( 32.92443518896833154, 39.98502408145596121, -5.678558825948271327 ) ) ;
#72089 = CARTESIAN_POINT ( 'NONE',  ( 155.5606021264401875, 261.5901729271447493, -16.99161892237499671 ) ) ;
#72090 = CARTESIAN_POINT ( 'NONE',  ( 183.8754313647489198, 256.5225093191261294, -2.022205659181245174 ) ) ;
#72091 = DIRECTION ( 'NONE',  ( 0.000000000000000000, -0.000000000000000000, 1.000000000000000000 ) ) ;
#72092 = CARTESIAN_POINT ( 'NONE',  ( 43.32193544081557945, 25.41603393254330001, -1.583844403245396437 ) ) ;
#72093 = DIRECTION ( 'NONE',  ( 0.4999999999999998890, -0.8660254037844385966, 0.000000000000000000 ) ) ;
#72094 =( LENGTH_UNIT ( ) NAMED_UNIT ( * ) SI_UNIT ( .MILLI., .METRE. ) );
#72095 = CARTESIAN_POINT ( 'NONE',  ( 8.534987971495436199, 16.87878583063839599, -9.188101187500006262 ) ) ;
#72096 = CARTESIAN_POINT ( 'NONE',  ( 153.5867603639496508, 277.8595165095850916, -5.207415017408751901 ) ) ;
#72097 = CARTESIAN_POINT ( 'NONE',  ( 19.63753723929501760, 13.19860640527291551, 2.839279412974134775 ) ) ;
#72098 = CARTESIAN_POINT ( 'NONE',  ( 75.87151652897675547, 204.6115022471901739, -5.000000000000041744 ) ) ;
#72099 = VECTOR ( 'NONE', #2006, 1000.000000000000114 ) ;
#72100 = CARTESIAN_POINT ( 'NONE',  ( 84.60739412327551179, 49.90025452092439906, -13.66407646797534703 ) ) ;
#72101 = CARTESIAN_POINT ( 'NONE',  ( 159.6962080797732710, 254.0450491601782232, -15.33973334987084947 ) ) ;
#72102 = VERTEX_POINT ( 'NONE', #26586 ) ;
#72104 = CARTESIAN_POINT ( 'NONE',  ( 192.5254593562406171, 297.1831179748913314, 11.00703791256144015 ) ) ;
#72103 =( BOUNDED_CURVE ( )  B_SPLINE_CURVE ( 2, ( #64455, #62428, #25449, #17869, #63453, #17346, #40131, #1672, #56338 ),
 .UNSPECIFIED., .F., .T. ) 
 B_SPLINE_CURVE_WITH_KNOTS ( ( 3, 2, 2, 2, 3 ),
 ( 0.5524193548387096309, 0.5537634408602150060, 0.5564516129032257563, 0.5591397849462365066, 0.5604838709677418818 ),
 .UNSPECIFIED. ) 
 CURVE ( )  GEOMETRIC_REPRESENTATION_ITEM ( )  RATIONAL_B_SPLINE_CURVE ( ( 0.9330127018922194093, 0.9330127018922194093, 1.000000000000000000, 0.8660254037844387076, 1.000000000000000000, 0.8660254037844387076, 1.000000000000000000, 0.9330127018922194093, 0.9330127018922194093 ) ) 
 REPRESENTATION_ITEM ( '' )  );
#72105 = CARTESIAN_POINT ( 'NONE',  ( 164.2953672501826929, 246.0790718049323687, -2.576662677987826111 ) ) ;
#72106 = CIRCLE ( 'NONE', #54265, 70.00000000000001421 ) ;
#72107 = CARTESIAN_POINT ( 'NONE',  ( 66.05163167928934342, 68.53992083822487302, 4.515471496088387049 ) ) ;
#72108 = CARTESIAN_POINT ( 'NONE',  ( 87.47489022187491514, 45.51477803643930287, 7.025279742117177761 ) ) ;
#72109 = CARTESIAN_POINT ( 'NONE',  ( 154.9683083969241011, 262.2340116239618055, 18.33261662430134109 ) ) ;
#72110 = EDGE_LOOP ( 'NONE', ( #70345, #11872, #93563, #96298 ) ) ;
#72111 = VERTEX_POINT ( 'NONE', #96023 ) ;
#72112 = CARTESIAN_POINT ( 'NONE',  ( 85.90360539940944307, 47.54977701528212464, 10.84765075726303785 ) ) ;
#72113 = ORIENTED_EDGE ( 'NONE', *, *, #5138, .F. ) ;
#72114 = CARTESIAN_POINT ( 'NONE',  ( 77.85016660199350724, 58.06595483709381256, 16.16712961033420015 ) ) ;
#72115 = CARTESIAN_POINT ( 'NONE',  ( -16.76269525828470464, 104.2312461070085021, 45.19948692389422717 ) ) ;
#72116 = ORIENTED_EDGE ( 'NONE', *, *, #45370, .F. ) ;
#72117 = DIRECTION ( 'NONE',  ( -0.9994626398093606756, -0.03277852384266338737, 0.000000000000000000 ) ) ;
#72118 = CARTESIAN_POINT ( 'NONE',  ( 79.25252407528778065, 59.49743072449278714, -16.53464936128686347 ) ) ;
#72119 = CARTESIAN_POINT ( 'NONE',  ( 82.85318063129575705, 47.73104734800577376, -12.93175278804887185 ) ) ;
#72120 = CARTESIAN_POINT ( 'NONE',  ( 80.48263234248918252, 43.57791934932684796, 9.754260794015122471 ) ) ;
#72121 = ORIENTED_EDGE ( 'NONE', *, *, #99957, .T. ) ;
#72122 = CARTESIAN_POINT ( 'NONE',  ( 200.4403816905005158, 283.4740703539914648, 16.81798557643505987 ) ) ;
#72123 = CARTESIAN_POINT ( 'NONE',  ( 166.8997956679749564, 274.6136247820161316, -15.18620604814603503 ) ) ;
#72124 = CARTESIAN_POINT ( 'NONE',  ( 16.05454730341465464, 46.50537555954188917, 59.99999999999999289 ) ) ;
#72125 = DIRECTION ( 'NONE',  ( 1.000000000000000000, 0.000000000000000000, 0.000000000000000000 ) ) ;
#72126 = ORIENTED_EDGE ( 'NONE', *, *, #19669, .F. ) ;
#72127 = CARTESIAN_POINT ( 'NONE',  ( 173.8258004643798245, 257.2059766620726009, -11.79308939057215255 ) ) ;
#72128 = FACE_OUTER_BOUND ( 'NONE', #83627, .T. ) ;
#72129 = ORIENTED_EDGE ( 'NONE', *, *, #76964, .T. ) ;
#72130 = ORIENTED_EDGE ( 'NONE', *, *, #45812, .T. ) ;
#72131 = CARTESIAN_POINT ( 'NONE',  ( 159.8820994310810022, 268.4908852645613706, -16.43388976517952571 ) ) ;
#72132 = AXIS2_PLACEMENT_3D ( 'NONE', #17717, #11624, #49599 ) ;
#72133 = ORIENTED_EDGE ( 'NONE', *, *, #3337, .F. ) ;
#72134 = CARTESIAN_POINT ( 'NONE',  ( 80.86586985908986946, 155.7185146834693512, 0.000000000000000000 ) ) ;
#72135 = ORIENTED_EDGE ( 'NONE', *, *, #92872, .F. ) ;
#72136 = DIRECTION ( 'NONE',  ( 0.4386133837897796539, 0.6599160945941811018, -0.6100238090894840592 ) ) ;
#72137 = CARTESIAN_POINT ( 'NONE',  ( 193.9762986263216646, 294.6701906454947562, 14.66460157377692042 ) ) ;
#72138 = CARTESIAN_POINT ( 'NONE',  ( 176.9659610627589359, 289.4039066173891115, -10.56313750161503151 ) ) ;
#72140 = CARTESIAN_POINT ( 'NONE',  ( 69.50297104555633609, 65.22433265006822012, 11.43951683047897205 ) ) ;
#72139 = B_SPLINE_CURVE_WITH_KNOTS ( 'NONE', 3,
 ( #47184, #24886, #62884, #78612, #40575, #40071, #86755, #34017, #17288, #71014, #1616, #32987, #79640, #16788, #63393, #56786, #26404, #32502, #9720, #17807, #94333, #10207, #78105, #8695, #55270, #64396, #18308, #95359, #86250, #48192, #16290, #48707, #87277, #79139, #87770, #31980, #71516, #39564, #2106, #10705, #70488, #25914, #80140, #3132 ),
 .UNSPECIFIED., .F., .F.,
 ( 4, 2, 2, 2, 2, 2, 2, 2, 2, 2, 2, 2, 2, 2, 2, 2, 2, 2, 2, 2, 2, 4 ),
 ( 0.0004122447795833745587, 0.001425156861282679847, 0.001931612902132293650, 0.002184840922557164736, 0.002311454932769600387, 0.002438068942982036039, 0.002691296963406946807, 0.002944524983831857574, 0.003450981024681599313, 0.004463893106381080188, 0.005476805188080561063, 0.005983261228930296730, 0.006236489249355129001, 0.006489717269779959538, 0.006553024274886150476, 0.006616331279992340546, 0.006679638285098531483, 0.006742945290204721553, 0.006996173310629566836, 0.007502629351479299900, 0.008009085392329034700, 0.008515541433178768632 ),
 .UNSPECIFIED. ) ;
#72141 = CARTESIAN_POINT ( 'NONE',  ( 193.3011194324739961, 295.0724505835075320, 13.25748537430616381 ) ) ;
#72142 = EDGE_CURVE ( 'NONE', #61085, #65492, #80835, .T. ) ;
#72143 = CARTESIAN_POINT ( 'NONE',  ( 175.2538527669093753, 291.0550713335976525, 6.537906992358419878 ) ) ;
#72144 = FACE_OUTER_BOUND ( 'NONE', #57516, .T. ) ;
#72145 = EDGE_LOOP ( 'NONE', ( #4597, #63633, #47116, #29649 ) ) ;
#72146 = CARTESIAN_POINT ( 'NONE',  ( -50.19188543474569997, 43.82156839606978593, 59.99999999999999289 ) ) ;
#72147 = CARTESIAN_POINT ( 'NONE',  ( 16.40018271037384068, 27.65586893147755987, -7.433330006724137462 ) ) ;
#72148 = CARTESIAN_POINT ( 'NONE',  ( 206.1932826529868805, 273.5097535960530877, 11.72208607728249241 ) ) ;
#72149 = CARTESIAN_POINT ( 'NONE',  ( 206.3505875407052486, 273.2372935382459787, 11.62318091048137880 ) ) ;
#72151 = ORIENTED_EDGE ( 'NONE', *, *, #9491, .F. ) ;
#72150 = DIRECTION ( 'NONE',  ( 1.000000000000000000, 0.000000000000000000, 0.000000000000000000 ) ) ;
#72152 = ORIENTED_EDGE ( 'NONE', *, *, #73646, .T. ) ;
#72153 = B_SPLINE_CURVE_WITH_KNOTS ( 'NONE', 3,
 ( #61170, #22691, #45957, #76874 ),
 .UNSPECIFIED., .F., .F.,
 ( 4, 4 ),
 ( 0.01224253334696489767, 0.01843315522474755358 ),
 .UNSPECIFIED. ) ;
#72154 = CARTESIAN_POINT ( 'NONE',  ( 146.7209331427380050, 276.5188845932982531, -2.966446756160787679 ) ) ;
#72155 = CARTESIAN_POINT ( 'NONE',  ( 80.91225347342312091, 52.52757887018025684, -15.32176213838356738 ) ) ;
#72156 = DIRECTION ( 'NONE',  ( -0.8660254037844387076, -0.4999999999999998890, -0.000000000000000000 ) ) ;
#72157 = EDGE_CURVE ( 'NONE', #82522, #56639, #95258, .T. ) ;
#72158 = CYLINDRICAL_SURFACE ( 'NONE', #53804, 6.749999999999988454 ) ;
#72159 = EDGE_CURVE ( 'NONE', #99538, #67236, #90409, .T. ) ;
#72160 = CARTESIAN_POINT ( 'NONE',  ( 189.4381674897702794, 265.0040801212285828, 12.03645615491573828 ) ) ;
#72161 = DIRECTION ( 'NONE',  ( 0.000000000000000000, -0.000000000000000000, 1.000000000000000000 ) ) ;
#72162 = ORIENTED_EDGE ( 'NONE', *, *, #99095, .F. ) ;
#72163 = CARTESIAN_POINT ( 'NONE',  ( -22.42236680055709641, 157.8615022471902591, 0.000000000000000000 ) ) ;
#72164 = CYLINDRICAL_SURFACE ( 'NONE', #84046, 16.60714546451156792 ) ;
#72165 = CARTESIAN_POINT ( 'NONE',  ( 49.80054343233477709, 192.8927522451417929, -10.00000000000009237 ) ) ;
#72166 = CARTESIAN_POINT ( 'NONE',  ( 207.4285356523023154, 271.3702326410368642, 7.833982582429932506 ) ) ;
#72167 = CARTESIAN_POINT ( 'NONE',  ( 16.02555268474158723, 193.3927522451419350, 2.944929066748280225E-16 ) ) ;
#72168 = CARTESIAN_POINT ( 'NONE',  ( 97.84665082640911749, 236.4869531367911293, 4.594050593750046652 ) ) ;
#72169 = CARTESIAN_POINT ( 'NONE',  ( 82.65268600941737986, 40.56492479297515530, -1.423195747375628928 ) ) ;
#72170 = CARTESIAN_POINT ( 'NONE',  ( 173.3920276507685401, 289.7572511702507541, -7.189583706006478891 ) ) ;
#72171 = CARTESIAN_POINT ( 'NONE',  ( 207.6964130646365163, 270.9062553526738384, 2.975933372805272814 ) ) ;
#72172 = CARTESIAN_POINT ( 'NONE',  ( 26.56245542105003210, 176.9548013555409796, -4.594050593750042211 ) ) ;
#72173 = VECTOR ( 'NONE', #15050, 1000.000000000000114 ) ;
#72174 = DIRECTION ( 'NONE',  ( -0.9682419296822714072, -0.2500151307524236532, 0.000000000000000000 ) ) ;
#72175 = ORIENTED_EDGE ( 'NONE', *, *, #36113, .F. ) ;
#72176 = ORIENTED_EDGE ( 'NONE', *, *, #73839, .T. ) ;
#72177 = CARTESIAN_POINT ( 'NONE',  ( 200.4912881644965807, 267.5564725962747161, -2.850958659151126007 ) ) ;
#72178 = CARTESIAN_POINT ( 'NONE',  ( 69.25966472908447713, 70.58289072661317221, 0.9580429418411622322 ) ) ;
#72179 = VECTOR ( 'NONE', #65910, 1000.000000000000000 ) ;
#72180 = CARTESIAN_POINT ( 'NONE',  ( 33.43624804430746877, 19.70852965304480620, 1.583844403245330712 ) ) ;
#72181 = CARTESIAN_POINT ( 'NONE',  ( 192.9756790785140765, 263.8394000145765972, -4.280765219900059648 ) ) ;
#72182 = CARTESIAN_POINT ( 'NONE',  ( 161.2488013048736377, 251.3558788108169040, -13.10044423494716170 ) ) ;
#72183 = CARTESIAN_POINT ( 'NONE',  ( 68.52907269813512414, 64.25491985315194654, 11.77327033154230840 ) ) ;
#72184 = CARTESIAN_POINT ( 'NONE',  ( 167.3696659777530158, 251.6663404442222713, 10.32696327628674915 ) ) ;
#72185 = EDGE_CURVE ( 'NONE', #79646, #45796, #2669, .T. ) ;
#72186 = CARTESIAN_POINT ( 'NONE',  ( 42.47567221558909267, 186.1423013555410080, -4.594050593750043987 ) ) ;
#72187 = CARTESIAN_POINT ( 'NONE',  ( 82.70950877614343710, 211.8927522451418213, 10.00000000000009592 ) ) ;
#72188 = ORIENTED_EDGE ( 'NONE', *, *, #31033, .T. ) ;
#72189 = CARTESIAN_POINT ( 'NONE',  ( 79.31708208686120543, 59.64451620468175719, -16.52545681491535134 ) ) ;
#72190 = EDGE_CURVE ( 'NONE', #10543, #39006, #39467, .T. ) ;
#72191 = EDGE_CURVE ( 'NONE', #11457, #61620, #72103, .T. ) ;
#72192 = CARTESIAN_POINT ( 'NONE',  ( 179.3683703725943417, 258.0455820962152984, -10.44019545301878082 ) ) ;
#72193 = CARTESIAN_POINT ( 'NONE',  ( -5.237175195983594378, 167.7833772461660828, -9.188101187500095079 ) ) ;
#72194 = EDGE_CURVE ( 'NONE', #47356, #5374, #23437, .T. ) ;
#72195 = CARTESIAN_POINT ( 'NONE',  ( 68.90356118335428448, 64.71243317138014106, -12.22457433626360945 ) ) ;
#72196 = CARTESIAN_POINT ( 'NONE',  ( 151.3898985249405200, 268.4319993325432847, -14.65018536945715510 ) ) ;
#72197 = VECTOR ( 'NONE', #53578, 1000.000000000000000 ) ;
#72198 = CARTESIAN_POINT ( 'NONE',  ( 186.1163208250084438, 283.4177454897106259, 16.70810301636890571 ) ) ;
#72199 = CARTESIAN_POINT ( 'NONE',  ( 147.5381343315788172, 275.1034506142203782, -4.056595942992749393 ) ) ;
#72200 = ADVANCED_FACE ( 'NONE', ( #93390 ), #8752, .F. ) ;
#72201 = LINE ( 'NONE', #96026, #8699 ) ;
#72202 = CARTESIAN_POINT ( 'NONE',  ( 164.2413944571582078, 246.1725554246774834, 7.304616466633322425 ) ) ;
#72203 = CARTESIAN_POINT ( 'NONE',  ( 147.2592533090473239, 275.5864867145116932, -0.3770461397900867762 ) ) ;
#72204 = CARTESIAN_POINT ( 'NONE',  ( 164.7243055739305078, 245.3361288348881999, -1.445094907380085170 ) ) ;
#72205 = ORIENTED_EDGE ( 'NONE', *, *, #15399, .T. ) ;
#72206 = CIRCLE ( 'NONE', #34923, 70.00000000000001421 ) ;
#72207 = CARTESIAN_POINT ( 'NONE',  ( 4.352251933111862314, 159.9865022471901739, 1.119607411625061291E-15 ) ) ;
#72208 = CARTESIAN_POINT ( 'NONE',  ( 143.4214980241629576, 243.6115022471902023, -5.000000000000041744 ) ) ;
#72209 = CARTESIAN_POINT ( 'NONE',  ( 132.2986577904150920, 241.0643266524159856, -9.188101187500093303 ) ) ;
#72210 = CARTESIAN_POINT ( 'NONE',  ( 18.45699304436188015, 28.84336893147756342, -7.433330006724137462 ) ) ;
#72211 = CARTESIAN_POINT ( 'NONE',  ( 80.15404930735284950, 58.24487849859603017, -16.60713908503101877 ) ) ;
#72212 = CARTESIAN_POINT ( 'NONE',  ( 151.0474090540779741, 270.2368430214293653, 13.84391263241849934 ) ) ;
#72214 = CARTESIAN_POINT ( 'NONE',  ( 141.9699493749754140, 259.7505386000626686, -7.968025677899344572 ) ) ;
#72213 = CARTESIAN_POINT ( 'NONE',  ( 195.8947060313465443, 291.3474115503753410, 16.07878593000791767 ) ) ;
#72215 = CARTESIAN_POINT ( 'NONE',  ( 191.0469974725420172, 299.7438890745112872, -6.451222553760779910 ) ) ;
#72216 = EDGE_LOOP ( 'NONE', ( #87402, #62478, #36057, #50297, #74881 ) ) ;
#72217 = CARTESIAN_POINT ( 'NONE',  ( 192.9845471803554346, 263.7469009655502532, -5.013485419990833414 ) ) ;
#72218 = CARTESIAN_POINT ( 'NONE',  ( 196.8363552541316324, 289.7164272536036265, -17.80258609350122967 ) ) ;
#72219 = CARTESIAN_POINT ( 'NONE',  ( 187.4784686605442232, 261.8693247467304559, 9.829215920296768161 ) ) ;
#72220 = LINE ( 'NONE', #64606, #33788 ) ;
#72221 = CARTESIAN_POINT ( 'NONE',  ( 81.55294353520883988, 55.93325196641738017, -16.02942048421892096 ) ) ;
#72222 = EDGE_LOOP ( 'NONE', ( #84982, #49909, #90740, #9572 ) ) ;
#72223 = CARTESIAN_POINT ( 'NONE',  ( 69.02380705549570905, 66.01831451487439040, -11.15343670725473402 ) ) ;
#72224 = CARTESIAN_POINT ( 'NONE',  ( 175.1874290394435434, 279.2259713227149973, 15.64062928220176474 ) ) ;
#72225 = CARTESIAN_POINT ( 'NONE',  ( 168.8736724576156405, 271.8586482977812011, -16.82536904539195532 ) ) ;
#72226 = CARTESIAN_POINT ( 'NONE',  ( 71.95794525336513914, 72.58301972798901147, 1.600903759350535749 ) ) ;
#72227 = CARTESIAN_POINT ( 'NONE',  ( 80.09789180664904507, 54.17278058467296376, 15.81966211497349484 ) ) ;
#72228 = CARTESIAN_POINT ( 'NONE',  ( 83.91681368584680456, 51.76886007642450949, -14.44478906560582310 ) ) ;
#72229 = CARTESIAN_POINT ( 'NONE',  ( 87.04122873496829982, 46.31593380912285340, -9.298662157179387933 ) ) ;
#72230 = CARTESIAN_POINT ( 'NONE',  ( 153.1314981037513121, 265.4154603756023789, 17.73969815997475408 ) ) ;
#72231 = VERTEX_POINT ( 'NONE', #85298 ) ;
#72232 = B_SPLINE_CURVE_WITH_KNOTS ( 'NONE', 3,
 ( #9665, #30576, #45270, #46247 ),
 .UNSPECIFIED., .F., .F.,
 ( 4, 4 ),
 ( 6.208857164277751492E-15, 0.0007264857576706923751 ),
 .UNSPECIFIED. ) ;
#72233 = CARTESIAN_POINT ( 'NONE',  ( 83.10776606998568639, 40.75710275334526500, -2.573362665496658816E-06 ) ) ;
#72234 = CARTESIAN_POINT ( 'NONE',  ( 13.50812563192542548, 9.927558733836244542, 6.180339887498953466 ) ) ;
#72235 = CARTESIAN_POINT ( 'NONE',  ( 191.9438504840783821, 288.0378779041730013, -15.85995341028061389 ) ) ;
#72236 = ORIENTED_EDGE ( 'NONE', *, *, #56572, .F. ) ;
#72237 = CARTESIAN_POINT ( 'NONE',  ( 163.8195406495391353, 279.5693214144951071, 12.35214766166425093 ) ) ;
#72238 = EDGE_CURVE ( 'NONE', #40804, #77173, #9774, .T. ) ;
#72239 = CARTESIAN_POINT ( 'NONE',  ( 194.9220242159064185, 293.0321458743159724, -14.92681063007793263 ) ) ;
#72240 = CARTESIAN_POINT ( 'NONE',  ( 86.47161471182764103, 44.02354154034633638, -6.066641966162809041 ) ) ;
#72241 = ORIENTED_EDGE ( 'NONE', *, *, #65292, .T. ) ;
#72242 = CARTESIAN_POINT ( 'NONE',  ( -22.42236680055709641, 157.8615022471902591, 0.000000000000000000 ) ) ;
#72243 = CARTESIAN_POINT ( 'NONE',  ( 187.8752290710686452, 292.6574842239962209, 12.38629875236594557 ) ) ;
#72244 = CARTESIAN_POINT ( 'NONE',  ( 191.4922467593309250, 298.9726946877590876, 7.604184559945784017 ) ) ;
#72245 = CIRCLE ( 'NONE', #90046, 70.00000000000001421 ) ;
#72246 = DIRECTION ( 'NONE',  ( -0.7909930170786232395, 0.6118251767726273771, 0.000000000000000000 ) ) ;
#72247 = CONICAL_SURFACE ( 'NONE', #33391, 2.749999999999999112, 0.7853981633974469467 ) ;
#72248 = CARTESIAN_POINT ( 'NONE',  ( 80.55710883583050474, 44.52789654886623794, 11.41067263359725992 ) ) ;
#72249 = CARTESIAN_POINT ( 'NONE',  ( 84.70579481679399692, 49.94286076369812832, -13.65556694543043825 ) ) ;
#72250 = DIRECTION ( 'NONE',  ( 1.000000000000000000, 3.241454723682375892E-13, 0.000000000000000000 ) ) ;
#72251 = VERTEX_POINT ( 'NONE', #15841 ) ;
#72252 = VERTEX_POINT ( 'NONE', #41130 ) ;
#72254 = VECTOR ( 'NONE', #16057, 1000.000000000000000 ) ;
#72253 = CARTESIAN_POINT ( 'NONE',  ( 175.3253744491786676, 258.9757446337468991, 12.55620439745121608 ) ) ;
#72255 = ORIENTED_EDGE ( 'NONE', *, *, #76246, .F. ) ;
#72256 = CARTESIAN_POINT ( 'NONE',  ( 52.03546399666511491, 212.3967562850347122, -4.648177544792955347E-16 ) ) ;
#72257 = VERTEX_POINT ( 'NONE', #79200 ) ;
#72258 = CARTESIAN_POINT ( 'NONE',  ( 88.35456099112356299, 44.18765297829227023, 0.2632442814954262245 ) ) ;
#72259 = FACE_OUTER_BOUND ( 'NONE', #77773, .T. ) ;
#72260 = ORIENTED_EDGE ( 'NONE', *, *, #40470, .F. ) ;
#72261 = CARTESIAN_POINT ( 'NONE',  ( 186.1558086338376370, 282.4460829780409199, -16.80270888845420174 ) ) ;
#72262 = CARTESIAN_POINT ( 'NONE',  ( 82.24971233127639891, 41.19297818149956925, 3.242131167557051441 ) ) ;
#72263 = CARTESIAN_POINT ( 'NONE',  ( 71.90400658755810070, 72.53437165389429708, 1.750395423964758557 ) ) ;
#72264 = CARTESIAN_POINT ( 'NONE',  ( 161.9353223911033410, 277.5374438971563222, -13.12909115375462576 ) ) ;
#72265 = CARTESIAN_POINT ( 'NONE',  ( 147.3236643320416022, 275.4749235501183193, -5.185334239426818037 ) ) ;
#72266 = CARTESIAN_POINT ( 'NONE',  ( 153.3544108199959908, 265.0293642254135307, -17.49105661178601423 ) ) ;
#72267 = DIRECTION ( 'NONE',  ( 0.000000000000000000, 0.000000000000000000, 1.000000000000000000 ) ) ;
#72268 = EDGE_CURVE ( 'NONE', #32592, #96097, #39623, .T. ) ;
#72269 = CARTESIAN_POINT ( 'NONE',  ( 157.9710662556744012, 281.0034536832922072, 2.292689402901011420 ) ) ;
#72270 = CARTESIAN_POINT ( 'NONE',  ( 136.3040252829181327, 243.3768266524159856, 9.188101187500098632 ) ) ;
#72271 = CARTESIAN_POINT ( 'NONE',  ( 70.43431413140284292, 61.24050369869113553, -14.83292379404218231 ) ) ;
#72272 = EDGE_LOOP ( 'NONE', ( #29481, #14708, #84966 ) ) ;
#72274 = ORIENTED_EDGE ( 'NONE', *, *, #51316, .T. ) ;
#72273 = CARTESIAN_POINT ( 'NONE',  ( 85.71030961992515529, 48.80922481583876049, -12.49884386288094440 ) ) ;
#72275 = VECTOR ( 'NONE', #28769, 1000.000000000000114 ) ;
#72276 = CARTESIAN_POINT ( 'NONE',  ( 177.7342311040593756, 255.2532439957012684, -8.367404576774948310 ) ) ;
#72277 = CARTESIAN_POINT ( 'NONE',  ( 178.9714194486930694, 253.6239517424200187, 1.422777586239305059 ) ) ;
#72278 = CARTESIAN_POINT ( 'NONE',  ( 129.5390911288783684, 234.0494855054051584, -2.679491924311248496 ) ) ;
#72279 = CARTESIAN_POINT ( 'NONE',  ( 147.2481089941287280, 275.6057892341661386, 4.088130380788767226 ) ) ;
#72280 = CARTESIAN_POINT ( 'NONE',  ( 155.8801288042594990, 278.4237519192228660, 7.215275691167001071 ) ) ;
#72281 = EDGE_CURVE ( 'NONE', #7878, #55188, #46750, .T. ) ;
#72282 = CARTESIAN_POINT ( 'NONE',  ( 192.1779685593947420, 266.1842805242176269, 11.64530923862864142 ) ) ;
#72283 = DIRECTION ( 'NONE',  ( 0.8660254037844394848, 0.4999999999999986122, 0.000000000000000000 ) ) ;
#72284 = VECTOR ( 'NONE', #86689, 1000.000000000000114 ) ;
#72285 = CARTESIAN_POINT ( 'NONE',  ( 170.9849025567062313, 280.9340470213971344, 14.23665144915766234 ) ) ;
#72286 = EDGE_CURVE ( 'NONE', #77851, #38792, #93792, .T. ) ;
#72287 = CYLINDRICAL_SURFACE ( 'NONE', #30481, 70.00000000000002842 ) ;
#72288 = CARTESIAN_POINT ( 'NONE',  ( 177.2393968558746735, 256.1135909324575550, -7.883863129844044693 ) ) ;
#72289 = ORIENTED_EDGE ( 'NONE', *, *, #33031, .T. ) ;
#72290 = CARTESIAN_POINT ( 'NONE',  ( 194.2900850603946310, 294.1266965989547657, -15.88613936555681505 ) ) ;
#72291 = CARTESIAN_POINT ( 'NONE',  ( 66.21613658270437952, 69.35617794467320607, 0.1791810972791403056 ) ) ;
#72292 = ORIENTED_EDGE ( 'NONE', *, *, #60788, .T. ) ;
#72293 = CARTESIAN_POINT ( 'NONE',  ( 188.6301707762981152, 265.0060877223691591, -12.46499516475016733 ) ) ;
#72294 = CARTESIAN_POINT ( 'NONE',  ( 201.4081090739200306, 268.0418142524571863, -2.853212221150517536 ) ) ;
#72295 = CARTESIAN_POINT ( 'NONE',  ( 151.8037247284637488, 267.7152313225378180, -16.71686542126332853 ) ) ;
#72296 = CARTESIAN_POINT ( 'NONE',  ( 190.8187029736043883, 300.1393067457597681, 3.941064102378585954 ) ) ;
#72297 = CARTESIAN_POINT ( 'NONE',  ( 202.5511585997265911, 279.8180975037686835, 17.12781264818056925 ) ) ;
#72299 = CARTESIAN_POINT ( 'NONE',  ( 152.1281151080858933, 275.3594634850046532, -8.621110135100591876 ) ) ;
#72298 = CARTESIAN_POINT ( 'NONE',  ( 161.4200482637542962, 281.4224831315765982, -7.121073954846943721 ) ) ;
#72300 = CARTESIAN_POINT ( 'NONE',  ( 111.2365322456207224, 223.4824982072973683, 3.021315404115420679E-15 ) ) ;
#72301 = ORIENTED_EDGE ( 'NONE', *, *, #93944, .T. ) ;
#72302 = CARTESIAN_POINT ( 'NONE',  ( 75.54185705060035616, 61.33622908259397377, -15.40001492952482742 ) ) ;
#72303 = CARTESIAN_POINT ( 'NONE',  ( 2.552633344394289239, 68.33802890835346489, -10.00000000000000000 ) ) ;
#72304 = CARTESIAN_POINT ( 'NONE',  ( 72.94657399261465969, 65.67239758029106156, -12.71627414374669307 ) ) ;
#72305 = CARTESIAN_POINT ( 'NONE',  ( 152.6656396574222754, 266.2223508737794759, 17.04346597795114349 ) ) ;
#72306 = CARTESIAN_POINT ( 'NONE',  ( 80.76782053159526242, 43.13182372017047328, -9.836536121486679107 ) ) ;
#72307 = CARTESIAN_POINT ( 'NONE',  ( 67.01113894376084090, 68.95971538285371594, 3.001280692439017184 ) ) ;
#72309 = EDGE_CURVE ( 'NONE', #96192, #14857, #68437, .T. ) ;
#72308 = B_SPLINE_CURVE_WITH_KNOTS ( 'NONE', 3,
 ( #48045, #49547, #73364, #88117 ),
 .UNSPECIFIED., .F., .F.,
 ( 4, 4 ),
 ( 0.009486792614561130252, 0.01778295607789639327 ),
 .UNSPECIFIED. ) ;
#72310 = CARTESIAN_POINT ( 'NONE',  ( -14.60124842228533915, 168.5024278399160949, 9.188101187500095079 ) ) ;
#72311 = CARTESIAN_POINT ( 'NONE',  ( 94.19319292813476352, 231.3149278399160664, 9.188101187500093303 ) ) ;
#72312 = CARTESIAN_POINT ( 'NONE',  ( 155.6535436963908694, 261.0471492701456668, -17.87366571046205976 ) ) ;
#72313 = CARTESIAN_POINT ( 'NONE',  ( 146.7842303614460207, 276.4092505945183689, -4.491116827832889236 ) ) ;
#72314 = CARTESIAN_POINT ( 'NONE',  ( 147.8194150887063643, 275.1866381610261101, 4.566218682955557107 ) ) ;
#72315 = CARTESIAN_POINT ( 'NONE',  ( -19.66365018104914242, 92.92360942013182523, 59.99999999999999289 ) ) ;
#72316 = VECTOR ( 'NONE', #10709, 1000.000000000000227 ) ;
#72317 = CARTESIAN_POINT ( 'NONE',  ( 74.77499314424673571, 55.31988034793729270, -16.13510914276501396 ) ) ;
#72318 = CARTESIAN_POINT ( 'NONE',  ( 172.7264208856190919, 290.8582626858774347, 2.771863430787652849 ) ) ;
#72319 = CIRCLE ( 'NONE', #15655, 10.00000000000007816 ) ;
#72320 = CARTESIAN_POINT ( 'NONE',  ( 160.9539812394163221, 281.6746053238863965, 5.581094101012241460 ) ) ;
#72322 = CARTESIAN_POINT ( 'NONE',  ( 163.3723087697842971, 247.6778559913402091, -10.08585062664141319 ) ) ;
#72321 = FACE_OUTER_BOUND ( 'NONE', #9342, .T. ) ;
#72323 = CARTESIAN_POINT ( 'NONE',  ( 177.9561663662901765, 289.9063764978683935, 9.646858304667830453 ) ) ;
#72324 = EDGE_CURVE ( 'NONE', #10254, #1997, #42630, .T. ) ;
#72325 = DIRECTION ( 'NONE',  ( 0.000000000000000000, 0.000000000000000000, 1.000000000000000000 ) ) ;
#72326 = B_SPLINE_CURVE_WITH_KNOTS ( 'NONE', 3,
 ( #75441, #29334, #77305, #36415, #7912, #38787, #792, #69693, #62076, #44005, #93024, #15998, #74947, #77821, #8403, #85969, #54990, #16494, #62576, #67319, #93538, #98247, #47391, #78315, #39765, #70694, #32192, #63094, #94040, #2319, #73216, #33199, #33717, #64608, #2828, #95564, #26110, #56496, #25088, #56985, #11430, #9917, #34207, #26608, #10915, #87970, #80858, #42282, #63595, #32694 ),
 .UNSPECIFIED., .F., .F.,
 ( 4, 2, 2, 2, 2, 2, 2, 2, 2, 2, 2, 2, 2, 2, 2, 2, 2, 2, 2, 2, 2, 2, 2, 2, 4 ),
 ( 0.0002455370680951060418, 0.0007226616231845173211, 0.001199786178273928600, 0.001438348455818573958, 0.001557629594590812178, 0.001676910733363050614, 0.001796191872135289051, 0.001915473010907527271, 0.002154035288451925430, 0.002631159843540722184, 0.003108284398629518504, 0.004062533508807189206, 0.005016782618984860775, 0.005493907174073697428, 0.005732469451618076722, 0.005851750590390267237, 0.005971031729162457752, 0.006030672298548521784, 0.006090312867934584082, 0.006209594006706670513, 0.006448156284250841641, 0.006925280839339159611, 0.007163843116883351556, 0.007402405394427543500, 0.007879529949515927389 ),
 .UNSPECIFIED. ) ;
#72327 = CARTESIAN_POINT ( 'NONE',  ( 164.5261241815984761, 245.6793890755219252, -5.756220888378682510 ) ) ;
#72328 = CARTESIAN_POINT ( 'NONE',  ( 76.77824862278549745, 55.54507606913799833, -16.16088072629311156 ) ) ;
#72329 = DIRECTION ( 'NONE',  ( -0.8660254037844379305, -0.5000000000000014433, -0.000000000000000000 ) ) ;
#72330 = CARTESIAN_POINT ( 'NONE',  ( 81.75096066047075283, 229.5530062829863027, -4.648177544792955347E-16 ) ) ;
#72331 = CARTESIAN_POINT ( 'NONE',  ( 73.49483902118549850, 69.87589544865461733, 9.786909576851130055 ) ) ;
#72332 = CARTESIAN_POINT ( 'NONE',  ( 49.32242524243604720, 199.2833772461660828, -9.188101187500095079 ) ) ;
#72333 = CARTESIAN_POINT ( 'NONE',  ( 76.88818783305237048, 63.31965297372375545, -15.46890590930648912 ) ) ;
#72334 = CARTESIAN_POINT ( 'NONE',  ( 65.45180129215621889, 220.8464784336661637, 1.353441290958777327E-15 ) ) ;
#72335 = CARTESIAN_POINT ( 'NONE',  ( 207.2683629543511756, 271.6476598918739001, -6.694388351944108528 ) ) ;
#72336 = CARTESIAN_POINT ( 'NONE',  ( 76.36065199378450075, 53.31052631447248302, -16.44376018799239958 ) ) ;
#72337 = CYLINDRICAL_SURFACE ( 'NONE', #9344, 16.60714546451156792 ) ;
#72338 = CARTESIAN_POINT ( 'NONE',  ( 24.55112987542764458, 40.41347472807389352, -10.00000000000000000 ) ) ;
#72339 = ADVANCED_FACE ( 'NONE', ( #74064 ), #91963, .T. ) ;
#72340 = CARTESIAN_POINT ( 'NONE',  ( 196.7338846360856337, 268.5824883939956180, -10.68874749315578399 ) ) ;
#72341 = CARTESIAN_POINT ( 'NONE',  ( 35.70653501523218409, 32.56628583063843507, 9.188101187500006262 ) ) ;
#72342 = AXIS2_PLACEMENT_3D ( 'NONE', #37744, #13973, #38234 ) ;
#72343 = CARTESIAN_POINT ( 'NONE',  ( 79.17986403524099615, 49.31136220171410400, -14.94917676811451379 ) ) ;
#72344 = CARTESIAN_POINT ( 'NONE',  ( 84.11950711319154550, 46.87244309510325024, -11.07336435221286131 ) ) ;
#72345 = ORIENTED_EDGE ( 'NONE', *, *, #73279, .F. ) ;
#72346 = CARTESIAN_POINT ( 'NONE',  ( 15.07467606819624173, 24.10171378149917842, 9.188101187500008038 ) ) ;
#72347 = CARTESIAN_POINT ( 'NONE',  ( 72.54255783352381570, 218.8149278399160664, -9.188101187500095079 ) ) ;
#72348 = CARTESIAN_POINT ( 'NONE',  ( 88.40853095561153907, 233.3967562850347122, -4.648177544792955347E-16 ) ) ;
#72349 = VECTOR ( 'NONE', #87539, 1000.000000000000000 ) ;
#72350 = DIRECTION ( 'NONE',  ( 0.4999999999999998890, -0.8660254037844385966, 0.000000000000000000 ) ) ;
#72351 = CARTESIAN_POINT ( 'NONE',  ( 192.6247335881259630, 297.0111699613833594, -13.30158778996737290 ) ) ;
#72352 = CARTESIAN_POINT ( 'NONE',  ( 202.1168934888335684, 280.5702667397902133, 16.99860635998273750 ) ) ;
#72353 = AXIS2_PLACEMENT_3D ( 'NONE', #70208, #30227, #15504 ) ;
#72354 = DIRECTION ( 'NONE',  ( -0.9954322480537355355, -0.09547062131716983757, 0.000000000000000000 ) ) ;
#72355 = CARTESIAN_POINT ( 'NONE',  ( 193.5890283099523401, 288.4767073959486652, 16.07932638873488074 ) ) ;
#72356 = CARTESIAN_POINT ( 'NONE',  ( 87.44817167685637571, 45.02922442914869805, -6.108700660266276117 ) ) ;
#72357 = CARTESIAN_POINT ( 'NONE',  ( 135.1942566882107997, 238.8615022471902023, 5.000000000000051514 ) ) ;
#72358 = CARTESIAN_POINT ( 'NONE',  ( 157.7733463334721478, 257.3755434007023268, -16.94489513499352995 ) ) ;
#72359 = EDGE_LOOP ( 'NONE', ( #33507, #33789, #87531, #91856 ) ) ;
#72360 = CARTESIAN_POINT ( 'NONE',  ( 188.2493976403605984, 273.3260856929751981, 15.61695768125983363 ) ) ;
#72361 = EDGE_LOOP ( 'NONE', ( #75739, #40692, #11237, #32678, #83362, #61379, #67064, #24397, #84843, #57871, #8280, #78726, #53167, #43528, #14529, #51020, #40415, #43811, #50567, #84578 ) ) ;
#72362 = CARTESIAN_POINT ( 'NONE',  ( 206.7893622945242385, 272.4773133715531230, -10.52881283832460291 ) ) ;
#72363 = DIRECTION ( 'NONE',  ( -0.9963824715083249295, 0.08498217737244645464, 0.000000000000000000 ) ) ;
#72364 = EDGE_CURVE ( 'NONE', #45522, #66829, #51755, .T. ) ;
#72365 = DIRECTION ( 'NONE',  ( -0.000000000000000000, -0.000000000000000000, 1.000000000000000000 ) ) ;
#72366 = ORIENTED_EDGE ( 'NONE', *, *, #88355, .F. ) ;
#72367 = CARTESIAN_POINT ( 'NONE',  ( 76.90746743093833970, 62.93938289886319382, -15.23233999435670150 ) ) ;
#72368 = ORIENTED_EDGE ( 'NONE', *, *, #79165, .T. ) ;
#72369 = CARTESIAN_POINT ( 'NONE',  ( 189.9629097242743399, 290.3047074849306455, 14.47560175050799813 ) ) ;
#72370 = CARTESIAN_POINT ( 'NONE',  ( 167.4002430202556582, 247.6565219373602531, 3.576405092176313971 ) ) ;
#72371 = CARTESIAN_POINT ( 'NONE',  ( 153.4542976351440302, 264.8563551865710224, -17.11782692037292009 ) ) ;
#72372 = ORIENTED_EDGE ( 'NONE', *, *, #99840, .F. ) ;
#72373 = CARTESIAN_POINT ( 'NONE',  ( 27.20206195878591870, 37.74646525600392266, 2.839279412974139660 ) ) ;
#72374 = CARTESIAN_POINT ( 'NONE',  ( 82.06425201348349674, 48.60968897072322648, -13.24680869277554862 ) ) ;
#72375 = CARTESIAN_POINT ( 'NONE',  ( 168.1167649493694398, 276.7715220293193283, 15.30949590115454129 ) ) ;
#72376 = CARTESIAN_POINT ( 'NONE',  ( 82.41933087055697627, 40.38430946167127900, -0.8419157719606891188 ) ) ;
#72377 = ORIENTED_EDGE ( 'NONE', *, *, #7138, .F. ) ;
#72378 = ORIENTED_EDGE ( 'NONE', *, *, #11354, .F. ) ;
#72379 = CARTESIAN_POINT ( 'NONE',  ( 186.1400847795470099, 298.1223424718040178, 1.048499119586248085 ) ) ;
#72381 = CARTESIAN_POINT ( 'NONE',  ( 194.8067605455144076, 293.2317884077015151, -16.00245909155922774 ) ) ;
#72380 = CARTESIAN_POINT ( 'NONE',  ( 164.1224127655298730, 246.3786377597482158, 7.356982420601481998 ) ) ;
#72382 = CARTESIAN_POINT ( 'NONE',  ( 85.41398746878978443, 48.60267188261818916, 12.47190137721841019 ) ) ;
#72383 = CARTESIAN_POINT ( 'NONE',  ( 155.6559071247401960, 261.0430556921643870, 17.79853447468815375 ) ) ;
#72384 = DIRECTION ( 'NONE',  ( -0.9291732088853876803, 0.3696446237802353818, 0.000000000000000000 ) ) ;
#72385 = CARTESIAN_POINT ( 'NONE',  ( 70.72929604436274076, 60.91355080922355114, 15.04203567179363965 ) ) ;
#72386 = CARTESIAN_POINT ( 'NONE',  ( 164.4343973647912946, 245.8382645826486055, 4.228584463013169703 ) ) ;
#72387 = CARTESIAN_POINT ( 'NONE',  ( 169.5474634885189005, 267.2654023188423480, 17.55852261903751099 ) ) ;
#72388 = DIRECTION ( 'NONE',  ( -0.8769651246872924855, 0.4805540241036398985, 0.000000000000000000 ) ) ;
#72389 = B_SPLINE_CURVE_WITH_KNOTS ( 'NONE', 3,
 ( #28734, #21153, #6918, #52032 ),
 .UNSPECIFIED., .F., .F.,
 ( 4, 4 ),
 ( 0.004231976529499276163, 0.009740177386616696159 ),
 .UNSPECIFIED. ) ;
#72390 = CARTESIAN_POINT ( 'NONE',  ( 86.66977078063996487, 220.8458772461660544, 9.188101187500095079 ) ) ;
#72391 = ORIENTED_EDGE ( 'NONE', *, *, #83883, .F. ) ;
#72392 = LINE ( 'NONE', #26274, #56076 ) ;
#72393 = CARTESIAN_POINT ( 'NONE',  ( 163.2006102744146290, 276.5399316210059055, -13.88336064207830312 ) ) ;
#72394 = AXIS2_PLACEMENT_3D ( 'NONE', #37772, #28691, #99106 ) ;
#72395 = ORIENTED_EDGE ( 'NONE', *, *, #5956, .F. ) ;
#72396 = VECTOR ( 'NONE', #21721, 1000.000000000000114 ) ;
#72397 = ORIENTED_EDGE ( 'NONE', *, *, #77789, .T. ) ;
#72398 = CARTESIAN_POINT ( 'NONE',  ( 79.95370688104166845, 44.47433224906099980, -10.99098430061395604 ) ) ;
#72400 = B_SPLINE_SURFACE_WITH_KNOTS ( 'NONE', 3, 1, ( 
 ( #25251, #87132 ),
 ( #33881, #18163 ),
 ( #71876, #17664 ),
 ( #86615, #1963 ),
 ( #88120, #41441 ),
 ( #79997, #81012 ),
 ( #34354, #65250 ),
 ( #72381, #88616 ),
 ( #48047, #48562 ),
 ( #49549, #55630 ),
 ( #25775, #64255 ),
 ( #33355, #11076 ),
 ( #96196, #71374 ),
 ( #64766, #18669 ),
 ( #96693, #32848 ),
 ( #9575, #63757 ),
 ( #41952, #56650 ),
 ( #72887, #57139 ),
 ( #2991, #10566 ),
 ( #79503, #65739 ),
 ( #11574, #40929 ),
 ( #95715, #26263 ),
 ( #3479, #26757 ),
 ( #19184, #42432 ),
 ( #73366, #3954 ),
 ( #78990, #40439 ),
 ( #13071, #27262 ),
 ( #60122, #28748 ),
 ( #14049, #4447 ),
 ( #36338, #75874 ),
 ( #66256, #97191 ),
 ( #59117, #90090 ),
 ( #27758, #58630 ),
 ( #4965, #20658 ) ),
 .UNSPECIFIED., .T., .F., .F.,
 ( 4, 2, 2, 2, 2, 2, 2, 2, 2, 2, 2, 2, 2, 2, 2, 2, 4 ),
 ( 2, 2 ),
 ( 0.000000000000000000, 0.06250000000000000000, 0.1250000000000000000, 0.1875000000000000000, 0.2500000000000000000, 0.3125000000000000000, 0.3750000000000000000, 0.4375000000000000000, 0.5000000000000000000, 0.5625000000000000000, 0.6250000000000000000, 0.6875000000000000000, 0.7500000000000000000, 0.8125000000000000000, 0.8750000000000000000, 0.9375000000000000000, 1.000000000000000000 ),
 ( 0.000000000000000000, 1.000000000000000000 ),
 .UNSPECIFIED. ) ;
#72399 = CARTESIAN_POINT ( 'NONE',  ( 191.0478321355427624, 299.7424433957868928, -9.006798842970001218 ) ) ;
#72401 = CYLINDRICAL_SURFACE ( 'NONE', #46595, 70.00000000000002842 ) ;
#72402 = CARTESIAN_POINT ( 'NONE',  ( 159.2713554375903300, 254.7809155221686410, -15.70062444474382168 ) ) ;
#72403 = ADVANCED_FACE ( 'NONE', ( #82697 ), #16111, .T. ) ;
#72404 = FACE_OUTER_BOUND ( 'NONE', #12591, .T. ) ;
#72405 = CARTESIAN_POINT ( 'NONE',  ( 88.29356841273579448, 221.7833772461660544, -9.188101187500095079 ) ) ;
#72406 = ORIENTED_EDGE ( 'NONE', *, *, #17188, .T. ) ;
#72407 = ADVANCED_FACE ( 'NONE', ( #5637 ), #13263, .F. ) ;
#72408 = CIRCLE ( 'NONE', #67523, 70.00000000000001421 ) ;
#72409 =( BOUNDED_CURVE ( )  B_SPLINE_CURVE ( 2, ( #39270, #78311, #16491, #70180, #40771, #788, #8892, #39761, #70690 ),
 .UNSPECIFIED., .F., .T. ) 
 B_SPLINE_CURVE_WITH_KNOTS ( ( 3, 2, 2, 2, 3 ),
 ( 0.7620967741935483764, 0.7634408602150537515, 0.7661290322580645018, 0.7688172043010752521, 0.7701612903225806273 ),
 .UNSPECIFIED. ) 
 CURVE ( )  GEOMETRIC_REPRESENTATION_ITEM ( )  RATIONAL_B_SPLINE_CURVE ( ( 0.9330127018922194093, 0.9330127018922194093, 1.000000000000000000, 0.8660254037844387076, 1.000000000000000000, 0.8660254037844387076, 1.000000000000000000, 0.9330127018922194093, 0.9330127018922194093 ) ) 
 REPRESENTATION_ITEM ( '' )  );
#72410 = EDGE_LOOP ( 'NONE', ( #7577, #8227, #66869, #14702 ) ) ;
#72412 = EDGE_CURVE ( 'NONE', #37985, #17180, #90552, .T. ) ;
#72411 = CARTESIAN_POINT ( 'NONE',  ( 208.2874212803407090, 269.8825990953837390, -1.143705256421198690 ) ) ;
#72413 = ORIENTED_EDGE ( 'NONE', *, *, #17444, .T. ) ;
#72414 = ADVANCED_FACE ( 'NONE', ( #68427 ), #91770, .T. ) ;
#72415 = CARTESIAN_POINT ( 'NONE',  ( 25.64360150771697633, 30.50829794293882102, -10.00000000000000355 ) ) ;
#72416 = CARTESIAN_POINT ( 'NONE',  ( 70.79495161673614234, 69.39911685413080988, -7.528900684444595370 ) ) ;
#72417 = CARTESIAN_POINT ( 'NONE',  ( 87.38898754588738882, 44.84176836479306871, -6.666552467508535251 ) ) ;
#72418 = CARTESIAN_POINT ( 'NONE',  ( -4.759057006084862707, 161.3927522451417929, -10.00000000000009059 ) ) ;
#72419 = CARTESIAN_POINT ( 'NONE',  ( 87.54784588100407916, 44.59992802364795494, 4.936297260842060552 ) ) ;
#72420 = ORIENTED_EDGE ( 'NONE', *, *, #47156, .F. ) ;
#72421 = AXIS2_PLACEMENT_3D ( 'NONE', #62909, #46709, #31007 ) ;
#72422 = CARTESIAN_POINT ( 'NONE',  ( 204.2992694100975939, 276.7902807629455992, 13.99537586056731620 ) ) ;
#72423 = CARTESIAN_POINT ( 'NONE',  ( 80.41304442479348324, 45.09799279809392658, 11.31444151523504260 ) ) ;
#72424 = CARTESIAN_POINT ( 'NONE',  ( 159.8946522441011382, 253.7013337850969492, -16.68230890105693121 ) ) ;
#72425 = CARTESIAN_POINT ( 'NONE',  ( 190.0181636008472594, 270.5760841432478969, 14.27037020729528294 ) ) ;
#72426 = FACE_OUTER_BOUND ( 'NONE', #90353, .T. ) ;
#72427 = CARTESIAN_POINT ( 'NONE',  ( -19.65312891409030271, 93.06504152958497400, 177.5919119679930134 ) ) ;
#72428 = DIRECTION ( 'NONE',  ( -0.9994626398093606756, -0.03277852384266338737, 0.000000000000000000 ) ) ;
#72429 = EDGE_LOOP ( 'NONE', ( #54253, #26245, #16661, #77998 ) ) ;
#72430 = CARTESIAN_POINT ( 'NONE',  ( 202.9431782839550635, 277.8530662632501276, -15.10408699085403583 ) ) ;
#72431 = CARTESIAN_POINT ( 'NONE',  ( 200.6097954076514895, 283.1806371883870383, 16.82611162221071766 ) ) ;
#72432 = AXIS2_PLACEMENT_3D ( 'NONE', #25311, #40989, #72945 ) ;
#72433 = CARTESIAN_POINT ( 'NONE',  ( 84.54996403203030297, 43.01056371783313637, 5.045017719461522887 ) ) ;
#72434 = CARTESIAN_POINT ( 'NONE',  ( 83.14271255481067158, 52.19653239224700059, 14.81391299184662813 ) ) ;
#72435 = CARTESIAN_POINT ( 'NONE',  ( 178.8030382587059819, 291.7907898142459544, -6.050371113150406543 ) ) ;
#72436 = CARTESIAN_POINT ( 'NONE',  ( 202.7185166046502331, 279.5282249361877120, -16.86058306256609640 ) ) ;
#72437 = CARTESIAN_POINT ( 'NONE',  ( 29.01663622185449753, 35.49103043416550918, -8.090169943749479842 ) ) ;
#72438 = CARTESIAN_POINT ( 'NONE',  ( 165.0387478276132072, 244.7914988754632191, -2.473354058663827626 ) ) ;
#72440 = CARTESIAN_POINT ( 'NONE',  ( 182.0920134730108941, 264.0013790589371183, 13.94626246933171210 ) ) ;
#72439 = CARTESIAN_POINT ( 'NONE',  ( 180.5277461560353913, 267.1741556918393599, -15.85281502895699290 ) ) ;
#72441 = CARTESIAN_POINT ( 'NONE',  ( 199.1791426384580745, 281.7616915630761127, -16.58245314267973214 ) ) ;
#72442 = CARTESIAN_POINT ( 'NONE',  ( 31.34407949807308569, 36.83478043621390441, -8.090169943749479842 ) ) ;
#72443 = DIRECTION ( 'NONE',  ( 1.000000000000000000, 5.352861011585574712E-15, 0.000000000000000000 ) ) ;
#72444 = SURFACE_SIDE_STYLE ('',( #58207 ) ) ;
#72445 = PLANE ( 'NONE',  #72432 ) ;
#72446 = CARTESIAN_POINT ( 'NONE',  ( 158.9658060689105525, 271.8015287571203089, -14.71752948393448435 ) ) ;
#72447 = CARTESIAN_POINT ( 'NONE',  ( 82.93837572039436168, 43.22210157649355722, -7.357460665149816670 ) ) ;
#72448 = CARTESIAN_POINT ( 'NONE',  ( 21.25804982287034406, 173.8923013555409796, 4.594050593750050204 ) ) ;
#72449 = CARTESIAN_POINT ( 'NONE',  ( 81.49265314619182732, 45.83748706731968525, 11.45477345881717213 ) ) ;
#72450 = VERTEX_POINT ( 'NONE', #90295 ) ;
#72451 = CIRCLE ( 'NONE', #41907, 50.00000000000000711 ) ;
#72452 = B_SPLINE_CURVE_WITH_KNOTS ( 'NONE', 3,
 ( #48118, #65320, #33944, #34419, #10128, #88183, #79061, #16719, #17211, #57206, #18234, #80568, #47613, #96258, #26330, #40506, #87202, #32425, #79570, #9647, #78540, #71439, #2028, #94755, #71937, #95281, #17734, #2542, #86680, #63320, #94260, #33424, #72449, #24815, #25843, #56718, #49129, #10633, #41509, #3056, #95776, #100104, #66317, #69172, #30688, #88680 ),
 .UNSPECIFIED., .F., .F.,
 ( 4, 1, 2, 2, 1, 2, 2, 1, 1, 2, 2, 1, 1, 2, 2, 1, 1, 2, 2, 1, 1, 1, 2, 2, 1, 1, 1, 2, 2, 4 ),
 ( 0.000000000000000000, 0.06250000000000034694, 0.09375000000000031919, 0.1250000000000003053, 0.1875000000000009159, 0.2187500000000013600, 0.2500000000000017764, 0.3125000000000036637, 0.3437500000000032752, 0.3593750000000032196, 0.3750000000000031641, 0.4375000000000084377, 0.4687500000000107137, 0.4843750000000112133, 0.5000000000000117684, 0.5625000000000167644, 0.5937500000000199840, 0.6093750000000217604, 0.6250000000000236478, 0.6875000000000259792, 0.7187500000000272005, 0.7343750000000270894, 0.7421875000000278666, 0.7500000000000287548, 0.8125000000000195399, 0.8437500000000142109, 0.8593750000000117684, 0.8671875000000103251, 0.8750000000000089928, 1.000000000000000000 ),
 .UNSPECIFIED. ) ;
#72453 = CARTESIAN_POINT ( 'NONE',  ( 86.54933037531351658, 46.26600125392582186, 8.987360782618976529 ) ) ;
#72454 = CARTESIAN_POINT ( 'NONE',  ( 13.69028360280385570, 30.83705186507753382, 3.090169943749475401 ) ) ;
#72455 = LINE ( 'NONE', #3547, #40382 ) ;
#72456 = CARTESIAN_POINT ( 'NONE',  ( 28.37526224051742929, 193.3149278399160949, -9.188101187500095079 ) ) ;
#72458 = EDGE_CURVE ( 'NONE', #20973, #24937, #77924, .T. ) ;
#72457 = VECTOR ( 'NONE', #10240, 1000.000000000000227 ) ;
#72459 = CARTESIAN_POINT ( 'NONE',  ( 161.8289209813647176, 250.3510820566641257, 13.28523796267037937 ) ) ;
#72460 = CARTESIAN_POINT ( 'NONE',  ( 190.9559560067148425, 299.9015775189195665, -4.895152914295826108 ) ) ;
#72461 = CARTESIAN_POINT ( 'NONE',  ( 29.10553579016685077, 39.73705186507756082, -3.090169943749475845 ) ) ;
#72462 = CARTESIAN_POINT ( 'NONE',  ( 199.5639001218976887, 267.6271046904498121, -6.591559436455099785 ) ) ;
#72463 = CARTESIAN_POINT ( 'NONE',  ( 146.5865263025993954, 276.7516840693029962, 0.4918294119671828835 ) ) ;
#72464 = CARTESIAN_POINT ( 'NONE',  ( 196.8446868189476788, 289.7019965600358091, 16.40794635810030755 ) ) ;
#72465 = CARTESIAN_POINT ( 'NONE',  ( 178.9488238674973388, 278.2840548466987798, -16.79158255535696043 ) ) ;
#72466 = LINE ( 'NONE', #3071, #13701 ) ;
#72467 = CARTESIAN_POINT ( 'NONE',  ( 87.15443966109820906, 46.07157893991718822, -8.233590127383161317 ) ) ;
#72468 = CARTESIAN_POINT ( 'NONE',  ( 83.41128051646016672, 51.86661034151835992, 14.99497567496408301 ) ) ;
#72469 = PRESENTATION_LAYER_ASSIGNMENT (  '', '', ( #70786 ) ) ;
#72470 = CARTESIAN_POINT ( 'NONE',  ( 78.90260544222221029, 226.3615022471903160, 5.000000000000046185 ) ) ;
#72471 = CARTESIAN_POINT ( 'NONE',  ( 2.064617007569734319, 27.83817977871672511, 10.00000000000000000 ) ) ;
#72472 = CARTESIAN_POINT ( 'NONE',  ( -78.57153713424663977, 57.64153020465174393, 10.00000000000000000 ) ) ;
#72473 = CARTESIAN_POINT ( 'NONE',  ( 48.45674693441662129, 186.5327760586659451, 1.948934522072303157E-15 ) ) ;
#72474 = DIRECTION ( 'NONE',  ( -0.000000000000000000, -0.000000000000000000, 1.000000000000000000 ) ) ;
#72475 = EDGE_CURVE ( 'NONE', #45639, #92014, #52230, .T. ) ;
#72476 = VERTEX_POINT ( 'NONE', #98863 ) ;
#72477 = CARTESIAN_POINT ( 'NONE',  ( -11.87431992379006296, 23.49859753039504895, -10.00000000000000000 ) ) ;
#72478 = CARTESIAN_POINT ( 'NONE',  ( 190.2236813008869660, 301.1699145145108218, -5.401374690107298093 ) ) ;
#72479 = CARTESIAN_POINT ( 'NONE',  ( 67.67290550563593854, 66.83298015526837332, -8.527019564984499311 ) ) ;
#72480 = VERTEX_POINT ( 'NONE', #91272 ) ;
#72481 = VECTOR ( 'NONE', #17142, 1000.000000000000000 ) ;
#72482 = CARTESIAN_POINT ( 'NONE',  ( 171.2055318311769554, 286.8032793947884329, 8.461617862201846307 ) ) ;
#72483 = CARTESIAN_POINT ( 'NONE',  ( 164.5416088356626290, 245.6525688679454618, -1.463507744092769292 ) ) ;
#72484 = CARTESIAN_POINT ( 'NONE',  ( 159.6707594272863275, 278.7937339944729160, -10.98969969888871212 ) ) ;
#72485 = CARTESIAN_POINT ( 'NONE',  ( 191.0785133773015332, 298.9844436051949401, -7.466887123898782619 ) ) ;
#72486 = CARTESIAN_POINT ( 'NONE',  ( 24.44940106416278169, 29.51421378149920116, -9.188101187500004485 ) ) ;
#72487 = CARTESIAN_POINT ( 'NONE',  ( 203.0398866899141126, 278.9715956204779559, 16.57839218037009132 ) ) ;
#72488 = CARTESIAN_POINT ( 'NONE',  ( 196.3286486926436680, 290.5958008134369948, -16.58330917766970458 ) ) ;
#72489 = CARTESIAN_POINT ( 'NONE',  ( 204.6163864379986705, 276.2410179586759682, 14.66911174422491726 ) ) ;
#72490 = ORIENTED_EDGE ( 'NONE', *, *, #36373, .T. ) ;
#72491 = AXIS2_PLACEMENT_3D ( 'NONE', #16671, #31858, #47565 ) ;
#72492 = CARTESIAN_POINT ( 'NONE',  ( 11.20403028766721398, 24.65586893147754921, -7.433330006724137462 ) ) ;
#72493 = CARTESIAN_POINT ( 'NONE',  ( 58.47569090598246078, 179.7419560658249509, -18.47570218321543223 ) ) ;
#72494 = DIRECTION ( 'NONE',  ( 0.8660254037844395958, 0.4999999999999985567, 0.000000000000000000 ) ) ;
#72495 = ORIENTED_EDGE ( 'NONE', *, *, #16299, .F. ) ;
#72496 = DIRECTION ( 'NONE',  ( 0.000000000000000000, 0.000000000000000000, 1.000000000000000000 ) ) ;
#72497 = CARTESIAN_POINT ( 'NONE',  ( 151.3883635558152321, 268.4346579770563608, 15.44343517165679103 ) ) ;
#72498 = CARTESIAN_POINT ( 'NONE',  ( 177.4109878776140761, 256.1497104635512869, -7.258573510546487917 ) ) ;
#72499 = CARTESIAN_POINT ( 'NONE',  ( -19.76587483483573138, 92.97900609503616920, 59.99999999999999289 ) ) ;
#72500 = ORIENTED_EDGE ( 'NONE', *, *, #15983, .F. ) ;
#72502 = LINE ( 'NONE', #3108, #52361 ) ;
#72501 = CARTESIAN_POINT ( 'NONE',  ( 161.8408514536557163, 250.3304178724980318, -14.12919723462510646 ) ) ;
#72503 = CARTESIAN_POINT ( 'NONE',  ( 196.4808189786114951, 290.3322341467384717, -17.84817245450773271 ) ) ;
#72504 = ORIENTED_EDGE ( 'NONE', *, *, #51905, .T. ) ;
#72505 = CARTESIAN_POINT ( 'NONE',  ( 34.73896580337741113, 43.55466486950702887, 7.012934429366973338E-14 ) ) ;
#72506 = CARTESIAN_POINT ( 'NONE',  ( 72.01037534753049840, 72.25474680761037405, -3.568257732133948590 ) ) ;
#72507 = CARTESIAN_POINT ( 'NONE',  ( 72.62323068768809264, 57.44918900967634556, -16.31697738479318716 ) ) ;
#72508 = CARTESIAN_POINT ( 'NONE',  ( 78.16005489154372299, 61.02200473696554894, -15.90480247637162137 ) ) ;
#72509 = CARTESIAN_POINT ( 'NONE',  ( 157.1458804504438831, 258.4623461901232417, -17.08829597948888335 ) ) ;
#72510 = CARTESIAN_POINT ( 'NONE',  ( 116.3314879560220163, 225.7202760586659167, -5.415160957724236172E-17 ) ) ;
#72511 = B_SPLINE_CURVE_WITH_KNOTS ( 'NONE', 3,
 ( #15613, #43657, #30833, #81713 ),
 .UNSPECIFIED., .F., .F.,
 ( 4, 4 ),
 ( 0.005569629907708512073, 0.01055668864777740447 ),
 .UNSPECIFIED. ) ;
#72512 = CARTESIAN_POINT ( 'NONE',  ( 184.1644723546534124, 288.8997711373874608, -13.10814152958829482 ) ) ;
#72513 = VERTEX_POINT ( 'NONE', #32806 ) ;
#72514 = CARTESIAN_POINT ( 'NONE',  ( 163.8947349411736525, 246.7729873192901664, -5.868803394723933309 ) ) ;
#72515 = ORIENTED_EDGE ( 'NONE', *, *, #82372, .T. ) ;
#72516 = CARTESIAN_POINT ( 'NONE',  ( 39.89592612264573290, 25.96004757982093025, -5.678558825948276656 ) ) ;
#72517 = CARTESIAN_POINT ( 'NONE',  ( 197.9598023461055902, 287.7705598106892921, 18.23120408239484291 ) ) ;
#72518 = CARTESIAN_POINT ( 'NONE',  ( 204.8580075507323102, 274.8627031754986092, -12.15300732346304358 ) ) ;
#72519 = CARTESIAN_POINT ( 'NONE',  ( 64.74867629522887569, 202.0643266524159856, -9.188101187500093303 ) ) ;
#72520 = CARTESIAN_POINT ( 'NONE',  ( 73.81469611240122219, 68.48838210847161179, 10.92215486908102839 ) ) ;
#72521 = CARTESIAN_POINT ( 'NONE',  ( 151.2455280670316711, 268.6820563007532314, 14.35914944935941229 ) ) ;
#72522 = DIRECTION ( 'NONE',  ( -0.000000000000000000, 0.000000000000000000, -1.000000000000000000 ) ) ;
#72523 = CARTESIAN_POINT ( 'NONE',  ( 147.7840609055601817, 276.6774932931532476, -0.9735537997635442808 ) ) ;
#72524 = ORIENTED_EDGE ( 'NONE', *, *, #9111, .F. ) ;
#72525 = CARTESIAN_POINT ( 'NONE',  ( 77.11906017550013814, 57.72506332681559371, -16.14635887841112094 ) ) ;
#72526 = CARTESIAN_POINT ( 'NONE',  ( 162.9254136962317148, 277.9293967287522946, 13.77390558128574760 ) ) ;
#72527 = VECTOR ( 'NONE', #91166, 1000.000000000000000 ) ;
#72528 = ORIENTED_EDGE ( 'NONE', *, *, #21544, .F. ) ;
#72529 = CARTESIAN_POINT ( 'NONE',  ( 109.6465072765698636, 224.1115022471901739, -5.000000000000041744 ) ) ;
#72530 = CARTESIAN_POINT ( 'NONE',  ( 173.9076247008792393, 277.9417859016587045, -16.84130823774900776 ) ) ;
#72531 = CARTESIAN_POINT ( 'NONE',  ( 161.1232569692349443, 251.5733279787459367, -14.02750397520710557 ) ) ;
#72532 = EDGE_CURVE ( 'NONE', #15648, #54612, #90215, .T. ) ;
#72533 = CARTESIAN_POINT ( 'NONE',  ( 80.54443990458493374, 52.78455055202924484, -15.87853153993444622 ) ) ;
#72534 = CARTESIAN_POINT ( 'NONE',  ( 190.2318383114841254, 301.1557861577188078, 3.177919994438449525 ) ) ;
#72535 = VECTOR ( 'NONE', #85754, 1000.000000000000114 ) ;
#72536 = CARTESIAN_POINT ( 'NONE',  ( 82.57385212973971989, 41.04541115053230982, -1.138833187496899768 ) ) ;
#72537 = CARTESIAN_POINT ( 'NONE',  ( 79.14312167556931854, 57.64441083166269664, 0.000000000000000000 ) ) ;
#72538 = CARTESIAN_POINT ( 'NONE',  ( 97.33941792859064890, 238.5530062829863027, -4.648177544792955347E-16 ) ) ;
#72539 = CARTESIAN_POINT ( 'NONE',  ( 49.09806598349715046, 107.5461990276917845, 10.00000000000000000 ) ) ;
#72540 = CARTESIAN_POINT ( 'NONE',  ( 208.3117541397001844, 269.8404533466799080, 2.895672523916592578 ) ) ;
#72541 = VECTOR ( 'NONE', #41194, 1000.000000000000000 ) ;
#72542 = CARTESIAN_POINT ( 'NONE',  ( 134.0307085979840167, 242.0643266524160140, 9.188101187500095079 ) ) ;
#72543 = ORIENTED_EDGE ( 'NONE', *, *, #59510, .F. ) ;
#72544 = CARTESIAN_POINT ( 'NONE',  ( 84.31659741720631018, 44.16501652472276618, -7.663753778293648011 ) ) ;
#72545 = CARTESIAN_POINT ( 'NONE',  ( 93.04999876614748189, 212.9824982072973683, 3.021315404115420679E-15 ) ) ;
#72546 = CARTESIAN_POINT ( 'NONE',  ( 74.83655476910678317, 53.51806293180211327, 16.54630480343736210 ) ) ;
#72547 = CARTESIAN_POINT ( 'NONE',  ( 204.6427704787179493, 276.1953194596412118, 13.28850621060895953 ) ) ;
#72548 = CARTESIAN_POINT ( 'NONE',  ( 74.95985714465535921, 62.05307465897563901, 15.09129879184485290 ) ) ;
#72549 = CARTESIAN_POINT ( 'NONE',  ( 168.6156890688689884, 286.4116463664167895, -8.226575548882113509 ) ) ;
#72550 = ORIENTED_EDGE ( 'NONE', *, *, #93781, .T. ) ;
#72551 = CARTESIAN_POINT ( 'NONE',  ( 80.64201675847387207, 57.55060183585958811, -16.24056620613974644 ) ) ;
#72552 = AXIS2_PLACEMENT_3D ( 'NONE', #75718, #37193, #13422 ) ;
#72553 = CARTESIAN_POINT ( 'NONE',  ( 158.4273715006077907, 275.2297750508094509, -12.38274785084877827 ) ) ;
#72555 = CARTESIAN_POINT ( 'NONE',  ( 75.63268008801900066, 65.14737934564519151, -14.41129995628930516 ) ) ;
#72554 = CARTESIAN_POINT ( 'NONE',  ( 147.7077217681684260, 275.8739656668705038, 2.732453793621575588 ) ) ;
#72556 = CARTESIAN_POINT ( 'NONE',  ( -19.65312891409030271, 93.06504152958497400, 10.00000000000000888 ) ) ;
#72557 = CARTESIAN_POINT ( 'NONE',  ( 136.8177939967088435, 258.9869531367911009, 4.594050593750046652 ) ) ;
#72558 = CIRCLE ( 'NONE', #48228, 70.00000000000001421 ) ;
#72559 = DIRECTION ( 'NONE',  ( -0.7352104281592295454, 0.6778389383370672094, 0.000000000000000000 ) ) ;
#72560 = LINE ( 'NONE', #3163, #87116 ) ;
#72561 = CARTESIAN_POINT ( 'NONE',  ( 71.83943283659645829, 200.0327760586659451, 1.948934522072303157E-15 ) ) ;
#72562 = CARTESIAN_POINT ( 'NONE',  ( 174.2379957965557651, 251.2590728793752248, 3.639292605338433795 ) ) ;
#72563 = CARTESIAN_POINT ( 'NONE',  ( 20.76744934909352125, 17.15404122711133184, 8.090169943749479842 ) ) ;
#72564 = CARTESIAN_POINT ( 'NONE',  ( 190.7516742497373059, 300.2554039010641418, 4.342609251298632067 ) ) ;
#72565 = CARTESIAN_POINT ( 'NONE',  ( 189.3883694580579800, 296.0778630567701839, -11.28578153020828800 ) ) ;
#72566 = CARTESIAN_POINT ( 'NONE',  ( 169.2593199950322287, 285.3159198430261654, -8.952739639644439862 ) ) ;
#72567 = CARTESIAN_POINT ( 'NONE',  ( 202.8549823380854491, 279.2918593523859272, -16.39745931995414807 ) ) ;
#72568 = DIRECTION ( 'NONE',  ( -1.000000000000000000, 0.000000000000000000, 0.000000000000000000 ) ) ;
#72569 = AXIS2_PLACEMENT_3D ( 'NONE', #23229, #85076, #77459 ) ;
#72570 = CARTESIAN_POINT ( 'NONE',  ( 123.7735466722555202, 252.2677522451419065, -5.000000000000047962 ) ) ;
#72571 = CARTESIAN_POINT ( 'NONE',  ( 83.23897458906459690, 51.01732238469139702, -14.23410810326086740 ) ) ;
#72572 = VERTEX_POINT ( 'NONE', #88077 ) ;
#72573 = CARTESIAN_POINT ( 'NONE',  ( 190.4744901378711290, 300.7355008658671522, 0.04566709859947504224 ) ) ;
#72574 = CARTESIAN_POINT ( 'NONE',  ( -7.997804718428996651, 172.3149278399160949, -9.188101187500095079 ) ) ;
#72576 = EDGE_CURVE ( 'NONE', #91263, #3024, #79457, .T. ) ;
#72575 = CIRCLE ( 'NONE', #75825, 15.50000000000000000 ) ;
#72577 = CARTESIAN_POINT ( 'NONE',  ( 40.98727782677583065, 182.2202760586659451, -5.415160957724236172E-17 ) ) ;
#72578 = CARTESIAN_POINT ( 'NONE',  ( -22.42236680055709641, 157.8615022471902591, 0.000000000000000000 ) ) ;
#72579 = CARTESIAN_POINT ( 'NONE',  ( 20.54487693938818538, 27.56454794089042082, 10.00000000000000355 ) ) ;
#72580 = CARTESIAN_POINT ( 'NONE',  ( 88.06269261788008862, 43.61796610520790551, 0.05835779599787207367 ) ) ;
#72581 = CARTESIAN_POINT ( 'NONE',  ( 180.7928668231496658, 266.7588196529836182, -14.70969064882298127 ) ) ;
#72582 = CARTESIAN_POINT ( 'NONE',  ( 71.98264401366868981, 72.39816763649429276, -2.869464145551835710 ) ) ;
#72583 = CARTESIAN_POINT ( 'NONE',  ( 190.5653282632609091, 300.5781646174276602, -5.775635208185608604 ) ) ;
#72584 = CARTESIAN_POINT ( 'NONE',  ( 73.95722056738210881, 55.62591273403975123, -16.58564036811612041 ) ) ;
#72586 = CARTESIAN_POINT ( 'NONE',  ( 57.59477206639472513, 197.3927522451418213, -10.00000000000009059 ) ) ;
#72585 = CARTESIAN_POINT ( 'NONE',  ( 76.57516216600367898, 205.0177522451417929, 5.000000000000051514 ) ) ;
#72587 = CARTESIAN_POINT ( 'NONE',  ( 163.1764708121493470, 256.0176783961395017, -14.93589095490696650 ) ) ;
#72588 = LINE ( 'NONE', #73566, #1353 ) ;
#72589 = ADVANCED_FACE ( 'NONE', ( #72841 ), #78941, .T. ) ;
#72590 = CARTESIAN_POINT ( 'NONE',  ( 161.7512311909553375, 267.3476107021334087, 16.49172225746472975 ) ) ;
#72591 = CARTESIAN_POINT ( 'NONE',  ( 41.59134429584263870, 201.4865022471903160, 10.00000000000009237 ) ) ;
#72592 = DIRECTION ( 'NONE',  ( -0.4999999999999987788, 0.8660254037844392627, 0.000000000000000000 ) ) ;
#72593 = CARTESIAN_POINT ( 'NONE',  ( 202.9093905060991005, 279.1976216410395182, 16.97070083370504179 ) ) ;
#72594 = VECTOR ( 'NONE', #22900, 1000.000000000000000 ) ;
#72595 = CARTESIAN_POINT ( 'NONE',  ( 13.57207436428344316, 169.4548013555409796, -4.594050593750042211 ) ) ;
#72596 = CARTESIAN_POINT ( 'NONE',  ( 38.14222467998226307, 24.94754757982092386, 5.678558825948272215 ) ) ;
#72598 = ADVANCED_FACE ( 'NONE', ( #9529 ), #63711, .T. ) ;
#72597 = CARTESIAN_POINT ( 'NONE',  ( 163.8447499958178355, 252.4744309047850948, 13.22366909537081092 ) ) ;
#72599 = CARTESIAN_POINT ( 'NONE',  ( 153.4389798490260262, 264.8828863703868137, 16.68923469758090761 ) ) ;
#72600 = CARTESIAN_POINT ( 'NONE',  ( 28.71100085020356474, 39.68290643055189548, 3.479690158560446702E-15 ) ) ;
#72601 = CARTESIAN_POINT ( 'NONE',  ( -42.47074677134370546, 28.21475011077167849, 10.00000000000000000 ) ) ;
#72603 = CARTESIAN_POINT ( 'NONE',  ( 179.5007171280461478, 277.3276706483341627, 16.42695695674407830 ) ) ;
#72602 = AXIS2_PLACEMENT_3D ( 'NONE', #54611, #69827, #8539 ) ;
#72604 = DIRECTION ( 'NONE',  ( -0.9922852870422774751, 0.1239754375649672058, 0.000000000000000000 ) ) ;
#72605 = LINE ( 'NONE', #41661, #191 ) ;
#72606 =( NAMED_UNIT ( * ) PLANE_ANGLE_UNIT ( ) SI_UNIT ( $, .RADIAN. ) );
#72607 = CARTESIAN_POINT ( 'NONE',  ( 7.668962567711002265, 16.37878583063838533, 9.188101187500006262 ) ) ;
#72608 = CARTESIAN_POINT ( 'NONE',  ( 168.3232405698885259, 288.2092820357482879, 0.5329914561559622177 ) ) ;
#72609 = CARTESIAN_POINT ( 'NONE',  ( 16.50122538818396478, 18.03085787977762777, 9.188101187500006262 ) ) ;
#72610 = CARTESIAN_POINT ( 'NONE',  ( 207.0929546865518489, 271.9514759237700900, 9.422783993648820910 ) ) ;
#72611 = CARTESIAN_POINT ( 'NONE',  ( 154.9683083969241011, 262.2340116239618055, 18.33261662430134109 ) ) ;
#72612 = AXIS2_PLACEMENT_3D ( 'NONE', #29119, #6802, #13904 ) ;
#72613 = CARTESIAN_POINT ( 'NONE',  ( 45.29894525614688661, 66.96469553601603764, 10.00000000000000000 ) ) ;
#72614 = CARTESIAN_POINT ( 'NONE',  ( 206.8791291248445532, 272.3218326606039454, -10.16823074922856840 ) ) ;
#72615 = VERTEX_POINT ( 'NONE', #2431 ) ;
#72616 = CARTESIAN_POINT ( 'NONE',  ( 153.2964645303881923, 266.7684033456591806, 16.41629521975045236 ) ) ;
#72617 = CARTESIAN_POINT ( 'NONE',  ( 164.3774690880109119, 245.9368672504194819, -2.805681983503304000 ) ) ;
#72618 = CARTESIAN_POINT ( 'NONE',  ( 66.29568901166975081, 68.16417104789285020, 4.350792714150624185 ) ) ;
#72619 = DIRECTION ( 'NONE',  ( -1.000000000000000000, 0.000000000000000000, 0.000000000000000000 ) ) ;
#72620 = VERTEX_POINT ( 'NONE', #95159 ) ;
#72621 = VECTOR ( 'NONE', #87523, 1000.000000000000114 ) ;
#72622 = ORIENTED_EDGE ( 'NONE', *, *, #11100, .F. ) ;
#72623 = DIRECTION ( 'NONE',  ( -0.5000000000000003331, 0.8660254037844383745, -9.251858538542983907E-17 ) ) ;
#72624 = CARTESIAN_POINT ( 'NONE',  ( 86.22252119400383208, 47.68394482253771116, 10.79685758221453007 ) ) ;
#72625 = ORIENTED_EDGE ( 'NONE', *, *, #2938, .F. ) ;
#72626 = DIRECTION ( 'NONE',  ( -0.8660254037844382635, -0.5000000000000004441, -1.232595164407830946E-32 ) ) ;
#72627 = CARTESIAN_POINT ( 'NONE',  ( 178.1953121367105837, 264.0555401404403142, 14.83908789417908913 ) ) ;
#72628 = ORIENTED_EDGE ( 'NONE', *, *, #43687, .F. ) ;
#72629 = CARTESIAN_POINT ( 'NONE',  ( 78.35930054750417639, 61.15116583347188595, -15.90188674197529473 ) ) ;
#72630 = CARTESIAN_POINT ( 'NONE',  ( 161.4397682720950797, 257.0206542164637540, -16.76434429226769041 ) ) ;
#72631 = CARTESIAN_POINT ( 'NONE',  ( 149.2923684163597784, 272.0650280510108701, -12.99082738998495756 ) ) ;
#72632 = CIRCLE ( 'NONE', #95288, 70.00000000000001421 ) ;
#72633 = CARTESIAN_POINT ( 'NONE',  ( 80.51848489276528653, 43.48937927821671678, 9.625745649737424969 ) ) ;
#72634 = VERTEX_POINT ( 'NONE', #19136 ) ;
#72635 = CARTESIAN_POINT ( 'NONE',  ( 161.8873598795597388, 250.2498629158519350, 13.90822209621415873 ) ) ;
#72636 = CARTESIAN_POINT ( 'NONE',  ( 67.21491844529386128, 62.30466486950709992, 1.224646799147354045E-15 ) ) ;
#72637 = CARTESIAN_POINT ( 'NONE',  ( 150.8555837531579868, 276.0290483310748755, -8.437460036063264113 ) ) ;
#72638 = B_SPLINE_SURFACE_WITH_KNOTS ( 'NONE', 3, 1, ( 
 ( #22002, #35712 ),
 ( #58980, #76230 ),
 ( #91440, #14413 ),
 ( #51918, #45296 ),
 ( #68597, #5320 ),
 ( #6805, #28602 ),
 ( #22502, #97539 ),
 ( #44788, #99520 ),
 ( #30104, #28107 ),
 ( #20527, #98532 ),
 ( #75724, #66611 ),
 ( #21036, #51406 ),
 ( #52897, #36197 ),
 ( #37200, #59484 ),
 ( #68102, #29609 ),
 ( #60482, #90466 ),
 ( #60986, #91952 ),
 ( #82369, #12940 ),
 ( #43799, #13429 ),
 ( #59989, #44297 ),
 ( #75226, #36693 ),
 ( #29123, #90959 ),
 ( #21515, #23479 ),
 ( #61973, #45779 ),
 ( #46274, #9302 ),
 ( #77197, #84838 ),
 ( #47288, #94435 ),
 ( #38690, #69595 ),
 ( #40178, #71117 ),
 ( #76701, #31580 ),
 ( #24990, #1718 ),
 ( #8798, #78212 ),
 ( #77720, #22987 ),
 ( #84345, #92440 ) ),
 .UNSPECIFIED., .T., .F., .F.,
 ( 4, 2, 2, 2, 2, 2, 2, 2, 2, 2, 2, 2, 2, 2, 2, 2, 4 ),
 ( 2, 2 ),
 ( 0.000000000000000000, 0.06250000000000000000, 0.1250000000000000000, 0.1875000000000000000, 0.2500000000000000000, 0.3125000000000000000, 0.3750000000000000000, 0.4375000000000000000, 0.5000000000000000000, 0.5625000000000000000, 0.6250000000000000000, 0.6875000000000000000, 0.7500000000000000000, 0.8125000000000000000, 0.8750000000000000000, 0.9375000000000000000, 1.000000000000000000 ),
 ( 0.000000000000000000, 1.000000000000000000 ),
 .UNSPECIFIED. ) ;
#72639 = ORIENTED_EDGE ( 'NONE', *, *, #71138, .F. ) ;
#72640 = EDGE_CURVE ( 'NONE', #40956, #44226, #50009, .T. ) ;
#72641 = EDGE_CURVE ( 'NONE', #95607, #21672, #17615, .T. ) ;
#72642 = CARTESIAN_POINT ( 'NONE',  ( 171.0368701920845638, 254.8364417340256978, -11.42128868109841378 ) ) ;
#72643 = CARTESIAN_POINT ( 'NONE',  ( 202.8167949821795446, 279.3580017930215149, 15.61966256214195070 ) ) ;
#72644 = ORIENTED_EDGE ( 'NONE', *, *, #14955, .T. ) ;
#72645 = ORIENTED_EDGE ( 'NONE', *, *, #28684, .T. ) ;
#72646 = CARTESIAN_POINT ( 'NONE',  ( 156.9842003858142334, 266.1501746981620045, -17.28325484864591743 ) ) ;
#72647 = ORIENTED_EDGE ( 'NONE', *, *, #94473, .F. ) ;
#72648 = CARTESIAN_POINT ( 'NONE',  ( 160.1176491762495857, 270.3263959031288550, 15.73714383883323720 ) ) ;
#72649 = EDGE_LOOP ( 'NONE', ( #39812, #100135, #25490, #96985 ) ) ;
#72650 = LINE ( 'NONE', #18435, #43150 ) ;
#72651 = CARTESIAN_POINT ( 'NONE',  ( 167.6595282994673539, 272.2419833626600507, 16.02614727597981670 ) ) ;
#72652 = CARTESIAN_POINT ( 'NONE',  ( 194.0765626714293717, 294.4965282251961298, 14.23820788189426167 ) ) ;
#72653 = CARTESIAN_POINT ( 'NONE',  ( 177.3343003988342446, 288.7990902974352707, -9.415208683635153619 ) ) ;
#72654 = CARTESIAN_POINT ( 'NONE',  ( 161.4250356354754672, 267.9004136800010656, 17.49898951125957680 ) ) ;
#72655 = LINE ( 'NONE', #42696, #71208 ) ;
#72656 = CARTESIAN_POINT ( 'NONE',  ( 86.51811418199767445, 43.18311598531779794, 0.5570016322997576319 ) ) ;
#72657 = EDGE_CURVE ( 'NONE', #84360, #59501, #85366, .T. ) ;
#72658 = CARTESIAN_POINT ( 'NONE',  ( 158.4279782117914124, 256.2416877271991211, -17.37099813172751794 ) ) ;
#72659 = ORIENTED_EDGE ( 'NONE', *, *, #51159, .F. ) ;
#72660 = CARTESIAN_POINT ( 'NONE',  ( -9.693023484072631035, 23.77726266618848072, 10.00000000000000000 ) ) ;
#72661 = CARTESIAN_POINT ( 'NONE',  ( 19.79331822069313418, 23.37878583063840665, 9.188101187500006262 ) ) ;
#72662 = CARTESIAN_POINT ( 'NONE',  ( 190.5851083282794320, 298.8997307812002191, -8.167350149732024889 ) ) ;
#72664 = ORIENTED_EDGE ( 'NONE', *, *, #58301, .F. ) ;
#72663 = CARTESIAN_POINT ( 'NONE',  ( 83.19608331955247138, 41.11598378048204694, -3.025298033747441107 ) ) ;
#72665 = ORIENTED_EDGE ( 'NONE', *, *, #87917, .T. ) ;
#72666 = EDGE_CURVE ( 'NONE', #100031, #43051, #72754, .T. ) ;
#72667 = CARTESIAN_POINT ( 'NONE',  ( 191.0277618347450073, 299.7772061764919158, 6.528316324927639691 ) ) ;
#72668 = CARTESIAN_POINT ( 'NONE',  ( 84.06604358195920668, 51.46910565605918464, 14.65639964578790710 ) ) ;
#72669 = EDGE_CURVE ( 'NONE', #85106, #55654, #41395, .T. ) ;
#72670 = CARTESIAN_POINT ( 'NONE',  ( 163.9070886935946874, 247.4979362769680620, 7.364863722913233879 ) ) ;
#72671 = CARTESIAN_POINT ( 'NONE',  ( 78.89368875498706757, 46.43720108942829228, 12.98266078055406680 ) ) ;
#72672 = CARTESIAN_POINT ( 'NONE',  ( 160.5989244697666720, 252.4814985078845382, -15.88649589014268315 ) ) ;
#72673 = CARTESIAN_POINT ( 'NONE',  ( 190.5937363720238977, 300.5289603297032954, -0.9120014529451631047 ) ) ;
#72674 = ORIENTED_EDGE ( 'NONE', *, *, #20094, .F. ) ;
#72675 = FACE_OUTER_BOUND ( 'NONE', #69074, .T. ) ;
#72676 = CARTESIAN_POINT ( 'NONE',  ( 72.04273812837080015, 59.28583566120335746, 15.84548535902080246 ) ) ;
#72677 = AXIS2_PLACEMENT_3D ( 'NONE', #53317, #75641, #6734 ) ;
#72678 = CARTESIAN_POINT ( 'NONE',  ( 164.2723164851102808, 246.1189969011916503, -1.993789335506892302 ) ) ;
#72679 = CARTESIAN_POINT ( 'NONE',  ( 26.41785753015494009, 179.3927522451418213, -10.00000000000009059 ) ) ;
#72680 = CARTESIAN_POINT ( 'NONE',  ( 110.8105760068962269, 222.5327760586659451, 1.948934522072302763E-15 ) ) ;
#72681 = CARTESIAN_POINT ( 'NONE',  ( 82.50844557763632281, 41.01330284059301334, -1.198675424783806287 ) ) ;
#72682 = AXIS2_PLACEMENT_3D ( 'NONE', #71702, #39246, #70156 ) ;
#72683 = CARTESIAN_POINT ( 'NONE',  ( 17.65531800687426056, 22.14441083166260427, 10.00000000000000533 ) ) ;
#72684 = CARTESIAN_POINT ( 'NONE',  ( 208.0941653616417852, 270.2173281654339689, 1.603026803260118704 ) ) ;
#72685 = VECTOR ( 'NONE', #20095, 1000.000000000000000 ) ;
#72686 = CARTESIAN_POINT ( 'NONE',  ( 19.39059577201889084, 175.8768266524160140, 9.188101187500098632 ) ) ;
#72687 = CARTESIAN_POINT ( 'NONE',  ( 168.1589593212097498, 275.9390298053305628, -16.40258036402506647 ) ) ;
#72688 = ORIENTED_EDGE ( 'NONE', *, *, #78282, .F. ) ;
#72689 = CIRCLE ( 'NONE', #38644, 7.273499999999997634 ) ;
#72690 = ORIENTED_EDGE ( 'NONE', *, *, #48483, .T. ) ;
#72691 = CARTESIAN_POINT ( 'NONE',  ( 188.2930696087533988, 261.4206402585738829, -5.929984520638014622 ) ) ;
#72692 = CARTESIAN_POINT ( 'NONE',  ( 88.32078559155080200, 44.16791947909882765, 0.3596700509409204716 ) ) ;
#72693 = CARTESIAN_POINT ( 'NONE',  ( 83.32940628703454422, 42.65613730677653592, 5.827714800416384122 ) ) ;
#72694 = PLANE ( 'NONE',  #46632 ) ;
#72695 = CARTESIAN_POINT ( 'NONE',  ( 34.30229714732359980, 200.6115022471903160, -5.000000000000047962 ) ) ;
#72696 = CIRCLE ( 'NONE', #96937, 9.212605237762131694 ) ;
#72697 =( BOUNDED_CURVE ( )  B_SPLINE_CURVE ( 2, ( #65554, #43238, #74181, #88937, #4771, #66554, #5258, #36140, #67043, #59424, #90403, #82800, #34169 ),
 .UNSPECIFIED., .F., .T. ) 
 B_SPLINE_CURVE_WITH_KNOTS ( ( 3, 2, 2, 2, 2, 2, 3 ),
 ( 0.06250000000000000000, 0.06500000000000000222, 0.07000000000000000666, 0.07499999999999999722, 0.08000000000000000167, 0.08500000000000000611, 0.08750000000000000833 ),
 .UNSPECIFIED. ) 
 CURVE ( )  GEOMETRIC_REPRESENTATION_ITEM ( )  RATIONAL_B_SPLINE_CURVE ( ( 0.9755282581475768211, 0.9755282581475768211, 1.000000000000000000, 0.9510565162951535312, 1.000000000000000000, 0.9510565162951535312, 1.000000000000000000, 0.9510565162951535312, 1.000000000000000000, 0.9510565162951535312, 1.000000000000000000, 0.9755282581475767101, 0.9755282581475768211 ) ) 
 REPRESENTATION_ITEM ( '' )  );
#72698 = DIRECTION ( 'NONE',  ( 1.000000000000000000, 0.000000000000000000, 0.000000000000000000 ) ) ;
#72699 = CARTESIAN_POINT ( 'NONE',  ( 73.82480279627529285, 68.30552952313148296, -11.59219441058860589 ) ) ;
#72700 = CARTESIAN_POINT ( 'NONE',  ( 48.29419362332453858, 192.5643266524160140, 9.188101187500095079 ) ) ;
#72701 = CARTESIAN_POINT ( 'NONE',  ( 80.97745796857455503, 210.8927522451417929, -10.00000000000009059 ) ) ;
#72702 = EDGE_LOOP ( 'NONE', ( #69742, #31013, #56123, #56673 ) ) ;
#72703 = CARTESIAN_POINT ( 'NONE',  ( 81.88992170983947005, 42.99646257747416200, 7.919497295398134185 ) ) ;
#72704 = CARTESIAN_POINT ( 'NONE',  ( 158.4906987444244635, 282.4944243069865593, -1.669741222482398424 ) ) ;
#72705 = B_SPLINE_CURVE_WITH_KNOTS ( 'NONE', 3,
 ( #55284, #40084, #40589, #88266, #16802, #17303, #56293, #25402, #63902, #48722, #33514, #48207, #79152, #18815, #64410, #79654, #71028, #34027, #26416, #1630, #11232, #33002, #9734, #62900, #93853, #71528, #9210, #95373, #63406, #2119, #87289, #10218, #47688, #80151, #72021, #56798, #10717, #78624, #41593, #57296, #80654, #42097, #1114, #27415, #5107, #42582, #58293, #50688, #19338, #65403 ),
 .UNSPECIFIED., .F., .F.,
 ( 4, 2, 2, 2, 2, 2, 2, 2, 2, 2, 2, 2, 2, 2, 2, 2, 2, 2, 2, 2, 2, 2, 2, 2, 4 ),
 ( 0.0001966302632834507791, 0.001208579006267713769, 0.001714553377759878887, 0.001967540563505931414, 0.002094034156378898372, 0.002220527749251865763, 0.002347021342124832721, 0.002473514934997800112, 0.002726502120743729256, 0.003232476492235519024, 0.004244425235219099861, 0.005256373978202681131, 0.005762348349694435337, 0.006015335535440235679, 0.006268322721186036887, 0.006331569517622465289, 0.006394816314058895425, 0.006458063110495323826, 0.006521309906931753962, 0.006774297092677275013, 0.007027284278422796064, 0.007280271464168316248, 0.007533258649913837299, 0.007786245835659358350, 0.008292220207150481984 ),
 .UNSPECIFIED. ) ;
#72706 = AXIS2_PLACEMENT_3D ( 'NONE', #30069, #4801, #67571 ) ;
#72707 = EDGE_CURVE ( 'NONE', #66378, #46791, #64720, .T. ) ;
#72708 = CARTESIAN_POINT ( 'NONE',  ( 9.810363290536042058, 164.2202760586659736, -5.415160957724236172E-17 ) ) ;
#72709 = CARTESIAN_POINT ( 'NONE',  ( 68.75122914510536987, 64.15569240841469423, -11.94966557906562166 ) ) ;
#72710 = CARTESIAN_POINT ( 'NONE',  ( 150.9115585710837877, 269.2605084359132093, -15.80434701481532578 ) ) ;
#72711 = DIRECTION ( 'NONE',  ( 0.9634819383873034493, -0.2491829092639731569, -0.09803281150812268030 ) ) ;
#72712 = CARTESIAN_POINT ( 'NONE',  ( 147.3236643320416022, 275.4749235501183193, -5.185334239426818037 ) ) ;
#72713 = EDGE_CURVE ( 'NONE', #20148, #96454, #63609, .T. ) ;
#72714 = DIRECTION ( 'NONE',  ( 0.000000000000000000, 0.000000000000000000, -1.000000000000000000 ) ) ;
#72715 = CARTESIAN_POINT ( 'NONE',  ( 163.7707306762541748, 246.9877690064858484, 7.021959502997312086 ) ) ;
#72716 = CARTESIAN_POINT ( 'NONE',  ( 156.6812872898450735, 261.2670451491295012, 0.000000000000000000 ) ) ;
#72717 = CARTESIAN_POINT ( 'NONE',  ( 147.6220714307702622, 274.9580672937808572, 8.392894244419288441 ) ) ;
#72718 = VERTEX_POINT ( 'NONE', #34309 ) ;
#72719 = CARTESIAN_POINT ( 'NONE',  ( 5.290446120544989306, 163.8615022471902023, 5.000000000000051514 ) ) ;
#72720 = LINE ( 'NONE', #35678, #57887 ) ;
#72721 = CARTESIAN_POINT ( 'NONE',  ( 127.7791744883563183, 235.3923013555409796, 4.594050593750050204 ) ) ;
#72722 = CARTESIAN_POINT ( 'NONE',  ( 26.01786902700012405, 17.94754757982089899, 5.678558825948272215 ) ) ;
#72724 = ADVANCED_FACE ( 'NONE', ( #97630 ), #55553, .F. ) ;
#72723 = CARTESIAN_POINT ( 'NONE',  ( 74.99160476570628475, 67.13646269190913074, 13.03024426091169197 ) ) ;
#72725 = DIRECTION ( 'NONE',  ( -0.4999999999999987788, 0.8660254037844392627, 0.000000000000000000 ) ) ;
#72727 = CARTESIAN_POINT ( 'NONE',  ( 49.87168060777529632, 103.2007005253944385, 10.00000000000000000 ) ) ;
#72726 = CARTESIAN_POINT ( 'NONE',  ( 196.2255671652529259, 290.7743432561995860, 16.01325193769018185 ) ) ;
#72728 = CARTESIAN_POINT ( 'NONE',  ( 190.8671785295675818, 300.0553446199063501, -7.998068249277817898 ) ) ;
#72729 = ORIENTED_EDGE ( 'NONE', *, *, #83127, .T. ) ;
#72730 = CARTESIAN_POINT ( 'NONE',  ( 190.8264243556038195, 300.1259329198319961, 8.466983560044813117 ) ) ;
#72731 = CARTESIAN_POINT ( 'NONE',  ( 149.5796913320911870, 271.5673701627850960, -12.80793412251569841 ) ) ;
#72732 = CARTESIAN_POINT ( 'NONE',  ( 58.00798602660123038, 188.7095308348468734, 4.041334437186271426E-16 ) ) ;
#72733 = CARTESIAN_POINT ( 'NONE',  ( 176.1322591638738118, 292.6111088397734648, -1.129813806047020863 ) ) ;
#72734 = CARTESIAN_POINT ( 'NONE',  ( 81.73893769428700296, 55.29113635392555892, -15.92164997284989703 ) ) ;
#72735 = ORIENTED_EDGE ( 'NONE', *, *, #55087, .F. ) ;
#72736 = DIRECTION ( 'NONE',  ( -0.5803476755362181327, -0.8143688203140567738, 0.000000000000000000 ) ) ;
#72737 = CARTESIAN_POINT ( 'NONE',  ( 176.2784824380131568, 278.9230878378185139, 15.47631285694224701 ) ) ;
#72738 = CARTESIAN_POINT ( 'NONE',  ( 165.6403964848181829, 269.1609729818266032, -16.85820533882582595 ) ) ;
#72739 = B_SPLINE_CURVE_WITH_KNOTS ( 'NONE', 3,
 ( #11043, #71848, #18640, #94662, #25743, #40900, #41410, #41920, #96662, #2446, #25220, #72856, #95687, #71342, #34325, #33326, #42403, #65222, #3925, #56623, #18132, #96165, #26726, #40409, #64736, #79967, #88589, #50024, #56107, #10535, #34807, #72355, #65709, #80979, #87095, #11545, #86583, #2959, #33851, #51008, #21140, #81959 ),
 .UNSPECIFIED., .F., .F.,
 ( 4, 2, 2, 2, 2, 2, 2, 2, 2, 2, 2, 2, 2, 2, 2, 2, 2, 2, 2, 2, 4 ),
 ( 0.003028838789308639992, 0.003226312173560616243, 0.003423785557812592060, 0.003522522249938576499, 0.003621258942064560938, 0.003719995634190545377, 0.003818732326316529382, 0.004016205710568453158, 0.004213679094820376933, 0.004608625863324152493, 0.005398519400331704479, 0.006188412937339255598, 0.007768200011354287580, 0.007866936703480216508, 0.007965673395606144569, 0.008015041741669108599, 0.008064410087732072629, 0.008163146779858087426, 0.008558093548362137939, 0.008953040316866188453, 0.009347987085370238966 ),
 .UNSPECIFIED. ) ;
#72740 = ADVANCED_FACE ( 'NONE', ( #83435 ), #46366, .F. ) ;
#72741 = EDGE_CURVE ( 'NONE', #48389, #21055, #40408, .T. ) ;
#72742 = CARTESIAN_POINT ( 'NONE',  ( 79.67407917426849906, 52.06013808976464929, 15.34621390177021283 ) ) ;
#72743 = PLANE ( 'NONE',  #10555 ) ;
#72744 = CARTESIAN_POINT ( 'NONE',  ( 72.31870688955723381, 71.66728745601001549, -5.813503713761849490 ) ) ;
#72745 = CARTESIAN_POINT ( 'NONE',  ( 148.0620100209659427, 274.6244786578839694, 6.173810397789149640 ) ) ;
#72746 = DIRECTION ( 'NONE',  ( -0.8660254037844387076, -0.4999999999999998890, -0.000000000000000000 ) ) ;
#72747 = CARTESIAN_POINT ( 'NONE',  ( 14.26996179277632848, 9.208019796199270246, -3.090169943749474069 ) ) ;
#72748 = CARTESIAN_POINT ( 'NONE',  ( 191.8314558436726145, 287.9551196214300148, -15.85916516023665856 ) ) ;
#72749 = ORIENTED_EDGE ( 'NONE', *, *, #71902, .F. ) ;
#72750 = CARTESIAN_POINT ( 'NONE',  ( 163.8647661177941757, 279.6316184227941903, 12.38387626794212970 ) ) ;
#72751 = CARTESIAN_POINT ( 'NONE',  ( 148.4042165687623083, 273.6033521758856750, -8.709765892313745539 ) ) ;
#72752 = CARTESIAN_POINT ( 'NONE',  ( 83.58619102057019745, 43.97462430113206011, -8.849062569972019787 ) ) ;
#72753 = ORIENTED_EDGE ( 'NONE', *, *, #57438, .F. ) ;
#72754 = CIRCLE ( 'NONE', #74331, 0.1418229129681522482 ) ;
#72755 = CARTESIAN_POINT ( 'NONE',  ( 79.33204938572286835, 59.85669560537334632, 16.15623921946350450 ) ) ;
#72756 = CARTESIAN_POINT ( 'NONE',  ( 190.5217943342473745, 281.4870030958396683, 17.81127109971334121 ) ) ;
#72757 = CARTESIAN_POINT ( 'NONE',  ( 70.34454795188869980, 61.29844696716961749, 14.78467410895967760 ) ) ;
#72758 = VECTOR ( 'NONE', #31907, 999.9999999999998863 ) ;
#72759 = CARTESIAN_POINT ( 'NONE',  ( 82.22619446726943693, 50.63112855324299488, -14.32323471781884372 ) ) ;
#72760 = DIRECTION ( 'NONE',  ( -0.8660254037844387076, -0.4999999999999998890, -0.000000000000000000 ) ) ;
#72761 = CARTESIAN_POINT ( 'NONE',  ( 155.6569868912636991, 261.0411854816857158, -17.75433477650897984 ) ) ;
#72762 = VERTEX_POINT ( 'NONE', #85440 ) ;
#72763 = EDGE_CURVE ( 'NONE', #29268, #45532, #14979, .T. ) ;
#72764 = VERTEX_POINT ( 'NONE', #14001 ) ;
#72765 = CARTESIAN_POINT ( 'NONE',  ( 177.2385493374541454, 260.3943833094866136, 12.25215814848759699 ) ) ;
#72766 = ORIENTED_EDGE ( 'NONE', *, *, #72741, .F. ) ;
#72767 = CARTESIAN_POINT ( 'NONE',  ( 77.47491854863321237, 49.58014053284396283, 14.91146804420484528 ) ) ;
#72768 = ORIENTED_EDGE ( 'NONE', *, *, #95250, .T. ) ;
#72769 = CARTESIAN_POINT ( 'NONE',  ( 74.54111643893327255, 56.67881626048158239, 16.07342755282378377 ) ) ;
#72771 = CARTESIAN_POINT ( 'NONE',  ( 203.0498946958275326, 278.9542612457532869, -15.11479947333269003 ) ) ;
#72770 = VECTOR ( 'NONE', #87240, 1000.000000000000114 ) ;
#72772 = ORIENTED_EDGE ( 'NONE', *, *, #66651, .T. ) ;
#72773 = EDGE_CURVE ( 'NONE', #21377, #60539, #85138, .T. ) ;
#72774 = CARTESIAN_POINT ( 'NONE',  ( 82.52834598917124254, 40.78028802545565412, 3.192646178055736694 ) ) ;
#72775 = CARTESIAN_POINT ( 'NONE',  ( 85.04377965201177858, 48.84687674572034410, 12.36303725827022149 ) ) ;
#72776 = CARTESIAN_POINT ( 'NONE',  ( 161.0515428782683500, 277.3244187559503189, -13.42420650014866368 ) ) ;
#72777 = CARTESIAN_POINT ( 'NONE',  ( 147.5851099763508216, 275.0220864107570264, -4.372720440640867956 ) ) ;
#72778 = CARTESIAN_POINT ( 'NONE',  ( 152.7691010214056462, 266.0431505347400503, -16.40662330462167162 ) ) ;
#72779 = CARTESIAN_POINT ( 'NONE',  ( 50.12332653952446293, 98.65487733484056321, 177.5919119679930134 ) ) ;
#72780 = CARTESIAN_POINT ( 'NONE',  ( 29.08982151148960682, 17.76426979415090912, 3.090169943749476733 ) ) ;
#72781 = EDGE_CURVE ( 'NONE', #9880, #99877, #17809, .T. ) ;
#72782 = CARTESIAN_POINT ( 'NONE',  ( 143.4758849319492526, 244.4548013555409796, -4.594050593750042211 ) ) ;
#72783 = CARTESIAN_POINT ( 'NONE',  ( 70.80606192109750907, 61.41720523217159666, -14.84941795604011539 ) ) ;
#72784 = ORIENTED_EDGE ( 'NONE', *, *, #21470, .T. ) ;
#72785 = CIRCLE ( 'NONE', #89029, 1.449999999999993072 ) ;
#72786 = ADVANCED_FACE ( 'NONE', ( #30190 ), #99114, .F. ) ;
#72787 = ADVANCED_FACE ( 'NONE', ( #30698 ), #76315, .T. ) ;
#72789 = ORIENTED_EDGE ( 'NONE', *, *, #2894, .T. ) ;
#72788 = CARTESIAN_POINT ( 'NONE',  ( 200.2245315327614605, 270.3076691078479712, 9.266824258444575690 ) ) ;
#72790 = EDGE_CURVE ( 'NONE', #44698, #48849, #69684, .T. ) ;
#72791 = CARTESIAN_POINT ( 'NONE',  ( -0.7717317059461257234, 170.3615022471902591, -10.00000000000009592 ) ) ;
#72792 = CARTESIAN_POINT ( 'NONE',  ( 162.6774150396764469, 248.8814472377480911, 10.88033986792731689 ) ) ;
#72793 = CARTESIAN_POINT ( 'NONE',  ( 172.9698904924519240, 250.6642211707864476, -4.168778760986519671 ) ) ;
#72794 = CARTESIAN_POINT ( 'NONE',  ( 146.6863996654837763, 276.5786983304647606, 3.619532364376333078 ) ) ;
#72795 = DIRECTION ( 'NONE',  ( -0.9879014915521906470, 0.1550826972584532504, 0.000000000000000000 ) ) ;
#72796 = CARTESIAN_POINT ( 'NONE',  ( 70.99909089399695006, 61.09348569631758608, 14.50421621802051853 ) ) ;
#72797 = CARTESIAN_POINT ( 'NONE',  ( 171.0847150063659683, 280.7602631364448484, 13.96071002983590859 ) ) ;
#72798 = CARTESIAN_POINT ( 'NONE',  ( 76.45572749639896415, 51.64231386251727685, -16.15369532822336751 ) ) ;
#72799 = CARTESIAN_POINT ( 'NONE',  ( 177.2731322035851349, 256.0571359664338047, -8.025376214617153892 ) ) ;
#72800 = ORIENTED_EDGE ( 'NONE', *, *, #56572, .T. ) ;
#72801 = DIRECTION ( 'NONE',  ( 1.000000000000000000, 0.000000000000000000, 0.000000000000000000 ) ) ;
#72802 = CARTESIAN_POINT ( 'NONE',  ( 75.64425446922575702, 62.03138304502632394, -15.24332385036787052 ) ) ;
#72803 = ORIENTED_EDGE ( 'NONE', *, *, #10932, .T. ) ;
#72804 = LINE ( 'NONE', #26668, #24108 ) ;
#72805 = CARTESIAN_POINT ( 'NONE',  ( 202.1068129883413746, 268.3794028533957317, -2.863715232315004133 ) ) ;
#72806 = CARTESIAN_POINT ( 'NONE',  ( 152.4183529982803407, 266.6506639314469567, -16.73371844995563862 ) ) ;
#72807 = CARTESIAN_POINT ( 'NONE',  ( 148.9232972370683399, 272.7042780851529642, 12.27045554427055940 ) ) ;
#72808 = CARTESIAN_POINT ( 'NONE',  ( 202.4943568615953779, 279.9164810001701085, 17.09064351659286984 ) ) ;
#72810 = CARTESIAN_POINT ( 'NONE',  ( 151.3683638516007477, 275.1446189862357414, -9.648240976932610735 ) ) ;
#72809 = CARTESIAN_POINT ( 'NONE',  ( 157.8667100161213739, 273.7629819761619956, 14.59697424305941382 ) ) ;
#72811 = CARTESIAN_POINT ( 'NONE',  ( -19.65312891409030271, 93.06504152958497400, -45.00000000000001421 ) ) ;
#72812 = ORIENTED_EDGE ( 'NONE', *, *, #27535, .T. ) ;
#72813 = CARTESIAN_POINT ( 'NONE',  ( 72.20202516581701957, 62.31549783853672153, -14.29472092056413501 ) ) ;
#72814 = CARTESIAN_POINT ( 'NONE',  ( 190.2326078713353752, 273.4588640468538188, -15.98580255482095325 ) ) ;
#72815 = CARTESIAN_POINT ( 'NONE',  ( 200.0313018224816801, 276.5939864008022369, 15.71640468486303099 ) ) ;
#72816 = CARTESIAN_POINT ( 'NONE',  ( -6.583630525541995127, 178.5530062829863027, -4.648177544792955347E-16 ) ) ;
#72817 = CARTESIAN_POINT ( 'NONE',  ( 80.64028050891147359, 43.44267665222750452, -9.484970014585552889 ) ) ;
#72818 = CARTESIAN_POINT ( 'NONE',  ( 52.05581792490468729, 190.8615022471902023, 5.000000000000051514 ) ) ;
#72819 = CARTESIAN_POINT ( 'NONE',  ( 163.0171530587457767, 248.2930037274571191, 9.677214176418313940 ) ) ;
#72820 = CARTESIAN_POINT ( 'NONE',  ( 10.86574497745707646, 167.8923013555410080, 4.594050593750050204 ) ) ;
#72821 = CARTESIAN_POINT ( 'NONE',  ( 104.5854977735480560, 237.3149278399160664, 9.188101187500093303 ) ) ;
#72822 = CARTESIAN_POINT ( 'NONE',  ( 89.31526421587503251, 210.8262482093457777, 3.021315404115420679E-15 ) ) ;
#72823 = CARTESIAN_POINT ( 'NONE',  ( 186.7545291922311890, 295.9253793373928261, -7.587588941354818317 ) ) ;
#72825 = CARTESIAN_POINT ( 'NONE',  ( 81.49135018016791321, 59.57715975391656116, -0.01744974835125552223 ) ) ;
#72824 = VECTOR ( 'NONE', #25781, 1000.000000000000227 ) ;
#72826 = CARTESIAN_POINT ( 'NONE',  ( 75.70758752364832844, 55.03446575750268721, -16.13395138078375268 ) ) ;
#72827 = CARTESIAN_POINT ( 'NONE',  ( 160.4265347487137205, 282.4329614563485507, 5.107902280202428535 ) ) ;
#72828 = CARTESIAN_POINT ( 'NONE',  ( 189.5113466251651744, 300.6005995191865736, -1.615647776261078583 ) ) ;
#72829 = CARTESIAN_POINT ( 'NONE',  ( 177.9124682818391250, 290.1927361200270070, 9.830732425089301785 ) ) ;
#72830 = FACE_OUTER_BOUND ( 'NONE', #3951, .T. ) ;
#72831 = FILL_AREA_STYLE ('',( #63197 ) ) ;
#72832 = CARTESIAN_POINT ( 'NONE',  ( 185.6713631041849055, 258.9584525764907426, -6.747383155299178092 ) ) ;
#72833 = DIRECTION ( 'NONE',  ( 0.000000000000000000, 0.000000000000000000, 1.000000000000000000 ) ) ;
#72834 = CARTESIAN_POINT ( 'NONE',  ( -20.65464553008483151, 23.07220643578490993, 177.5919119679930134 ) ) ;
#72835 = CARTESIAN_POINT ( 'NONE',  ( 77.02263550477385934, 63.85671778288190836, -15.30752586418454086 ) ) ;
#72836 = CARTESIAN_POINT ( 'NONE',  ( 80.49933977867583224, 217.2833772461660544, -9.188101187500095079 ) ) ;
#72837 = CARTESIAN_POINT ( 'NONE',  ( 161.6923300915171922, 250.5876644177310482, -14.43081872899884566 ) ) ;
#72839 = EDGE_CURVE ( 'NONE', #5980, #14868, #41977, .T. ) ;
#72838 = CARTESIAN_POINT ( 'NONE',  ( -78.71521058394758086, 57.86724000996476747, -10.00000000000000000 ) ) ;
#72840 = CARTESIAN_POINT ( 'NONE',  ( -16.57839871714885760, 103.5154107798534113, 12.75852272963258471 ) ) ;
#72842 = DIRECTION ( 'NONE',  ( 0.8816062427480149122, 0.4719856276919119353, 0.000000000000000000 ) ) ;
#72841 = FACE_OUTER_BOUND ( 'NONE', #42550, .T. ) ;
#72843 = CARTESIAN_POINT ( 'NONE',  ( 173.2279903352282986, 268.2393894133472827, -16.29216417966541641 ) ) ;
#72844 = CARTESIAN_POINT ( 'NONE',  ( 33.10845880387886808, 31.06628583063843863, -9.188101187500006262 ) ) ;
#72845 = LINE ( 'NONE', #33313, #9471 ) ;
#72846 = CARTESIAN_POINT ( 'NONE',  ( 136.1966614240191689, 237.8932355074535678, -2.679491924311248496 ) ) ;
#72847 = EDGE_LOOP ( 'NONE', ( #68347, #34833, #64133, #92740 ) ) ;
#72848 = CARTESIAN_POINT ( 'NONE',  ( 23.27484393518965788, 15.29860640527292226, -2.839279412974138328 ) ) ;
#72849 = CARTESIAN_POINT ( 'NONE',  ( 75.49289073487081225, 205.2048013555409796, 4.594050593750051981 ) ) ;
#72850 = CARTESIAN_POINT ( 'NONE',  ( 169.4774712875160390, 288.1570225834816483, -1.094182444139154775 ) ) ;
#72851 = CARTESIAN_POINT ( 'NONE',  ( 147.2658550951450422, 275.5750520855697800, -5.215660180131691526 ) ) ;
#72852 = CARTESIAN_POINT ( 'NONE',  ( 153.4767009694824367, 264.8175514732376996, 16.67166765953223617 ) ) ;
#72853 = EDGE_CURVE ( 'NONE', #8078, #65825, #25599, .T. ) ;
#72854 = ADVANCED_FACE ( 'NONE', ( #55466 ), #95035, .F. ) ;
#72855 = CARTESIAN_POINT ( 'NONE',  ( 70.33404001443909692, 61.26294760300035591, 14.79771436642047533 ) ) ;
#72856 = CARTESIAN_POINT ( 'NONE',  ( 189.8520780095588805, 286.5250076688263334, 16.49189287256407610 ) ) ;
#72857 = CARTESIAN_POINT ( 'NONE',  ( 72.20842434904899676, 71.50474725277734933, 5.031331199130571363 ) ) ;
#72858 = CARTESIAN_POINT ( 'NONE',  ( 87.32127743178345725, 44.99235608909022233, -6.181280657231217113 ) ) ;
#72859 = CARTESIAN_POINT ( 'NONE',  ( 125.2349645446896886, 253.1115022471903160, -5.000000000000047962 ) ) ;
#72860 = CARTESIAN_POINT ( 'NONE',  ( 157.1269483542914998, 258.4951375425532092, -17.15328932028234377 ) ) ;
#72861 = DIRECTION ( 'NONE',  ( 1.000000000000000000, 0.000000000000000000, 0.000000000000000000 ) ) ;
#72862 = ORIENTED_EDGE ( 'NONE', *, *, #34805, .T. ) ;
#72863 = CARTESIAN_POINT ( 'NONE',  ( 165.7251599921764864, 247.0382640774007541, -1.865539601759665933 ) ) ;
#72864 = VERTEX_POINT ( 'NONE', #8887 ) ;
#72865 = CARTESIAN_POINT ( 'NONE',  ( 162.7644741734472120, 248.7306563947940958, 9.865755277559742353 ) ) ;
#72866 = DIRECTION ( 'NONE',  ( -0.8660254037844387076, -0.4999999999999998890, -0.000000000000000000 ) ) ;
#72867 = CARTESIAN_POINT ( 'NONE',  ( -72.39633208959961053, 47.04162880533178992, 10.00000000000000000 ) ) ;
#72868 = VERTEX_POINT ( 'NONE', #85960 ) ;
#72869 = CARTESIAN_POINT ( 'NONE',  ( 77.31286743954092344, 63.20723050550007827, -15.22062317857226965 ) ) ;
#72870 = EDGE_LOOP ( 'NONE', ( #45375, #99038, #38192, #84775 ) ) ;
#72871 = CARTESIAN_POINT ( 'NONE',  ( 192.8220505326807199, 292.3911712377218350, 15.11976871725602933 ) ) ;
#72872 = CYLINDRICAL_SURFACE ( 'NONE', #8707, 5.000000000000058620 ) ;
#72873 = CARTESIAN_POINT ( 'NONE',  ( -19.65312891409030271, 93.06504152958497400, 59.99999999999999289 ) ) ;
#72874 = CARTESIAN_POINT ( 'NONE',  ( 191.6148588865760871, 296.7603242537468873, -11.89382487812838995 ) ) ;
#72875 = VERTEX_POINT ( 'NONE', #71210 ) ;
#72876 = CARTESIAN_POINT ( 'NONE',  ( 102.2852913444020686, 239.8615022471903160, 5.000000000000046185 ) ) ;
#72877 = CARTESIAN_POINT ( 'NONE',  ( 27.74993340135630859, 36.99752408145592852, 5.678558825948276656 ) ) ;
#72878 = CARTESIAN_POINT ( 'NONE',  ( 81.31198753610523511, 48.79742522285970807, -13.59794317573495981 ) ) ;
#72879 = CARTESIAN_POINT ( 'NONE',  ( 158.4316519640294132, 269.2869727094641235, -16.76269917448883717 ) ) ;
#72880 = CARTESIAN_POINT ( 'NONE',  ( 44.12520995882072583, 207.8297689869269220, -2.679491924311252493 ) ) ;
#72881 = ORIENTED_EDGE ( 'NONE', *, *, #37382, .F. ) ;
#72882 = ORIENTED_EDGE ( 'NONE', *, *, #99831, .T. ) ;
#72883 = CARTESIAN_POINT ( 'NONE',  ( 183.4103682618680295, 295.6271469934868605, 7.008542154348483599 ) ) ;
#72885 = EDGE_CURVE ( 'NONE', #33130, #56117, #8003, .T. ) ;
#72884 = B_SPLINE_CURVE_WITH_KNOTS ( 'NONE', 3,
 ( #72526, #31985, #47681, #32993 ),
 .UNSPECIFIED., .F., .F.,
 ( 4, 4 ),
 ( 0.01401801354063230039, 0.02268410888174763121 ),
 .UNSPECIFIED. ) ;
#72887 = CARTESIAN_POINT ( 'NONE',  ( 194.7900911235093133, 293.2606606935473792, -14.66228443412922999 ) ) ;
#72886 = CARTESIAN_POINT ( 'NONE',  ( 163.9587364689194260, 246.6621334214722481, 5.816126667419880825 ) ) ;
#72888 = CARTESIAN_POINT ( 'NONE',  ( 85.75771426040881806, 48.69409737863756504, -11.92208042066353535 ) ) ;
#72889 = DIRECTION ( 'NONE',  ( -0.8660254037844359321, -0.5000000000000051070, -0.000000000000000000 ) ) ;
#72890 = CARTESIAN_POINT ( 'NONE',  ( 131.9051165326627881, 235.4155109091896065, 2.679491924311254714 ) ) ;
#72891 = DIRECTION ( 'NONE',  ( -0.8660254037844379305, -0.5000000000000014433, -0.000000000000000000 ) ) ;
#72892 = CARTESIAN_POINT ( 'NONE',  ( 164.7632660535861930, 245.2686473046373692, 4.980011448959140274 ) ) ;
#72893 = AXIS2_PLACEMENT_3D ( 'NONE', #14759, #83708, #29466 ) ;
#72894 = CARTESIAN_POINT ( 'NONE',  ( 169.7896959808458632, 267.4449072945214994, 17.07133255476025724 ) ) ;
#72895 = CARTESIAN_POINT ( 'NONE',  ( -2.330697855141256269, 26.52822386297705393, -10.00000000000000000 ) ) ;
#72896 = EDGE_CURVE ( 'NONE', #46298, #85762, #32284, .T. ) ;
#72897 = CARTESIAN_POINT ( 'NONE',  ( 110.8105760068962127, 222.5327760586659736, 1.948934522072303157E-15 ) ) ;
#72898 = EDGE_LOOP ( 'NONE', ( #3454, #12041, #29356, #66726 ) ) ;
#72899 = LINE ( 'NONE', #11585, #75498 ) ;
#72900 = CARTESIAN_POINT ( 'NONE',  ( 166.2473226288001626, 277.8849993475402016, -13.37946549092444393 ) ) ;
#72901 = ORIENTED_EDGE ( 'NONE', *, *, #5083, .T. ) ;
#72902 = ORIENTED_EDGE ( 'NONE', *, *, #54513, .F. ) ;
#72903 = CARTESIAN_POINT ( 'NONE',  ( 189.3775153017087973, 300.6355170167246911, -1.634152055493470757 ) ) ;
#72904 = ADVANCED_FACE ( 'NONE', ( #16486 ), #9486, .F. ) ;
#72905 = CARTESIAN_POINT ( 'NONE',  ( 71.38860822316976851, 59.37102963310187675, 15.21422888946525731 ) ) ;
#72906 = CARTESIAN_POINT ( 'NONE',  ( 85.19546613154977877, 42.46598081436301442, -0.1273095977939074364 ) ) ;
#72907 = CARTESIAN_POINT ( 'NONE',  ( 206.1062572280473546, 273.6604860535989587, -9.773577984388410300 ) ) ;
#72908 = CARTESIAN_POINT ( 'NONE',  ( 163.1685298068643988, 248.0308115086310465, 10.61953511350444046 ) ) ;
#72909 = CARTESIAN_POINT ( 'NONE',  ( 100.2557178503908517, 222.5643266524160140, 9.188101187500095079 ) ) ;
#72910 = ORIENTED_EDGE ( 'NONE', *, *, #62157, .T. ) ;
#72911 = AXIS2_PLACEMENT_3D ( 'NONE', #66414, #97341, #58788 ) ;
#72912 = VERTEX_POINT ( 'NONE', #88967 ) ;
#72913 = DIRECTION ( 'NONE',  ( -0.8660254037844387076, -0.4999999999999998890, -0.000000000000000000 ) ) ;
#72914 = ORIENTED_EDGE ( 'NONE', *, *, #98351, .T. ) ;
#72915 = CARTESIAN_POINT ( 'NONE',  ( 76.03425298724704362, 64.70400164203398674, -14.34693053486635606 ) ) ;
#72916 = CARTESIAN_POINT ( 'NONE',  ( 153.7130981888246026, 265.1850621614574948, 16.50407132121065246 ) ) ;
#72917 = CARTESIAN_POINT ( 'NONE',  ( 72.94457269381892672, 69.24349002572374445, -9.567436796043198299 ) ) ;
#72919 = CARTESIAN_POINT ( 'NONE',  ( -22.42236680055709641, 157.8615022471902591, 0.000000000000000000 ) ) ;
#72918 = CARTESIAN_POINT ( 'NONE',  ( 143.0428722300570143, 244.2048013555409511, 4.594050593750051981 ) ) ;
#72920 = CARTESIAN_POINT ( 'NONE',  ( -11.83159780365783398, 170.6427522451419065, 10.00000000000009237 ) ) ;
#72921 = DIRECTION ( 'NONE',  ( 0.8845109580947966288, -0.1124011590738275557, -0.4527762631246090574 ) ) ;
#72922 = ORIENTED_EDGE ( 'NONE', *, *, #88565, .F. ) ;
#72923 = CARTESIAN_POINT ( 'NONE',  ( 157.0150015346687553, 258.6890351218854676, 16.85538724311808068 ) ) ;
#72924 = CARTESIAN_POINT ( 'NONE',  ( 80.65166287433959269, 45.65901089857030115, 11.68184599996163797 ) ) ;
#72925 = B_SPLINE_CURVE_WITH_KNOTS ( 'NONE', 3,
 ( #87307, #95878, #47705, #78643, #9226, #9751, #10235, #25942, #70517, #32531, #72039, #41610, #64934, #40610, #71544, #62919, #63919, #94858, #2643, #17840, #40105, #18341, #49235, #80169, #33021, #10737, #71045, #8725, #1647, #63425, #94364, #33531, #3159, #86785, #55792, #39596, #48224, #2138, #25418, #64428, #95390, #34044, #26436, #57315, #32009, #93869, #24426, #55302 ),
 .UNSPECIFIED., .F., .F.,
 ( 4, 2, 2, 2, 2, 2, 2, 2, 2, 2, 2, 2, 2, 2, 2, 2, 2, 2, 2, 2, 2, 2, 2, 4 ),
 ( 0.0002174362994174117863, 0.001238585736266362711, 0.001749160454690868328, 0.002004447813903081996, 0.002132091493509117273, 0.002259735173115152550, 0.002387378852721187394, 0.002515022532327222671, 0.002770309891539291490, 0.003280884609963429562, 0.004302034046811783335, 0.005323183483660138410, 0.005833758202084277783, 0.006089045561296346602, 0.006344332920508415422, 0.006408154760311396414, 0.006471976600114376539, 0.006535798439917356664, 0.006599620279720337657, 0.006854907638932357904, 0.007365482357356391459, 0.007620769716568408236, 0.007876057075780427616, 0.008386631794204362292 ),
 .UNSPECIFIED. ) ;
#72926 = CARTESIAN_POINT ( 'NONE',  ( 82.28003896804979433, 40.62557011389661454, -3.142018250930367795 ) ) ;
#72927 = CARTESIAN_POINT ( 'NONE',  ( 188.8786019601460282, 269.6712879289298144, 14.62574647380142778 ) ) ;
#72928 = CARTESIAN_POINT ( 'NONE',  ( -22.42236680055709641, 157.8615022471902591, 0.000000000000000000 ) ) ;
#72929 = DIRECTION ( 'NONE',  ( -0.5000000000000003331, 0.8660254037844383745, 0.000000000000000000 ) ) ;
#72930 = FACE_OUTER_BOUND ( 'NONE', #54852, .T. ) ;
#72931 = DIRECTION ( 'NONE',  ( -1.000000000000000000, 0.000000000000000000, 0.000000000000000000 ) ) ;
#72932 = CARTESIAN_POINT ( 'NONE',  ( 153.5324998095718456, 266.8834243315761796, 16.61741842784684664 ) ) ;
#72933 = CARTESIAN_POINT ( 'NONE',  ( 85.70872427756812328, 44.59920998664200198, 7.110704347725950392 ) ) ;
#72934 = CARTESIAN_POINT ( 'NONE',  ( 206.8106726053982811, 272.4404028303941914, -10.47827087991598560 ) ) ;
#72935 = CARTESIAN_POINT ( 'NONE',  ( 78.04004269445073305, 61.96668518898951561, 15.68684486111242293 ) ) ;
#72936 = CARTESIAN_POINT ( 'NONE',  ( 175.0025046748339435, 290.6155586575834491, -6.507390672453347236 ) ) ;
#72937 = EDGE_CURVE ( 'NONE', #39006, #4740, #59455, .T. ) ;
#72938 = CARTESIAN_POINT ( 'NONE',  ( -17.42236680055705023, 149.2012482093457777, 0.000000000000000000 ) ) ;
#72939 = CARTESIAN_POINT ( 'NONE',  ( 207.6508796976096107, 270.9851214578045528, 6.713685698622268383 ) ) ;
#72940 = CARTESIAN_POINT ( 'NONE',  ( 74.32104487728463482, 55.32907616431677411, 16.60218531702808065 ) ) ;
#72941 = CARTESIAN_POINT ( 'NONE',  ( 69.64695893572810803, 221.0177522451419065, 5.000000000000046185 ) ) ;
#72942 = CARTESIAN_POINT ( 'NONE',  ( 34.10980067877857635, 31.64441083166263269, -10.00000000000000533 ) ) ;
#72943 = CARTESIAN_POINT ( 'NONE',  ( -22.42236680055709641, 157.8615022471902591, 0.000000000000000000 ) ) ;
#72944 = FACE_OUTER_BOUND ( 'NONE', #50825, .T. ) ;
#72945 = DIRECTION ( 'NONE',  ( -0.5000000000000002220, 0.8660254037844384856, 0.000000000000000000 ) ) ;
#72946 = CARTESIAN_POINT ( 'NONE',  ( 160.9223551016720251, 273.3990656506861683, -15.46406356478478195 ) ) ;
#72947 = CARTESIAN_POINT ( 'NONE',  ( 86.86181906774642414, 43.72161649829373431, -3.208833253784785011 ) ) ;
#72948 = CARTESIAN_POINT ( 'NONE',  ( 161.1492466472929266, 251.5283125358769212, -13.33353587056634915 ) ) ;
#72949 = CARTESIAN_POINT ( 'NONE',  ( 23.85612603422365297, 175.3923013555409796, 4.594050593750050204 ) ) ;
#72950 = CARTESIAN_POINT ( 'NONE',  ( -28.04097607764120781, 24.82386083235215679, -10.00000000000000000 ) ) ;
#72951 = VERTEX_POINT ( 'NONE', #27604 ) ;
#72952 = CARTESIAN_POINT ( 'NONE',  ( 86.78549426258132371, 45.83013854792883279, 8.849882187839877901 ) ) ;
#72953 = CARTESIAN_POINT ( 'NONE',  ( 88.42017002704760387, 43.92753743058676719, 1.721442031696316377 ) ) ;
#72954 = CARTESIAN_POINT ( 'NONE',  ( 207.8302079587528794, 270.6745157982714431, 3.572475529330238153 ) ) ;
#72955 = LINE ( 'NONE', #18239, #56596 ) ;
#72956 = CARTESIAN_POINT ( 'NONE',  ( 36.52174756457106497, 182.7048013555409796, 4.594050593750051981 ) ) ;
#72957 = CARTESIAN_POINT ( 'NONE',  ( 200.6097954076514895, 283.1806371883870383, 16.82611162221071766 ) ) ;
#72958 = CARTESIAN_POINT ( 'NONE',  ( 147.2494378675467033, 275.6034875578896504, 3.639370109197119341 ) ) ;
#72959 = CARTESIAN_POINT ( 'NONE',  ( 32.74284248606149106, 41.83705186507756224, 3.090169943749475401 ) ) ;
#72960 = CARTESIAN_POINT ( 'NONE',  ( 181.7502401732105000, 294.1801057147719121, 6.322034055514200723 ) ) ;
#72961 = CARTESIAN_POINT ( 'NONE',  ( 146.6834825911944620, 276.5837508513432681, 0.6716460511724984261 ) ) ;
#72962 = CARTESIAN_POINT ( 'NONE',  ( 178.7151539974932462, 270.9650308319119176, 17.63195993801104677 ) ) ;
#72963 = LINE ( 'NONE', #49143, #67050 ) ;
#72964 = CARTESIAN_POINT ( 'NONE',  ( 84.34903687182406884, 231.0530062829863027, -4.648177544792955347E-16 ) ) ;
#72965 = CARTESIAN_POINT ( 'NONE',  ( 74.39841895140679640, 68.21392270468032848, 11.95628786500076934 ) ) ;
#72966 = ADVANCED_FACE ( 'NONE', ( #90436 ), #14500, .F. ) ;
#72967 = EDGE_CURVE ( 'NONE', #66065, #63171, #57500, .T. ) ;
#72968 = VECTOR ( 'NONE', #51962, 1000.000000000000000 ) ;
#72969 = CARTESIAN_POINT ( 'NONE',  ( 89.36707907128422335, 215.7365022471902023, 10.00000000000009592 ) ) ;
#72970 = CARTESIAN_POINT ( 'NONE',  ( 13.51768745649711789, 178.6115022471902591, 10.00000000000009592 ) ) ;
#72971 = CARTESIAN_POINT ( 'NONE',  ( 53.16558651961199899, 195.3768266524160140, 9.188101187500098632 ) ) ;
#72972 = ORIENTED_EDGE ( 'NONE', *, *, #41389, .F. ) ;
#72973 = CARTESIAN_POINT ( 'NONE',  ( -18.15312891409030982, 79.21382371532438071, 13.90677182048132998 ) ) ;
#72974 = CARTESIAN_POINT ( 'NONE',  ( 190.1858949294064871, 301.2353624297489887, -5.249932979468886707 ) ) ;
#72975 = CARTESIAN_POINT ( 'NONE',  ( 67.44824590140864018, 66.75839308862164501, -8.448268966284212311 ) ) ;
#72976 = VERTEX_POINT ( 'NONE', #74713 ) ;
#72977 = CARTESIAN_POINT ( 'NONE',  ( 167.4464793182998221, 285.4026007275220422, 7.926851182865696899 ) ) ;
#72978 = DIRECTION ( 'NONE',  ( 0.9041295198386993803, -0.4272584830711297910, 0.000000000000000000 ) ) ;
#72979 = LINE ( 'NONE', #42045, #65540 ) ;
#72980 = CARTESIAN_POINT ( 'NONE',  ( 30.88926192328758447, 20.76004757982090609, 5.678558825948272215 ) ) ;
#72981 = CARTESIAN_POINT ( 'NONE',  ( 189.1222366604172294, 265.5048954663608924, 10.64636282005728596 ) ) ;
#72982 = CARTESIAN_POINT ( 'NONE',  ( 86.16184129357679922, 46.97112889942257397, -10.09731433673572276 ) ) ;
#72983 = CARTESIAN_POINT ( 'NONE',  ( 171.3148662694858331, 255.7789367394895237, 12.02744102109133628 ) ) ;
#72984 = VERTEX_POINT ( 'NONE', #97035 ) ;
#72985 = CARTESIAN_POINT ( 'NONE',  ( 15.78914702631840150, 24.51421378149918695, -9.188101187500004485 ) ) ;
#72986 = CARTESIAN_POINT ( 'NONE',  ( 198.7634891777862549, 264.9856665559012185, 0.1351954043397823324 ) ) ;
#72987 = CARTESIAN_POINT ( 'NONE',  ( 172.2873880799365338, 253.3886587257176473, 8.406275390072382336 ) ) ;
#72988 = DIRECTION ( 'NONE',  ( -0.8660254037844387076, -0.4999999999999998890, -0.000000000000000000 ) ) ;
#72989 = EDGE_LOOP ( 'NONE', ( #44944, #696, #16071, #80935 ) ) ;
#72990 = CARTESIAN_POINT ( 'NONE',  ( 72.34188612886940462, 71.14473754787812254, -6.071946735866348810 ) ) ;
#72991 = CARTESIAN_POINT ( 'NONE',  ( 151.4025156491502742, 268.4101458323662541, 14.71049357081981235 ) ) ;
#72992 = DIRECTION ( 'NONE',  ( -0.000000000000000000, -0.000000000000000000, -1.000000000000000000 ) ) ;
#72993 = DIRECTION ( 'NONE',  ( -0.000000000000000000, 0.000000000000000000, 1.000000000000000000 ) ) ;
#72994 = ORIENTED_EDGE ( 'NONE', *, *, #43447, .F. ) ;
#72995 = ORIENTED_EDGE ( 'NONE', *, *, #64630, .F. ) ;
#72996 = EDGE_CURVE ( 'NONE', #60981, #59884, #22523, .T. ) ;
#72998 = CARTESIAN_POINT ( 'NONE',  ( -22.42236680055709641, 157.8615022471902591, 0.000000000000000000 ) ) ;
#72997 = CARTESIAN_POINT ( 'NONE',  ( 161.8750289368003621, 250.2712207352165592, -13.97436367953006098 ) ) ;
#72999 = CARTESIAN_POINT ( 'NONE',  ( 184.1482295286804458, 294.7143494075100421, -9.263004813192097231 ) ) ;
#73000 = ORIENTED_EDGE ( 'NONE', *, *, #71996, .T. ) ;
#73001 = CARTESIAN_POINT ( 'NONE',  ( 65.87995410094603699, 68.93345956842472333, -2.563197177700018425 ) ) ;
#73002 = CARTESIAN_POINT ( 'NONE',  ( 197.9952413503812352, 287.7091776547143809, 17.17611241386010690 ) ) ;
#73003 = CARTESIAN_POINT ( 'NONE',  ( 72.59318330222436089, 57.33635058732104994, -16.33242561347062960 ) ) ;
#73004 = CARTESIAN_POINT ( 'NONE',  ( 77.84440724905273612, 61.40677674231441330, -16.14086307328630809 ) ) ;
#73005 = EDGE_CURVE ( 'NONE', #93038, #25226, #81826, .T. ) ;
#73006 = CARTESIAN_POINT ( 'NONE',  ( 157.4805323096970255, 257.8827121670497036, -16.70238855805511591 ) ) ;
#73007 = CARTESIAN_POINT ( 'NONE',  ( 121.9063529450018279, 235.0643266524160424, -9.188101187500093303 ) ) ;
#73008 = CARTESIAN_POINT ( 'NONE',  ( 74.41009865654258704, 203.7677522451417929, -5.000000000000041744 ) ) ;
#73009 = CARTESIAN_POINT ( 'NONE',  ( 207.5230514910949182, 271.2065264061283756, 2.678931747975364708 ) ) ;
#73010 = VERTEX_POINT ( 'NONE', #43267 ) ;
#73011 = CARTESIAN_POINT ( 'NONE',  ( 29.13557404741141355, 37.79752408145594700, -5.678558825948271327 ) ) ;
#73012 = FACE_BOUND ( 'NONE', #50998, .T. ) ;
#73013 = CARTESIAN_POINT ( 'NONE',  ( 78.26893986734688724, 47.80136226004309208, -14.50496253017350767 ) ) ;
#73014 = CARTESIAN_POINT ( 'NONE',  ( 71.13526655237410523, 218.0024278399160664, 9.188101187500095079 ) ) ;
#73015 = CARTESIAN_POINT ( 'NONE',  ( -30.13607937982481744, 95.41016082721114344, 12.74739955043256501 ) ) ;
#73016 = CARTESIAN_POINT ( 'NONE',  ( 150.6790040019602088, 269.6633047651677089, 15.38315204620803378 ) ) ;
#73017 = CARTESIAN_POINT ( 'NONE',  ( 198.7606870255174272, 286.3833868549447743, 17.68329551240030284 ) ) ;
#73018 = CARTESIAN_POINT ( 'NONE',  ( 175.5753062590537752, 278.4498914399613909, 15.48226569750622694 ) ) ;
#73019 = VERTEX_POINT ( 'NONE', #73206 ) ;
#73020 = CARTESIAN_POINT ( 'NONE',  ( 78.00315723853645977, 57.40260998422804306, -16.18978363693141276 ) ) ;
#73021 = CARTESIAN_POINT ( 'NONE',  ( -46.74660806181546491, 29.87360136034011049, 10.00000000000000000 ) ) ;
#73022 = CARTESIAN_POINT ( 'NONE',  ( 86.66305821822952282, 42.85738816998053835, 1.351321920865392823 ) ) ;
#73023 = VERTEX_POINT ( 'NONE', #34681 ) ;
#73024 = CARTESIAN_POINT ( 'NONE',  ( 148.6879145481387638, 273.1119728616009752, 9.952982990420577991 ) ) ;
#73025 = CARTESIAN_POINT ( 'NONE',  ( 70.64645261124985609, 69.81531829990819915, -6.590501872596628452 ) ) ;
#73026 = CARTESIAN_POINT ( 'NONE',  ( 161.8750289368003621, 250.2712207352165592, -13.97436367953006098 ) ) ;
#73027 = CARTESIAN_POINT ( 'NONE',  ( 83.08469416262596496, 51.79154804246269350, -15.04490442047335641 ) ) ;
#73028 = CARTESIAN_POINT ( 'NONE',  ( 190.0445576990143195, 301.4801656937889902, 4.140328216824785912 ) ) ;
#73029 = ADVANCED_FACE ( 'NONE', ( #74213 ), #4803, .F. ) ;
#73030 = CARTESIAN_POINT ( 'NONE',  ( 206.0041637419966776, 273.8373171585603814, 11.66586596407113596 ) ) ;
#73031 = CARTESIAN_POINT ( 'NONE',  ( 206.4695239676918845, 273.0312896038346366, 10.41704154450801667 ) ) ;
#73032 = CARTESIAN_POINT ( 'NONE',  ( 125.8022308496927195, 254.9860189848785410, -2.679491924311252493 ) ) ;
#73033 = CARTESIAN_POINT ( 'NONE',  ( 166.9567796355807729, 256.1732514150568818, 13.73539047231146171 ) ) ;
#73034 = ORIENTED_EDGE ( 'NONE', *, *, #60928, .T. ) ;
#73035 = CARTESIAN_POINT ( 'NONE',  ( 164.2647213391612979, 246.1321520798662164, -5.830872732487307530 ) ) ;
#73036 = CARTESIAN_POINT ( 'NONE',  ( 128.2121871902485566, 235.6423013555409796, -4.594050593750043987 ) ) ;
#73037 = ORIENTED_EDGE ( 'NONE', *, *, #43432, .F. ) ;
#73038 = CARTESIAN_POINT ( 'NONE',  ( 146.5689048584090699, 276.7822053059436485, -0.4306668706573002492 ) ) ;
#73039 = CARTESIAN_POINT ( 'NONE',  ( 90.50373741020339935, 216.3927522451418213, 10.00000000000009948 ) ) ;
#73040 = CARTESIAN_POINT ( 'NONE',  ( 205.3549208985294001, 273.3626630250829521, -10.87845838788729758 ) ) ;
#73041 = CARTESIAN_POINT ( 'NONE',  ( 164.2297246530060875, 246.1927681183832988, 5.803160395959773510 ) ) ;
#73042 = CARTESIAN_POINT ( 'NONE',  ( 75.18665594272103192, 63.32462222244616612, 14.68879760224534436 ) ) ;
#73043 = CARTESIAN_POINT ( 'NONE',  ( 175.7520323455595417, 252.2218298946914388, 4.007223628156822315 ) ) ;
#73044 = VERTEX_POINT ( 'NONE', #43769 ) ;
#73045 = CARTESIAN_POINT ( 'NONE',  ( 80.25178558894602077, 57.14685393251871659, -16.23521980932008546 ) ) ;
#73046 = CARTESIAN_POINT ( 'NONE',  ( 71.65939579155516981, 72.09010134313686535, 0.6730539622211891837 ) ) ;
#73048 = CARTESIAN_POINT ( 'NONE',  ( -74.97640825042664403, 52.25402898078436920, -10.00000000000000000 ) ) ;
#73047 = DIRECTION ( 'NONE',  ( -0.8660254037844387076, -0.4999999999999998890, -0.000000000000000000 ) ) ;
#73049 = CARTESIAN_POINT ( 'NONE',  ( 164.9590787296926067, 244.9294898008548387, -2.278052160087662870 ) ) ;
#73050 = CARTESIAN_POINT ( 'NONE',  ( 138.6312950077063135, 250.8458772461660260, 9.188101187500095079 ) ) ;
#73051 = CARTESIAN_POINT ( 'NONE',  ( 184.9432817549989352, 285.0648861408565722, 16.61117941084251726 ) ) ;
#73052 = CARTESIAN_POINT ( 'NONE',  ( 68.33041130487251280, 69.19949468873031151, 4.826233711656780834 ) ) ;
#73053 = CARTESIAN_POINT ( 'NONE',  ( 170.9566650728496882, 250.6362774811119891, 3.411191216732029297 ) ) ;
#73054 = CARTESIAN_POINT ( 'NONE',  ( 14.11247099069668742, 31.08080186712592052, -3.090169943749475845 ) ) ;
#73055 = CARTESIAN_POINT ( 'NONE',  ( 149.4539134692060145, 271.7852238117696402, 12.95627816374690688 ) ) ;
#73056 = CARTESIAN_POINT ( 'NONE',  ( 41.76871284172324295, 36.06628583063844928, -9.188101187500006262 ) ) ;
#73058 = CARTESIAN_POINT ( 'NONE',  ( 171.9374462982776492, 287.8333287246510963, -8.532231483866285160 ) ) ;
#73057 = B_SPLINE_CURVE_WITH_KNOTS ( 'NONE', 3,
 ( #81591, #11180, #42047, #12160, #3572, #34453, #29353, #60217, #67850, #68333, #30340, #92194, #39778, #94054, #60713, #91181, #9416, #76457, #59732, #98771, #86474, #70709, #84095, #37425 ),
 .UNSPECIFIED., .F., .F.,
 ( 4, 2, 2, 2, 2, 2, 2, 2, 2, 2, 2, 4 ),
 ( 0.000000000000000000, 0.1249999999999923395, 0.2499999999999846789, 0.3749999999999770184, 0.4374999999999794054, 0.4999999999999817923, 0.5624999999999841238, 0.6249999999999865663, 0.6874999999999888978, 0.7499999999999913403, 0.8749999999999956701, 1.000000000000000000 ),
 .UNSPECIFIED. ) ;
#73059 = CARTESIAN_POINT ( 'NONE',  ( 159.3291946290163992, 279.0199804063916531, 10.96233109238993109 ) ) ;
#73060 = CARTESIAN_POINT ( 'NONE',  ( 193.6579322423270355, 288.5700127970677045, 16.06830834735240643 ) ) ;
#73061 = CARTESIAN_POINT ( 'NONE',  ( 128.9696990949622091, 245.2677522451418497, 10.00000000000009592 ) ) ;
#73062 = CARTESIAN_POINT ( 'NONE',  ( 83.41434387094278691, 50.95609258043517542, -14.15981904929085822 ) ) ;
#73063 = ORIENTED_EDGE ( 'NONE', *, *, #25001, .F. ) ;
#73064 = CARTESIAN_POINT ( 'NONE',  ( 196.4677418905696129, 290.3548843276421394, 17.08610552292358520 ) ) ;
#73065 = CARTESIAN_POINT ( 'NONE',  ( 148.3997536239841679, 273.6110822229926498, 8.713694244701960301 ) ) ;
#73066 = CARTESIAN_POINT ( 'NONE',  ( -3.992090130160959482, 162.3768266524160140, 9.188101187500096856 ) ) ;
#73067 = CARTESIAN_POINT ( 'NONE',  ( 43.09804120061789945, 189.5643266524160140, 9.188101187500095079 ) ) ;
#73068 = CARTESIAN_POINT ( 'NONE',  ( 178.5061629747377765, 273.6775914088984223, -17.34296752049866086 ) ) ;
#73069 = CARTESIAN_POINT ( 'NONE',  ( 13.69028360280385570, 30.83705186507753382, 3.090169943749475401 ) ) ;
#73070 = CARTESIAN_POINT ( 'NONE',  ( 88.07426949318437437, 43.62472922332415237, 0.07787791115677776543 ) ) ;
#73071 = CARTESIAN_POINT ( 'NONE',  ( 157.0877926458200307, 258.5629572190321710, -17.40668770468195703 ) ) ;
#73072 = CARTESIAN_POINT ( 'NONE',  ( 72.28747768279822594, 72.05077469953971558, -3.362523527234974718 ) ) ;
#73073 = CARTESIAN_POINT ( 'NONE',  ( 190.1813752874636805, 301.2431906792259042, -4.710625539811892359 ) ) ;
#73074 = CARTESIAN_POINT ( 'NONE',  ( 73.78486849093569333, 55.14556177349142274, -16.59920503071222697 ) ) ;
#73076 = CARTESIAN_POINT ( 'NONE',  ( 61.41971759977597145, 206.2677522451418781, 10.00000000000009592 ) ) ;
#73075 = CARTESIAN_POINT ( 'NONE',  ( 168.1589593212097498, 275.9390298053305628, -16.40258036402506647 ) ) ;
#73077 = CARTESIAN_POINT ( 'NONE',  ( 74.86380167504295002, 67.20554747851282684, 12.49214931513423466 ) ) ;
#73078 = CARTESIAN_POINT ( 'NONE',  ( 204.7764732025852084, 275.9637395487929439, -14.02287343454361412 ) ) ;
#73079 = CARTESIAN_POINT ( 'NONE',  ( 169.3846196238007735, 270.7800964535849744, -17.72459440982018108 ) ) ;
#73080 = EDGE_CURVE ( 'NONE', #85089, #12428, #5290, .T. ) ;
#73081 = B_SPLINE_CURVE_WITH_KNOTS ( 'NONE', 3,
 ( #76422, #6511, #68293, #92635 ),
 .UNSPECIFIED., .F., .F.,
 ( 4, 4 ),
 ( 0.02105975151895524838, 0.02524676605399324425 ),
 .UNSPECIFIED. ) ;
#73082 = EDGE_CURVE ( 'NONE', #99484, #17163, #12980, .T. ) ;
#73083 = CARTESIAN_POINT ( 'NONE',  ( 179.7192414948235069, 294.1200435161542828, 1.033553133877518126 ) ) ;
#73084 = CARTESIAN_POINT ( 'NONE',  ( 47.29267820409023670, 198.1115022471902591, 10.00000000000009592 ) ) ;
#73085 = CARTESIAN_POINT ( 'NONE',  ( 184.9287284004330729, 293.9407481508790170, 9.651135569905934020 ) ) ;
#73086 = CARTESIAN_POINT ( 'NONE',  ( 203.0398866899141126, 278.9715956204779559, 16.57839218037009132 ) ) ;
#73087 = CARTESIAN_POINT ( 'NONE',  ( 6.887527552763561545, 162.5327760586659736, 1.948934522072303157E-15 ) ) ;
#73088 = CARTESIAN_POINT ( 'NONE',  ( 37.43858582280105907, 33.56628583063844218, 9.188101187500006262 ) ) ;
#73089 = FACE_OUTER_BOUND ( 'NONE', #80378, .T. ) ;
#73090 = EDGE_CURVE ( 'NONE', #82635, #35356, #99858, .T. ) ;
#73091 = CARTESIAN_POINT ( 'NONE',  ( 153.1745822862813498, 265.3408363824576668, 16.18092354043443493 ) ) ;
#73092 = CARTESIAN_POINT ( 'NONE',  ( 35.70653501523218409, 32.56628583063843507, 9.188101187500006262 ) ) ;
#73093 = CARTESIAN_POINT ( 'NONE',  ( 84.11911179316838627, 207.8262482093457777, 3.021315404115420679E-15 ) ) ;
#73094 = B_SPLINE_CURVE_WITH_KNOTS ( 'NONE', 3,
 ( #86367, #56400, #87395, #1215 ),
 .UNSPECIFIED., .F., .F.,
 ( 4, 4 ),
 ( 0.02632407315735414005, 0.03555975659152819934 ),
 .UNSPECIFIED. ) ;
#73095 = CARTESIAN_POINT ( 'NONE',  ( 182.0984742165180705, 278.2391700500209026, 16.50274708701968862 ) ) ;
#73096 = CARTESIAN_POINT ( 'NONE',  ( 80.75837978203962564, 43.06974379819217091, -9.769810117882439471 ) ) ;
#73097 = DIRECTION ( 'NONE',  ( -0.5000000000000014433, 0.8660254037844379305, 0.000000000000000000 ) ) ;
#73098 = CARTESIAN_POINT ( 'NONE',  ( 176.6391464052069296, 260.6212487597024392, -13.24495383745690447 ) ) ;
#73099 = DIRECTION ( 'NONE',  ( 1.000000000000000000, 0.000000000000000000, 0.000000000000000000 ) ) ;
#73100 = CARTESIAN_POINT ( 'NONE',  ( 7.739928672529463149, 22.65586893147754211, -7.433330006724137462 ) ) ;
#73101 = CARTESIAN_POINT ( 'NONE',  ( 126.7089641099561845, 232.4155109091895781, 2.679491924311254714 ) ) ;
#73102 = CARTESIAN_POINT ( 'NONE',  ( 10.75418485208671804, 27.18502408145590366, 5.678558825948276656 ) ) ;
#73103 = PLANE ( 'NONE',  #42446 ) ;
#73104 = CARTESIAN_POINT ( 'NONE',  ( 189.5534384022301424, 269.0062095459838929, -14.92796778812864922 ) ) ;
#73105 = EDGE_LOOP ( 'NONE', ( #5212, #91829, #27016, #77832 ) ) ;
#73106 = CARTESIAN_POINT ( 'NONE',  ( 156.7117516780912183, 276.4586797656536419, 10.26618125257395242 ) ) ;
#73107 = FACE_OUTER_BOUND ( 'NONE', #68346, .T. ) ;
#73108 = ORIENTED_EDGE ( 'NONE', *, *, #15521, .F. ) ;
#73109 = CARTESIAN_POINT ( 'NONE',  ( 152.7153488183568300, 266.1362520814392951, 17.33540622643059237 ) ) ;
#73110 = CARTESIAN_POINT ( 'NONE',  ( 206.9059968923335475, 272.2752963222270068, 6.902135944297345560 ) ) ;
#73111 = DIRECTION ( 'NONE',  ( -0.9946578707245746775, -0.1032265479692855564, 0.000000000000000000 ) ) ;
#73112 = CARTESIAN_POINT ( 'NONE',  ( 87.42157367659969225, 45.50835484090782046, 7.071803456770564544 ) ) ;
#73113 = AXIS2_PLACEMENT_3D ( 'NONE', #28454, #19405, #50756 ) ;
#73114 = ORIENTED_EDGE ( 'NONE', *, *, #5791, .T. ) ;
#73115 = VERTEX_POINT ( 'NONE', #37657 ) ;
#73117 = LINE ( 'NONE', #39786, #76846 ) ;
#73116 = CARTESIAN_POINT ( 'NONE',  ( 159.7424789065890991, 278.4861631006231732, -9.771801590140540839 ) ) ;
#73118 = CARTESIAN_POINT ( 'NONE',  ( 86.67919437798869353, 47.13106718819364716, 10.49222478779208068 ) ) ;
#73119 = ORIENTED_EDGE ( 'NONE', *, *, #37503, .T. ) ;
#73120 = CARTESIAN_POINT ( 'NONE',  ( 46.50192534792603283, 74.36443251879779837, -10.00000000000000000 ) ) ;
#73121 = CARTESIAN_POINT ( 'NONE',  ( 174.3220357038730128, 262.5849746787575327, 15.23774525505547395 ) ) ;
#73122 = ORIENTED_EDGE ( 'NONE', *, *, #22287, .T. ) ;
#73123 = CARTESIAN_POINT ( 'NONE',  ( 33.24377527499414242, 31.14441083166263269, 10.00000000000000533 ) ) ;
#73124 = CARTESIAN_POINT ( 'NONE',  ( 80.18890285298550680, 49.85588249849323716, -14.45051987738599486 ) ) ;
#73125 = CARTESIAN_POINT ( 'NONE',  ( 196.9319848161575806, 289.5507919934690335, -17.64330560362266453 ) ) ;
#73126 = CARTESIAN_POINT ( 'NONE',  ( 42.00631479827483616, 188.3927522451417929, -10.00000000000009237 ) ) ;
#73127 = ORIENTED_EDGE ( 'NONE', *, *, #59099, .T. ) ;
#73128 = CARTESIAN_POINT ( 'NONE',  ( 200.7079229450794173, 283.0106753079404029, 16.90512463913211505 ) ) ;
#73129 = CARTESIAN_POINT ( 'NONE',  ( 169.5268067963925205, 276.4064337483826534, -15.74407357586045464 ) ) ;
#73130 = DIRECTION ( 'NONE',  ( -0.000000000000000000, -0.000000000000000000, -1.000000000000000000 ) ) ;
#73131 = EDGE_LOOP ( 'NONE', ( #5819, #73225, #48879, #94504 ) ) ;
#73132 = CARTESIAN_POINT ( 'NONE',  ( 174.6031362836316703, 276.7578777746297760, -16.67970167110237512 ) ) ;
#73133 = CARTESIAN_POINT ( 'NONE',  ( 163.3854574543125580, 247.6550818016845597, 10.82482370245618775 ) ) ;
#73134 = EDGE_LOOP ( 'NONE', ( #55425, #76754, #68745, #18258 ) ) ;
#73135 = DIRECTION ( 'NONE',  ( -0.8660254037844387076, -0.4999999999999998890, -0.000000000000000000 ) ) ;
#73136 = ORIENTED_EDGE ( 'NONE', *, *, #90616, .F. ) ;
#73137 = FACE_OUTER_BOUND ( 'NONE', #25772, .T. ) ;
#73138 = ORIENTED_EDGE ( 'NONE', *, *, #11169, .F. ) ;
#73139 = CARTESIAN_POINT ( 'NONE',  ( 147.9079810727873223, 274.4628572674334919, 6.305649893024213526 ) ) ;
#73140 = CARTESIAN_POINT ( 'NONE',  ( 178.6359132194422727, 289.6913899023020917, -9.365969567067413237 ) ) ;
#73141 = CARTESIAN_POINT ( 'NONE',  ( 192.5455529438217468, 269.1281655793299592, -13.93448690431165105 ) ) ;
#73142 = CARTESIAN_POINT ( 'NONE',  ( 192.6030823458456780, 295.3171989905301871, 13.41425101105791384 ) ) ;
#73143 = CARTESIAN_POINT ( 'NONE',  ( 86.99613933060332727, 43.49019189568694799, 1.303767148709912505 ) ) ;
#73144 = CARTESIAN_POINT ( 'NONE',  ( 197.2708468743591652, 288.9638656919068467, -16.67412905307064008 ) ) ;
#73145 = EDGE_CURVE ( 'NONE', #70099, #15824, #76678, .T. ) ;
#73146 = ORIENTED_EDGE ( 'NONE', *, *, #87559, .T. ) ;
#73147 = CARTESIAN_POINT ( 'NONE',  ( 38.52196584993465223, 56.41980893122115504, 10.00000000000000000 ) ) ;
#73148 = CARTESIAN_POINT ( 'NONE',  ( 20.47532000956703513, 32.79752408145593279, -5.678558825948271327 ) ) ;
#73149 = ADVANCED_FACE ( 'NONE', ( #30072 ), #54345, .F. ) ;
#73150 = AXIS2_PLACEMENT_3D ( 'NONE', #62457, #75339, #23465 ) ;
#73152 = LINE ( 'NONE', #88396, #56352 ) ;
#73151 = CARTESIAN_POINT ( 'NONE',  ( 77.41810753117228217, 49.76551275768444782, -14.98827377503008584 ) ) ;
#73154 = ORIENTED_EDGE ( 'NONE', *, *, #88798, .F. ) ;
#73153 = CARTESIAN_POINT ( 'NONE',  ( 159.7897726928491409, 253.8829904965402875, 16.83923858130328810 ) ) ;
#73155 = ORIENTED_EDGE ( 'NONE', *, *, #45758, .F. ) ;
#73156 = CARTESIAN_POINT ( 'NONE',  ( 147.1020895757533538, 275.8587022856839326, -2.572889012152433708 ) ) ;
#73157 = CARTESIAN_POINT ( 'NONE',  ( 69.62506531815498079, 62.65334623341696840, 13.89417082518318836 ) ) ;
#73158 = CARTESIAN_POINT ( 'NONE',  ( 23.64814127513160358, 118.0650415295850166, 25.00000000000000000 ) ) ;
#73159 = CARTESIAN_POINT ( 'NONE',  ( 126.8249895137406043, 232.4824982072973683, 3.021315404115420679E-15 ) ) ;
#73160 = EDGE_CURVE ( 'NONE', #34200, #24743, #53899, .T. ) ;
#73161 = CARTESIAN_POINT ( 'NONE',  ( 160.4075704321521130, 252.8129334232662586, -14.67865048504329906 ) ) ;
#73162 = CARTESIAN_POINT ( 'NONE',  ( 148.5298631380253767, 273.3857259341252757, -8.957191713326388083 ) ) ;
#73163 = ORIENTED_EDGE ( 'NONE', *, *, #93807, .T. ) ;
#73164 = DIRECTION ( 'NONE',  ( -0.8660254037844387076, -0.4999999999999998890, -0.000000000000000000 ) ) ;
#73165 = CARTESIAN_POINT ( 'NONE',  ( 39.80235952159635815, 84.99999999999998579, -10.00000000000000000 ) ) ;
#73166 = CARTESIAN_POINT ( 'NONE',  ( 133.7328388157766312, 238.0177522451417929, 5.000000000000051514 ) ) ;
#73168 = EDGE_CURVE ( 'NONE', #12913, #57260, #8109, .T. ) ;
#73167 = CARTESIAN_POINT ( 'NONE',  ( 164.8670003495851404, 245.0889742334797177, -1.557028074864921674 ) ) ;
#73169 = CARTESIAN_POINT ( 'NONE',  ( 32.84087927488944558, 199.7677522451419350, -5.000000000000047962 ) ) ;
#73170 = CARTESIAN_POINT ( 'NONE',  ( 99.66015183740654493, 228.3458772461660544, 9.188101187500095079 ) ) ;
#73171 = CARTESIAN_POINT ( 'NONE',  ( 183.4553195968295256, 297.0403188216897661, -2.838562726794640056 ) ) ;
#73172 = LINE ( 'NONE', #34644, #13021 ) ;
#73173 = CARTESIAN_POINT ( 'NONE',  ( 163.8070446421170629, 255.0663642890118581, -15.42060242571707818 ) ) ;
#73174 = CARTESIAN_POINT ( 'NONE',  ( 18.76822678699008051, 172.4548013555409796, -4.594050593750042211 ) ) ;
#73175 = CARTESIAN_POINT ( 'NONE',  ( 171.9930234791391399, 277.2658286946252701, -16.71261851089754558 ) ) ;
#73176 = ORIENTED_EDGE ( 'NONE', *, *, #24680, .F. ) ;
#73177 = VERTEX_POINT ( 'NONE', #40657 ) ;
#73178 = CARTESIAN_POINT ( 'NONE',  ( 185.3117431063705283, 259.6004929598439048, -5.362663101281642142 ) ) ;
#73179 = CARTESIAN_POINT ( 'NONE',  ( 67.71136690417436910, 69.33268738728419578, 3.139524805400198293 ) ) ;
#73180 = CARTESIAN_POINT ( 'NONE',  ( 193.0451532016805913, 263.6626746619177766, -3.983151606634049990 ) ) ;
#73181 = CARTESIAN_POINT ( 'NONE',  ( 161.1750406344237661, 251.4836360396366501, -14.21198410781773802 ) ) ;
#73182 = DIRECTION ( 'NONE',  ( -0.8660254037844387076, -0.4999999999999998890, -0.000000000000000000 ) ) ;
#73183 = CARTESIAN_POINT ( 'NONE',  ( 167.9816492369689911, 251.8180079618673233, 10.45878825870253159 ) ) ;
#73184 = CARTESIAN_POINT ( 'NONE',  ( 39.09232661234986494, 199.5024278399160949, -9.188101187500093303 ) ) ;
#73185 = CARTESIAN_POINT ( 'NONE',  ( 97.79278455872243114, 217.2677522451417644, -5.000000000000041744 ) ) ;
#73186 = ORIENTED_EDGE ( 'NONE', *, *, #60072, .T. ) ;
#73187 = CARTESIAN_POINT ( 'NONE',  ( 83.75471768118535465, 46.64312366483261485, 11.04520889654889970 ) ) ;
#73188 = CARTESIAN_POINT ( 'NONE',  ( -6.807019788225388446, 173.0024278399160949, 9.188101187500095079 ) ) ;
#73189 = CARTESIAN_POINT ( 'NONE',  ( 68.79385422379222348, 64.21269200074630135, -11.92370147360801980 ) ) ;
#73190 = CARTESIAN_POINT ( 'NONE',  ( 150.6626254231123880, 269.6916732958875969, -15.32062296289003811 ) ) ;
#73191 = CARTESIAN_POINT ( 'NONE',  ( -7.471379830813591916, 36.41558964265287557, 59.99999999999999289 ) ) ;
#73192 = CARTESIAN_POINT ( 'NONE',  ( 192.4259603496955719, 297.3554553095298729, -12.40738485318142814 ) ) ;
#73193 = EDGE_CURVE ( 'NONE', #52672, #86487, #87360, .T. ) ;
#73194 = CARTESIAN_POINT ( 'NONE',  ( 68.71236162956441262, 68.31727361646146335, -8.171850045985486588 ) ) ;
#73195 = CARTESIAN_POINT ( 'NONE',  ( 203.7159275419774360, 276.2629543621159769, 13.33400116652491718 ) ) ;
#73196 = CARTESIAN_POINT ( 'NONE',  ( 78.80693396667733452, 204.7592609112379876, 2.679491924311254714 ) ) ;
#73197 = CARTESIAN_POINT ( 'NONE',  ( 164.2600772519394923, 246.1401958748887182, -2.110785484364219311 ) ) ;
#73198 = ORIENTED_EDGE ( 'NONE', *, *, #92136, .T. ) ;
#73199 = CARTESIAN_POINT ( 'NONE',  ( 1.826344505407192287, 171.8615022471902591, -10.00000000000009592 ) ) ;
#73200 = FACE_OUTER_BOUND ( 'NONE', #83371, .T. ) ;
#73201 = CARTESIAN_POINT ( 'NONE',  ( 115.3025621453804490, 243.5024278399160949, 9.188101187500095079 ) ) ;
#73202 = CARTESIAN_POINT ( 'NONE',  ( 20.98410315089673261, 24.06628583063841376, -9.188101187500006262 ) ) ;
#73203 = CARTESIAN_POINT ( 'NONE',  ( 74.78129183281730263, 67.18734618188521779, 12.47178672914711584 ) ) ;
#73204 = ADVANCED_FACE ( 'NONE', ( #87845 ), #32057, .F. ) ;
#73205 = CARTESIAN_POINT ( 'NONE',  ( 151.1161590537679444, 269.2899787152654767, 13.95646909953505599 ) ) ;
#73207 = DIRECTION ( 'NONE',  ( -0.8660254037844387076, -0.4999999999999998890, -0.000000000000000000 ) ) ;
#73206 = CARTESIAN_POINT ( 'NONE',  ( 165.4473470637335879, 246.0837842385732301, 3.196113342258863899 ) ) ;
#73208 = CARTESIAN_POINT ( 'NONE',  ( 81.63951372615375135, 59.32053296443953627, -0.4567727288213029868 ) ) ;
#73209 = EDGE_LOOP ( 'NONE', ( #44291, #88016, #53376, #86535 ) ) ;
#73210 = CARTESIAN_POINT ( 'NONE',  ( 150.6487462746963502, 269.7157126861102370, 15.18501655901553704 ) ) ;
#73211 = CARTESIAN_POINT ( 'NONE',  ( 196.6317700900902139, 290.0707791521982131, -17.91116578096951883 ) ) ;
#73212 = CARTESIAN_POINT ( 'NONE',  ( 45.19716250472275476, 70.24742367233086782, 10.00000000000000000 ) ) ;
#73213 = CARTESIAN_POINT ( 'NONE',  ( 203.9436454561111134, 276.7717721749480688, 13.76990199114231572 ) ) ;
#73214 = CARTESIAN_POINT ( 'NONE',  ( 81.63547489262985835, 55.73921394657421757, -16.35272683298455476 ) ) ;
#73215 = ORIENTED_EDGE ( 'NONE', *, *, #76767, .T. ) ;
#73216 = CARTESIAN_POINT ( 'NONE',  ( 189.3176312642889627, 265.7376729923254857, 10.75542669776848470 ) ) ;
#73217 = VECTOR ( 'NONE', #51899, 1000.000000000000000 ) ;
#73218 = CARTESIAN_POINT ( 'NONE',  ( 165.4318461280464874, 269.5429478206821159, -16.34563326180095189 ) ) ;
#73219 = B_SPLINE_SURFACE_WITH_KNOTS ( 'NONE', 3, 1, ( 
 ( #79316, #48875 ),
 ( #16454, #85930 ),
 ( #55432, #40741 ),
 ( #87448, #63557 ),
 ( #95527, #25055 ),
 ( #86927, #70655 ),
 ( #87934, #49363 ),
 ( #17981, #33159 ),
 ( #1267, #71686 ),
 ( #26072, #64064 ),
 ( #32151, #94001 ),
 ( #79809, #10374 ),
 ( #3289, #72182 ),
 ( #56948, #18477 ),
 ( #80307, #54951 ),
 ( #63059, #41751 ),
 ( #62538, #93497 ),
 ( #24056, #11878 ),
 ( #49857, #89417 ),
 ( #75172, #57448 ),
 ( #97967, #42734 ),
 ( #57954, #73181 ),
 ( #73671, #82310 ),
 ( #11392, #19970 ),
 ( #4252, #42245 ),
 ( #97483, #81307 ),
 ( #50847, #20470 ),
 ( #88427, #18987 ),
 ( #96503, #81796 ),
 ( #28543, #34655 ),
 ( #12882, #35655 ),
 ( #35151, #20978 ),
 ( #51861, #43739 ),
 ( #74684, #28048 ) ),
 .UNSPECIFIED., .T., .F., .F.,
 ( 4, 2, 2, 2, 2, 2, 2, 2, 2, 2, 2, 2, 2, 2, 2, 2, 4 ),
 ( 2, 2 ),
 ( 0.000000000000000000, 0.06250000000000000000, 0.1250000000000000000, 0.1875000000000000000, 0.2500000000000000000, 0.3125000000000000000, 0.3750000000000000000, 0.4375000000000000000, 0.5000000000000000000, 0.5625000000000000000, 0.6250000000000000000, 0.6875000000000000000, 0.7500000000000000000, 0.8125000000000000000, 0.8750000000000000000, 0.9375000000000000000, 1.000000000000000000 ),
 ( 0.000000000000000000, 1.000000000000000000 ),
 .UNSPECIFIED. ) ;
#73220 = CARTESIAN_POINT ( 'NONE',  ( 85.68836362758381142, 45.52427758709214345, 8.553938247697089992 ) ) ;
#73221 = CARTESIAN_POINT ( 'NONE',  ( 80.20007227937493610, 54.77581058227145405, 15.92427733993149985 ) ) ;
#73222 = CARTESIAN_POINT ( 'NONE',  ( 29.78943643340442549, 199.5530062829863027, -4.648177544792955347E-16 ) ) ;
#73223 = CARTESIAN_POINT ( 'NONE',  ( 72.16236457449060993, 71.55515601828724925, -5.863900035885150075 ) ) ;
#73224 = CARTESIAN_POINT ( 'NONE',  ( 153.2712411579340426, 265.1734183057532732, 16.26687330118495467 ) ) ;
#73225 = ORIENTED_EDGE ( 'NONE', *, *, #70921, .F. ) ;
#73226 = CARTESIAN_POINT ( 'NONE',  ( 194.5520723251022162, 283.0158833145478070, 17.60059791576126997 ) ) ;
#73227 = CARTESIAN_POINT ( 'NONE',  ( 7.263013161461002731, 16.14441083166258295, 10.00000000000000533 ) ) ;
#73228 = CARTESIAN_POINT ( 'NONE',  ( 173.9008529106967558, 272.4049662731551962, -17.79092985220220058 ) ) ;
#73229 = VERTEX_POINT ( 'NONE', #47753 ) ;
#73230 = CARTESIAN_POINT ( 'NONE',  ( 167.8099530253072089, 271.3928698661641761, -17.53051755021046532 ) ) ;
#73231 = LINE ( 'NONE', #5317, #87266 ) ;
#73232 = CARTESIAN_POINT ( 'NONE',  ( 159.7188570120185034, 264.1459342443484957, -17.63143322946013214 ) ) ;
#73233 = EDGE_LOOP ( 'NONE', ( #67221, #25210, #34505, #93832 ) ) ;
#73234 = CARTESIAN_POINT ( 'NONE',  ( 78.96241633089614709, 60.10021242361892035, 16.11556649788965601 ) ) ;
#73235 = CARTESIAN_POINT ( 'NONE',  ( 185.3856663186220715, 291.1121785684215411, 12.07308616320444017 ) ) ;
#73236 = DIRECTION ( 'NONE',  ( -0.000000000000000000, 1.000000000000000000, -0.000000000000000000 ) ) ;
#73237 = ORIENTED_EDGE ( 'NONE', *, *, #46220, .F. ) ;
#73238 = CARTESIAN_POINT ( 'NONE',  ( -2.512112762712737091, 143.3759306620403891, 22.50000000000002132 ) ) ;
#73239 = CARTESIAN_POINT ( 'NONE',  ( 84.46699969863880142, 49.90279977532637901, -13.71381277893580197 ) ) ;
#73240 = FACE_OUTER_BOUND ( 'NONE', #26103, .T. ) ;
#73241 = ORIENTED_EDGE ( 'NONE', *, *, #71633, .T. ) ;
#73242 = ORIENTED_EDGE ( 'NONE', *, *, #19237, .T. ) ;
#73243 = CARTESIAN_POINT ( 'NONE',  ( 177.6456495537226772, 260.6504471429459500, 12.23025887897517983 ) ) ;
#73244 = ORIENTED_EDGE ( 'NONE', *, *, #17691, .F. ) ;
#73245 = CARTESIAN_POINT ( 'NONE',  ( 173.9582802083413640, 250.9521034096781023, -3.022749797112575632 ) ) ;
#73246 = ORIENTED_EDGE ( 'NONE', *, *, #30024, .T. ) ;
#73247 = CARTESIAN_POINT ( 'NONE',  ( 75.22035300883564446, 59.77421810351211917, 15.71776402631701686 ) ) ;
#73248 = CARTESIAN_POINT ( 'NONE',  ( 154.9048824156581361, 262.3438686460345366, -17.40627786727128168 ) ) ;
#73249 = ORIENTED_EDGE ( 'NONE', *, *, #27472, .F. ) ;
#73250 = CARTESIAN_POINT ( 'NONE',  ( 110.0000000000000000, -8.000000000000000000, -14.21260523776213347 ) ) ;
#73251 = CARTESIAN_POINT ( 'NONE',  ( 82.00610100450838047, 41.07700615983480930, 3.349603895260225173 ) ) ;
#73252 = CARTESIAN_POINT ( 'NONE',  ( 163.0037873698800581, 255.9019164637528831, -14.93970584870495699 ) ) ;
#73253 = CARTESIAN_POINT ( 'NONE',  ( 158.6202604900994686, 274.9997957384633764, -12.56136378133423470 ) ) ;
#73254 = CARTESIAN_POINT ( 'NONE',  ( 152.7295469705997277, 266.1116601603806657, -17.40211458100010589 ) ) ;
#73255 = LINE ( 'NONE', #88506, #29122 ) ;
#73256 = CARTESIAN_POINT ( 'NONE',  ( 23.98812876850004727, 25.80066082961422325, 10.00000000000000533 ) ) ;
#73257 = CARTESIAN_POINT ( 'NONE',  ( 146.6963301283313967, 249.3768266524160140, 9.188101187500098632 ) ) ;
#73258 = CARTESIAN_POINT ( 'NONE',  ( 75.59476737973361082, 54.41781083123701279, 16.10556637520365442 ) ) ;
#73259 = CARTESIAN_POINT ( 'NONE',  ( 15.84867609773810138, 11.01110640527290840, 2.839279412974134775 ) ) ;
#73260 = VERTEX_POINT ( 'NONE', #49280 ) ;
#73261 = EDGE_CURVE ( 'NONE', #20256, #88849, #50335, .T. ) ;
#73263 = EDGE_LOOP ( 'NONE', ( #34339, #100282, #79484, #36656, #27607, #68328, #59926, #99496, #63968, #7015, #79254, #31062 ) ) ;
#73262 = CARTESIAN_POINT ( 'NONE',  ( 85.63146384662782395, 48.39429698310328121, -12.21155806772681629 ) ) ;
#73264 = CARTESIAN_POINT ( 'NONE',  ( -19.65312891409030271, 93.06504152958497400, -10.00000000000000888 ) ) ;
#73265 = CARTESIAN_POINT ( 'NONE',  ( 181.3414764931898162, 255.3117459804828400, 0.6552448166232091031 ) ) ;
#73266 = ADVANCED_FACE ( 'NONE', ( #2691 ), #95438, .F. ) ;
#73267 = CARTESIAN_POINT ( 'NONE',  ( 121.1754704609021900, 250.7677522451419065, -5.000000000000047962 ) ) ;
#73268 = CARTESIAN_POINT ( 'NONE',  ( 153.1667354219324011, 277.1489508030442153, 6.793483612096318680 ) ) ;
#73269 = CARTESIAN_POINT ( 'NONE',  ( 70.67229411587209142, 60.84139834894546794, 14.53033638096200875 ) ) ;
#73270 = CARTESIAN_POINT ( 'NONE',  ( 192.6772867332300621, 292.3908774927655259, -14.35745613815102928 ) ) ;
#73271 = CARTESIAN_POINT ( 'NONE',  ( 85.52015394113763591, 42.90618313698004727, 2.701328592287737251 ) ) ;
#73272 = CARTESIAN_POINT ( 'NONE',  ( 88.39284856500222531, 43.98633817645592359, -2.257003550805378733 ) ) ;
#73273 =( BOUNDED_CURVE ( )  B_SPLINE_CURVE ( 2, ( #38677, #75712, #52885, #7283, #29597, #14879, #91938, #13896, #76216 ),
 .UNSPECIFIED., .F., .T. ) 
 B_SPLINE_CURVE_WITH_KNOTS ( ( 3, 2, 2, 2, 3 ),
 ( 0.6572580645161290036, 0.6586021505376343788, 0.6612903225806451291, 0.6639784946236558794, 0.6653225806451612545 ),
 .UNSPECIFIED. ) 
 CURVE ( )  GEOMETRIC_REPRESENTATION_ITEM ( )  RATIONAL_B_SPLINE_CURVE ( ( 0.9330127018922194093, 0.9330127018922194093, 1.000000000000000000, 0.8660254037844387076, 1.000000000000000000, 0.8660254037844387076, 1.000000000000000000, 0.9330127018922194093, 0.9330127018922194093 ) ) 
 REPRESENTATION_ITEM ( '' )  );
#73274 = VERTEX_POINT ( 'NONE', #73238 ) ;
#73275 = CARTESIAN_POINT ( 'NONE',  ( 184.9711235847237276, 272.9950566324947658, -17.00090985181319780 ) ) ;
#73276 = CARTESIAN_POINT ( 'NONE',  ( 65.89235171844839556, 69.16849825365757454, 0.2321662580319230340 ) ) ;
#73277 = ORIENTED_EDGE ( 'NONE', *, *, #52765, .F. ) ;
#73279 = EDGE_CURVE ( 'NONE', #90112, #95476, #72060, .T. ) ;
#73278 = CARTESIAN_POINT ( 'NONE',  ( -39.52511050156712002, 25.94496742513405962, 177.5919119679930134 ) ) ;
#73280 = CARTESIAN_POINT ( 'NONE',  ( 156.2648642422210514, 277.5543309471286193, 10.15725722932580410 ) ) ;
#73281 = CARTESIAN_POINT ( 'NONE',  ( -72.92390943388483038, 47.25396573843040926, 10.00000000000000000 ) ) ;
#73282 = DIRECTION ( 'NONE',  ( -0.000000000000000000, 0.000000000000000000, -1.000000000000000000 ) ) ;
#73284 = AXIS2_PLACEMENT_3D ( 'NONE', #71461, #9144, #68569 ) ;
#73283 = CARTESIAN_POINT ( 'NONE',  ( 202.9685995779611858, 279.0950685203052899, 16.84977534244423580 ) ) ;
#73286 = CARTESIAN_POINT ( 'NONE',  ( 88.23680129110753967, 43.93620611740950466, 2.496076054743389783 ) ) ;
#73285 = CARTESIAN_POINT ( 'NONE',  ( 168.9285091408607684, 266.8905904589466900, 17.77692745299157195 ) ) ;
#73287 = CARTESIAN_POINT ( 'NONE',  ( 200.3681102454790448, 268.1092862786254614, 6.092393729374322220 ) ) ;
#73288 = ORIENTED_EDGE ( 'NONE', *, *, #25233, .T. ) ;
#73289 = DIRECTION ( 'NONE',  ( 0.03487823687205911238, -0.06041087834082882468, 0.9975640502598247528 ) ) ;
#73290 = CARTESIAN_POINT ( 'NONE',  ( 117.8737486125219505, 248.8615022471903160, 5.000000000000046185 ) ) ;
#73292 = ADVANCED_FACE ( 'NONE', ( #48427 ), #80369, .T. ) ;
#73291 = AXIS2_PLACEMENT_3D ( 'NONE', #75972, #90697, #52131 ) ;
#73293 = CARTESIAN_POINT ( 'NONE',  ( -76.38857681351474582, 54.22815603855766398, -10.00000000000000000 ) ) ;
#73294 = ADVANCED_FACE ( 'NONE', ( #95071 ), #87505, .F. ) ;
#73295 = CARTESIAN_POINT ( 'NONE',  ( -35.82302091652844922, 24.69132351629776423, -10.00000000000000000 ) ) ;
#73296 = CARTESIAN_POINT ( 'NONE',  ( 80.77907182703577860, 43.03124623689828354, -9.709161605721851274 ) ) ;
#73297 = CARTESIAN_POINT ( 'NONE',  ( 49.03918259513507394, 79.59780946358316100, 10.00000000000000000 ) ) ;
#73298 = B_SPLINE_CURVE_WITH_KNOTS ( 'NONE', 3,
 ( #20987, #60935, #75181, #45245, #14359, #53346, #51870, #13376, #77145, #13856, #15327, #37634, #52347, #83795, #7242, #5753 ),
 .UNSPECIFIED., .F., .F.,
 ( 4, 2, 2, 2, 2, 2, 2, 4 ),
 ( 0.000000000000000000, 0.0003786681000626840776, 0.0007573362001253681553, 0.001136004300188052070, 0.001514672400250736311, 0.001893340500313420334, 0.002272008600376104141, 0.003029344800501419278 ),
 .UNSPECIFIED. ) ;
#73299 = CARTESIAN_POINT ( 'NONE',  ( -2.098180203030011182, 181.8464784336661637, 1.353441290958777525E-15 ) ) ;
#73300 = CARTESIAN_POINT ( 'NONE',  ( 108.7534185771431510, 233.5958772461660260, -9.188101187500095079 ) ) ;
#73301 = CARTESIAN_POINT ( 'NONE',  ( 202.7602807045765019, 279.4558873931827065, -15.90558713185497020 ) ) ;
#73302 = CARTESIAN_POINT ( 'NONE',  ( 192.4259603496955719, 297.3554553095298729, -12.40738485318142814 ) ) ;
#73303 = CARTESIAN_POINT ( 'NONE',  ( 180.2803958731623197, 254.8946283151103955, -2.457077073020527358 ) ) ;
#73304 = CARTESIAN_POINT ( 'NONE',  ( -1.617403181491035902, 158.3262482093458061, 3.021315404115420679E-15 ) ) ;
#73305 = VECTOR ( 'NONE', #60088, 1000.000000000000000 ) ;
#73306 = DIRECTION ( 'NONE',  ( 0.06415622980647768536, -0.9979398670145503969, 0.000000000000000000 ) ) ;
#73307 = CARTESIAN_POINT ( 'NONE',  ( 160.8174585145418405, 281.7671747025778473, 5.344995675835433779 ) ) ;
#73308 = CARTESIAN_POINT ( 'NONE',  ( 194.8432095198904221, 293.1686569321988145, -14.74101036184996616 ) ) ;
#73309 = ADVANCED_FACE ( 'NONE', ( #48931 ), #10431, .T. ) ;
#73310 = CARTESIAN_POINT ( 'NONE',  ( 182.7847760313759409, 280.0284915794045446, -17.53211380394024843 ) ) ;
#73311 = FACE_OUTER_BOUND ( 'NONE', #84128, .T. ) ;
#73312 = CARTESIAN_POINT ( 'NONE',  ( 74.25223132960039152, 56.37754847584465523, -16.09006086798675739 ) ) ;
#73313 = FACE_OUTER_BOUND ( 'NONE', #12712, .T. ) ;
#73314 = EDGE_CURVE ( 'NONE', #8304, #87111, #49090, .T. ) ;
#73315 = CARTESIAN_POINT ( 'NONE',  ( 172.5878269333680350, 263.4941563848159944, -15.40501487940348646 ) ) ;
#73316 = CARTESIAN_POINT ( 'NONE',  ( 89.86341300497758766, 216.5643266524160140, 9.188101187500095079 ) ) ;
#73317 = EDGE_CURVE ( 'NONE', #24915, #3476, #51413, .T. ) ;
#73318 = CARTESIAN_POINT ( 'NONE',  ( 161.2977680094314223, 251.2710659906439616, -13.03191437619249982 ) ) ;
#73319 = CYLINDRICAL_SURFACE ( 'NONE', #41140, 10.00000000000010658 ) ;
#73320 = EDGE_CURVE ( 'NONE', #53652, #58927, #71143, .T. ) ;
#73321 = CARTESIAN_POINT ( 'NONE',  ( 163.2942584940569191, 258.1478583562382028, 16.77787020301746779 ) ) ;
#73323 = CARTESIAN_POINT ( 'NONE',  ( 4.102725850843912170, 28.55253618238880620, -10.00000000000000000 ) ) ;
#73322 = CARTESIAN_POINT ( 'NONE',  ( 157.0957870390718369, 258.5491105237443321, 17.69218919045495397 ) ) ;
#73324 = CARTESIAN_POINT ( 'NONE',  ( 199.2299651681423143, 285.5705732690366858, -17.65328173313980642 ) ) ;
#73325 = CARTESIAN_POINT ( 'NONE',  ( 173.1817746140479244, 268.1958027911921363, -16.29107544405880859 ) ) ;
#73326 = EDGE_CURVE ( 'NONE', #68451, #13298, #62322, .T. ) ;
#73327 = CARTESIAN_POINT ( 'NONE',  ( 35.22599450741489591, 22.19860640527294393, 2.839279412974134775 ) ) ;
#73328 = CARTESIAN_POINT ( 'NONE',  ( 84.22812144220274888, 48.05245718175660130, -12.57432882457237966 ) ) ;
#73329 = CARTESIAN_POINT ( 'NONE',  ( 74.81457254233032472, 57.45830024592526541, 16.48667394790776086 ) ) ;
#73330 = VERTEX_POINT ( 'NONE', #37693 ) ;
#73331 = CARTESIAN_POINT ( 'NONE',  ( 14.38185574516869458, 23.70171378149918695, -9.188101187500004485 ) ) ;
#73332 = CARTESIAN_POINT ( 'NONE',  ( 74.03095222233704931, 222.7369531367911293, -4.594050593750048428 ) ) ;
#73333 = CARTESIAN_POINT ( 'NONE',  ( 172.7158920701056957, 289.4533927640794673, -1.057531439601499201 ) ) ;
#73334 = CARTESIAN_POINT ( 'NONE',  ( -31.22174636879925202, 93.45486797506030996, 11.33730873907181369 ) ) ;
#73335 = CARTESIAN_POINT ( 'NONE',  ( 188.3784916956350344, 286.3721210266486992, -16.81851773412965301 ) ) ;
#73336 = ADVANCED_FACE ( 'NONE', ( #28113 ), #53074, .F. ) ;
#73337 = EDGE_CURVE ( 'NONE', #72572, #16478, #84117, .T. ) ;
#73338 = CARTESIAN_POINT ( 'NONE',  ( 86.54431918921495992, 47.23684621844409293, 10.68448168089783756 ) ) ;
#73339 = CARTESIAN_POINT ( 'NONE',  ( 72.53811683814018352, 71.57833605577215508, 5.312062988065741287 ) ) ;
#73340 = CARTESIAN_POINT ( 'NONE',  ( 124.0080952226617796, 235.7365022471902023, -10.00000000000009059 ) ) ;
#73341 = CARTESIAN_POINT ( 'NONE',  ( 157.8043799545718286, 257.3217915922150496, -17.97575562758749257 ) ) ;
#73342 = CARTESIAN_POINT ( 'NONE',  ( 28.32887064134541077, 16.75978393459165261, -1.583844403245362020 ) ) ;
#73343 = ORIENTED_EDGE ( 'NONE', *, *, #68249, .F. ) ;
#73344 = CARTESIAN_POINT ( 'NONE',  ( 85.66375497126256278, 46.86456526682530210, 10.26853249941764012 ) ) ;
#73345 = ORIENTED_EDGE ( 'NONE', *, *, #32416, .T. ) ;
#73346 = CARTESIAN_POINT ( 'NONE',  ( 163.3706531435203146, 247.6807236201477735, 10.06957846017757241 ) ) ;
#73347 = CARTESIAN_POINT ( 'NONE',  ( 72.26191451101281871, 71.91445694603925176, -5.118044210176698527 ) ) ;
#73348 = VERTEX_POINT ( 'NONE', #16402 ) ;
#73349 = DIRECTION ( 'NONE',  ( 0.7886751345947996539, -0.2113248654051860242, -0.5773502691896443828 ) ) ;
#73350 = ORIENTED_EDGE ( 'NONE', *, *, #63690, .F. ) ;
#73351 = CARTESIAN_POINT ( 'NONE',  ( 188.8058653551997566, 290.9426387842769373, 14.85089295608895021 ) ) ;
#73352 = CARTESIAN_POINT ( 'NONE',  ( 158.4819084462915839, 256.1482778209808089, 16.21549387834203415 ) ) ;
#73353 = FACE_OUTER_BOUND ( 'NONE', #74740, .T. ) ;
#73354 = CARTESIAN_POINT ( 'NONE',  ( 88.16744270275496831, 44.54586846255803323, -4.939063992914630497 ) ) ;
#73355 = CARTESIAN_POINT ( 'NONE',  ( -19.65312891409030271, 93.06504152958497400, -10.00000000000000888 ) ) ;
#73356 = VECTOR ( 'NONE', #97640, 1000.000000000000000 ) ;
#73357 = CARTESIAN_POINT ( 'NONE',  ( 37.04286019156342746, 27.10170272979929607, -7.433330006724141015 ) ) ;
#73358 = CARTESIAN_POINT ( 'NONE',  ( 73.30726679204248342, 60.50815918352778766, -15.22201117688972971 ) ) ;
#73359 = AXIS2_PLACEMENT_3D ( 'NONE', #81207, #49762, #11291 ) ;
#73360 = CARTESIAN_POINT ( 'NONE',  ( 164.0781508658037637, 275.4055464209769752, 15.63836535835214114 ) ) ;
#73361 = DIRECTION ( 'NONE',  ( -0.000000000000000000, -0.000000000000000000, -1.000000000000000000 ) ) ;
#73362 = VERTEX_POINT ( 'NONE', #15383 ) ;
#73363 = ORIENTED_EDGE ( 'NONE', *, *, #92492, .T. ) ;
#73364 = CARTESIAN_POINT ( 'NONE',  ( 186.9477914209481355, 275.4121812026439216, 17.59542901063888820 ) ) ;
#73366 = CARTESIAN_POINT ( 'NONE',  ( 194.3011251241114508, 294.1075746476782342, -14.76047579547631905 ) ) ;
#73365 = CARTESIAN_POINT ( 'NONE',  ( 204.6427704787179493, 276.1953194596412118, 13.28850621060895953 ) ) ;
#73367 = CARTESIAN_POINT ( 'NONE',  ( 85.93449727955278661, 48.41344338607260767, 12.08598331734388509 ) ) ;
#73368 = FACE_OUTER_BOUND ( 'NONE', #31363, .T. ) ;
#73369 = AXIS2_PLACEMENT_3D ( 'NONE', #98124, #36299, #51505 ) ;
#73370 = LINE ( 'NONE', #88123, #86895 ) ;
#73371 = CARTESIAN_POINT ( 'NONE',  ( 70.32079880886523426, 61.21821433514125488, 14.81414658500229109 ) ) ;
#73372 = CARTESIAN_POINT ( 'NONE',  ( 207.4535553197589763, 271.3268973058138158, -4.905507205346139266 ) ) ;
#73373 = CARTESIAN_POINT ( 'NONE',  ( 169.1799572416250612, 267.0414233079974338, 17.70411709586223736 ) ) ;
#73374 = VECTOR ( 'NONE', #31541, 1000.000000000000000 ) ;
#73375 = CARTESIAN_POINT ( 'NONE',  ( 178.5561507476227234, 255.7288023451889671, 4.885752237254268771 ) ) ;
#73376 = CARTESIAN_POINT ( 'NONE',  ( 95.24857461505581568, 234.9869531367911293, 4.594050593750046652 ) ) ;
#73377 = EDGE_LOOP ( 'NONE', ( #23983, #47187, #48538, #88134 ) ) ;
#73378 = DIRECTION ( 'NONE',  ( -0.09573633691163400961, -0.9954067278227238802, 0.000000000000000000 ) ) ;
#73379 = FACE_OUTER_BOUND ( 'NONE', #22513, .T. ) ;
#73380 = CARTESIAN_POINT ( 'NONE',  ( 166.8352072885147948, 278.2578104396429808, -13.33477771316318261 ) ) ;
#73381 = ORIENTED_EDGE ( 'NONE', *, *, #546, .F. ) ;
#73382 = ORIENTED_EDGE ( 'NONE', *, *, #186, .F. ) ;
#73383 = CARTESIAN_POINT ( 'NONE',  ( 87.15358044669149251, 46.07130289202554252, -8.233871337641097909 ) ) ;
#73384 = DIRECTION ( 'NONE',  ( 0.4999999999999998890, -0.8660254037844385966, 0.000000000000000000 ) ) ;
#73385 = CARTESIAN_POINT ( 'NONE',  ( 163.6378993367609382, 249.6457029564056711, 10.23770952667803691 ) ) ;
#73386 = CARTESIAN_POINT ( 'NONE',  ( 17.89217828605986327, 10.73415679381820986, 1.333680081654574804E-15 ) ) ;
#73387 = CARTESIAN_POINT ( 'NONE',  ( 77.77867966053455007, 61.43039905302717330, -16.12786080876372807 ) ) ;
#73388 = CARTESIAN_POINT ( 'NONE',  ( 95.57333414147498729, 235.1744531367911293, 4.594050593750047540 ) ) ;
#73389 = ORIENTED_EDGE ( 'NONE', *, *, #49308, .F. ) ;
#73390 = ORIENTED_EDGE ( 'NONE', *, *, #39206, .T. ) ;
#73391 = CARTESIAN_POINT ( 'NONE',  ( 48.95103868752454446, 97.61288834769685252, -10.00000000000000000 ) ) ;
#73392 = CARTESIAN_POINT ( 'NONE',  ( 208.3194307158603067, 269.8271571267425770, -2.120200867047394855 ) ) ;
#73393 = ORIENTED_EDGE ( 'NONE', *, *, #62419, .T. ) ;
#73394 = ADVANCED_FACE ( 'NONE', ( #30612 ), #93609, .F. ) ;
#73395 = CARTESIAN_POINT ( 'NONE',  ( 191.6165807384784046, 263.6474570320527278, -8.167173469078569781 ) ) ;
#73396 = CARTESIAN_POINT ( 'NONE',  ( 153.2087289474062572, 265.9906550880538134, 16.15720884485870812 ) ) ;
#73397 = CARTESIAN_POINT ( 'NONE',  ( 71.17136799091453270, 69.39928743177321735, -7.895708389734693355 ) ) ;
#73399 = CARTESIAN_POINT ( 'NONE',  ( 69.43848462473566485, 62.96533099991498261, -13.64912705282497818 ) ) ;
#73398 = CARTESIAN_POINT ( 'NONE',  ( 135.6816562978893330, 239.9548013555409796, -4.594050593750042211 ) ) ;
#73400 = CARTESIAN_POINT ( 'NONE',  ( -11.32641631811688221, 164.2677522451418781, 10.00000000000009592 ) ) ;
#73401 = DIRECTION ( 'NONE',  ( -0.8660254037844392627, -0.4999999999999987232, 0.000000000000000000 ) ) ;
#73402 = ORIENTED_EDGE ( 'NONE', *, *, #70805, .F. ) ;
#73403 = CARTESIAN_POINT ( 'NONE',  ( 204.9604304439480416, 275.6451162603322587, 13.28912526856024279 ) ) ;
#73404 = B_SPLINE_CURVE_WITH_KNOTS ( 'NONE', 3,
 ( #36583, #35097, #42685, #20418, #5204, #43690, #74630, #67488, #12828, #20926, #66006, #51285, #82254, #89367, #36085, #59882, #12317, #50300, #82751, #73616, #66988, #19921, #21402, #19443, #51808, #97914, #35602, #81252, #80768, #11826, #28489, #59370, #90849, #13318, #96957, #27522, #98418, #44179, #75117, #5693, #11340, #29011, #42197, #73132, #27996, #3725, #34604, #43180 ),
 .UNSPECIFIED., .F., .F.,
 ( 4, 2, 2, 2, 2, 2, 2, 2, 2, 2, 2, 2, 2, 2, 2, 2, 2, 2, 2, 2, 2, 2, 2, 4 ),
 ( 0.0001333623287611991604, 0.001159685769147140652, 0.001672847489340077232, 0.001801137919388335175, 0.001929428349436593118, 0.002057718779484850845, 0.002186009209533108788, 0.002442590069629720084, 0.002699170929726331814, 0.003212332649919709231, 0.004238656090306530851, 0.005264979530693353338, 0.005778141250886801444, 0.006034722110983567998, 0.006291302971080335420, 0.006355448186104469162, 0.006419593401128602037, 0.006547883831177029983, 0.006804464691273848578, 0.007061045551370668041, 0.007317626411467486637, 0.007574207271564305233, 0.007830788131661124696, 0.008343949851854678620 ),
 .UNSPECIFIED. ) ;
#73405 = CARTESIAN_POINT ( 'NONE',  ( 81.12175378958070837, 46.86607467030008678, 12.41971840815434014 ) ) ;
#73406 = CARTESIAN_POINT ( 'NONE',  ( 206.5237403681858552, 272.9373840435757188, -10.81420335655575116 ) ) ;
#73407 = LINE ( 'NONE', #48606, #88566 ) ;
#73409 = EDGE_CURVE ( 'NONE', #19773, #179, #81248, .T. ) ;
#73408 = CARTESIAN_POINT ( 'NONE',  ( -37.40701240123934213, 25.35389310390295137, -10.00000000000000000 ) ) ;
#73410 = CARTESIAN_POINT ( 'NONE',  ( -13.11024591527723437, 27.99999999999999645, -17.00000000000016698 ) ) ;
#73411 = EDGE_CURVE ( 'NONE', #41871, #6045, #28542, .T. ) ;
#73412 = CARTESIAN_POINT ( 'NONE',  ( 83.53204454370725784, 52.39401912150449903, -15.17729711222452238 ) ) ;
#73413 = CARTESIAN_POINT ( 'NONE',  ( 80.69930153274798101, 53.64823478532364476, 15.66247753479108340 ) ) ;
#73414 = DIRECTION ( 'NONE',  ( -0.5000000000000001110, 0.8660254037844384856, 0.000000000000000000 ) ) ;
#73415 = CARTESIAN_POINT ( 'NONE',  ( 159.8732321751776624, 253.7384344327741132, -15.51998349828054202 ) ) ;
#73416 = CARTESIAN_POINT ( 'NONE',  ( 78.21665545015443399, 61.78861457223207054, 15.74551361518583548 ) ) ;
#73417 = CARTESIAN_POINT ( 'NONE',  ( 208.1912724900461740, 270.0491336852600170, -0.9856800448607289100 ) ) ;
#73418 = LINE ( 'NONE', #34405, #62460 ) ;
#73419 = CONICAL_SURFACE ( 'NONE', #42654, 16.60714546451156082, 0.7853981633974407295 ) ;
#73420 = CARTESIAN_POINT ( 'NONE',  ( 70.38699400097776504, 64.88736316116830949, -12.15252907320628672 ) ) ;
#73422 = CARTESIAN_POINT ( 'NONE',  ( 185.2786651606941746, 266.4582656545080681, 13.16981717527268536 ) ) ;
#73421 = CARTESIAN_POINT ( 'NONE',  ( 73.51948839908330058, 69.73627507762923017, -9.361350578256050881 ) ) ;
#73423 = CARTESIAN_POINT ( 'NONE',  ( 168.2694307985145770, 247.7137964094873439, -3.237542012886357234 ) ) ;
#73424 = CARTESIAN_POINT ( 'NONE',  ( 31.84840506572257723, 40.16126292948897003, -6.180339887498951690 ) ) ;
#73425 = CARTESIAN_POINT ( 'NONE',  ( -19.65312891409030271, 93.06504152958497400, -10.00000000000000888 ) ) ;
#73426 = CARTESIAN_POINT ( 'NONE',  ( 71.64668629127858424, 59.15370159437364350, -15.31769636727452877 ) ) ;
#73427 = CARTESIAN_POINT ( 'NONE',  ( 83.00116628026432863, 43.22466567352054767, -7.302193047968875028 ) ) ;
#73428 = AXIS2_PLACEMENT_3D ( 'NONE', #43037, #58744, #89717 ) ;
#73429 = EDGE_CURVE ( 'NONE', #79972, #19414, #84221, .T. ) ;
#73430 = CARTESIAN_POINT ( 'NONE',  ( 22.04262502322622908, 183.5333772461660544, 9.188101187500095079 ) ) ;
#73431 = VECTOR ( 'NONE', #59694, 1000.000000000000000 ) ;
#73432 = CARTESIAN_POINT ( 'NONE',  ( 207.3442821610807414, 271.1161826646066970, 2.723480558286873521 ) ) ;
#73433 = ORIENTED_EDGE ( 'NONE', *, *, #16335, .T. ) ;
#73434 = ADVANCED_FACE ( 'NONE', ( #68356 ), #97422, .F. ) ;
#73435 = CARTESIAN_POINT ( 'NONE',  ( 86.99418556918212175, 46.03399372306155612, 8.963501050606421217 ) ) ;
#73436 = EDGE_CURVE ( 'NONE', #29477, #52312, #4758, .T. ) ;
#73437 = B_SPLINE_CURVE_WITH_KNOTS ( 'NONE', 3,
 ( #64457, #71573, #17871, #93899, #17348, #48255, #86311, #16353, #93392, #95417, #32557, #72070, #18367, #16846, #1163, #55334, #39127, #48768, #79202, #25973, #2169, #24453, #8754, #63949 ),
 .UNSPECIFIED., .F., .F.,
 ( 4, 2, 2, 2, 2, 2, 2, 2, 2, 2, 2, 4 ),
 ( 0.000000000000000000, 0.1249999999999944211, 0.2499999999999888423, 0.3749999999999832356, 0.4374999999999849565, 0.4999999999999866773, 0.5624999999999884537, 0.6249999999999901190, 0.6874999999999917843, 0.7499999999999933387, 0.8749999999999966693, 1.000000000000000000 ),
 .UNSPECIFIED. ) ;
#73438 = DIRECTION ( 'NONE',  ( -0.8660254037844387076, -0.4999999999999998890, -0.000000000000000000 ) ) ;
#73439 = CARTESIAN_POINT ( 'NONE',  ( 81.81993950966820250, 41.65085046188367102, 5.428165815223279900 ) ) ;
#73440 = CARTESIAN_POINT ( 'NONE',  ( 39.90439897628026955, 193.8458772461660544, 9.188101187500095079 ) ) ;
#73441 = CARTESIAN_POINT ( 'NONE',  ( 161.5431944097339851, 250.8459749958011287, 14.52339846942414603 ) ) ;
#73442 = CARTESIAN_POINT ( 'NONE',  ( 190.4976253092930278, 300.6954295735222900, -5.764807383508308902 ) ) ;
#73443 = CARTESIAN_POINT ( 'NONE',  ( 38.51650576605270260, 30.43677371833804202, -10.00000000000000355 ) ) ;
#73444 = CARTESIAN_POINT ( 'NONE',  ( 178.5414132024961873, 291.6442548996461710, 6.015133232593436574 ) ) ;
#73445 = CARTESIAN_POINT ( 'NONE',  ( 178.8763131426492521, 293.7076375770308800, 2.674743856691759181 ) ) ;
#73446 = CARTESIAN_POINT ( 'NONE',  ( 179.0083614005145307, 278.2908046544912395, -16.68097254531133800 ) ) ;
#73447 = CARTESIAN_POINT ( 'NONE',  ( 68.84278490277841911, 67.88251720973005376, -8.019614188230095309 ) ) ;
#73448 = B_SPLINE_SURFACE_WITH_KNOTS ( 'NONE', 3, 1, ( 
 ( #46380, #91541 ),
 ( #69197, #22106 ),
 ( #30710, #61590 ),
 ( #92541, #53002 ),
 ( #62080, #31189 ),
 ( #38791, #29222 ),
 ( #69697, #48280 ),
 ( #60089, #76802 ),
 ( #23088, #44893 ),
 ( #45397, #6902 ),
 ( #53980, #93027 ),
 ( #36802, #54475 ),
 ( #23583, #84938 ),
 ( #37300, #302 ),
 ( #17373, #85453 ),
 ( #37791, #91052 ),
 ( #21619, #52499 ),
 ( #53494, #83447 ),
 ( #14015, #68692 ),
 ( #7395, #92060 ),
 ( #75834, #30204 ),
 ( #61090, #84446 ),
 ( #14991, #45878 ),
 ( #57362, #35058 ),
 ( #3689, #94912 ),
 ( #56860, #49282 ),
 ( #42161, #87847 ),
 ( #64479, #95925 ),
 ( #25474, #65469 ),
 ( #49772, #65965 ),
 ( #58354, #81217 ),
 ( #88841, #10284 ),
 ( #79226, #80218 ),
 ( #89332, #33584 ) ),
 .UNSPECIFIED., .T., .F., .F.,
 ( 4, 2, 2, 2, 2, 2, 2, 2, 2, 2, 2, 2, 2, 2, 2, 2, 4 ),
 ( 2, 2 ),
 ( 0.000000000000000000, 0.06250000000000000000, 0.1250000000000000000, 0.1875000000000000000, 0.2500000000000000000, 0.3125000000000000000, 0.3750000000000000000, 0.4375000000000000000, 0.5000000000000000000, 0.5625000000000000000, 0.6250000000000000000, 0.6875000000000000000, 0.7500000000000000000, 0.8125000000000000000, 0.8750000000000000000, 0.9375000000000000000, 1.000000000000000000 ),
 ( 0.000000000000000000, 1.000000000000000000 ),
 .UNSPECIFIED. ) ;
#73449 = EDGE_CURVE ( 'NONE', #38805, #30217, #24952, .T. ) ;
#73450 = EDGE_CURVE ( 'NONE', #55017, #6693, #24265, .T. ) ;
#73451 = CARTESIAN_POINT ( 'NONE',  ( 83.46272733064347449, 51.93221652752758644, 15.00972995268699961 ) ) ;
#73452 = CARTESIAN_POINT ( 'NONE',  ( 72.04657099559535993, 225.7365022471903160, 2.944929066748280225E-16 ) ) ;
#73453 = CARTESIAN_POINT ( 'NONE',  ( 16.62094515339138212, 173.7365022471902307, 10.00000000000009948 ) ) ;
#73454 = PLANE ( 'NONE',  #32049 ) ;
#73455 = EDGE_LOOP ( 'NONE', ( #98766, #67113, #10160, #40192 ) ) ;
#73456 = CARTESIAN_POINT ( 'NONE',  ( 36.54820344085055694, 204.1589784336661637, -6.496448406907675876E-16 ) ) ;
#73457 = VERTEX_POINT ( 'NONE', #95212 ) ;
#73458 = CARTESIAN_POINT ( 'NONE',  ( 162.5280598625341497, 263.2215374870250457, 17.43915653070007110 ) ) ;
#73459 = CARTESIAN_POINT ( 'NONE',  ( 190.6954410837624607, 300.3528026016029457, -5.728531842148099962 ) ) ;
#73460 = FACE_OUTER_BOUND ( 'NONE', #43718, .T. ) ;
#73461 = EDGE_LOOP ( 'NONE', ( #27402, #11102, #69890, #8467, #57099 ) ) ;
#73462 = CARTESIAN_POINT ( 'NONE',  ( 170.9080147460631736, 286.3543506222695783, 7.469236110414841256 ) ) ;
#73463 = CARTESIAN_POINT ( 'NONE',  ( 164.4781197247689306, 245.7625352337404649, -1.511762618280499515 ) ) ;
#73464 = DIRECTION ( 'NONE',  ( 0.8660254037844390407, 0.4999999999999993339, 0.000000000000000000 ) ) ;
#73465 = CARTESIAN_POINT ( 'NONE',  ( 23.41017057962146097, 28.91421378149919619, 9.188101187500008038 ) ) ;
#73466 = CARTESIAN_POINT ( 'NONE',  ( 188.7940803133921577, 265.4288857401144810, 10.73849653901970491 ) ) ;
#73467 = LINE ( 'NONE', #4050, #47292 ) ;
#73468 = CARTESIAN_POINT ( 'NONE',  ( 171.2975384787696100, 255.8152646582991849, 11.65888598572620438 ) ) ;
#73469 = ORIENTED_EDGE ( 'NONE', *, *, #85523, .F. ) ;
#73470 = CARTESIAN_POINT ( 'NONE',  ( 17.90851666933368236, 18.84335787977762067, 9.188101187500006262 ) ) ;
#73471 = CARTESIAN_POINT ( 'NONE',  ( 75.98838095635207424, 59.87856586137668558, 15.81821194684219734 ) ) ;
#73472 = CARTESIAN_POINT ( 'NONE',  ( 174.5500181047472381, 255.0162374629895226, 8.241104149140888069 ) ) ;
#73473 = DIRECTION ( 'NONE',  ( -1.000000000000000000, 0.000000000000000000, 0.000000000000000000 ) ) ;
#73474 = ORIENTED_EDGE ( 'NONE', *, *, #45013, .F. ) ;
#73475 = CARTESIAN_POINT ( 'NONE',  ( 15.11407551230992041, 32.30945333909092909, 177.5919119679930134 ) ) ;
#73476 = CARTESIAN_POINT ( 'NONE',  ( 22.49293824011677856, 13.39040679176982707, 1.333680081654574804E-15 ) ) ;
#73477 = CARTESIAN_POINT ( 'NONE',  ( 82.18753490691527475, 40.78579184768808830, -0.6546124752527386903 ) ) ;
#73478 = VERTEX_POINT ( 'NONE', #23745 ) ;
#73479 = ORIENTED_EDGE ( 'NONE', *, *, #19412, .F. ) ;
#73481 = LINE ( 'NONE', #4065, #99320 ) ;
#73480 = CARTESIAN_POINT ( 'NONE',  ( 161.0965315767822972, 251.6196177163260188, -13.76772246540905442 ) ) ;
#73482 = CARTESIAN_POINT ( 'NONE',  ( 30.68386671255119325, 44.42157463747831514, 10.00000000000000000 ) ) ;
#73483 = ORIENTED_EDGE ( 'NONE', *, *, #32635, .F. ) ;
#73484 = CARTESIAN_POINT ( 'NONE',  ( 66.04626366651064018, 69.11317259379546840, -2.045714799961292574 ) ) ;
#73485 = CARTESIAN_POINT ( 'NONE',  ( 13.90223112049948639, 33.06302660730329279, -10.00000000000000000 ) ) ;
#73486 = CARTESIAN_POINT ( 'NONE',  ( 81.46866702687000839, 55.81909161095428829, 16.37896761046575378 ) ) ;
#73487 = CARTESIAN_POINT ( 'NONE',  ( 77.79976927246816842, 61.42068562798239384, -16.13251659512815550 ) ) ;
#73488 = EDGE_CURVE ( 'NONE', #49704, #43692, #63260, .T. ) ;
#73489 = CARTESIAN_POINT ( 'NONE',  ( 157.8043799545718286, 257.3217915922150496, -17.97575562758749257 ) ) ;
#73490 = CARTESIAN_POINT ( 'NONE',  ( 106.6423081075360670, 238.5024278399160949, -9.188101187500093303 ) ) ;
#73491 = CARTESIAN_POINT ( 'NONE',  ( 112.2445834879231086, 235.6115022471902307, 10.00000000000009592 ) ) ;
#73492 = ORIENTED_EDGE ( 'NONE', *, *, #18517, .F. ) ;
#73493 = B_SPLINE_CURVE_WITH_KNOTS ( 'NONE', 3,
 ( #24069, #46870, #272, #86435 ),
 .UNSPECIFIED., .F., .F.,
 ( 4, 4 ),
 ( 0.01007082774348767168, 0.01841198851506076553 ),
 .UNSPECIFIED. ) ;
#73494 = CARTESIAN_POINT ( 'NONE',  ( 163.9910908123517288, 246.6060940548019289, -7.333295033952830444 ) ) ;
#73495 = ORIENTED_EDGE ( 'NONE', *, *, #88252, .F. ) ;
#73496 = CARTESIAN_POINT ( 'NONE',  ( 36.52324494929276710, 26.80170272979929180, 7.433330006724137462 ) ) ;
#73497 = CARTESIAN_POINT ( 'NONE',  ( 159.7953104873542145, 253.8733987550956783, 15.41928249285404107 ) ) ;
#73498 = CARTESIAN_POINT ( 'NONE',  ( 165.2351475709818089, 262.2120121923977649, 17.49020206947767875 ) ) ;
#73499 = CARTESIAN_POINT ( 'NONE',  ( 69.94482871793549350, 205.0643266524159856, -9.188101187500093303 ) ) ;
#73500 = CARTESIAN_POINT ( 'NONE',  ( 19.85049821812290816, 182.2677522451418497, 10.00000000000009592 ) ) ;
#73501 = CARTESIAN_POINT ( 'NONE',  ( 142.6123662252853421, 259.5780487066560340, -7.305945665944390655 ) ) ;
#73502 = FACE_OUTER_BOUND ( 'NONE', #64685, .T. ) ;
#73503 = CARTESIAN_POINT ( 'NONE',  ( 175.1717403937841198, 278.2705980278694256, 15.46858508767819629 ) ) ;
#73504 = ORIENTED_EDGE ( 'NONE', *, *, #53760, .T. ) ;
#73505 = VECTOR ( 'NONE', #8726, 1000.000000000000000 ) ;
#73506 = DIRECTION ( 'NONE',  ( -0.7909930170786166892, 0.6118251767726361479, 0.000000000000000000 ) ) ;
#73507 = CARTESIAN_POINT ( 'NONE',  ( 66.52392041426838887, 68.84470833973988135, -4.415679280545959706 ) ) ;
#73508 = EDGE_LOOP ( 'NONE', ( #77892, #81251, #99882, #90363, #200, #2134, #80271, #63778 ) ) ;
#73509 = CARTESIAN_POINT ( 'NONE',  ( 147.9505753669699857, 274.3890817857965772, 9.316607266155644496 ) ) ;
#73510 = CARTESIAN_POINT ( 'NONE',  ( 70.86412831381173305, 69.83143264938641437, -6.808367436344060053 ) ) ;
#73511 = CARTESIAN_POINT ( 'NONE',  ( 163.5290595954285777, 260.2326466906550877, -16.19227360478010169 ) ) ;
#73512 = CARTESIAN_POINT ( 'NONE',  ( 85.25577013208754806, 208.4824982072973967, 3.021315404115420679E-15 ) ) ;
#73514 = EDGE_CURVE ( 'NONE', #16265, #78871, #47914, .T. ) ;
#73513 = VECTOR ( 'NONE', #41823, 1000.000000000000000 ) ;
#73515 = CARTESIAN_POINT ( 'NONE',  ( 24.82038151633537026, 14.73415679381822230, 1.333680081654574804E-15 ) ) ;
#73516 = CARTESIAN_POINT ( 'NONE',  ( 205.7867067512454184, 274.2139637150027056, 10.62737868262404106 ) ) ;
#73517 = CARTESIAN_POINT ( 'NONE',  ( 164.5813345449211624, 245.5837619211427523, 1.447064457712487373 ) ) ;
#73518 = CARTESIAN_POINT ( 'NONE',  ( -63.60198981653986294, 65.77656800267020287, 59.99999999999999289 ) ) ;
#73519 = CARTESIAN_POINT ( 'NONE',  ( 164.1634658209742952, 254.0895655750726689, 14.32597737159830409 ) ) ;
#73520 = CARTESIAN_POINT ( 'NONE',  ( 164.4414259850711915, 245.8260906552167171, -6.983224448873608381 ) ) ;
#73521 = CARTESIAN_POINT ( 'NONE',  ( 124.1521724663614492, 251.6744531367911577, 4.594050593750047540 ) ) ;
#73522 = ORIENTED_EDGE ( 'NONE', *, *, #50727, .T. ) ;
#73523 = CARTESIAN_POINT ( 'NONE',  ( 146.5046981847821428, 276.8934145268504494, 0.02269072295920678689 ) ) ;
#73524 = DIRECTION ( 'NONE',  ( -0.3105719460338643989, -0.9505498757754579087, 0.000000000000000000 ) ) ;
#73525 = CARTESIAN_POINT ( 'NONE',  ( 199.2985792285494995, 282.8172808829962150, -17.62369519561723408 ) ) ;
#73526 = EDGE_CURVE ( 'NONE', #94383, #94311, #77478, .T. ) ;
#73527 = CARTESIAN_POINT ( 'NONE',  ( 164.3961040135806968, 245.9045906125373904, 7.095190383188031191 ) ) ;
#73528 = EDGE_CURVE ( 'NONE', #78092, #31631, #54640, .T. ) ;
#73529 = CARTESIAN_POINT ( 'NONE',  ( 73.60933432321982650, 55.64367109616565443, 16.10230547196763595 ) ) ;
#73530 = DIRECTION ( 'NONE',  ( -0.000000000000000000, -0.000000000000000000, -1.000000000000000000 ) ) ;
#73531 = EDGE_LOOP ( 'NONE', ( #85591, #29987, #28565, #61251 ) ) ;
#73532 = CARTESIAN_POINT ( 'NONE',  ( 80.64248598438099691, 57.30349260802955058, -16.23283928966112200 ) ) ;
#73533 = EDGE_CURVE ( 'NONE', #2731, #29851, #9172, .T. ) ;
#73534 = LINE ( 'NONE', #96867, #25218 ) ;
#73535 = CARTESIAN_POINT ( 'NONE',  ( 205.9226911964632052, 273.9784317468465815, -10.54881836492553404 ) ) ;
#73536 = CARTESIAN_POINT ( 'NONE',  ( 138.9828575061699496, 260.2369531367911009, -4.594050593750048428 ) ) ;
#73537 = CARTESIAN_POINT ( 'NONE',  ( 190.1858949294064871, 301.2353624297489887, -5.249932979468886707 ) ) ;
#73538 = CARTESIAN_POINT ( 'NONE',  ( 69.22557465782018937, 70.15747877712618674, 3.469537545477277884 ) ) ;
#73539 = CARTESIAN_POINT ( 'NONE',  ( 154.5458477507173143, 280.1990093249386859, 3.569508088704419713 ) ) ;
#73540 = B_SPLINE_CURVE_WITH_KNOTS ( 'NONE', 3,
 ( #38355, #83018, #21195, #69265, #91604, #13588 ),
 .UNSPECIFIED., .F., .F.,
 ( 4, 2, 4 ),
 ( 0.000000000000000000, 0.0004057782954188846980, 0.0008115565908377693960 ),
 .UNSPECIFIED. ) ;
#73541 = CARTESIAN_POINT ( 'NONE',  ( 10.82157445631582249, 29.18080186712591839, 3.090169943749475401 ) ) ;
#73542 = CARTESIAN_POINT ( 'NONE',  ( 149.7162292714551199, 271.3308795146458010, 12.12826134257344357 ) ) ;
#73543 = DIRECTION ( 'NONE',  ( 0.3400251696390308997, -0.9404163354663445107, 0.000000000000000000 ) ) ;
#73544 = CARTESIAN_POINT ( 'NONE',  ( 169.3669221716730533, 285.1312214744803555, -8.684624577439414850 ) ) ;
#73545 = CARTESIAN_POINT ( 'NONE',  ( -55.24278990345137430, 55.52121124131609520, 59.99999999999999289 ) ) ;
#73546 = CARTESIAN_POINT ( 'NONE',  ( -65.04438592786723916, 55.88340059208193367, 59.99999999999999289 ) ) ;
#73547 = EDGE_CURVE ( 'NONE', #95263, #70646, #27268, .T. ) ;
#73548 = CARTESIAN_POINT ( 'NONE',  ( 128.9696990949621522, 255.2677522451419350, -5.000000000000047962 ) ) ;
#73549 = CARTESIAN_POINT ( 'NONE',  ( 175.9525681479302932, 285.3181954580452953, -12.02530750686166705 ) ) ;
#73550 = ORIENTED_EDGE ( 'NONE', *, *, #11905, .T. ) ;
#73551 = CARTESIAN_POINT ( 'NONE',  ( 196.1613785401733878, 290.8855212161054737, 15.98157687694135021 ) ) ;
#73552 = CARTESIAN_POINT ( 'NONE',  ( 190.1730848958311810, 301.2575500587478814, 0.2415986433272204748 ) ) ;
#73553 = CARTESIAN_POINT ( 'NONE',  ( -5.399728507075681527, 173.8149278399160949, -9.188101187500095079 ) ) ;
#73554 = CARTESIAN_POINT ( 'NONE',  ( 39.09232661234986494, 199.5024278399160664, -9.188101187500093303 ) ) ;
#73555 = CARTESIAN_POINT ( 'NONE',  ( 84.36910100733514639, 42.65695583307471139, 5.752001605179764887 ) ) ;
#73556 = CARTESIAN_POINT ( 'NONE',  ( 13.10165252270984304, 31.65659080271450421, -1.878358725466461243E-16 ) ) ;
#73557 = PLANE ( 'NONE',  #46454 ) ;
#73558 = CARTESIAN_POINT ( 'NONE',  ( 157.8043799545718286, 257.3217915922150496, -17.97575562758749257 ) ) ;
#73559 = CARTESIAN_POINT ( 'NONE',  ( 72.18990340680744566, 72.03918383723205920, -3.149060597287212104 ) ) ;
#73560 = CARTESIAN_POINT ( 'NONE',  ( 190.1693911629507738, 301.2639477917662703, -5.112716700269980485 ) ) ;
#73561 = CARTESIAN_POINT ( 'NONE',  ( 148.3593702730603070, 275.6694849721874334, 3.735352563252699820 ) ) ;
#73563 = CARTESIAN_POINT ( 'NONE',  ( 80.83312040127718490, 204.1427522451417644, 1.119607411625061291E-15 ) ) ;
#73562 = CARTESIAN_POINT ( 'NONE',  ( 77.34551609424316609, 203.9155109091896065, 2.679491924311254714 ) ) ;
#73564 = CARTESIAN_POINT ( 'NONE',  ( 76.96536368249300608, 60.63192262470904836, 16.19594659928378277 ) ) ;
#73565 = CARTESIAN_POINT ( 'NONE',  ( 204.6075833744878878, 276.2562653119390461, -13.34672481898815910 ) ) ;
#73566 = CARTESIAN_POINT ( 'NONE',  ( -21.31413092498266693, 24.33771760303832465, -10.00000000000000000 ) ) ;
#73568 =( BOUNDED_CURVE ( )  B_SPLINE_CURVE ( 2, ( #79970, #2962, #80982, #10539, #12537, #95176, #19154, #33856, #41413 ),
 .UNSPECIFIED., .F., .T. ) 
 B_SPLINE_CURVE_WITH_KNOTS ( ( 3, 2, 2, 2, 3 ),
 ( 0.1895161290322580627, 0.1908602150537634379, 0.1935483870967741882, 0.1962365591397849385, 0.1975806451612903136 ),
 .UNSPECIFIED. ) 
 CURVE ( )  GEOMETRIC_REPRESENTATION_ITEM ( )  RATIONAL_B_SPLINE_CURVE ( ( 0.9330127018922194093, 0.9330127018922194093, 1.000000000000000000, 0.8660254037844387076, 1.000000000000000000, 0.8660254037844387076, 1.000000000000000000, 0.9330127018922194093, 0.9330127018922194093 ) ) 
 REPRESENTATION_ITEM ( '' )  );
#73567 = CARTESIAN_POINT ( 'NONE',  ( 35.60133525300030755, 191.3615022471902591, -10.00000000000009592 ) ) ;
#73569 = CARTESIAN_POINT ( 'NONE',  ( 181.1843555769024476, 292.6731038405765162, 9.241987700880018863 ) ) ;
#73570 = CARTESIAN_POINT ( 'NONE',  ( 166.8033540930419463, 285.5752247180022323, -7.877208387440095549 ) ) ;
#73571 = CARTESIAN_POINT ( 'NONE',  ( 2.394500126984267396, 178.3149278399160949, -9.188101187500095079 ) ) ;
#73572 = CARTESIAN_POINT ( 'NONE',  ( 168.2746533154106316, 286.3035412645079418, 4.462338258111298472 ) ) ;
#73573 = B_SPLINE_CURVE_WITH_KNOTS ( 'NONE', 3,
 ( #84282, #45716, #76639, #51334, #7224, #38108, #99951, #82302, #12872, #74674 ),
 .UNSPECIFIED., .F., .F.,
 ( 4, 2, 2, 2, 4 ),
 ( 0.000000000000000000, 0.0002622400424272593612, 0.0005244800848545187223, 0.0007867201272817780835, 0.001048960169709037445 ),
 .UNSPECIFIED. ) ;
#73574 = CARTESIAN_POINT ( 'NONE',  ( 192.3606619183491091, 297.4685555102766443, 10.99569063633359889 ) ) ;
#73575 = CARTESIAN_POINT ( 'NONE',  ( 35.63556891041371699, 26.28920272979929607, -7.433330006724141015 ) ) ;
#73576 = CARTESIAN_POINT ( 'NONE',  ( 206.5508451493652444, 272.8904371854448527, 11.05407534521577695 ) ) ;
#73577 = AXIS2_PLACEMENT_3D ( 'NONE', #82760, #89852, #14306 ) ;
#73578 = CARTESIAN_POINT ( 'NONE',  ( 164.7243055739305078, 245.3361288348881999, -1.445094907380085170 ) ) ;
#73579 = CARTESIAN_POINT ( 'NONE',  ( 154.8556227199321427, 262.4291889417971788, 17.77326384500479861 ) ) ;
#73580 = CARTESIAN_POINT ( 'NONE',  ( 34.09918582485539673, 43.18528772668523175, -1.583844403245329602 ) ) ;
#73581 = CARTESIAN_POINT ( 'NONE',  ( 179.7099650035556238, 262.7785925330675241, -12.85976170404427776 ) ) ;
#73582 = APPLICATION_PROTOCOL_DEFINITION ( 'draft international standard', 'automotive_design', 1998, #44826 ) ;
#73583 = ADVANCED_FACE ( 'NONE', ( #96700 ), #58636, .F. ) ;
#73584 = CARTESIAN_POINT ( 'NONE',  ( 10.26703877906431472, 17.87878583063839599, -9.188101187500006262 ) ) ;
#73585 = CARTESIAN_POINT ( 'NONE',  ( 71.59874412008123556, 72.43189726433809028, 0.9745913883648391618 ) ) ;
#73586 = CARTESIAN_POINT ( 'NONE',  ( 11.39049277451480080, 29.68290643055186706, 3.479690158560446702E-15 ) ) ;
#73587 = CARTESIAN_POINT ( 'NONE',  ( 159.6001914315565955, 258.6705862423590361, 17.36259334898762319 ) ) ;
#73588 = LINE ( 'NONE', #80737, #100157 ) ;
#73589 = VERTEX_POINT ( 'NONE', #4455 ) ;
#73590 = CARTESIAN_POINT ( 'NONE',  ( 20.35638218401011912, 30.49103043416549497, -8.090169943749479842 ) ) ;
#73591 = CARTESIAN_POINT ( 'NONE',  ( -4.653128914090328472, 78.77562236714182120, 13.81405534229504717 ) ) ;
#73592 = PLANE ( 'NONE',  #2552 ) ;
#73593 = ORIENTED_EDGE ( 'NONE', *, *, #68385, .F. ) ;
#73594 = CARTESIAN_POINT ( 'NONE',  ( 153.1314981037513121, 265.4154603756023789, 17.73969815997475408 ) ) ;
#73595 = CARTESIAN_POINT ( 'NONE',  ( 164.2672861321391053, 246.1277097281173667, -2.417001679502223777 ) ) ;
#73596 = CARTESIAN_POINT ( 'NONE',  ( 66.36404765992830335, 68.16983728735020520, 4.450399946281168084 ) ) ;
#73597 = CARTESIAN_POINT ( 'NONE',  ( 87.68151411726066158, 45.11153824597518280, 6.862463844403655422 ) ) ;
#73598 = ORIENTED_EDGE ( 'NONE', *, *, #89652, .F. ) ;
#73599 = EDGE_LOOP ( 'NONE', ( #3870, #15668 ) ) ;
#73601 = CARTESIAN_POINT ( 'NONE',  ( 17.29678581741014654, 10.39040679176981996, 1.333680081654574804E-15 ) ) ;
#73600 = CARTESIAN_POINT ( 'NONE',  ( 164.5641499066685469, 246.8022252770303169, -5.664862832761055955 ) ) ;
#73602 = CARTESIAN_POINT ( 'NONE',  ( 153.4619471835925708, 264.8431057800031567, 16.95044998314351758 ) ) ;
#73603 = VERTEX_POINT ( 'NONE', #35353 ) ;
#73604 = DIRECTION ( 'NONE',  ( 0.000000000000000000, 0.000000000000000000, 1.000000000000000000 ) ) ;
#73605 = CARTESIAN_POINT ( 'NONE',  ( 178.2640794854746105, 263.8995157064278487, 15.14098684682329932 ) ) ;
#73606 = ORIENTED_EDGE ( 'NONE', *, *, #56679, .F. ) ;
#73607 = CARTESIAN_POINT ( 'NONE',  ( -19.15453390681661716, 24.31945705462846163, 10.00000000000000000 ) ) ;
#73608 = CARTESIAN_POINT ( 'NONE',  ( 88.48828274770076519, 43.87397573844135934, -0.5490789642627269540 ) ) ;
#73609 = CARTESIAN_POINT ( 'NONE',  ( 81.05466020238847591, 43.66611230261246135, 9.465821864999529822 ) ) ;
#73610 = AXIS2_PLACEMENT_3D ( 'NONE', #88091, #79473, #49033 ) ;
#73611 = VERTEX_POINT ( 'NONE', #19190 ) ;
#73612 = CARTESIAN_POINT ( 'NONE',  ( 203.3286960320409094, 267.8359400968079171, 2.569349860321338941 ) ) ;
#73613 = CARTESIAN_POINT ( 'NONE',  ( 168.1589593212097498, 275.9390298053305628, -16.40258036402506647 ) ) ;
#73614 = CARTESIAN_POINT ( 'NONE',  ( 151.2755745006645896, 275.3008544589386020, -8.292818474215351898 ) ) ;
#73615 = ORIENTED_EDGE ( 'NONE', *, *, #73695, .T. ) ;
#73616 = CARTESIAN_POINT ( 'NONE',  ( 176.7827973027407040, 278.6576878780061861, -15.83051026523116533 ) ) ;
#73617 = CARTESIAN_POINT ( 'NONE',  ( 169.1454831004496384, 261.3880614413394028, -16.47743258951610557 ) ) ;
#73618 = VERTEX_POINT ( 'NONE', #43448 ) ;
#73619 = CARTESIAN_POINT ( 'NONE',  ( 156.7634869529680373, 266.5784725184484500, -16.23112445323594244 ) ) ;
#73620 = VERTEX_POINT ( 'NONE', #50061 ) ;
#73621 = CARTESIAN_POINT ( 'NONE',  ( 157.3802686514316349, 269.1245054408723263, 15.58885404214087878 ) ) ;
#73622 = ORIENTED_EDGE ( 'NONE', *, *, #65240, .F. ) ;
#73623 = CARTESIAN_POINT ( 'NONE',  ( 158.8270733235451075, 260.0119502166541565, 17.68969926203419618 ) ) ;
#73624 = CARTESIAN_POINT ( 'NONE',  ( 147.7232839279827203, 274.7827621062478443, 5.908844693136329873 ) ) ;
#73625 = CARTESIAN_POINT ( 'NONE',  ( 82.42561518943209364, 53.83419803862934572, 15.85509184085860390 ) ) ;
#73626 = CARTESIAN_POINT ( 'NONE',  ( 10.44586698754085674, 29.52903772873355948, -1.583844403245363575 ) ) ;
#73627 = CARTESIAN_POINT ( 'NONE',  ( 199.8071198270451703, 281.1414453001559082, -17.28171234339430029 ) ) ;
#73628 = CARTESIAN_POINT ( 'NONE',  ( 86.68115352851880573, 43.28345336846571456, 0.8059148367177517702 ) ) ;
#73629 = CARTESIAN_POINT ( 'NONE',  ( 158.9356049992396152, 255.3624523400558246, -16.15158836202271075 ) ) ;
#73630 = ORIENTED_EDGE ( 'NONE', *, *, #52370, .F. ) ;
#73632 = CARTESIAN_POINT ( 'NONE',  ( 78.35675126109745747, 56.49915297402233705, -16.20020041168814018 ) ) ;
#73631 = B_SPLINE_CURVE_WITH_KNOTS ( 'NONE', 3,
 ( #38175, #62998, #69093, #32084 ),
 .UNSPECIFIED., .F., .F.,
 ( 4, 4 ),
 ( 0.000000000000000000, 0.0001209126443684359120 ),
 .UNSPECIFIED. ) ;
#73633 = CARTESIAN_POINT ( 'NONE',  ( 21.59633513308047270, 30.65586893147756697, -7.433330006724137462 ) ) ;
#73634 = CARTESIAN_POINT ( 'NONE',  ( 165.0565241268390366, 244.7607094220335568, 2.191926263411719589 ) ) ;
#73635 = CARTESIAN_POINT ( 'NONE',  ( 206.4229368915142686, 273.1119807867502800, 10.31819530520674810 ) ) ;
#73637 = ORIENTED_EDGE ( 'NONE', *, *, #89062, .T. ) ;
#73636 = CARTESIAN_POINT ( 'NONE',  ( 83.73300642799732429, 41.31124303260040875, -2.428015798050618734 ) ) ;
#73638 = ORIENTED_EDGE ( 'NONE', *, *, #31697, .T. ) ;
#73639 = CARTESIAN_POINT ( 'NONE',  ( 185.9583416565622258, 276.2403346773022577, 16.51595490223188278 ) ) ;
#73640 = CARTESIAN_POINT ( 'NONE',  ( -71.45866285464214229, 45.60329508610311677, 10.00000000000000000 ) ) ;
#73641 = CARTESIAN_POINT ( 'NONE',  ( 188.2505817719666652, 300.0599093194876446, 0.6416181545256018914 ) ) ;
#73642 = CARTESIAN_POINT ( 'NONE',  ( 181.1375824994216828, 258.0330255649733999, 9.585308223983551201 ) ) ;
#73643 = EDGE_CURVE ( 'NONE', #75541, #31533, #68376, .T. ) ;
#73644 = AXIS2_PLACEMENT_3D ( 'NONE', #23780, #48080, #69880 ) ;
#73645 = CARTESIAN_POINT ( 'NONE',  ( 160.3446501917713931, 252.9219144764300893, -16.21746572878571158 ) ) ;
#73646 = EDGE_CURVE ( 'NONE', #91333, #39135, #4971, .T. ) ;
#73647 = CARTESIAN_POINT ( 'NONE',  ( 148.4879991328100175, 273.4582365181666432, -8.909052134456917571 ) ) ;
#73648 = VERTEX_POINT ( 'NONE', #65747 ) ;
#73649 = CARTESIAN_POINT ( 'NONE',  ( 157.4655681218829670, 259.9086309006383431, -17.75190047967350893 ) ) ;
#73650 = CARTESIAN_POINT ( 'NONE',  ( 205.7347617114599529, 273.8573068914000714, 10.24322677079193333 ) ) ;
#73651 = CARTESIAN_POINT ( 'NONE',  ( 123.4362054459082572, 253.6199935810940929, 2.679491924311251605 ) ) ;
#73652 = EDGE_CURVE ( 'NONE', #79145, #87147, #96238, .T. ) ;
#73653 = CARTESIAN_POINT ( 'NONE',  ( -19.65312891409032403, 93.06504152958505927, 0.000000000000000000 ) ) ;
#73654 = ADVANCED_FACE ( 'NONE', ( #28755 ), #39350, .T. ) ;
#73655 = CARTESIAN_POINT ( 'NONE',  ( 35.94413697178375600, 184.8927522451418213, 10.00000000000009592 ) ) ;
#73656 = CARTESIAN_POINT ( 'NONE',  ( 113.4086522182495287, 224.0327760586659167, 1.948934522072302763E-15 ) ) ;
#73657 = AXIS2_PLACEMENT_3D ( 'NONE', #38782, #30195, #85444 ) ;
#73658 = CARTESIAN_POINT ( 'NONE',  ( 183.9912383556867610, 296.9911047963649935, -2.788240429904596862 ) ) ;
#73659 = CARTESIAN_POINT ( 'NONE',  ( 167.7859171384422154, 281.8497203286631816, -10.91337641437639761 ) ) ;
#73660 = CARTESIAN_POINT ( 'NONE',  ( 89.66121469831512059, 234.1199935810940929, 2.679491924311251605 ) ) ;
#73661 = CARTESIAN_POINT ( 'NONE',  ( 208.2512496840233496, 269.9452501379965952, 1.821023623773176947 ) ) ;
#73662 = CARTESIAN_POINT ( 'NONE',  ( 27.67213724359008964, 174.5327760586659451, 1.948934522072303157E-15 ) ) ;
#73663 = LINE ( 'NONE', #2780, #44595 ) ;
#73664 = ORIENTED_EDGE ( 'NONE', *, *, #96675, .T. ) ;
#73665 = ORIENTED_EDGE ( 'NONE', *, *, #29165, .T. ) ;
#73666 = DIRECTION ( 'NONE',  ( -0.8393827800519415572, -0.5435407515102007592, 0.000000000000000000 ) ) ;
#73667 = CARTESIAN_POINT ( 'NONE',  ( 185.5146895125434980, 259.2464410770732002, -5.300532970778875530 ) ) ;
#73668 = CARTESIAN_POINT ( 'NONE',  ( 19.51315699177561314, 193.6199935810941213, 2.679491924311251605 ) ) ;
#73669 = CARTESIAN_POINT ( 'NONE',  ( 190.7569505155522904, 300.2462651405980978, -5.670926626284815697 ) ) ;
#73670 = CARTESIAN_POINT ( 'NONE',  ( -27.23973145446879940, 106.0054225863516280, 45.19937630303415688 ) ) ;
#73671 = CARTESIAN_POINT ( 'NONE',  ( 207.1432938686257046, 271.8642859028066141, -6.405155839440290322 ) ) ;
#73672 = CARTESIAN_POINT ( 'NONE',  ( 181.8774662184618194, 285.1120569720015965, 15.89814067624403116 ) ) ;
#73673 = DIRECTION ( 'NONE',  ( 0.4999999999999998890, -0.8660254037844385966, 0.000000000000000000 ) ) ;
#73674 = CARTESIAN_POINT ( 'NONE',  ( 53.97765888354242492, 189.7202760586659451, -5.415160957724236172E-17 ) ) ;
#73675 = CARTESIAN_POINT ( 'NONE',  ( 104.2158063034570290, 217.6427522451417360, 1.119607411625061291E-15 ) ) ;
#73676 = ORIENTED_EDGE ( 'NONE', *, *, #81736, .F. ) ;
#73677 = CARTESIAN_POINT ( 'NONE',  ( 79.25704083171595471, 59.98661423191555286, -16.48971415753125314 ) ) ;
#73678 = VECTOR ( 'NONE', #81152, 1000.000000000000000 ) ;
#73679 = CARTESIAN_POINT ( 'NONE',  ( 2.016134656476094023, 159.7202760586659736, -5.415160957724236172E-17 ) ) ;
#73680 = CARTESIAN_POINT ( 'NONE',  ( 72.97045661744296297, 70.75163901906789476, -7.462049238873905033 ) ) ;
#73681 = CARTESIAN_POINT ( 'NONE',  ( 198.5201458116119397, 286.8000164587433005, -18.30276554821096013 ) ) ;
#73682 = FACE_OUTER_BOUND ( 'NONE', #18298, .T. ) ;
#73683 = CARTESIAN_POINT ( 'NONE',  ( 193.1028332910263998, 296.1830769848763225, -12.04975758233223893 ) ) ;
#73684 = CARTESIAN_POINT ( 'NONE',  ( -57.88150100324660485, 35.92665207732902388, 10.00000000000000000 ) ) ;
#73685 = CARTESIAN_POINT ( 'NONE',  ( 204.1633547645365638, 275.3510256380408237, 13.36249479004741580 ) ) ;
#73686 = CARTESIAN_POINT ( 'NONE',  ( 69.80643203780810779, 69.29736018695484745, 6.650341497908645039 ) ) ;
#73687 = CARTESIAN_POINT ( 'NONE',  ( 189.8238368927809745, 301.8624653444729802, -0.3620111495846872751 ) ) ;
#73688 = VERTEX_POINT ( 'NONE', #63138 ) ;
#73689 = CARTESIAN_POINT ( 'NONE',  ( -0.7717317059461257234, 170.3615022471902591, -10.00000000000009592 ) ) ;
#73690 = CYLINDRICAL_SURFACE ( 'NONE', #51453, 70.00000000000002842 ) ;
#73691 = CARTESIAN_POINT ( 'NONE',  ( 123.3675972660055749, 242.0333772461660544, 9.188101187500095079 ) ) ;
#73692 = CARTESIAN_POINT ( 'NONE',  ( 17.33597792084844258, 30.98502408145592213, -5.678558825948271327 ) ) ;
#73693 = CARTESIAN_POINT ( 'NONE',  ( 74.70717368071740339, 67.14741735073857853, 12.46980216122492990 ) ) ;
#73694 = CARTESIAN_POINT ( 'NONE',  ( 58.97569090598252473, 178.8759306620404175, -17.47570218321536473 ) ) ;
#73695 = EDGE_CURVE ( 'NONE', #89109, #76961, #32238, .T. ) ;
#73697 = CARTESIAN_POINT ( 'NONE',  ( 75.22447641198338886, 66.97122069168695191, 13.23119059164781852 ) ) ;
#73696 = DIRECTION ( 'NONE',  ( 1.000000000000000000, 0.000000000000000000, 0.000000000000000000 ) ) ;
#73698 = CARTESIAN_POINT ( 'NONE',  ( 190.8003542858887158, 300.1710876051355399, -7.952726366508386491 ) ) ;
#73699 = VERTEX_POINT ( 'NONE', #40817 ) ;
#73700 = B_SPLINE_CURVE_WITH_KNOTS ( 'NONE', 3,
 ( #15183, #46083, #14705, #30902 ),
 .UNSPECIFIED., .F., .F.,
 ( 4, 4 ),
 ( 0.03034436796817569643, 0.03943245488163680396 ),
 .UNSPECIFIED. ) ;
#73701 = CARTESIAN_POINT ( 'NONE',  ( 191.2645787786270262, 299.3670271975948367, 7.309947121636420242 ) ) ;
#73702 = CARTESIAN_POINT ( 'NONE',  ( 164.0609569930187206, 246.4850822801560639, 8.623773733057504387 ) ) ;
#73703 = ADVANCED_FACE ( 'NONE', ( #63641 ), #77858, .T. ) ;
#73704 = CARTESIAN_POINT ( 'NONE',  ( 181.4283053378885597, 267.7238133557910373, 16.48022347432943135 ) ) ;
#73705 = CARTESIAN_POINT ( 'NONE',  ( 169.5303480748956417, 265.9959136028709281, -17.12794529520477838 ) ) ;
#73706 = CARTESIAN_POINT ( 'NONE',  ( 81.53672410393728853, 56.04530558232496418, -16.40539795406885304 ) ) ;
#73707 = ORIENTED_EDGE ( 'NONE', *, *, #16908, .T. ) ;
#73708 = CARTESIAN_POINT ( 'NONE',  ( 69.03448990137108865, 67.04097112400465619, 9.310083799442864461 ) ) ;
#73709 = CARTESIAN_POINT ( 'NONE',  ( 165.6547257697228588, 269.1390321728339359, -17.08687207675598430 ) ) ;
#73710 = CARTESIAN_POINT ( 'NONE',  ( 82.90096945690618213, 41.76309762099524647, 4.006682518572778129 ) ) ;
#73711 = CARTESIAN_POINT ( 'NONE',  ( 80.52421224103476050, 57.15337481666037434, 16.20884293195102899 ) ) ;
#73712 = AXIS2_PLACEMENT_3D ( 'NONE', #62284, #96750, #19236 ) ;
#73713 = CARTESIAN_POINT ( 'NONE',  ( 185.8923765766539589, 296.7039355726019494, 5.058929278049905776 ) ) ;
#73714 = CARTESIAN_POINT ( 'NONE',  ( 70.52245475048280809, 71.40325566580152383, 0.2397668356339602846 ) ) ;
#73715 = CARTESIAN_POINT ( 'NONE',  ( -13.11024591527734628, 6.000000000000000000, -32.50000000000000000 ) ) ;
#73716 = ORIENTED_EDGE ( 'NONE', *, *, #10976, .F. ) ;
#73717 = CARTESIAN_POINT ( 'NONE',  ( 3.720166145283430925, 25.08080186712590276, -3.090169943749475845 ) ) ;
#73718 = CARTESIAN_POINT ( 'NONE',  ( 86.89529822776817980, 227.6427522451419065, 10.00000000000009415 ) ) ;
#73719 = EDGE_LOOP ( 'NONE', ( #21473, #94951, #23881, #77844 ) ) ;
#73720 = PLANE ( 'NONE',  #53050 ) ;
#73721 = ADVANCED_FACE ( 'NONE', ( #17032 ), #47433, .F. ) ;
#73722 = CARTESIAN_POINT ( 'NONE',  ( 194.1852025340051284, 294.3083584634874796, -15.46421316575964688 ) ) ;
#73723 = CARTESIAN_POINT ( 'NONE',  ( 157.8749902780253365, 263.0387574327914422, -16.96638006302123713 ) ) ;
#73724 = ORIENTED_EDGE ( 'NONE', *, *, #73279, .T. ) ;
#73725 = CARTESIAN_POINT ( 'NONE',  ( 79.03265986744987970, 60.09179323390554117, 16.12040655615884077 ) ) ;
#73726 = DIRECTION ( 'NONE',  ( 0.2347357813929421555, -0.4065742997269585213, 0.8829475928589297640 ) ) ;
#73727 = CARTESIAN_POINT ( 'NONE',  ( 75.37843707191279918, 53.50823561223473490, 16.04097401286667335 ) ) ;
#73728 = VERTEX_POINT ( 'NONE', #8942 ) ;
#73729 = CARTESIAN_POINT ( 'NONE',  ( 86.72372382049401551, 227.0024278399160949, 9.188101187500095079 ) ) ;
#73730 = CARTESIAN_POINT ( 'NONE',  ( 78.99320801705290762, 51.70865386193722202, -15.35962929047159520 ) ) ;
#73731 = CARTESIAN_POINT ( 'NONE',  ( 41.82599275875796252, 62.29945068332010294, -10.00000000000000000 ) ) ;
#73732 = CARTESIAN_POINT ( 'NONE',  ( 182.3576772462011206, 258.0377563476427554, -5.917524771864123068 ) ) ;
#73733 = ORIENTED_EDGE ( 'NONE', *, *, #90750, .F. ) ;
#73734 = ORIENTED_EDGE ( 'NONE', *, *, #17598, .T. ) ;
#73735 = CARTESIAN_POINT ( 'NONE',  ( 194.5481722404243214, 283.9256704378062182, -17.81052777154215860 ) ) ;
#73736 = ORIENTED_EDGE ( 'NONE', *, *, #27275, .F. ) ;
#73737 = DIRECTION ( 'NONE',  ( 0.8660254037844384856, 0.5000000000000002220, 3.252519625699449945E-16 ) ) ;
#73738 = ORIENTED_EDGE ( 'NONE', *, *, #29393, .F. ) ;
#73739 = CARTESIAN_POINT ( 'NONE',  ( 75.53649560587535916, 61.34551538626548250, 15.39653084909254233 ) ) ;
#73740 = CARTESIAN_POINT ( 'NONE',  ( 203.5555343017997529, 278.0784677578903370, -15.71723084798551362 ) ) ;
#73741 = ORIENTED_EDGE ( 'NONE', *, *, #99048, .T. ) ;
#73742 = CARTESIAN_POINT ( 'NONE',  ( 207.4139425164918293, 271.3955086937027090, -6.918700682290102932 ) ) ;
#73743 = CARTESIAN_POINT ( 'NONE',  ( 82.20918741961230580, 40.63530303777752550, 3.361810051138397704 ) ) ;
#73744 = CARTESIAN_POINT ( 'NONE',  ( 80.97755617445423582, 43.68821843711276642, -9.544220554497766074 ) ) ;
#73745 = PLANE ( 'NONE',  #20396 ) ;
#73746 = CARTESIAN_POINT ( 'NONE',  ( 28.46864935082047410, 149.7156766241961350, 37.50000000000000000 ) ) ;
#73747 = CARTESIAN_POINT ( 'NONE',  ( -19.60707684373364046, 93.19917931493495189, 59.99999999999999289 ) ) ;
#73748 = CARTESIAN_POINT ( 'NONE',  ( 136.8177939967088435, 258.9869531367911009, 4.594050593750046652 ) ) ;
#73749 = DIRECTION ( 'NONE',  ( 0.4999999999999998890, -0.8660254037844385966, 0.000000000000000000 ) ) ;
#73750 = CARTESIAN_POINT ( 'NONE',  ( 70.96527508345572244, 61.11905909413832205, -14.48497578840443900 ) ) ;
#73751 = B_SPLINE_CURVE_WITH_KNOTS ( 'NONE', 3,
 ( #23352, #93300, #46144, #9171 ),
 .UNSPECIFIED., .F., .F.,
 ( 4, 4 ),
 ( 0.008808793980068530330, 0.01508001664632129327 ),
 .UNSPECIFIED. ) ;
#73752 = CARTESIAN_POINT ( 'NONE',  ( 8.149503075528279794, 26.74646525600388358, 2.839279412974139660 ) ) ;
#73753 = ORIENTED_EDGE ( 'NONE', *, *, #58963, .F. ) ;
#73754 = VECTOR ( 'NONE', #60264, 1000.000000000000000 ) ;
#73755 = PLANE ( 'NONE',  #89914 ) ;
#73757 = ORIENTED_EDGE ( 'NONE', *, *, #57053, .T. ) ;
#73756 = CARTESIAN_POINT ( 'NONE',  ( 85.53665298850141596, 48.34007191699684114, -12.21196891364052739 ) ) ;
#73758 = DIRECTION ( 'NONE',  ( 0.9874311856918874808, -0.1580495287025984186, 0.000000000000000000 ) ) ;
#73759 = EDGE_CURVE ( 'NONE', #49794, #8436, #27536, .T. ) ;
#73760 = CARTESIAN_POINT ( 'NONE',  ( 202.8211298556536804, 279.3504935719197988, 17.07914446815911447 ) ) ;
#73761 = CARTESIAN_POINT ( 'NONE',  ( 76.27279963928798168, 65.10967569403835853, -14.21370627898815542 ) ) ;
#73762 = CARTESIAN_POINT ( 'NONE',  ( 153.4389471588997651, 276.9034970075614410, 7.158391495164361906 ) ) ;
#73763 = CARTESIAN_POINT ( 'NONE',  ( 84.18008060907449419, 49.39655662477972697, -13.52276195833983508 ) ) ;
#73764 = VECTOR ( 'NONE', #60038, 1000.000000000000000 ) ;
#73765 = CARTESIAN_POINT ( 'NONE',  ( 171.6183182742749977, 280.0105497640429917, 13.87264028713023301 ) ) ;
#73766 = CARTESIAN_POINT ( 'NONE',  ( 86.09437418083463456, 43.42260935030300573, 3.587124466458941008 ) ) ;
#73767 = CARTESIAN_POINT ( 'NONE',  ( 88.26279489949382651, 43.89118386701247942, -2.126167786569203244 ) ) ;
#73768 = ORIENTED_EDGE ( 'NONE', *, *, #15466, .T. ) ;
#73769 = CARTESIAN_POINT ( 'NONE',  ( 184.7835433439430801, 272.8597739924990151, -17.09939324130442273 ) ) ;
#73770 = CARTESIAN_POINT ( 'NONE',  ( 65.75918626998540617, 69.09342105489017172, 0.05498200154574946208 ) ) ;
#73771 = ORIENTED_EDGE ( 'NONE', *, *, #720, .F. ) ;
#73773 = CARTESIAN_POINT ( 'NONE',  ( 160.4213754921470922, 276.0766563818076520, 12.64007677385747996 ) ) ;
#73772 = B_SPLINE_CURVE_WITH_KNOTS ( 'NONE', 3,
 ( #84857, #85365, #31105, #51558, #93460, #84363, #54910, #46816, #7826, #61993, #100041, #15912, #13082, #70104, #85889, #47309, #36349, #67252, #14910, #28760, #22521, #3246, #49325, #94455, #71139, #17415, #72651, #64018, #95968, #79270, #71644, #2238, #64524, #3733, #25523, #87406, #10332, #88385, #49816, #11347, #65511, #24514, #16910, #59379, #36593, #35105, #74640, #20936, #5215, #27530, #89851, #52295, #50802, #97923 ),
 .UNSPECIFIED., .F., .F.,
 ( 4, 2, 2, 2, 2, 2, 2, 2, 2, 2, 2, 2, 2, 2, 2, 2, 2, 2, 2, 2, 2, 2, 2, 2, 2, 2, 4 ),
 ( 0.0003707374380231760508, 0.0008344351438995525547, 0.001066283996837772601, 0.001298132849775992430, 0.001414057276245102345, 0.001529981702714212259, 0.001645906129183322391, 0.001761830555652432522, 0.001993679408590594022, 0.002225528261528755738, 0.002689225967405013250, 0.003152923673281270763, 0.004080319085033785355, 0.005007714496786301248, 0.005471412202662599526, 0.005703261055600751701, 0.005819185482069867688, 0.005877147695304387950, 0.005935109908538907346, 0.005993072121773427609, 0.006051034335007947872, 0.006166958761476983193, 0.006398807614415211696, 0.006862505320291640946, 0.007326203026168070197, 0.007558051879106252730, 0.007789900732044434395 ),
 .UNSPECIFIED. ) ;
#73774 = EDGE_CURVE ( 'NONE', #77218, #78854, #46942, .T. ) ;
#73775 = CARTESIAN_POINT ( 'NONE',  ( 156.8019257795724002, 276.6452858554906697, 10.13430466171780786 ) ) ;
#73776 = DIRECTION ( 'NONE',  ( -1.000000000000000000, 0.000000000000000000, 0.000000000000000000 ) ) ;
#73777 = FACE_OUTER_BOUND ( 'NONE', #59204, .T. ) ;
#73778 = CARTESIAN_POINT ( 'NONE',  ( 164.7211056338534547, 274.2655263718911556, 14.88749732853323593 ) ) ;
#73780 = CARTESIAN_POINT ( 'NONE',  ( 87.96634291186354915, 44.23737611247270252, 2.817315086374476252 ) ) ;
#73779 = CARTESIAN_POINT ( 'NONE',  ( 161.3905752240380593, 281.4725768632542895, -7.270332528193686805 ) ) ;
#73781 = CARTESIAN_POINT ( 'NONE',  ( 202.6672992768344841, 269.6846706196681680, 6.012455439154622994 ) ) ;
#73782 = ORIENTED_EDGE ( 'NONE', *, *, #16681, .T. ) ;
#73783 = CARTESIAN_POINT ( 'NONE',  ( 73.21090299573339166, 62.05059075953648318, -14.66927370496624228 ) ) ;
#73784 = CARTESIAN_POINT ( 'NONE',  ( 189.8717058746474606, 274.3034288976620019, -15.65974089894849364 ) ) ;
#73785 = CARTESIAN_POINT ( 'NONE',  ( 73.90979809287503599, 65.40799970079461900, -13.26813225058578460 ) ) ;
#73786 = CARTESIAN_POINT ( 'NONE',  ( 6.802937163926562114, 15.87878583063839066, -9.188101187500006262 ) ) ;
#73787 = VECTOR ( 'NONE', #9884, 1000.000000000000227 ) ;
#73788 = CARTESIAN_POINT ( 'NONE',  ( -17.33262083840143930, 129.0458036431182904, 30.52142883766505221 ) ) ;
#73789 = FACE_OUTER_BOUND ( 'NONE', #12827, .T. ) ;
#73790 = FACE_OUTER_BOUND ( 'NONE', #77488, .T. ) ;
#73791 = CARTESIAN_POINT ( 'NONE',  ( 0.1211834420501121945, 177.0024278399160949, -9.188101187500093303 ) ) ;
#73792 = CARTESIAN_POINT ( 'NONE',  ( 105.6408794604690797, 240.9869531367911293, 4.594050593750046652 ) ) ;
#73793 = LINE ( 'NONE', #98605, #66116 ) ;
#73794 = CARTESIAN_POINT ( 'NONE',  ( 186.1423004029541062, 295.4822973340021690, -7.680234142728118663 ) ) ;
#73795 = CARTESIAN_POINT ( 'NONE',  ( -19.65312891409030271, 93.06504152958497400, 10.00000000000000888 ) ) ;
#73796 = CARTESIAN_POINT ( 'NONE',  ( 196.7523914512457281, 284.9123565375628573, 17.81558562320455508 ) ) ;
#73797 = CARTESIAN_POINT ( 'NONE',  ( 160.8319974213378600, 281.7448561697519267, 5.375735037517149095 ) ) ;
#73798 = CARTESIAN_POINT ( 'NONE',  ( 147.6884207308302450, 274.8431469350302336, -8.096293592099874203 ) ) ;
#73799 = DIRECTION ( 'NONE',  ( -0.2473641778533918756, -0.9689225787001330970, 0.000000000000000000 ) ) ;
#73800 = CARTESIAN_POINT ( 'NONE',  ( 85.05760017557965114, 49.81609225799626017, 13.45342997944402796 ) ) ;
#73801 = CARTESIAN_POINT ( 'NONE',  ( 48.51954752611815991, 205.4865022471903444, -10.00000000000009592 ) ) ;
#73802 = CARTESIAN_POINT ( 'NONE',  ( 165.6450024763602755, 253.6044069627646991, -13.13053692596552047 ) ) ;
#73803 = CARTESIAN_POINT ( 'NONE',  ( 176.0505323877982846, 265.6043802274069208, -15.93901269056853920 ) ) ;
#73804 = CARTESIAN_POINT ( 'NONE',  ( 89.24104401994878799, 213.1423013555409796, -4.594050593750043987 ) ) ;
#73805 = CARTESIAN_POINT ( 'NONE',  ( 207.3646600298985447, 271.4808684644054324, -5.284084612275558257 ) ) ;
#73806 = CARTESIAN_POINT ( 'NONE',  ( 72.64192451535615191, 57.19042016050428145, 15.87647339435071103 ) ) ;
#73807 = CARTESIAN_POINT ( 'NONE',  ( -15.78145869460660045, 102.8555426466057838, 12.52892818809898934 ) ) ;
#73809 = CARTESIAN_POINT ( 'NONE',  ( 151.7927911171883295, 267.7341688927767791, 15.72584582110084206 ) ) ;
#73808 = CARTESIAN_POINT ( 'NONE',  ( 195.9359860111818250, 291.2759125279654882, 17.49638312768267312 ) ) ;
#73810 = B_SPLINE_CURVE_WITH_KNOTS ( 'NONE', 3,
 ( #71221, #63096, #24593, #15483 ),
 .UNSPECIFIED., .F., .F.,
 ( 4, 4 ),
 ( 0.007902357107153172230, 0.01373811809388502357 ),
 .UNSPECIFIED. ) ;
#73811 = CARTESIAN_POINT ( 'NONE',  ( 198.8194531333411419, 286.2816009704309863, -17.01510935557533344 ) ) ;
#73812 = CARTESIAN_POINT ( 'NONE',  ( 204.4092890902271904, 276.1033601826059112, -13.04005437736222106 ) ) ;
#73814 = ADVANCED_FACE ( 'NONE', ( #24637 ), #23126, .T. ) ;
#73813 = CIRCLE ( 'NONE', #75487, 70.00000000000001421 ) ;
#73815 = CARTESIAN_POINT ( 'NONE',  ( 36.75658403392715456, 24.14754757982092315, -5.678558825948275768 ) ) ;
#73816 = CARTESIAN_POINT ( 'NONE',  ( 192.5143468344189728, 297.2023654272867361, -12.06830393602581530 ) ) ;
#73817 = CARTESIAN_POINT ( 'NONE',  ( 131.7301550730730071, 246.8615022471902591, -10.00000000000009592 ) ) ;
#73818 = ORIENTED_EDGE ( 'NONE', *, *, #62888, .T. ) ;
#73819 = CARTESIAN_POINT ( 'NONE',  ( 30.02984208470827454, 19.19860640527293327, 2.839279412974134775 ) ) ;
#73820 = LINE ( 'NONE', #35308, #73356 ) ;
#73821 = AXIS2_PLACEMENT_3D ( 'NONE', #98690, #76850, #7447 ) ;
#73822 = CARTESIAN_POINT ( 'NONE',  ( 164.3663504224794565, 247.9561253440330972, -9.019399920391260039 ) ) ;
#73823 = CARTESIAN_POINT ( 'NONE',  ( 188.0428630768715834, 286.0956317496587644, -16.61304186841477559 ) ) ;
#73824 = EDGE_CURVE ( 'NONE', #24668, #44579, #1854, .T. ) ;
#73825 = ORIENTED_EDGE ( 'NONE', *, *, #92683, .F. ) ;
#73826 = AXIS2_PLACEMENT_3D ( 'NONE', #88009, #79886, #96088 ) ;
#73827 = CARTESIAN_POINT ( 'NONE',  ( 86.13530110067358692, 47.09369226531615737, 10.77952153921811096 ) ) ;
#73828 = CARTESIAN_POINT ( 'NONE',  ( 74.80446345125277219, 64.37471161530348240, 14.55526155763435447 ) ) ;
#73829 = CARTESIAN_POINT ( 'NONE',  ( 202.9526507793443955, 267.5288703438144466, -1.989423397307486185 ) ) ;
#73830 = CARTESIAN_POINT ( 'NONE',  ( 87.37434817825219113, 45.00237579746140426, -6.140289852623291189 ) ) ;
#73831 = CARTESIAN_POINT ( 'NONE',  ( 138.2253456014563255, 240.6115022471902023, -5.000000000000041744 ) ) ;
#73832 = CARTESIAN_POINT ( 'NONE',  ( 157.8719920515997046, 257.2046840049564480, -17.69857783492101433 ) ) ;
#73833 = CARTESIAN_POINT ( 'NONE',  ( 74.92984376288937653, 53.18925172189641160, 16.51450970368439997 ) ) ;
#73834 = VERTEX_POINT ( 'NONE', #47925 ) ;
#73835 = CARTESIAN_POINT ( 'NONE',  ( 188.6826127332440421, 272.6057162039079458, 16.71479996418005243 ) ) ;
#73836 = ORIENTED_EDGE ( 'NONE', *, *, #1249, .T. ) ;
#73837 = CARTESIAN_POINT ( 'NONE',  ( 196.9200716942098950, 264.9052758880268925, -4.632697318226754568 ) ) ;
#73838 = CARTESIAN_POINT ( 'NONE',  ( 66.04055754153552016, 68.56503372374930905, 4.418449956977249293 ) ) ;
#73839 = EDGE_CURVE ( 'NONE', #34021, #63497, #61417, .T. ) ;
#73840 = ORIENTED_EDGE ( 'NONE', *, *, #351, .F. ) ;
#73841 = CARTESIAN_POINT ( 'NONE',  ( 85.60299542505936188, 42.69774087082240754, 0.4164213344292336805 ) ) ;
#73842 = ORIENTED_EDGE ( 'NONE', *, *, #13412, .F. ) ;
#73843 = CARTESIAN_POINT ( 'NONE',  ( 189.5277700490664472, 290.0407984534384127, 14.44961698594945609 ) ) ;
#73844 = CARTESIAN_POINT ( 'NONE',  ( 158.7703600882743729, 255.6486649215402167, 17.63461153596049158 ) ) ;
#73845 = CARTESIAN_POINT ( 'NONE',  ( 149.6191658661038559, 251.0643266524160140, 9.188101187500095079 ) ) ;
#73846 = CARTESIAN_POINT ( 'NONE',  ( 87.96405694255219032, 44.24133552746449283, -4.384643187820144838 ) ) ;
#73847 = CARTESIAN_POINT ( 'NONE',  ( 79.99999999999997158, 26.16025403784438907, -54.99999999999999289 ) ) ;
#73848 = CARTESIAN_POINT ( 'NONE',  ( -19.65312891409030271, 93.06504152958497400, 59.99999999999999289 ) ) ;
#73849 = CARTESIAN_POINT ( 'NONE',  ( 38.53854167689037524, 24.11110640527295246, -2.839279412974138328 ) ) ;
#73850 = AXIS2_PLACEMENT_3D ( 'NONE', #56582, #33812, #62672 ) ;
#73851 = CARTESIAN_POINT ( 'NONE',  ( 77.16999198201305887, 59.24405183509369266, -16.02415114386362305 ) ) ;
#73852 = CYLINDRICAL_SURFACE ( 'NONE', #44961, 70.00000000000002842 ) ;
#73853 = EDGE_CURVE ( 'NONE', #74497, #62997, #95523, .T. ) ;
#73854 = CARTESIAN_POINT ( 'NONE',  ( 68.07728789491675059, 210.1115022471902591, 10.00000000000009592 ) ) ;
#73855 = AXIS2_PLACEMENT_3D ( 'NONE', #86073, #92640, #16597 ) ;
#73856 = ORIENTED_EDGE ( 'NONE', *, *, #31023, .T. ) ;
#73857 = ORIENTED_EDGE ( 'NONE', *, *, #60899, .F. ) ;
#73858 = DIRECTION ( 'NONE',  ( -0.5000000000000014433, 0.8660254037844378194, 0.000000000000000000 ) ) ;
#73859 =( BOUNDED_CURVE ( )  B_SPLINE_CURVE ( 2, ( #51578, #81040, #51064, #97218, #19212, #88148, #20194, #35372, #13098 ),
 .UNSPECIFIED., .F., .T. ) 
 B_SPLINE_CURVE_WITH_KNOTS ( ( 3, 2, 2, 2, 3 ),
 ( 0.1975806451612903136, 0.1989247311827956888, 0.2016129032258064391, 0.2043010752688172171, 0.2056451612903225923 ),
 .UNSPECIFIED. ) 
 CURVE ( )  GEOMETRIC_REPRESENTATION_ITEM ( )  RATIONAL_B_SPLINE_CURVE ( ( 0.9330127018922194093, 0.9330127018922194093, 1.000000000000000000, 0.8660254037844387076, 1.000000000000000000, 0.8660254037844387076, 1.000000000000000000, 0.9330127018922194093, 0.9330127018922194093 ) ) 
 REPRESENTATION_ITEM ( '' )  );
#73860 = CARTESIAN_POINT ( 'NONE',  ( 204.1953342137782954, 276.9703018036655067, 13.84727111424505885 ) ) ;
#73861 = CARTESIAN_POINT ( 'NONE',  ( 85.70666193128211319, 48.42516261524464483, -11.73486726784230072 ) ) ;
#73862 = CARTESIAN_POINT ( 'NONE',  ( 66.11687220234264828, 68.50194426514640611, -2.649008205479342237 ) ) ;
#73863 = CARTESIAN_POINT ( 'NONE',  ( 152.1671311979278016, 269.0857928536317445, 15.36489295260887822 ) ) ;
#73864 = CARTESIAN_POINT ( 'NONE',  ( 81.88814419999580707, 58.88989235143515799, 0.4045084971874752799 ) ) ;
#73865 = CARTESIAN_POINT ( 'NONE',  ( 164.2436631241379246, 246.1686259782033517, 4.255161687766976009 ) ) ;
#73866 = CARTESIAN_POINT ( 'NONE',  ( 167.4183826251619678, 266.1184513312476270, 16.55919039627169909 ) ) ;
#73867 = CARTESIAN_POINT ( 'NONE',  ( 181.1523296486749643, 256.9212113246534273, 4.964240719889960296 ) ) ;
#73868 = CARTESIAN_POINT ( 'NONE',  ( 97.41363812451689341, 236.2369531367911009, -4.594050593750048428 ) ) ;
#73869 = EDGE_LOOP ( 'NONE', ( #84702, #39444, #62892, #72528 ) ) ;
#73870 = CARTESIAN_POINT ( 'NONE',  ( 73.97539535980833136, 55.64209510402770320, -16.58538844966203385 ) ) ;
#73871 = CARTESIAN_POINT ( 'NONE',  ( 163.5882744166410703, 276.6356449797434038, -13.72909506296926629 ) ) ;
#73872 = ORIENTED_EDGE ( 'NONE', *, *, #8000, .F. ) ;
#73873 = ORIENTED_EDGE ( 'NONE', *, *, #92441, .T. ) ;
#73874 = EDGE_CURVE ( 'NONE', #51421, #28368, #24144, .T. ) ;
#73875 = CARTESIAN_POINT ( 'NONE',  ( 86.92624412656546440, 45.88388850009498299, -8.154586621708650895 ) ) ;
#73876 = EDGE_CURVE ( 'NONE', #22609, #27174, #69735, .T. ) ;
#73877 = CARTESIAN_POINT ( 'NONE',  ( 180.6484119781345328, 294.0070947715454395, -2.628133096437607730 ) ) ;
#73878 = CARTESIAN_POINT ( 'NONE',  ( 157.6673516573649181, 257.5591315650518141, 16.79781451397666103 ) ) ;
#73879 = CARTESIAN_POINT ( 'NONE',  ( 206.7923762329701276, 272.4720930770340033, -9.496103119940368487 ) ) ;
#73880 = CARTESIAN_POINT ( 'NONE',  ( 207.1661313457130404, 271.3965419664068577, -4.352715553263532655 ) ) ;
#73881 = CARTESIAN_POINT ( 'NONE',  ( 83.63833477162944519, 231.3464784336661637, 1.353441290958777327E-15 ) ) ;
#73882 = ORIENTED_EDGE ( 'NONE', *, *, #10017, .F. ) ;
#73883 = EDGE_CURVE ( 'NONE', #6477, #98545, #93577, .T. ) ;
#73884 = VERTEX_POINT ( 'NONE', #79392 ) ;
#73885 = CARTESIAN_POINT ( 'NONE',  ( 163.3409975114459485, 247.7320886816312111, -10.96358124877083640 ) ) ;
#73886 = ORIENTED_EDGE ( 'NONE', *, *, #16914, .F. ) ;
#73887 = EDGE_CURVE ( 'NONE', #42808, #59347, #78360, .T. ) ;
#73888 = EDGE_CURVE ( 'NONE', #26545, #5700, #11352, .T. ) ;
#73889 = CARTESIAN_POINT ( 'NONE',  ( 191.3867969386575680, 263.7415086189949989, -8.063185982860206380 ) ) ;
#73890 = CARTESIAN_POINT ( 'NONE',  ( 30.01653393904200584, 17.73415679381823296, -6.890680421881970419E-14 ) ) ;
#73891 = AXIS2_PLACEMENT_3D ( 'NONE', #90727, #85103, #21284 ) ;
#73892 = CARTESIAN_POINT ( 'NONE',  ( 191.4738032422262677, 260.7793432447242594, -0.2951778641931921410 ) ) ;
#73894 = CARTESIAN_POINT ( 'NONE',  ( 69.61542750543651437, 62.56132062526208415, -13.94275833713536628 ) ) ;
#73893 = CARTESIAN_POINT ( 'NONE',  ( 137.8467198073504107, 241.2048013555409796, 4.594050593750051981 ) ) ;
#73895 = CARTESIAN_POINT ( 'NONE',  ( 177.6444986370304946, 293.6980009803469329, 2.770296639708824227 ) ) ;
#73896 = ORIENTED_EDGE ( 'NONE', *, *, #21394, .T. ) ;
#73898 = CARTESIAN_POINT ( 'NONE',  ( 157.4725523017146429, 257.8965339463198916, 17.43710027717953892 ) ) ;
#73897 = VECTOR ( 'NONE', #23123, 1000.000000000000000 ) ;
#73899 = ADVANCED_FACE ( 'NONE', ( #3371 ), #12454, .T. ) ;
#73900 = CARTESIAN_POINT ( 'NONE',  ( 52.92184332868904306, 211.3615022471903160, 5.000000000000046185 ) ) ;
#73901 = CARTESIAN_POINT ( 'NONE',  ( 81.98093041017179416, 40.98279097121832137, -3.023795677445690000 ) ) ;
#73902 = EDGE_CURVE ( 'NONE', #43596, #67223, #43325, .T. ) ;
#73903 = CARTESIAN_POINT ( 'NONE',  ( 190.7986890213734625, 271.0762054634549258, 14.19875726436414176 ) ) ;
#73904 = CARTESIAN_POINT ( 'NONE',  ( 114.2732676653602510, 248.3297689869269220, -2.679491924311252493 ) ) ;
#73905 = AXIS2_PLACEMENT_3D ( 'NONE', #65155, #18072, #56034 ) ;
#73906 = DIRECTION ( 'NONE',  ( 0.000000000000000000, 0.000000000000000000, 1.000000000000000000 ) ) ;
#73907 = DIRECTION ( 'NONE',  ( -0.000000000000000000, -0.000000000000000000, -1.000000000000000000 ) ) ;
#73908 = DIRECTION ( 'NONE',  ( -0.8660254037844387076, -0.4999999999999998890, -0.000000000000000000 ) ) ;
#73909 = CARTESIAN_POINT ( 'NONE',  ( 161.5431944097339851, 250.8459749958011287, 14.52339846942414603 ) ) ;
#73910 = CARTESIAN_POINT ( 'NONE',  ( 67.18400125431875836, 69.34949600813865800, -0.8641136148527382987 ) ) ;
#73911 = CARTESIAN_POINT ( 'NONE',  ( 206.6912923161529818, 272.6471755567893638, -9.325620632947922317 ) ) ;
#73912 = LINE ( 'NONE', #91134, #15919 ) ;
#73913 = CARTESIAN_POINT ( 'NONE',  ( 207.7625791259561652, 270.7916523727319031, -1.015623356719550063 ) ) ;
#73914 = CARTESIAN_POINT ( 'NONE',  ( 168.4809247738020019, 252.9187805847961670, 12.05003015331094041 ) ) ;
#73915 = AXIS2_PLACEMENT_3D ( 'NONE', #33006, #94845, #63907 ) ;
#73917 = CARTESIAN_POINT ( 'NONE',  ( 182.9064100835608144, 264.9912211263795143, 13.33838763049125831 ) ) ;
#73916 = CARTESIAN_POINT ( 'NONE',  ( 73.68541970440786315, 69.64416370799906986, -9.598864117728750145 ) ) ;
#73918 = CARTESIAN_POINT ( 'NONE',  ( 77.51335635343683350, 208.8927522451418213, 10.00000000000009948 ) ) ;
#73919 = CARTESIAN_POINT ( 'NONE',  ( 41.56734871454121816, 26.12755873383629535, -6.180339887498949025 ) ) ;
#73920 = CARTESIAN_POINT ( 'NONE',  ( -50.36082798260552806, 30.16005589317048674, 10.00000000000000000 ) ) ;
#73922 = LINE ( 'NONE', #48632, #66311 ) ;
#73921 = B_SPLINE_CURVE_WITH_KNOTS ( 'NONE', 3,
 ( #61627, #24634, #38826, #78358, #63638, #69234, #16038, #70738, #1349, #31715 ),
 .UNSPECIFIED., .F., .F.,
 ( 4, 2, 2, 2, 4 ),
 ( 0.000000000000000000, 0.2500000000000000000, 0.5000000000000000000, 0.7500000000000000000, 1.000000000000000000 ),
 .UNSPECIFIED. ) ;
#73923 = VECTOR ( 'NONE', #77201, 1000.000000000000114 ) ;
#73924 = CARTESIAN_POINT ( 'NONE',  ( 81.99434118348091260, 43.19859484614419642, -8.157555647291429679 ) ) ;
#73925 = CARTESIAN_POINT ( 'NONE',  ( 24.91150772114469092, 179.0643266524160140, 9.188101187500095079 ) ) ;
#73926 = LINE ( 'NONE', #19253, #46827 ) ;
#73927 = VERTEX_POINT ( 'NONE', #27154 ) ;
#73928 = CARTESIAN_POINT ( 'NONE',  ( 86.95101435003084589, 46.48366829287757440, 8.967845595998873875 ) ) ;
#73929 = CARTESIAN_POINT ( 'NONE',  ( 182.9770351804424706, 269.0381230690315988, 16.62995593613592504 ) ) ;
#73930 = CARTESIAN_POINT ( 'NONE',  ( 71.81881128194709163, 72.53313204687133009, -1.300380427722385823 ) ) ;
#73931 = CARTESIAN_POINT ( 'NONE',  ( 36.54820344085055694, 204.1589784336661637, -6.496448406907676862E-16 ) ) ;
#73932 = EDGE_CURVE ( 'NONE', #99285, #79909, #89496, .T. ) ;
#73933 = CARTESIAN_POINT ( 'NONE',  ( 161.8016137473484548, 250.3983795733946636, 14.25000412375400316 ) ) ;
#73934 = CARTESIAN_POINT ( 'NONE',  ( 174.6026413853588508, 289.1850952631716041, 7.771083852652256319 ) ) ;
#73935 = CARTESIAN_POINT ( 'NONE',  ( 147.3023124603499809, 275.5119060767245287, 5.196938859334171212 ) ) ;
#73936 = CARTESIAN_POINT ( 'NONE',  ( 4.836955906052805787, 24.83396525600387861, -2.839279412974133887 ) ) ;
#73937 = CARTESIAN_POINT ( 'NONE',  ( 202.9409128566982758, 270.0839114184054779, -6.625179921953246343 ) ) ;
#73938 = CARTESIAN_POINT ( 'NONE',  ( 146.9235493515124062, 276.1679430252639804, 0.7994986043261682607 ) ) ;
#73939 = LINE ( 'NONE', #27831, #55398 ) ;
#73940 = CARTESIAN_POINT ( 'NONE',  ( 82.86586985908988368, 152.2544130683315871, 0.000000000000000000 ) ) ;
#73941 = CARTESIAN_POINT ( 'NONE',  ( 166.9032805970908839, 257.6634323422801458, -15.74477645480126142 ) ) ;
#73942 = EDGE_CURVE ( 'NONE', #59818, #50345, #4327, .T. ) ;
#73943 = CARTESIAN_POINT ( 'NONE',  ( -8.669243101527598583, 25.19333184544593252, -10.00000000000000000 ) ) ;
#73944 = CARTESIAN_POINT ( 'NONE',  ( 81.95417956210631871, 41.06112128662814342, 3.409771386804488102 ) ) ;
#73945 = CARTESIAN_POINT ( 'NONE',  ( 87.66109131259325693, 45.42289479680125908, -6.627856213955100273 ) ) ;
#73946 = CARTESIAN_POINT ( 'NONE',  ( 100.6254093204819497, 222.2365022471902023, -10.00000000000009059 ) ) ;
#73947 = FACE_OUTER_BOUND ( 'NONE', #24377, .T. ) ;
#73948 = CARTESIAN_POINT ( 'NONE',  ( 161.9624950439807094, 268.0139618835574424, -17.50977960935507127 ) ) ;
#73949 = VERTEX_POINT ( 'NONE', #26151 ) ;
#73950 = CARTESIAN_POINT ( 'NONE',  ( 63.01627839189497138, 213.3149278399160949, 9.188101187500093303 ) ) ;
#73951 = ORIENTED_EDGE ( 'NONE', *, *, #8927, .T. ) ;
#73952 = CARTESIAN_POINT ( 'NONE',  ( 162.6241144845578503, 263.2905756906662305, 17.26806262333970565 ) ) ;
#73953 = CARTESIAN_POINT ( 'NONE',  ( 190.9335643195044838, 299.9403610588350944, -4.692880224846124548 ) ) ;
#73954 = EDGE_CURVE ( 'NONE', #17465, #44815, #10961, .T. ) ;
#73955 = CARTESIAN_POINT ( 'NONE',  ( 67.33238274588912020, 67.23450051695161278, -8.593907957288223542 ) ) ;
#73956 = ORIENTED_EDGE ( 'NONE', *, *, #56591, .T. ) ;
#73957 = CARTESIAN_POINT ( 'NONE',  ( 171.3677841791904086, 286.5144775268977924, 7.813166782325457582 ) ) ;
#73958 = CARTESIAN_POINT ( 'NONE',  ( 207.6727254509676186, 270.9472835030587703, 7.315149605389819953 ) ) ;
#73959 = DIRECTION ( 'NONE',  ( 0.000000000000000000, 0.000000000000000000, 1.000000000000000000 ) ) ;
#73960 = CARTESIAN_POINT ( 'NONE',  ( 35.07444006175263240, 22.11110640527294535, -2.839279412974138328 ) ) ;
#73961 = CARTESIAN_POINT ( 'NONE',  ( 188.9599767341003940, 265.5171183316097654, 10.73179992602947941 ) ) ;
#73962 = CARTESIAN_POINT ( 'NONE',  ( 149.1429535397850827, 272.3238222086447990, -12.91457852089092384 ) ) ;
#73963 = VECTOR ( 'NONE', #15305, 1000.000000000000114 ) ;
#73964 = CARTESIAN_POINT ( 'NONE',  ( -66.69146994933839778, 41.22495595238228105, -10.00000000000000000 ) ) ;
#73965 = EDGE_LOOP ( 'NONE', ( #24981, #76028, #6917, #7031 ) ) ;
#73966 = VECTOR ( 'NONE', #79467, 1000.000000000000114 ) ;
#73967 = CARTESIAN_POINT ( 'NONE',  ( 9.333682440526761326, 28.49540643055185996, 3.479690158560446702E-15 ) ) ;
#73968 = CARTESIAN_POINT ( 'NONE',  ( 21.97483017187327192, 36.18528772668518911, -1.583844403245363575 ) ) ;
#73969 = CARTESIAN_POINT ( 'NONE',  ( -24.92236680055716036, 162.1916292661125283, 5.188172501216621122E-14 ) ) ;
#73970 = DIRECTION ( 'NONE',  ( -0.6141984594095519778, -0.7891516029629116469, 0.000000000000000000 ) ) ;
#73971 = EDGE_CURVE ( 'NONE', #77610, #73457, #73255, .T. ) ;
#73972 = ORIENTED_EDGE ( 'NONE', *, *, #161, .F. ) ;
#73973 = CARTESIAN_POINT ( 'NONE',  ( 77.72205534048291042, 61.52847525230063042, 16.09962475150207339 ) ) ;
#73974 = CARTESIAN_POINT ( 'NONE',  ( 191.5281967176683509, 298.9104275333885994, 7.715154960566919407 ) ) ;
#73975 = EDGE_CURVE ( 'NONE', #24993, #77732, #46660, .T. ) ;
#73976 = FACE_OUTER_BOUND ( 'NONE', #98042, .T. ) ;
#73977 = ORIENTED_EDGE ( 'NONE', *, *, #69517, .F. ) ;
#73978 = ORIENTED_EDGE ( 'NONE', *, *, #48031, .T. ) ;
#73979 = AXIS2_PLACEMENT_3D ( 'NONE', #83750, #71526, #56289 ) ;
#73981 = CARTESIAN_POINT ( 'NONE',  ( -19.65312891409030271, 93.06504152958497400, -20.00000000000000355 ) ) ;
#73980 = CARTESIAN_POINT ( 'NONE',  ( 161.4143265314674522, 251.0691807084224365, -12.94469757303959234 ) ) ;
#73982 = CARTESIAN_POINT ( 'NONE',  ( 149.1486417047969155, 272.3139700178423368, -11.47583619705022606 ) ) ;
#73983 = VERTEX_POINT ( 'NONE', #80902 ) ;
#73984 = CARTESIAN_POINT ( 'NONE',  ( 66.13947098823611270, 69.16665220597090524, -2.048021925782174346 ) ) ;
#73985 = CARTESIAN_POINT ( 'NONE',  ( -167.0327448629461742, 42.61639673982678289, -30.52142883766498116 ) ) ;
#73986 = CARTESIAN_POINT ( 'NONE',  ( -19.65312891409030271, 93.06504152958497400, 177.5919119679930134 ) ) ;
#73987 = CARTESIAN_POINT ( 'NONE',  ( 78.04817985968655591, 62.07294584189650521, -16.01854286150912898 ) ) ;
#73988 = CARTESIAN_POINT ( 'NONE',  ( 72.10919973083444745, 72.28739807568710773, -1.448965806592429795 ) ) ;
#73989 = CARTESIAN_POINT ( 'NONE',  ( 115.5733686319456126, 237.5333772461660544, 9.188101187500095079 ) ) ;
#73990 = CARTESIAN_POINT ( 'NONE',  ( 42.76202708541288899, 64.24573752441608576, -10.00000000000000000 ) ) ;
#73991 = CARTESIAN_POINT ( 'NONE',  ( 205.4317452772315278, 270.7218421723977144, 7.456875539217049820 ) ) ;
#73992 = CARTESIAN_POINT ( 'NONE',  ( 76.56683408466376761, 148.6176630683316091, 8.907468493598274475E-16 ) ) ;
#73993 = EDGE_LOOP ( 'NONE', ( #92788, #1955, #76727, #11447 ) ) ;
#73994 = AXIS2_PLACEMENT_3D ( 'NONE', #67516, #37113, #68016 ) ;
#73995 = CARTESIAN_POINT ( 'NONE',  ( 207.8725590214046406, 270.6011616060040410, 1.988011721677743093 ) ) ;
#73996 = ORIENTED_EDGE ( 'NONE', *, *, #98725, .F. ) ;
#73997 = CARTESIAN_POINT ( 'NONE',  ( 26.65419051621551461, 38.49540643055190259, 3.479690158560446702E-15 ) ) ;
#73998 = ADVANCED_FACE ( 'NONE', ( #42327 ), #25656, .F. ) ;
#73999 = FACE_BOUND ( 'NONE', #50676, .T. ) ;
#74000 = CARTESIAN_POINT ( 'NONE',  ( 75.21170341390104852, 66.97160359861173617, -12.78114342037769013 ) ) ;
#74001 = CARTESIAN_POINT ( 'NONE',  ( 71.40607303893924040, 212.0333772461660544, 9.188101187500095079 ) ) ;
#74002 = CARTESIAN_POINT ( 'NONE',  ( 177.8222571804544430, 286.5223583772871621, 13.77940225188420875 ) ) ;
#74003 = CARTESIAN_POINT ( 'NONE',  ( 81.62315923969183018, 55.76054528319124159, 16.35706999678057727 ) ) ;
#74004 = CARTESIAN_POINT ( 'NONE',  ( 198.5328126748496516, 286.7780768080430676, 18.48542741931266775 ) ) ;
#74005 = CARTESIAN_POINT ( 'NONE',  ( 174.7265224105599657, 278.0225128774238215, 15.48253028248275065 ) ) ;
#74006 = B_SPLINE_CURVE_WITH_KNOTS ( 'NONE', 3,
 ( #88021, #52932, #28640, #69127, #30133, #100053, #21550, #6834, #6348, #23018, #76262, #60025, #45329, #90989, #83885, #44330, #60516, #44828, #68629, #7329, #30641, #13464, #91988, #37719, #37235, #68133, #5847, #52432, #61528, #83379, #67638, #36732, #29643, #99550, #75262, #13945, #53425, #82411, #98571, #99061, #14447, #90501, #61016, #22540, #84375, #5354, #29154, #12976 ),
 .UNSPECIFIED., .F., .F.,
 ( 4, 2, 2, 2, 2, 2, 2, 2, 2, 2, 2, 2, 2, 2, 2, 2, 2, 2, 2, 2, 2, 2, 2, 4 ),
 ( 0.0003007692019500355176, 0.001319192577369706146, 0.001828404265079501372, 0.002083010108934399418, 0.002210313030861848008, 0.002337615952789296597, 0.002592221796644032447, 0.002846827640498767863, 0.003356039328208184486, 0.004374462703627130487, 0.005392886079046075622, 0.005902097766755467524, 0.006156703610610120107, 0.006411309454464772691, 0.006474960915428472699, 0.006538612376392171840, 0.006602263837355871849, 0.006665915298319570990, 0.006920521142174513272, 0.007429732829884467225, 0.007684338673739515325, 0.007938944517594562558, 0.008193550361449610658, 0.008448156205304658758 ),
 .UNSPECIFIED. ) ;
#74007 = ORIENTED_EDGE ( 'NONE', *, *, #87198, .F. ) ;
#74008 = EDGE_CURVE ( 'NONE', #76358, #16775, #96089, .T. ) ;
#74009 = CARTESIAN_POINT ( 'NONE',  ( 112.8118497929261252, 247.4860189848785126, -2.679491924311252493 ) ) ;
#74010 = CARTESIAN_POINT ( 'NONE',  ( 203.3349860717029571, 278.4604684979374838, -16.59553970625579566 ) ) ;
#74011 = ORIENTED_EDGE ( 'NONE', *, *, #62187, .F. ) ;
#74012 = CARTESIAN_POINT ( 'NONE',  ( 195.4137072836104494, 292.1805258198313027, 15.38860452967709413 ) ) ;
#74013 = CARTESIAN_POINT ( 'NONE',  ( -16.52256874082355864, 171.2677522451419350, -5.000000000000047962 ) ) ;
#74014 = CARTESIAN_POINT ( 'NONE',  ( 161.8408514536557163, 250.3304178724980318, -14.12919723462510646 ) ) ;
#74015 = CARTESIAN_POINT ( 'NONE',  ( 192.4663556654298588, 297.2854885702906245, -12.98646995774174684 ) ) ;
#74016 = EDGE_CURVE ( 'NONE', #2736, #17295, #40445, .T. ) ;
#74018 = CARTESIAN_POINT ( 'NONE',  ( 199.8798371376168745, 283.2826252849788489, -17.21687883691964771 ) ) ;
#74017 = B_SPLINE_CURVE_WITH_KNOTS ( 'NONE', 3,
 ( #87776, #49212, #80144, #18808 ),
 .UNSPECIFIED., .F., .F.,
 ( 4, 4 ),
 ( 0.04143897040461883702, 0.04887120950165265570 ),
 .UNSPECIFIED. ) ;
#74019 = FACE_OUTER_BOUND ( 'NONE', #70048, .T. ) ;
#74020 = DIRECTION ( 'NONE',  ( 0.6355427771210591104, 0.000000000000000000, 0.7720656568254100627 ) ) ;
#74021 = CARTESIAN_POINT ( 'NONE',  ( 208.2764314485352770, 269.9016340424377063, 2.433736665191914117 ) ) ;
#74022 = ADVANCED_FACE ( 'NONE', ( #34733 ), #58523, .F. ) ;
#74023 = CARTESIAN_POINT ( 'NONE',  ( 118.5230073417626073, 248.4244531367911293, -4.594050593750046652 ) ) ;
#74024 = VERTEX_POINT ( 'NONE', #64142 ) ;
#74025 = CARTESIAN_POINT ( 'NONE',  ( 85.24313230617720194, 44.17383514321656435, -6.788908311595864831 ) ) ;
#74026 = CARTESIAN_POINT ( 'NONE',  ( 37.34220537994157496, 54.61056725541210710, 10.00000000000000000 ) ) ;
#74027 = CARTESIAN_POINT ( 'NONE',  ( 205.8688675895746201, 273.6846427845131871, -9.898080752049997599 ) ) ;
#74028 = CARTESIAN_POINT ( 'NONE',  ( 164.4294002498235159, 245.8469198396639399, 6.098783631055905374 ) ) ;
#74029 = CARTESIAN_POINT ( 'NONE',  ( 74.74991615466120720, 60.94473038293241274, 15.38198754237874688 ) ) ;
#74030 = PLANE ( 'NONE',  #68023 ) ;
#74031 = EDGE_LOOP ( 'NONE', ( #15485, #43820, #47574, #82157, #60599, #80887, #7588, #28728, #34719, #87400, #90857, #74204, #6282, #15118, #67614, #77216, #84085, #48892, #50421, #12547 ) ) ;
#74032 = CARTESIAN_POINT ( 'NONE',  ( 76.94944781827869917, 56.99682769027370455, 16.18096124992289120 ) ) ;
#74033 = CARTESIAN_POINT ( 'NONE',  ( 119.0104069514411123, 249.5177522451419065, 5.000000000000046185 ) ) ;
#74034 = CARTESIAN_POINT ( 'NONE',  ( 164.7026013006809251, 246.9704538741483759, -5.638495517494114928 ) ) ;
#74035 = CARTESIAN_POINT ( 'NONE',  ( 147.8331127587908043, 276.3582630845543804, 2.721914673797492412 ) ) ;
#74036 = CARTESIAN_POINT ( 'NONE',  ( 29.67341102961999155, 199.4860189848785410, -2.679491924311252493 ) ) ;
#74037 = CARTESIAN_POINT ( 'NONE',  ( 198.5699292022329416, 266.2780175646987573, 0.8405458176556424021 ) ) ;
#74038 = CARTESIAN_POINT ( 'NONE',  ( 147.0670278774466908, 275.9194309285509235, 3.666898409139099257 ) ) ;
#74039 = DIRECTION ( 'NONE',  ( -0.000000000000000000, -0.000000000000000000, -1.000000000000000000 ) ) ;
#74040 = AXIS2_PLACEMENT_3D ( 'NONE', #30907, #69898, #512 ) ;
#74041 = AXIS2_PLACEMENT_3D ( 'NONE', #89695, #20254, #20758 ) ;
#74042 = CARTESIAN_POINT ( 'NONE',  ( 172.8463378600133353, 251.6495383470449099, 3.423699583515463996 ) ) ;
#74043 = B_SPLINE_SURFACE_WITH_KNOTS ( 'NONE', 3, 1, ( 
 ( #75396, #45463 ),
 ( #53563, #30781 ),
 ( #68765, #84516 ),
 ( #36875, #6972 ),
 ( #83519, #99689 ),
 ( #52076, #99192 ),
 ( #7465, #15059 ),
 ( #21684, #100196 ),
 ( #92131, #29777 ),
 ( #44967, #37364 ),
 ( #60650, #92612 ),
 ( #6486, #76867 ),
 ( #75906, #23158 ),
 ( #38357, #90634 ),
 ( #98706, #69267 ),
 ( #38861, #53071 ),
 ( #77383, #54049 ),
 ( #91606, #85007 ),
 ( #21197, #15551 ),
 ( #46452, #22178 ),
 ( #7985, #69767 ),
 ( #375, #83020 ),
 ( #60155, #1884 ),
 ( #870, #1387 ),
 ( #2392, #16569 ),
 ( #46972, #93606 ),
 ( #85527, #17573 ),
 ( #47955, #40849 ),
 ( #31749, #77891 ),
 ( #71794, #63671 ),
 ( #16070, #78898 ),
 ( #33272, #62654 ),
 ( #93096, #94610 ),
 ( #8971, #64175 ) ),
 .UNSPECIFIED., .T., .F., .F.,
 ( 4, 2, 2, 2, 2, 2, 2, 2, 2, 2, 2, 2, 2, 2, 2, 2, 4 ),
 ( 2, 2 ),
 ( 0.000000000000000000, 0.06250000000000000000, 0.1250000000000000000, 0.1875000000000000000, 0.2500000000000000000, 0.3125000000000000000, 0.3750000000000000000, 0.4375000000000000000, 0.5000000000000000000, 0.5625000000000000000, 0.6250000000000000000, 0.6875000000000000000, 0.7500000000000000000, 0.8125000000000000000, 0.8750000000000000000, 0.9375000000000000000, 1.000000000000000000 ),
 ( 0.000000000000000000, 1.000000000000000000 ),
 .UNSPECIFIED. ) ;
#74044 = CARTESIAN_POINT ( 'NONE',  ( 18.71539827744147999, 26.50829794293879615, -10.00000000000000355 ) ) ;
#74045 = CARTESIAN_POINT ( 'NONE',  ( 149.5633513747893346, 271.5956717990251832, 12.83777201928511325 ) ) ;
#74046 = FACE_OUTER_BOUND ( 'NONE', #60207, .T. ) ;
#74047 = LINE ( 'NONE', #35529, #4646 ) ;
#74048 = CARTESIAN_POINT ( 'NONE',  ( 159.3528137482544196, 254.6398255893999476, 16.73628156321660398 ) ) ;
#74049 = CARTESIAN_POINT ( 'NONE',  ( 189.9879251633717558, 299.5782561228834879, -6.671532329245590809 ) ) ;
#74050 = AXIS2_PLACEMENT_3D ( 'NONE', #7485, #38377, #15573 ) ;
#74051 = CARTESIAN_POINT ( 'NONE',  ( 132.0729567918564555, 240.3927522451418213, 10.00000000000009592 ) ) ;
#74052 = CARTESIAN_POINT ( 'NONE',  ( 183.3367312544899619, 279.0378104038655351, 17.10307584900649402 ) ) ;
#74053 = ORIENTED_EDGE ( 'NONE', *, *, #18748, .F. ) ;
#74054 = VECTOR ( 'NONE', #44428, 1000.000000000000227 ) ;
#74055 = CARTESIAN_POINT ( 'NONE',  ( 157.3025066944120454, 258.1910615777721887, 18.21299529665260053 ) ) ;
#74056 = CARTESIAN_POINT ( 'NONE',  ( 199.0756812798354645, 285.8378008023734083, -18.45377816087746936 ) ) ;
#74057 = CARTESIAN_POINT ( 'NONE',  ( -11.27255005043015856, 173.4869531367911293, 4.594050593750046652 ) ) ;
#74058 = CARTESIAN_POINT ( 'NONE',  ( 50.89226983467786170, 194.0643266524160424, 9.188101187500095079 ) ) ;
#74059 = CARTESIAN_POINT ( 'NONE',  ( 178.6236953501245353, 259.1675616789437981, -10.33478249233844259 ) ) ;
#74060 = CARTESIAN_POINT ( 'NONE',  ( 17.15438521794160920, 32.83705186507754092, 3.090169943749475401 ) ) ;
#74061 = CARTESIAN_POINT ( 'NONE',  ( 85.48911027617603509, 49.06452166842702667, 12.33247222509585228 ) ) ;
#74062 = AXIS2_PLACEMENT_3D ( 'NONE', #64275, #25792, #56668 ) ;
#74063 = CARTESIAN_POINT ( 'NONE',  ( 204.9658583905037688, 275.6357147811169170, -12.57240504404813564 ) ) ;
#74064 = FACE_OUTER_BOUND ( 'NONE', #99533, .T. ) ;
#74065 = CARTESIAN_POINT ( 'NONE',  ( 73.75633218949143100, 55.22183339029175642, -16.59646955798544354 ) ) ;
#74067 = CARTESIAN_POINT ( 'NONE',  ( 71.81202244518924260, 212.2677522451418497, 10.00000000000009592 ) ) ;
#74066 = CARTESIAN_POINT ( 'NONE',  ( 171.2891392173955012, 258.0937863124287333, 14.46422458907198383 ) ) ;
#74068 = CARTESIAN_POINT ( 'NONE',  ( 76.86551199909389709, 60.02806529646827016, 16.29612583600000875 ) ) ;
#74069 = CARTESIAN_POINT ( 'NONE',  ( 36.10619739613039059, 52.83927550304669296, -10.00000000000000000 ) ) ;
#74070 = CARTESIAN_POINT ( 'NONE',  ( 150.6881537519499830, 269.6474569333088311, 15.31267828461696467 ) ) ;
#74071 = CARTESIAN_POINT ( 'NONE',  ( 36.90037335867696555, 192.1115022471902591, 10.00000000000009592 ) ) ;
#74072 = CARTESIAN_POINT ( 'NONE',  ( 181.7591720214631721, 291.6897925616224256, 9.200304531648196615 ) ) ;
#74073 = AXIS2_PLACEMENT_3D ( 'NONE', #36777, #84911, #28683 ) ;
#74074 = CARTESIAN_POINT ( 'NONE',  ( 33.92732256784238132, 47.61654385008751689, 10.00000000000000000 ) ) ;
#74075 = CARTESIAN_POINT ( 'NONE',  ( -2.422939729449181012, 181.6589784336661637, -6.496448406907675876E-16 ) ) ;
#74076 = CARTESIAN_POINT ( 'NONE',  ( 167.6502826215564994, 287.3877002845107995, 4.891367078714356609 ) ) ;
#74077 = CARTESIAN_POINT ( 'NONE',  ( 152.7314557461996571, 266.1083540640618708, 17.39314074348802208 ) ) ;
#74078 = CARTESIAN_POINT ( 'NONE',  ( 31.70236382085744609, 33.70171378149921537, -9.188101187500004485 ) ) ;
#74079 = B_SPLINE_CURVE_WITH_KNOTS ( 'NONE', 3,
 ( #47200, #15798, #85253, #53787, #69997, #47692, #23899, #63906, #46704, #77630, #612, #78124, #70502, #8214, #39084, #61891, #94349, #40592, #31494, #78627, #38600, #62386, #55287, #71031, #7707, #46185, #48210, #1633, #33005, #93343, #2123, #22901, #84748, #15288, #8712, #1117, #77104, #32517, #79156, #63410, #39581, #24903, #93856, #31994, #69504, #54801 ),
 .UNSPECIFIED., .F., .F.,
 ( 4, 1, 1, 1, 2, 2, 1, 1, 1, 2, 2, 1, 1, 2, 2, 1, 1, 2, 2, 1, 1, 2, 2, 1, 2, 2, 1, 2, 2, 4 ),
 ( 0.000000000000000000, 0.06249999999998294420, 0.09374999999997277178, 0.1093749999999694966, 0.1171874999999694411, 0.1249999999999693578, 0.1874999999999802103, 0.2187499999999858724, 0.2343749999999902023, 0.2421874999999925893, 0.2499999999999950040, 0.3125000000000006106, 0.3437500000000021094, 0.3593750000000013878, 0.3750000000000006661, 0.4374999999999905631, 0.4687499999999855671, 0.4843749999999844014, 0.4999999999999832356, 0.5624999999999895639, 0.5937499999999904521, 0.6093749999999907851, 0.6249999999999912292, 0.6874999999999906741, 0.7187499999999904521, 0.7499999999999902300, 0.8124999999999934497, 0.8437499999999931166, 0.8749999999999927836, 1.000000000000000000 ),
 .UNSPECIFIED. ) ;
#74080 = CARTESIAN_POINT ( 'NONE',  ( 27.68909066282341058, 16.39040679176984128, 1.333680081654574804E-15 ) ) ;
#74081 = EDGE_CURVE ( 'NONE', #25798, #65437, #56536, .T. ) ;
#74082 = CARTESIAN_POINT ( 'NONE',  ( 207.4285356523023154, 271.3702326410368642, 7.833982582429932506 ) ) ;
#74083 = CARTESIAN_POINT ( 'NONE',  ( 155.0303156110108489, 262.1266119787277944, 17.11986653161320859 ) ) ;
#74084 = CARTESIAN_POINT ( 'NONE',  ( 125.6883311748214425, 231.8262482093457493, 3.021315404115420679E-15 ) ) ;
#74085 = CARTESIAN_POINT ( 'NONE',  ( 176.4522659647303442, 260.3536617702438889, -13.41910003846964550 ) ) ;
#74086 = CARTESIAN_POINT ( 'NONE',  ( 15.18774714507562962, 26.95586893147754992, 7.433330006724141015 ) ) ;
#74087 = CARTESIAN_POINT ( 'NONE',  ( 82.20091667785729328, 54.22338727706198114, 15.63590626746406009 ) ) ;
#74088 = CARTESIAN_POINT ( 'NONE',  ( 159.5744557550824823, 258.7184754996998777, 17.16512081183459415 ) ) ;
#74089 = CARTESIAN_POINT ( 'NONE',  ( 194.6820509838467785, 270.8910309865917156, -14.27696746312268239 ) ) ;
#74090 = ORIENTED_EDGE ( 'NONE', *, *, #5255, .T. ) ;
#74091 = CARTESIAN_POINT ( 'NONE',  ( 156.8023757504856803, 276.4965331495019427, 10.27696673126826532 ) ) ;
#74092 = CARTESIAN_POINT ( 'NONE',  ( 75.02147862394267008, 53.42613012923004590, -16.05124535999422974 ) ) ;
#74093 = CARTESIAN_POINT ( 'NONE',  ( 81.36599162659588558, 42.15504690410337929, 8.050126262897936869 ) ) ;
#74094 = EDGE_CURVE ( 'NONE', #65992, #70878, #33972, .T. ) ;
#74095 = EDGE_LOOP ( 'NONE', ( #84964, #24327, #19275, #17632 ) ) ;
#74096 = CARTESIAN_POINT ( 'NONE',  ( 153.3920560952016956, 264.9641606960921649, 16.50453917291963535 ) ) ;
#74097 = CARTESIAN_POINT ( 'NONE',  ( 81.52103558181507026, 206.3262482093457493, 3.021315404115420679E-15 ) ) ;
#74098 = CARTESIAN_POINT ( 'NONE',  ( 66.49005502223729991, 68.69345493094031951, 4.810109871286462280 ) ) ;
#74099 = EDGE_CURVE ( 'NONE', #4549, #4372, #54599, .T. ) ;
#74100 = CARTESIAN_POINT ( 'NONE',  ( 117.4407359106297264, 248.6115022471903160, -5.000000000000047962 ) ) ;
#74101 = ORIENTED_EDGE ( 'NONE', *, *, #8863, .T. ) ;
#74102 = ORIENTED_EDGE ( 'NONE', *, *, #30863, .T. ) ;
#74104 = CARTESIAN_POINT ( 'NONE',  ( 163.7064929935861244, 247.0990319366274548, 6.401263337036986023 ) ) ;
#74103 = CARTESIAN_POINT ( 'NONE',  ( 164.1745675548848737, 246.6954794637676116, -4.690626445906736386 ) ) ;
#74105 = CARTESIAN_POINT ( 'NONE',  ( 192.5049767439991513, 297.2185948999652965, 12.57567268027295881 ) ) ;
#74106 = VERTEX_POINT ( 'NONE', #22021 ) ;
#74107 = CARTESIAN_POINT ( 'NONE',  ( 88.02868988710136477, 43.76708177457258842, -2.199075477856099692 ) ) ;
#74108 = AXIS2_PLACEMENT_3D ( 'NONE', #12904, #36162, #26594 ) ;
#74109 = CARTESIAN_POINT ( 'NONE',  ( 80.21108484470566680, 57.40951183915923650, -16.59077246605596301 ) ) ;
#74110 = CARTESIAN_POINT ( 'NONE',  ( 174.4548664363482260, 262.3557869890522625, 15.65842366412776165 ) ) ;
#74111 = ORIENTED_EDGE ( 'NONE', *, *, #64828, .T. ) ;
#74112 = DIRECTION ( 'NONE',  ( 0.5078630399532038098, 0.8614378286617615510, 0.000000000000000000 ) ) ;
#74113 = CARTESIAN_POINT ( 'NONE',  ( 81.49213971395570866, 49.47327963668817574, -13.93402821202839625 ) ) ;
#74114 = CARTESIAN_POINT ( 'NONE',  ( 149.4908848037268001, 271.7211875819559737, -12.92288068979413573 ) ) ;
#74115 = VECTOR ( 'NONE', #58800, 1000.000000000000000 ) ;
#74116 = CARTESIAN_POINT ( 'NONE',  ( 80.94772830529335295, 43.03073618849790449, 9.590346675963626666 ) ) ;
#74117 = VERTEX_POINT ( 'NONE', #83873 ) ;
#74118 = CARTESIAN_POINT ( 'NONE',  ( 177.1952554510797313, 269.3654139093299023, 16.08787487811796169 ) ) ;
#74119 = CARTESIAN_POINT ( 'NONE',  ( 164.2801755739368446, 246.1053845600426087, 2.518777461081745717 ) ) ;
#74120 = CIRCLE ( 'NONE', #28830, 17.82106496071138224 ) ;
#74121 = CARTESIAN_POINT ( 'NONE',  ( 150.9278749657586900, 275.9046242529769870, -8.333285154183892374 ) ) ;
#74122 = VERTEX_POINT ( 'NONE', #82878 ) ;
#74123 = CARTESIAN_POINT ( 'NONE',  ( 148.9694607950094394, 272.6243204573405592, 11.81236034532910573 ) ) ;
#74124 = CARTESIAN_POINT ( 'NONE',  ( 169.0457665943022505, 261.5072838169340343, -16.06598790874472726 ) ) ;
#74125 = VERTEX_POINT ( 'NONE', #5341 ) ;
#74126 = CARTESIAN_POINT ( 'NONE',  ( 156.7830287337671109, 266.5187050023503161, -16.25525341925989764 ) ) ;
#74127 = B_SPLINE_CURVE_WITH_KNOTS ( 'NONE', 3,
 ( #23421, #58201, #86297, #87318, #79684, #97241, #1657, #63439, #71056, #40619 ),
 .UNSPECIFIED., .F., .F.,
 ( 4, 2, 2, 2, 4 ),
 ( 0.000000000000000000, 0.0002622400424272996935, 0.0005244800848545993870, 0.0007867201272818990804, 0.001048960169709198774 ),
 .UNSPECIFIED. ) ;
#74128 = ORIENTED_EDGE ( 'NONE', *, *, #70159, .T. ) ;
#74129 = CYLINDRICAL_SURFACE ( 'NONE', #26649, 15.50000000000000000 ) ;
#74130 = ORIENTED_EDGE ( 'NONE', *, *, #70725, .F. ) ;
#74131 = AXIS2_PLACEMENT_3D ( 'NONE', #78929, #41891, #9518 ) ;
#74132 = EDGE_CURVE ( 'NONE', #52552, #87881, #17603, .T. ) ;
#74133 = CARTESIAN_POINT ( 'NONE',  ( -65.00000000000000000, 10.00000000000000000, 54.99999999999999289 ) ) ;
#74134 = CARTESIAN_POINT ( 'NONE',  ( 87.53138335513271784, 43.77696556206725376, 0.8862036439340156280 ) ) ;
#74135 = CARTESIAN_POINT ( 'NONE',  ( 191.2278159864466431, 297.4307022214792937, -10.96893880474589267 ) ) ;
#74136 = FACE_BOUND ( 'NONE', #5699, .T. ) ;
#74137 = CARTESIAN_POINT ( 'NONE',  ( -19.65312891409030271, 93.06504152958497400, -10.00000000000000888 ) ) ;
#74138 = CARTESIAN_POINT ( 'NONE',  ( 153.4389798490260262, 264.8828863703868137, 16.68923469758090761 ) ) ;
#74139 = CARTESIAN_POINT ( 'NONE',  ( 4.698709606056801213, 26.21091486745858390, -1.111400068045478839E-16 ) ) ;
#74140 = CARTESIAN_POINT ( 'NONE',  ( 196.9376666616535942, 289.5409507483896618, -17.49204032314444390 ) ) ;
#74141 = AXIS2_PLACEMENT_3D ( 'NONE', #25200, #86077, #38895 ) ;
#74142 = EDGE_LOOP ( 'NONE', ( #92075, #44643, #35222, #78467 ) ) ;
#74143 = CARTESIAN_POINT ( 'NONE',  ( 75.70440440058339959, 57.47974519366773194, -16.09699729114145939 ) ) ;
#74144 = CARTESIAN_POINT ( 'NONE',  ( 39.81344631580554250, 23.39040679176985904, -6.890680421881970419E-14 ) ) ;
#74146 = LINE ( 'NONE', #27543, #49940 ) ;
#74145 = CARTESIAN_POINT ( 'NONE',  ( 77.48815792355858889, 49.76915981755508511, -14.97591747096309689 ) ) ;
#74147 = CARTESIAN_POINT ( 'NONE',  ( -22.42236680055709641, 157.8615022471902591, 0.000000000000000000 ) ) ;
#74148 = DIRECTION ( 'NONE',  ( 0.7751245550734536804, 0.6318084552474590998, 0.000000000000000000 ) ) ;
#74149 = ORIENTED_EDGE ( 'NONE', *, *, #98412, .T. ) ;
#74150 = CARTESIAN_POINT ( 'NONE',  ( 190.3695739790057075, 300.9172209835572858, 5.653673465233093332 ) ) ;
#74151 = CARTESIAN_POINT ( 'NONE',  ( 69.33329605705168319, 62.86184331883654153, 13.67499948212078564 ) ) ;
#74152 = ADVANCED_FACE ( 'NONE', ( #44318 ), #6824, .T. ) ;
#74153 = CYLINDRICAL_SURFACE ( 'NONE', #86814, 10.00000000000010658 ) ;
#74154 = CARTESIAN_POINT ( 'NONE',  ( 19.02883662497902861, 11.39040679176981996, 1.333680081654574804E-15 ) ) ;
#74155 = CARTESIAN_POINT ( 'NONE',  ( 160.4591988848097230, 252.7235103201471702, -16.13450096157204072 ) ) ;
#74156 = CARTESIAN_POINT ( 'NONE',  ( 148.7027604483410528, 273.0862590081663939, -9.872652348069028250 ) ) ;
#74157 = ORIENTED_EDGE ( 'NONE', *, *, #97779, .F. ) ;
#74158 = CARTESIAN_POINT ( 'NONE',  ( 208.0006710756887287, 270.3792650189220126, -0.8737665032493013850 ) ) ;
#74159 = FACE_OUTER_BOUND ( 'NONE', #11175, .T. ) ;
#74160 = CIRCLE ( 'NONE', #28868, 10.00000000000001066 ) ;
#74161 = CARTESIAN_POINT ( 'NONE',  ( 49.91331508509971115, 100.8438505198844553, 10.00000000000000000 ) ) ;
#74162 = CARTESIAN_POINT ( 'NONE',  ( 207.5338226493333025, 271.1878702128032614, 6.432541580693135863 ) ) ;
#74163 = CARTESIAN_POINT ( 'NONE',  ( 26.27351996285747049, 192.6427522451419634, -10.00000000000009415 ) ) ;
#74164 = CARTESIAN_POINT ( 'NONE',  ( 101.9066655502961964, 220.4548013555409511, -4.594050593750042211 ) ) ;
#74165 = B_SPLINE_CURVE_WITH_KNOTS ( 'NONE', 3,
 ( #57190, #88170, #26315, #60050 ),
 .UNSPECIFIED., .F., .F.,
 ( 4, 4 ),
 ( 0.04063817219314667939, 0.04887120950165274591 ),
 .UNSPECIFIED. ) ;
#74166 = CARTESIAN_POINT ( 'NONE',  ( 183.0594061691496961, 295.7039273298110515, -2.683685864958768708 ) ) ;
#74167 = CARTESIAN_POINT ( 'NONE',  ( 167.2887110157984125, 281.5736242869099897, -10.92832022129961977 ) ) ;
#74168 = CARTESIAN_POINT ( 'NONE',  ( 190.1114827020009841, 297.9905665084500583, 9.484015614658840576 ) ) ;
#74169 = CARTESIAN_POINT ( 'NONE',  ( 26.37028381016232004, 40.32183835407518302, 10.00000000000000000 ) ) ;
#74170 = CARTESIAN_POINT ( 'NONE',  ( 15.22267496842377099, 179.5958772461660544, -9.188101187500095079 ) ) ;
#74171 = CARTESIAN_POINT ( 'NONE',  ( 15.59500490259069139, 53.45320653094265140, 59.99999999999999289 ) ) ;
#74172 = EDGE_LOOP ( 'NONE', ( #90342, #59150, #40906, #2971 ) ) ;
#74173 = VERTEX_POINT ( 'NONE', #98557 ) ;
#74174 = CARTESIAN_POINT ( 'NONE',  ( 74.10605571268695257, 68.62492193873490010, 11.45106078344675637 ) ) ;
#74175 = CARTESIAN_POINT ( 'NONE',  ( 74.46402575432118454, 68.25533967602589769, -11.46783318448646050 ) ) ;
#74176 =( BOUNDED_CURVE ( )  B_SPLINE_CURVE ( 2, ( #16199, #10607, #32890, #17189, #79549, #18211, #70393 ),
 .UNSPECIFIED., .F., .F. ) 
 B_SPLINE_CURVE_WITH_KNOTS ( ( 3, 2, 2, 3 ),
 ( 0.9717741935483871218, 0.9731182795698924970, 0.9758064516129032473, 0.9784858563273379772 ),
 .UNSPECIFIED. ) 
 CURVE ( )  GEOMETRIC_REPRESENTATION_ITEM ( )  RATIONAL_B_SPLINE_CURVE ( ( 0.9330127018922194093, 0.9330127018922194093, 1.000000000000000000, 0.8660254037844387076, 1.000000000000000000, 0.8664623547262191305, 0.9991289483004428540 ) ) 
 REPRESENTATION_ITEM ( '' )  );
#74177 = DIRECTION ( 'NONE',  ( 0.4999999999999992784, -0.8660254037844390407, 0.000000000000000000 ) ) ;
#74178 = CARTESIAN_POINT ( 'NONE',  ( 190.1858949294064871, 301.2353624297489887, -5.249932979468886707 ) ) ;
#74179 = CARTESIAN_POINT ( 'NONE',  ( 205.6103970483690659, 272.1329265362093111, -9.537080485986734857 ) ) ;
#74180 = ADVANCED_FACE ( 'NONE', ( #90488 ), #75735, .F. ) ;
#74181 = CARTESIAN_POINT ( 'NONE',  ( 3.893371226040319044, 25.18080186712590773, 3.090169943749475401 ) ) ;
#74182 = CARTESIAN_POINT ( 'NONE',  ( 176.1186201279473096, 285.3276135723396578, -12.10217071624021123 ) ) ;
#74183 = CARTESIAN_POINT ( 'NONE',  ( 47.28113444070024229, 72.57591296950350568, 10.00000000000000000 ) ) ;
#74184 = CARTESIAN_POINT ( 'NONE',  ( 51.92050145378936321, 200.7833772461660828, -9.188101187500095079 ) ) ;
#74185 = CARTESIAN_POINT ( 'NONE',  ( 96.42157766939699570, 233.1427522451419065, -10.00000000000009415 ) ) ;
#74186 = AXIS2_PLACEMENT_3D ( 'NONE', #23289, #29903, #8606 ) ;
#74187 = EDGE_CURVE ( 'NONE', #63013, #3586, #32621, .T. ) ;
#74188 = CARTESIAN_POINT ( 'NONE',  ( 79.01889296114717354, 59.41967273037256092, -16.52995258344893159 ) ) ;
#74189 = AXIS2_PLACEMENT_3D ( 'NONE', #54729, #1054, #39027 ) ;
#74190 = CARTESIAN_POINT ( 'NONE',  ( 180.0250856602858960, 259.9265448933365974, -10.32933125829473830 ) ) ;
#74191 = CARTESIAN_POINT ( 'NONE',  ( 38.52196584993465223, 56.41980893122115504, -10.00000000000000000 ) ) ;
#74192 = VECTOR ( 'NONE', #26443, 1000.000000000000000 ) ;
#74193 = CARTESIAN_POINT ( 'NONE',  ( -7.294332625736644538, 178.8464784336661637, 1.353441290958777327E-15 ) ) ;
#74194 = AXIS2_PLACEMENT_3D ( 'NONE', #49811, #73135, #27526 ) ;
#74195 = CARTESIAN_POINT ( 'NONE',  ( 150.7133245577828689, 269.6038598187387834, -14.58664962216439598 ) ) ;
#74196 = CARTESIAN_POINT ( 'NONE',  ( 79.16919300666631898, 46.29637006420016121, -12.78014982653817810 ) ) ;
#74197 = CARTESIAN_POINT ( 'NONE',  ( 146.9370072200009645, 276.1446333132804511, -3.799807221059707363 ) ) ;
#74198 = CARTESIAN_POINT ( 'NONE',  ( 73.25535670630372920, 69.88482930906741331, 9.609716971570463784 ) ) ;
#74199 = CARTESIAN_POINT ( 'NONE',  ( 55.46605327235566563, 193.6423013555410080, -4.594050593750043987 ) ) ;
#74200 = CARTESIAN_POINT ( 'NONE',  ( 164.3053959849042087, 246.0617015268593661, -7.251939739328854273 ) ) ;
#74201 = CARTESIAN_POINT ( 'NONE',  ( 204.9768178125733016, 275.6167325052707611, 13.98665089523138505 ) ) ;
#74202 = CARTESIAN_POINT ( 'NONE',  ( 69.70345325596831287, 69.13798228350341901, 6.832978093666964625 ) ) ;
#74203 = CARTESIAN_POINT ( 'NONE',  ( 189.8171280724701546, 301.8740853621098950, -0.4360232994423257624 ) ) ;
#74204 = ORIENTED_EDGE ( 'NONE', *, *, #84985, .F. ) ;
#74205 = VECTOR ( 'NONE', #31675, 1000.000000000000000 ) ;
#74206 = CARTESIAN_POINT ( 'NONE',  ( -2.070769811622779510, 169.6115022471902591, 10.00000000000009592 ) ) ;
#74207 = PLANE ( 'NONE',  #12635 ) ;
#74208 = CARTESIAN_POINT ( 'NONE',  ( 114.8152493078691947, 249.3464784336661637, 1.353441290958777327E-15 ) ) ;
#74209 = CARTESIAN_POINT ( 'NONE',  ( 21.14648969749996610, 33.18502408145591431, 5.678558825948277544 ) ) ;
#74210 = CARTESIAN_POINT ( 'NONE',  ( 164.2882413842225731, 246.0914141668236539, 1.641966415049095795 ) ) ;
#74211 = CARTESIAN_POINT ( 'NONE',  ( 83.82917762730355093, 51.97629592023758249, -14.94018958758825022 ) ) ;
#74212 = CARTESIAN_POINT ( 'NONE',  ( 191.2104420009116836, 280.2857515794617598, 17.80337293751487593 ) ) ;
#74214 = CARTESIAN_POINT ( 'NONE',  ( 186.5015629097202918, 288.3730187221656820, 14.57764263923063019 ) ) ;
#74213 = FACE_OUTER_BOUND ( 'NONE', #26601, .T. ) ;
#74215 = B_SPLINE_CURVE_WITH_KNOTS ( 'NONE', 3,
 ( #71412, #18209, #24786, #18707 ),
 .UNSPECIFIED., .F., .F.,
 ( 4, 4 ),
 ( 0.03463969976448799670, 0.04344658197601434374 ),
 .UNSPECIFIED. ) ;
#74216 = CARTESIAN_POINT ( 'NONE',  ( 68.45344762038320141, 64.57392882354749020, 12.12708197217120798 ) ) ;
#74217 = EDGE_LOOP ( 'NONE', ( #10547, #68609, #85470, #82379 ) ) ;
#74218 = B_SPLINE_CURVE_WITH_KNOTS ( 'NONE', 3,
 ( #45816, #84877, #69131, #98576, #99555, #68138, #68634, #29159, #99066, #14926, #23518, #38215, #21556, #60030, #29648, #15417, #46314, #22042, #7844, #52937, #83890, #45333, #30138, #61022, #86397, #24030, #63035, #94475, #10353, #33656, #16929, #54929, #48344, #64544, #31617, #56927, #79788, #47816, #87914, #78754, #17437, #95505, #40722, #9341, #85907, #16433, #2766, #26053, #86902, #56433 ),
 .UNSPECIFIED., .F., .F.,
 ( 4, 2, 2, 2, 2, 2, 2, 2, 2, 2, 2, 2, 2, 2, 2, 2, 2, 2, 2, 2, 2, 2, 2, 2, 4 ),
 ( 0.0002266190613796248594, 0.0007024597989655380478, 0.001178300536551451236, 0.001416220905344407885, 0.001535181089740794052, 0.001654141274137180435, 0.001773101458533567036, 0.001892061642929953203, 0.002129982011722625791, 0.002605822749307888566, 0.003081663486893151341, 0.004033344962063676459, 0.004985026437234200275, 0.005460867174819500347, 0.005698787543612112219, 0.005817747728008340960, 0.005936707912404571436, 0.005996188004602654581, 0.006055668096800735992, 0.006174628281196945651, 0.006412548649989363234, 0.006888389387574264319, 0.007126309756366766904, 0.007364230125159267754, 0.007840070862744271188 ),
 .UNSPECIFIED. ) ;
#74219 = CARTESIAN_POINT ( 'NONE',  ( 150.8167050463783312, 269.4247995599803289, 14.38040671671637938 ) ) ;
#74220 = CARTESIAN_POINT ( 'NONE',  ( 208.3800376108834485, 269.7221829052733142, -1.355162556537697904 ) ) ;
#74221 = CARTESIAN_POINT ( 'NONE',  ( 181.3897897703101023, 287.9624256778719200, 13.95846517440433310 ) ) ;
#74222 = CARTESIAN_POINT ( 'NONE',  ( 172.3266757524851300, 267.7393374298979438, -16.32508309337648811 ) ) ;
#74223 = CARTESIAN_POINT ( 'NONE',  ( 196.2038536313239661, 272.5484090068244427, -13.37539213265573146 ) ) ;
#74224 = ORIENTED_EDGE ( 'NONE', *, *, #10832, .T. ) ;
#74225 = CARTESIAN_POINT ( 'NONE',  ( 69.39669185256211392, 67.72053295272533546, 8.719490259099096363 ) ) ;
#74226 = CARTESIAN_POINT ( 'NONE',  ( 171.2941760164128198, 284.5531234145211670, -11.44789784273924838 ) ) ;
#74227 = EDGE_CURVE ( 'NONE', #79527, #2619, #90627, .T. ) ;
#74228 = CARTESIAN_POINT ( 'NONE',  ( 85.18722491056296064, 44.62996190128500018, 7.606051790527071255 ) ) ;
#74229 = CARTESIAN_POINT ( 'NONE',  ( 205.2127215196890120, 270.8542949291791047, -7.926103670997396655 ) ) ;
#74230 = CARTESIAN_POINT ( 'NONE',  ( 185.8682827460642670, 296.7038206768884265, 4.702033971577086469 ) ) ;
#74231 = EDGE_CURVE ( 'NONE', #54612, #44705, #53902, .T. ) ;
#74232 = CARTESIAN_POINT ( 'NONE',  ( 69.83738656355549779, 70.92545396396145918, 1.304034296880247412 ) ) ;
#74233 = DIRECTION ( 'NONE',  ( -0.9879428538673736826, -0.1548189829846108034, 0.000000000000000000 ) ) ;
#74234 = VERTEX_POINT ( 'NONE', #33120 ) ;
#74235 = DIRECTION ( 'NONE',  ( 0.8660254037844373753, 0.5000000000000021094, 0.000000000000000000 ) ) ;
#74236 = EDGE_CURVE ( 'NONE', #97401, #88729, #79771, .T. ) ;
#74237 = CARTESIAN_POINT ( 'NONE',  ( 10.89475974595093000, 11.45404122711131478, -8.090169943749478065 ) ) ;
#74238 = CARTESIAN_POINT ( 'NONE',  ( 82.93658845200469898, 45.09976895464361490, 10.63726503173775484 ) ) ;
#74239 = ORIENTED_EDGE ( 'NONE', *, *, #11339, .F. ) ;
#74240 = DIRECTION ( 'NONE',  ( 1.000000000000000000, 0.000000000000000000, 0.000000000000000000 ) ) ;
#74241 = EDGE_CURVE ( 'NONE', #47030, #54902, #3250, .T. ) ;
#74242 = CARTESIAN_POINT ( 'NONE',  ( 86.52685127962818967, 47.39493317473652212, -10.85533565734823824 ) ) ;
#74243 = CARTESIAN_POINT ( 'NONE',  ( 158.4984048909838634, 263.4026134211973726, -17.02607271676052392 ) ) ;
#74244 = ORIENTED_EDGE ( 'NONE', *, *, #83368, .T. ) ;
#74245 = FACE_OUTER_BOUND ( 'NONE', #36684, .T. ) ;
#74246 = CARTESIAN_POINT ( 'NONE',  ( 67.15772368909350121, 67.74692886573922124, -6.548511843863573212 ) ) ;
#74247 = CARTESIAN_POINT ( 'NONE',  ( 164.4864504671816690, 245.7481059646165704, 6.337356894698421783 ) ) ;
#74248 = CARTESIAN_POINT ( 'NONE',  ( 162.5887743522035294, 284.9919049736276975, -2.844505511527740005 ) ) ;
#74249 = CARTESIAN_POINT ( 'NONE',  ( 32.07315653955451040, 47.77038272570916888, -10.00000000000000000 ) ) ;
#74250 = ORIENTED_EDGE ( 'NONE', *, *, #16187, .T. ) ;
#74251 = CARTESIAN_POINT ( 'NONE',  ( 83.09741599002914825, 218.7833772461660544, -9.188101187500095079 ) ) ;
#74252 = CARTESIAN_POINT ( 'NONE',  ( 155.3607606009346398, 261.5542644670730965, 17.00535455698268095 ) ) ;
#74253 = CARTESIAN_POINT ( 'NONE',  ( 81.23970239364686563, 42.24692268292314168, -7.309682766412492150 ) ) ;
#74254 = ORIENTED_EDGE ( 'NONE', *, *, #18587, .F. ) ;
#74255 = ORIENTED_EDGE ( 'NONE', *, *, #3970, .T. ) ;
#74256 = DIRECTION ( 'NONE',  ( -0.8660254037844383745, -0.5000000000000004441, 0.000000000000000000 ) ) ;
#74257 = ORIENTED_EDGE ( 'NONE', *, *, #55587, .T. ) ;
#74258 = LINE ( 'NONE', #96580, #83829 ) ;
#74259 = VERTEX_POINT ( 'NONE', #88389 ) ;
#74260 = CARTESIAN_POINT ( 'NONE',  ( 167.8099530253072089, 271.3928698661641761, -17.53051755021046532 ) ) ;
#74261 = CARTESIAN_POINT ( 'NONE',  ( 156.6812872898450735, 261.2670451491295012, 0.000000000000000000 ) ) ;
#74262 = VERTEX_POINT ( 'NONE', #65027 ) ;
#74263 = B_SPLINE_CURVE_WITH_KNOTS ( 'NONE', 3,
 ( #86759, #56789, #87775, #2110, #17293, #48195, #95364, #25395, #79143, #32992, #63894, #94832, #56282, #87281, #17812, #48713, #79644, #10210, #41075, #72012, #2617, #8264, #31047, #99477, #39128, #54329, #15335, #52852, #75676, #91903, #59946, #91394, #61934, #7248, #98980, #22945, #60438, #92398, #6763, #76660, #22458, #46230, #83802, #30053, #84303, #83302, #38650, #14367, #90917, #29564, #21959, #70042 ),
 .UNSPECIFIED., .F., .F.,
 ( 4, 2, 2, 2, 2, 2, 2, 2, 2, 2, 2, 2, 2, 2, 2, 2, 2, 2, 2, 2, 2, 2, 2, 2, 2, 4 ),
 ( 0.0001479525476070201362, 0.0006328501284903549802, 0.001117747709373689878, 0.001360196499815357436, 0.001481420895036139824, 0.001602645290256922211, 0.001723869685477704815, 0.001845094080698487203, 0.001966318475919270024, 0.002087542871140052412, 0.002572440452022936499, 0.003057338032905820152, 0.004027133194671691542, 0.004996928356437562932, 0.005481825937320463499, 0.005724274727761836587, 0.005845499122982446803, 0.005966723518203056152, 0.006027335715813398991, 0.006087947913423741829, 0.006209172308644423169, 0.006451621099085631458, 0.006936518679968144314, 0.007178967470409401176, 0.007421416260850658038, 0.007906313841733193445 ),
 .UNSPECIFIED. ) ;
#74264 = CARTESIAN_POINT ( 'NONE',  ( 207.5070909066002116, 271.2341709493916255, -7.107478141010028949 ) ) ;
#74265 = EDGE_CURVE ( 'NONE', #84750, #4766, #34653, .T. ) ;
#74266 = CARTESIAN_POINT ( 'NONE',  ( 82.15776938016838926, 40.64327202660170713, 3.515950796866609718 ) ) ;
#74267 = CARTESIAN_POINT ( 'NONE',  ( 80.61131623575732874, 43.32435129898595960, -9.365491868763141881 ) ) ;
#74268 = AXIS2_PLACEMENT_3D ( 'NONE', #72537, #77884, #23149 ) ;
#74269 = CARTESIAN_POINT ( 'NONE',  ( 152.8721808860877616, 265.8646109718731623, -17.65676496037632504 ) ) ;
#74270 = DIRECTION ( 'NONE',  ( 0.000000000000000000, 1.000000000000000000, 0.000000000000000000 ) ) ;
#74272 = CARTESIAN_POINT ( 'NONE',  ( -44.49648453423615990, 28.96346851210257611, -10.00000000000000000 ) ) ;
#74271 = VECTOR ( 'NONE', #66308, 1000.000000000000227 ) ;
#74273 = CARTESIAN_POINT ( 'NONE',  ( 138.9021014942714487, 244.8768266524159856, 9.188101187500098632 ) ) ;
#74274 = CARTESIAN_POINT ( 'NONE',  ( 168.1505723841142128, 267.0769752754364390, -17.55733195497056798 ) ) ;
#74275 = ORIENTED_EDGE ( 'NONE', *, *, #22452, .T. ) ;
#74276 = CARTESIAN_POINT ( 'NONE',  ( 76.86366411620821282, 60.80910549659888886, 15.73837547318715480 ) ) ;
#74277 = CARTESIAN_POINT ( 'NONE',  ( 15.64721481668148328, 11.96004757982088940, -5.678558825948276656 ) ) ;
#74278 = VECTOR ( 'NONE', #87643, 1000.000000000000114 ) ;
#74279 = ORIENTED_EDGE ( 'NONE', *, *, #38510, .T. ) ;
#74280 = CARTESIAN_POINT ( 'NONE',  ( 25.96864935082048831, 154.0458036431183189, 30.52142883766506998 ) ) ;
#74281 = VECTOR ( 'NONE', #27870, 1000.000000000000000 ) ;
#74283 = EDGE_LOOP ( 'NONE', ( #42990, #61978, #67384, #93847 ) ) ;
#74282 = CARTESIAN_POINT ( 'NONE',  ( 200.2816180127317125, 270.3372598560825395, 9.268223811809287227 ) ) ;
#74284 = CARTESIAN_POINT ( 'NONE',  ( 2.117331368781439682, 160.4824982072973683, 3.021315404115420679E-15 ) ) ;
#74285 = CARTESIAN_POINT ( 'NONE',  ( 170.7320525446532713, 288.3325263888784207, -5.627708583524104746 ) ) ;
#74286 = CARTESIAN_POINT ( 'NONE',  ( 160.6734846709049691, 282.6943762970620924, -6.583290857611773461 ) ) ;
#74287 = CARTESIAN_POINT ( 'NONE',  ( 82.75883821533659557, 49.82052486449969564, -14.21782099992554116 ) ) ;
#74288 = CARTESIAN_POINT ( 'NONE',  ( 157.8323084318549547, 257.8542024558915955, 16.74327773638376726 ) ) ;
#74289 = DIRECTION ( 'NONE',  ( -0.5000000000000006661, 0.8660254037844382635, -1.877843081442121204E-16 ) ) ;
#74290 = CARTESIAN_POINT ( 'NONE',  ( -23.47208873469913115, 24.42380372261332155, -10.00000000000000000 ) ) ;
#74291 = AXIS2_PLACEMENT_3D ( 'NONE', #4071, #34961, #66372 ) ;
#74292 = VERTEX_POINT ( 'NONE', #41711 ) ;
#74293 = CARTESIAN_POINT ( 'NONE',  ( 181.5913590924892560, 271.3060279288629317, -15.97644946730743598 ) ) ;
#74294 = CARTESIAN_POINT ( 'NONE',  ( 65.98410341620582642, 69.22083730553454473, 0.2678598787953536675 ) ) ;
#74295 = ORIENTED_EDGE ( 'NONE', *, *, #81114, .F. ) ;
#74296 = CARTESIAN_POINT ( 'NONE',  ( 160.6982348739816757, 275.7565010011308004, 12.80364755394902687 ) ) ;
#74297 = CARTESIAN_POINT ( 'NONE',  ( 173.4859908262079955, 280.5480941373698442, -14.23958667651489129 ) ) ;
#74298 = CARTESIAN_POINT ( 'NONE',  ( -57.88150100324660485, 35.92665207732902388, -10.00000000000000000 ) ) ;
#74299 = CARTESIAN_POINT ( 'NONE',  ( 81.88567891057422798, 44.78205882872802590, -10.20763061476163536 ) ) ;
#74300 = EDGE_CURVE ( 'NONE', #88206, #46023, #94962, .T. ) ;
#74301 = CARTESIAN_POINT ( 'NONE',  ( 160.8321869569444971, 272.7815025554300519, 15.68266994514650214 ) ) ;
#74303 = CARTESIAN_POINT ( 'NONE',  ( 88.06349342987242323, 44.28914147295815695, 2.792731503129179504 ) ) ;
#74302 = CARTESIAN_POINT ( 'NONE',  ( 79.14312167556931854, 57.64441083166269664, 0.000000000000000000 ) ) ;
#74304 = VECTOR ( 'NONE', #60924, 1000.000000000000000 ) ;
#74305 = CARTESIAN_POINT ( 'NONE',  ( -105.0000000000000000, 10.00000000000000000, -54.99999999999999289 ) ) ;
#74306 = ORIENTED_EDGE ( 'NONE', *, *, #19017, .F. ) ;
#74307 = PRODUCT ( 'Lower Tilting Cradle Base Segment', 'Lower Tilting Cradle Base Segment', '', ( #46129 ) ) ;
#74308 = ORIENTED_EDGE ( 'NONE', *, *, #73887, .F. ) ;
#74309 = DIRECTION ( 'NONE',  ( -1.000000000000000000, 0.000000000000000000, 0.000000000000000000 ) ) ;
#74310 = CARTESIAN_POINT ( 'NONE',  ( 80.31495243796621253, 58.05602015539035676, 16.26171843954676177 ) ) ;
#74311 = CARTESIAN_POINT ( 'NONE',  ( 85.74709191876297609, 48.50741248266042049, -11.78150043536521174 ) ) ;
#74312 = CARTESIAN_POINT ( 'NONE',  ( 192.7693357657653053, 296.7607116428271183, 12.22606306887835714 ) ) ;
#74313 = CARTESIAN_POINT ( 'NONE',  ( 80.82785412337717901, 42.97997768494945348, -9.612963753214643248 ) ) ;
#74314 = FACE_OUTER_BOUND ( 'NONE', #59878, .T. ) ;
#74315 = CARTESIAN_POINT ( 'NONE',  ( 7.590999645455913658, 169.0643266524160140, -9.188101187500093303 ) ) ;
#74316 = CARTESIAN_POINT ( 'NONE',  ( 98.90203251333015544, 240.1589784336661637, -6.496448406907675876E-16 ) ) ;
#74317 = CARTESIAN_POINT ( 'NONE',  ( 87.87366831029828518, 44.19753277059973584, -4.411077605820556968 ) ) ;
#74318 = CARTESIAN_POINT ( 'NONE',  ( 186.6730029007337919, 295.8052390787480022, -7.682216135788281441 ) ) ;
#74319 = CARTESIAN_POINT ( 'NONE',  ( 78.14971419250070994, 52.01379824954777575, 15.54497553320235248 ) ) ;
#74320 = CARTESIAN_POINT ( 'NONE',  ( 76.25499879835211914, 51.34390249587517019, 15.62284479604242549 ) ) ;
#74321 = FACE_OUTER_BOUND ( 'NONE', #39287, .T. ) ;
#74322 = CARTESIAN_POINT ( 'NONE',  ( 194.6310785344323904, 293.5360785768717165, -14.54510914272505495 ) ) ;
#74323 = CARTESIAN_POINT ( 'NONE',  ( 84.46805331009542783, 50.67741563211675526, 13.74683494288181507 ) ) ;
#74324 = CARTESIAN_POINT ( 'NONE',  ( 196.2517347386735480, 266.7219944345126237, 8.057602692514423737 ) ) ;
#74325 = CARTESIAN_POINT ( 'NONE',  ( 32.07315653955450330, 47.77038272570916888, -10.00000000000000000 ) ) ;
#74326 = CARTESIAN_POINT ( 'NONE',  ( 66.95321124882991626, 197.9155109091896350, 2.679491924311254714 ) ) ;
#74327 = CARTESIAN_POINT ( 'NONE',  ( 172.6066657261125101, 263.4582241914548604, -15.40626036171160607 ) ) ;
#74328 = CARTESIAN_POINT ( 'NONE',  ( 75.46539357129627490, 220.5024278399160664, -9.188101187500093303 ) ) ;
#74329 = CARTESIAN_POINT ( 'NONE',  ( 8.146472837920740062, 20.10171378149916777, 9.188101187500008038 ) ) ;
#74330 = CARTESIAN_POINT ( 'NONE',  ( 190.8443993347725325, 300.0947993426467519, 8.522468760355437212 ) ) ;
#74331 = AXIS2_PLACEMENT_3D ( 'NONE', #49019, #71833, #10519 ) ;
#74332 = CARTESIAN_POINT ( 'NONE',  ( -13.86269525828472204, 104.0355397767245194, 10.71312146367169404 ) ) ;
#74334 = CARTESIAN_POINT ( 'NONE',  ( 152.3580564471173489, 266.7551006215829261, 15.57995064934159046 ) ) ;
#74333 = CARTESIAN_POINT ( 'NONE',  ( 196.4677418905696129, 290.3548843276421394, 17.08610552292358520 ) ) ;
#74335 = CARTESIAN_POINT ( 'NONE',  ( 197.0269530679106254, 289.3863021563271900, 16.70650816643942704 ) ) ;
#74336 = CARTESIAN_POINT ( 'NONE',  ( 198.7357616895271804, 286.4265588032756114, -17.04018524297827497 ) ) ;
#74337 = CARTESIAN_POINT ( 'NONE',  ( 80.46653820500203835, 44.39910589696482646, 11.34020455946100370 ) ) ;
#74338 = CARTESIAN_POINT ( 'NONE',  ( 33.97448420766330202, 31.56628583063843152, 9.188101187500006262 ) ) ;
#74339 = CARTESIAN_POINT ( 'NONE',  ( 147.2658550951450422, 275.5750520855697800, -5.215660180131691526 ) ) ;
#74340 = CARTESIAN_POINT ( 'NONE',  ( -3.985554314188680003, 180.0530062829863311, 2.649461200531984646E-14 ) ) ;
#74341 = ORIENTED_EDGE ( 'NONE', *, *, #90386, .F. ) ;
#74342 = CARTESIAN_POINT ( 'NONE',  ( 20.59861825492957621, 33.93396525600390845, 2.839279412974139660 ) ) ;
#74343 = AXIS2_PLACEMENT_3D ( 'NONE', #68026, #52321, #44215 ) ;
#74344 = CARTESIAN_POINT ( 'NONE',  ( 172.4419760422836134, 290.9306500000749907, -0.6531725299933459628 ) ) ;
#74345 = CARTESIAN_POINT ( 'NONE',  ( 192.4259603496955719, 297.3554553095298729, -12.40738485318142814 ) ) ;
#74346 = LINE ( 'NONE', #96660, #39618 ) ;
#74347 = VERTEX_POINT ( 'NONE', #48839 ) ;
#74348 = EDGE_CURVE ( 'NONE', #98895, #88538, #72655, .T. ) ;
#74349 = CARTESIAN_POINT ( 'NONE',  ( 70.51412929403316809, 60.93737776118788929, 14.98137441988405705 ) ) ;
#74350 = CARTESIAN_POINT ( 'NONE',  ( 198.2489255580726422, 287.2697837179150042, 18.53597557040773225 ) ) ;
#74351 = CARTESIAN_POINT ( 'NONE',  ( 157.8111766759666068, 268.3688148911334110, 16.25763562993056510 ) ) ;
#74352 = EDGE_CURVE ( 'NONE', #41536, #42536, #70909, .T. ) ;
#74353 = CARTESIAN_POINT ( 'NONE',  ( 184.5341303888194773, 280.6061766946581315, -17.60036545423847087 ) ) ;
#74355 = CARTESIAN_POINT ( 'NONE',  ( 87.40330451559304947, 45.01222676107010301, -6.126549417040136447 ) ) ;
#74354 = VECTOR ( 'NONE', #26267, 1000.000000000000000 ) ;
#74356 = CARTESIAN_POINT ( 'NONE',  ( 136.8541387121308901, 256.4865022471902876, -10.00000000000009415 ) ) ;
#74357 = CARTESIAN_POINT ( 'NONE',  ( 204.9658583905037688, 275.6357147811169170, -12.57240504404813564 ) ) ;
#74358 = CARTESIAN_POINT ( 'NONE',  ( 75.36158518500756998, 53.45249184671629905, 16.03634573857044288 ) ) ;
#74359 = EDGE_LOOP ( 'NONE', ( #95098, #41048, #98669 ) ) ;
#74360 = CARTESIAN_POINT ( 'NONE',  ( 72.00273082287530713, 68.45064935962042796, 10.42463711869592657 ) ) ;
#74361 = CARTESIAN_POINT ( 'NONE',  ( 167.3097680743688613, 247.9456010488782454, -1.868104155933442145 ) ) ;
#74362 = ORIENTED_EDGE ( 'NONE', *, *, #58942, .T. ) ;
#74363 = DIRECTION ( 'NONE',  ( -0.000000000000000000, -0.000000000000000000, -1.000000000000000000 ) ) ;
#74364 = DIRECTION ( 'NONE',  ( -0.8660254037844387076, -0.4999999999999998890, -0.000000000000000000 ) ) ;
#74365 = EDGE_CURVE ( 'NONE', #77218, #58030, #3738, .T. ) ;
#74366 = ORIENTED_EDGE ( 'NONE', *, *, #2725, .F. ) ;
#74367 = CARTESIAN_POINT ( 'NONE',  ( 77.31168512783449387, 63.18411157796573008, -15.22841949698756459 ) ) ;
#74368 = ORIENTED_EDGE ( 'NONE', *, *, #43760, .F. ) ;
#74369 = CARTESIAN_POINT ( 'NONE',  ( 190.2861294957589564, 290.5072236206235061, 14.49960583659686009 ) ) ;
#74370 = CARTESIAN_POINT ( 'NONE',  ( 205.8468767641892043, 274.1097461954921073, 10.74163015103096797 ) ) ;
#74371 = CARTESIAN_POINT ( 'NONE',  ( 157.5215017335775940, 258.4853116787141971, -16.92298772477023761 ) ) ;
#74372 = CARTESIAN_POINT ( 'NONE',  ( 25.34687108590969729, 93.06504152958497400, 45.00000000000000711 ) ) ;
#74373 = CARTESIAN_POINT ( 'NONE',  ( 84.06604358195920668, 51.46910565605918464, 14.65639964578790710 ) ) ;
#74374 = VECTOR ( 'NONE', #39024, 1000.000000000000000 ) ;
#74375 = CARTESIAN_POINT ( 'NONE',  ( 38.84587710395076954, 34.37878583063844218, 9.188101187500006262 ) ) ;
#74376 = DIRECTION ( 'NONE',  ( 0.4999999999999998890, -0.8660254037844385966, 0.000000000000000000 ) ) ;
#74377 = CARTESIAN_POINT ( 'NONE',  ( 87.35606880162971777, 45.77061481740688009, 8.290963297571636303 ) ) ;
#74378 = DIRECTION ( 'NONE',  ( 0.3103181967972123423, -0.9506327454577433445, 0.000000000000000000 ) ) ;
#74379 = ORIENTED_EDGE ( 'NONE', *, *, #71324, .F. ) ;
#74380 = VERTEX_POINT ( 'NONE', #34615 ) ;
#74381 = CARTESIAN_POINT ( 'NONE',  ( -51.42721978966704910, 42.16899896210639298, -54.99999999999999289 ) ) ;
#74383 = CARTESIAN_POINT ( 'NONE',  ( 162.7122087945529927, 272.4192740586219657, -15.63422411579954563 ) ) ;
#74382 = FACE_OUTER_BOUND ( 'NONE', #64031, .T. ) ;
#74384 = CARTESIAN_POINT ( 'NONE',  ( 85.59998877908455484, 48.66343243370425142, 12.43629469118824638 ) ) ;
#74385 = DIRECTION ( 'NONE',  ( 0.5000000000000048850, -0.8660254037844358210, 0.000000000000000000 ) ) ;
#74386 = CARTESIAN_POINT ( 'NONE',  ( 160.9155581428462085, 282.2930683307629920, -7.657675304491033508 ) ) ;
#74387 = CARTESIAN_POINT ( 'NONE',  ( 82.33791607580600669, 40.35809408978042967, 1.142683882547790519 ) ) ;
#74388 = CARTESIAN_POINT ( 'NONE',  ( 170.3564602903425111, 288.9689526880741823, -4.407563815828527964 ) ) ;
#74389 = CARTESIAN_POINT ( 'NONE',  ( 159.2720798248943765, 273.8135256516483764, -15.04173180978755298 ) ) ;
#74390 = CARTESIAN_POINT ( 'NONE',  ( 178.9144291139083975, 255.9268924588826621, 4.886238089006308627 ) ) ;
#74391 = CARTESIAN_POINT ( 'NONE',  ( 102.5290345353249961, 223.8768266524159856, 9.188101187500098632 ) ) ;
#74392 = VERTEX_POINT ( 'NONE', #11837 ) ;
#74393 = DIRECTION ( 'NONE',  ( 0.000000000000000000, 0.000000000000000000, 1.000000000000000000 ) ) ;
#74394 = CARTESIAN_POINT ( 'NONE',  ( 192.0603001030472683, 293.3461588932823929, -14.68827779892621344 ) ) ;
#74395 = ORIENTED_EDGE ( 'NONE', *, *, #49575, .T. ) ;
#74396 = ORIENTED_EDGE ( 'NONE', *, *, #34932, .F. ) ;
#74397 = CARTESIAN_POINT ( 'NONE',  ( 186.8003541658358984, 299.2222177555264011, -0.6103433986344138917 ) ) ;
#74398 = CARTESIAN_POINT ( 'NONE',  ( 71.96307967416730378, 59.12692550662651314, 15.37583765050489859 ) ) ;
#74399 = CARTESIAN_POINT ( 'NONE',  ( 164.2183954753924979, 249.9265173926981163, 10.12780430522023423 ) ) ;
#74400 = CARTESIAN_POINT ( 'NONE',  ( 159.3586121662929713, 254.6297824347537642, -15.50090345830412630 ) ) ;
#74401 = CARTESIAN_POINT ( 'NONE',  ( 163.1611253217825492, 248.0436364529968216, 11.42797785440508029 ) ) ;
#74402 = VERTEX_POINT ( 'NONE', #58405 ) ;
#74403 = ORIENTED_EDGE ( 'NONE', *, *, #46504, .F. ) ;
#74404 = CARTESIAN_POINT ( 'NONE',  ( 163.3020905273760093, 247.7994775548095845, -11.05431316445765155 ) ) ;
#74405 = ORIENTED_EDGE ( 'NONE', *, *, #61760, .F. ) ;
#74406 = VECTOR ( 'NONE', #35236, 1000.000000000000000 ) ;
#74407 = B_SPLINE_CURVE_WITH_KNOTS ( 'NONE', 3,
 ( #70273, #17076, #39853, #16081, #8489, #63181, #86054, #39359, #32277, #79928, #94124, #95133, #56578, #16579, #56058, #86545, #47477, #31763, #24678, #2916, #17586, #8982, #18094, #40860, #62667, #70788, #9498, #1397, #47966, #40364, #85539, #32775, #94620, #25178, #87051, #71807, #10488, #2403, #25698, #26191, #41369, #72307, #33808, #64692, #95644, #81922 ),
 .UNSPECIFIED., .F., .F.,
 ( 4, 1, 2, 2, 1, 2, 2, 1, 1, 2, 2, 1, 1, 2, 2, 1, 1, 2, 2, 1, 1, 1, 2, 2, 1, 1, 1, 2, 2, 4 ),
 ( 0.000000000000000000, 0.06250000000000142941, 0.09375000000000123512, 0.1250000000000010547, 0.1874999999999988898, 0.2187499999999966693, 0.2499999999999944489, 0.3124999999999933387, 0.3437499999999927836, 0.3593749999999907851, 0.3749999999999887867, 0.4374999999999796829, 0.4687499999999751310, 0.4843749999999724110, 0.4999999999999696354, 0.5624999999999605871, 0.5937499999999549249, 0.6093749999999518163, 0.6249999999999485967, 0.6874999999999394928, 0.7187499999999349409, 0.7343749999999334976, 0.7421874999999338307, 0.7499999999999340528, 0.8124999999999359401, 0.8437499999999379385, 0.8593749999999398259, 0.8671874999999427125, 0.8749999999999454880, 1.000000000000000000 ),
 .UNSPECIFIED. ) ;
#74408 = CARTESIAN_POINT ( 'NONE',  ( 193.8703746310723943, 265.8671889252453866, -7.747450020969885109 ) ) ;
#74409 = CARTESIAN_POINT ( 'NONE',  ( 153.2832131836460121, 266.4580806215291773, 16.33893799534572722 ) ) ;
#74410 = ADVANCED_FACE ( 'NONE', ( #65515 ), #30433, .F. ) ;
#74411 = CARTESIAN_POINT ( 'NONE',  ( 83.89386139451886493, 49.22207443597933008, 13.04948611042680540 ) ) ;
#74413 = CARTESIAN_POINT ( 'NONE',  ( 69.41166179968418248, 62.72696118611258242, -13.78096777156330077 ) ) ;
#74412 = CARTESIAN_POINT ( 'NONE',  ( 136.0332187963529975, 249.3458772461660544, 9.188101187500095079 ) ) ;
#74414 = CARTESIAN_POINT ( 'NONE',  ( -23.39332202855467813, 99.74324603395649547, 45.19937630303414977 ) ) ;
#74415 = ORIENTED_EDGE ( 'NONE', *, *, #37950, .T. ) ;
#74416 = CARTESIAN_POINT ( 'NONE',  ( 190.6954410837624607, 300.3528026016029457, -5.728531842148099962 ) ) ;
#74417 = CYLINDRICAL_SURFACE ( 'NONE', #77231, 10.00000000000010658 ) ;
#74418 = CARTESIAN_POINT ( 'NONE',  ( 206.7408728089182546, 272.5612996242556960, -10.63134519248043475 ) ) ;
#74419 = DIRECTION ( 'NONE',  ( 1.000000000000000000, 0.000000000000000000, 0.000000000000000000 ) ) ;
#74420 = CARTESIAN_POINT ( 'NONE',  ( 39.49844957003027446, 193.6115022471902591, 10.00000000000009592 ) ) ;
#74421 = FACE_OUTER_BOUND ( 'NONE', #97090, .T. ) ;
#74422 = ADVANCED_FACE ( 'NONE', ( #59383 ), #50806, .T. ) ;
#74423 = CARTESIAN_POINT ( 'NONE',  ( 199.0467776771448882, 281.9810065596747108, -16.63176243157295175 ) ) ;
#74424 = CYLINDRICAL_SURFACE ( 'NONE', #70542, 10.00000000000010658 ) ;
#74425 = CARTESIAN_POINT ( 'NONE',  ( 80.25206473404905694, 51.20499363921007330, 14.98319710954680417 ) ) ;
#74426 = CARTESIAN_POINT ( 'NONE',  ( 86.18027666378027618, 49.75620593066998509, 1.003037947553365612E-13 ) ) ;
#74427 = CARTESIAN_POINT ( 'NONE',  ( 55.22204975783502334, 208.8149278399160664, 9.188101187500093303 ) ) ;
#74428 = CARTESIAN_POINT ( 'NONE',  ( 167.6185327982364015, 249.9494983323436088, 7.055657055613346884 ) ) ;
#74429 = CARTESIAN_POINT ( 'NONE',  ( 77.62454426129153262, 61.88953154547135682, 15.65088405748084988 ) ) ;
#74430 = CARTESIAN_POINT ( 'NONE',  ( 162.9383752892161397, 248.4294508267893491, -11.25953730674605957 ) ) ;
#74431 = EDGE_CURVE ( 'NONE', #42198, #54426, #10439, .T. ) ;
#74432 = CARTESIAN_POINT ( 'NONE',  ( 66.64574440031255165, 67.65126300000102333, 6.155624976568763174 ) ) ;
#74433 = AXIS2_PLACEMENT_3D ( 'NONE', #55978, #38796, #9923 ) ;
#74434 = DIRECTION ( 'NONE',  ( -0.4621356007560455392, 0.8868092729070039537, 0.000000000000000000 ) ) ;
#74436 = DIRECTION ( 'NONE',  ( 0.8660254037844384856, 0.5000000000000002220, 3.252519625699449945E-16 ) ) ;
#74435 = CARTESIAN_POINT ( 'NONE',  ( 73.55996738445699634, 69.73057641899073644, -9.398744228737333728 ) ) ;
#74437 = CARTESIAN_POINT ( 'NONE',  ( 172.9698904924519240, 250.6642211707864476, -4.168778760986519671 ) ) ;
#74438 = CARTESIAN_POINT ( 'NONE',  ( 37.37984742713354791, 29.78052372038643369, -10.00000000000000355 ) ) ;
#74439 = CARTESIAN_POINT ( 'NONE',  ( 77.47571766935273274, 57.04508641376936851, -16.61716333516349664 ) ) ;
#74440 = CARTESIAN_POINT ( 'NONE',  ( 157.6510097567892501, 270.8399773495983709, -14.84913773220146993 ) ) ;
#74441 = FACE_OUTER_BOUND ( 'NONE', #86355, .T. ) ;
#74442 = CARTESIAN_POINT ( 'NONE',  ( 161.0965315767822972, 251.6196177163260188, -13.76772246540905442 ) ) ;
#74443 = CARTESIAN_POINT ( 'NONE',  ( 13.49027706508988267, 190.8464784336661637, 1.353441290958777327E-15 ) ) ;
#74444 = DIRECTION ( 'NONE',  ( -0.7071067811865465735, 8.659560562354921765E-17, 0.7071067811865484609 ) ) ;
#74445 = ORIENTED_EDGE ( 'NONE', *, *, #87798, .T. ) ;
#74446 = CARTESIAN_POINT ( 'NONE',  ( 86.80277191894818145, 46.47277518407399555, 9.069725256793763180 ) ) ;
#74447 = CARTESIAN_POINT ( 'NONE',  ( 181.0686324902563911, 280.4193002135394295, 17.28172028329132104 ) ) ;
#74448 = CARTESIAN_POINT ( 'NONE',  ( 208.1876422586379647, 270.0554214305024630, 3.377638779759113863 ) ) ;
#74449 = CARTESIAN_POINT ( 'NONE',  ( 71.95078207959971905, 72.63412948483367870, -0.9918729297793668076 ) ) ;
#74450 = CARTESIAN_POINT ( 'NONE',  ( 42.85403768609726427, 204.7369531367911293, -4.594050593750048428 ) ) ;
#74451 = CARTESIAN_POINT ( 'NONE',  ( 87.36774593059779193, 45.94567951850589083, 8.539250186115692642 ) ) ;
#74452 = CARTESIAN_POINT ( 'NONE',  ( 199.2205425252482200, 285.5868937652708155, -18.05012564782189344 ) ) ;
#74453 = CARTESIAN_POINT ( 'NONE',  ( 190.2648877593310317, 301.0985428348857340, -4.426259207433023590 ) ) ;
#74454 = CARTESIAN_POINT ( 'NONE',  ( 41.28778705816291961, 32.03677371833806120, 10.00000000000000533 ) ) ;
#74455 = CARTESIAN_POINT ( 'NONE',  ( 203.0676174199914215, 269.8692695890372306, -7.319173559847955701 ) ) ;
#74456 = CARTESIAN_POINT ( 'NONE',  ( 178.8150194001607360, 293.5229817246915331, 2.654719043459385031 ) ) ;
#74457 = CARTESIAN_POINT ( 'NONE',  ( 180.0213682611045556, 276.4079177606270150, 16.56764346391123510 ) ) ;
#74458 = CARTESIAN_POINT ( 'NONE',  ( 180.2261984326610218, 279.1782745765357276, -17.42438828499370729 ) ) ;
#74459 = CARTESIAN_POINT ( 'NONE',  ( 70.96446909585041851, 67.83507693878627265, -9.741514685561401876 ) ) ;
#74460 = EDGE_CURVE ( 'NONE', #67048, #57230, #1624, .T. ) ;
#74461 = CARTESIAN_POINT ( 'NONE',  ( 167.0953271602620305, 257.8792139306702893, -15.57180271813312444 ) ) ;
#74462 = CARTESIAN_POINT ( 'NONE',  ( 74.19247292150758710, 57.10187714277506643, -16.01396260610887268 ) ) ;
#74464 =( BOUNDED_CURVE ( )  B_SPLINE_CURVE ( 2, ( #99315, #29894, #68880, #59789, #59276, #90253, #20826, #13225, #75022 ),
 .UNSPECIFIED., .F., .T. ) 
 B_SPLINE_CURVE_WITH_KNOTS ( ( 3, 2, 2, 2, 3 ),
 ( 0.06048387096774193727, 0.06182795698924731242, 0.06451612903225806273, 0.06720430107526881303, 0.06854838709677418818 ),
 .UNSPECIFIED. ) 
 CURVE ( )  GEOMETRIC_REPRESENTATION_ITEM ( )  RATIONAL_B_SPLINE_CURVE ( ( 0.9330127018922194093, 0.9330127018922194093, 1.000000000000000000, 0.8660254037844387076, 1.000000000000000000, 0.8660254037844387076, 1.000000000000000000, 0.9330127018922194093, 0.9330127018922194093 ) ) 
 REPRESENTATION_ITEM ( '' )  );
#74463 = CARTESIAN_POINT ( 'NONE',  ( 96.65612621980328356, 216.6115022471901739, -5.000000000000041744 ) ) ;
#74465 = DIRECTION ( 'NONE',  ( 0.5000000000000014433, -0.8660254037844378194, 0.000000000000000000 ) ) ;
#74466 = CARTESIAN_POINT ( 'NONE',  ( 165.2649712138198481, 269.7723956468109350, -16.27622833696107918 ) ) ;
#74467 = ORIENTED_EDGE ( 'NONE', *, *, #67191, .T. ) ;
#74468 = CARTESIAN_POINT ( 'NONE',  ( 46.94050828626382099, 210.1589784336661637, -6.496448406907675876E-16 ) ) ;
#74469 = ORIENTED_EDGE ( 'NONE', *, *, #33309, .F. ) ;
#74470 = CARTESIAN_POINT ( 'NONE',  ( 46.80963145949300497, 71.09457308843315104, 10.00000000000000000 ) ) ;
#74471 = CARTESIAN_POINT ( 'NONE',  ( 190.4240181651484818, 300.8229208869809668, -4.214281362166949485 ) ) ;
#74473 = DIRECTION ( 'NONE',  ( -0.3371987438498166290, 0.9414334852479520066, 0.000000000000000000 ) ) ;
#74472 = AXIS2_PLACEMENT_3D ( 'NONE', #53739, #37547, #29960 ) ;
#74474 = EDGE_CURVE ( 'NONE', #70064, #33315, #35727, .T. ) ;
#74475 = VERTEX_POINT ( 'NONE', #47684 ) ;
#74476 = CARTESIAN_POINT ( 'NONE',  ( 59.82969263072505584, 216.8967562850347122, -4.648177544792955347E-16 ) ) ;
#74477 = CARTESIAN_POINT ( 'NONE',  ( 207.1122325394003951, 271.9180857031755636, 7.794245785756032774 ) ) ;
#74478 = FACE_OUTER_BOUND ( 'NONE', #55439, .T. ) ;
#74479 = CARTESIAN_POINT ( 'NONE',  ( 24.92213970864663963, 37.49540643055189548, 3.479690158560446702E-15 ) ) ;
#74480 = CARTESIAN_POINT ( 'NONE',  ( 0.1270659342858249108, 66.35802143352867688, -10.00000000000000000 ) ) ;
#74481 = CARTESIAN_POINT ( 'NONE',  ( 86.12135434523638366, 46.98046262810483142, -10.13131473785488090 ) ) ;
#74482 = CARTESIAN_POINT ( 'NONE',  ( 204.2956748066270620, 276.7965067987898919, 13.85972809245231119 ) ) ;
#74483 = ORIENTED_EDGE ( 'NONE', *, *, #7153, .F. ) ;
#74484 = CARTESIAN_POINT ( 'NONE',  ( 21.59269996301512506, 13.26216523072493914, -2.296566073217252530E-15 ) ) ;
#74485 = CARTESIAN_POINT ( 'NONE',  ( 5.476650724650769853, 71.31612877608863243, -10.00000000000000000 ) ) ;
#74486 = CARTESIAN_POINT ( 'NONE',  ( 67.70878694032322187, 69.48726129358172443, -2.441691297528492566 ) ) ;
#74487 = LINE ( 'NONE', #43546, #55310 ) ;
#74488 = ORIENTED_EDGE ( 'NONE', *, *, #34307, .F. ) ;
#74489 = CARTESIAN_POINT ( 'NONE',  ( 182.5376139826708197, 283.9547259621338071, 16.22153700475692517 ) ) ;
#74490 = CARTESIAN_POINT ( 'NONE',  ( 191.4685399627163633, 299.0137560639802814, 7.545791216288330716 ) ) ;
#74491 = CARTESIAN_POINT ( 'NONE',  ( 159.8732321751776624, 253.7384344327741132, -15.51998349828054202 ) ) ;
#74492 = AXIS2_PLACEMENT_3D ( 'NONE', #11123, #73907, #66298 ) ;
#74493 = EDGE_LOOP ( 'NONE', ( #64403, #82857, #73138, #76388 ) ) ;
#74495 = DIRECTION ( 'NONE',  ( -0.000000000000000000, -0.000000000000000000, -1.000000000000000000 ) ) ;
#74494 = CARTESIAN_POINT ( 'NONE',  ( 161.8807657183444064, 250.2612843381103573, -13.52770735624900311 ) ) ;
#74496 = CARTESIAN_POINT ( 'NONE',  ( 181.4204268205617154, 259.5203828285251006, -11.17471347674236348 ) ) ;
#74497 = VERTEX_POINT ( 'NONE', #99916 ) ;
#74498 = CARTESIAN_POINT ( 'NONE',  ( 66.28959039141291498, 69.23996339252364862, -2.139077115682002983 ) ) ;
#74499 = CARTESIAN_POINT ( 'NONE',  ( 197.9552487813401456, 287.7784468162186613, 17.26493623863614602 ) ) ;
#74500 = DIRECTION ( 'NONE',  ( -0.8660254037844387076, -0.4999999999999998890, -0.000000000000000000 ) ) ;
#74501 = CARTESIAN_POINT ( 'NONE',  ( 78.32598375782600897, 61.10224562959768235, -15.90800848020992220 ) ) ;
#74502 = CARTESIAN_POINT ( 'NONE',  ( 125.6948669907937415, 249.5024278399160664, 9.188101187500095079 ) ) ;
#74503 = DIRECTION ( 'NONE',  ( -0.000000000000000000, -0.000000000000000000, 1.000000000000000000 ) ) ;
#74504 = LINE ( 'NONE', #42558, #86810 ) ;
#74505 = ORIENTED_EDGE ( 'NONE', *, *, #83747, .F. ) ;
#74506 = CARTESIAN_POINT ( 'NONE',  ( 163.7038023771459052, 247.1036922210055025, -6.448491958542482472 ) ) ;
#74507 = ORIENTED_EDGE ( 'NONE', *, *, #28717, .F. ) ;
#74508 = ORIENTED_EDGE ( 'NONE', *, *, #99046, .T. ) ;
#74509 = CARTESIAN_POINT ( 'NONE',  ( 198.3075590527773784, 287.1682275260610027, 16.94807365630277118 ) ) ;
#74510 = CARTESIAN_POINT ( 'NONE',  ( 170.3127733705114224, 263.9010670580030364, 17.23448983536806622 ) ) ;
#74511 = CARTESIAN_POINT ( 'NONE',  ( 67.50895872190925218, 209.7833772461660544, -9.188101187500095079 ) ) ;
#74512 = DIRECTION ( 'NONE',  ( -0.8660254037844387076, -0.4999999999999998890, -0.000000000000000000 ) ) ;
#74513 = DIRECTION ( 'NONE',  ( 0.000000000000000000, 0.000000000000000000, 1.000000000000000000 ) ) ;
#74514 = CARTESIAN_POINT ( 'NONE',  ( 80.55977923466276991, 44.53388773495298381, 11.41474457630165062 ) ) ;
#74515 = CARTESIAN_POINT ( 'NONE',  ( 175.8011943468589777, 278.1488512039077818, 16.59015806188801889 ) ) ;
#74516 = CARTESIAN_POINT ( 'NONE',  ( 87.57478309584621456, 45.08285526713720515, 6.924932389716528469 ) ) ;
#74517 = ORIENTED_EDGE ( 'NONE', *, *, #31039, .F. ) ;
#74518 = CARTESIAN_POINT ( 'NONE',  ( 72.36414345318156904, 63.72805025348669972, -13.64787615739589555 ) ) ;
#74519 = CARTESIAN_POINT ( 'NONE',  ( 86.82688353415350946, 43.55230325865861829, -2.297822768102545599 ) ) ;
#74520 = CARTESIAN_POINT ( 'NONE',  ( 201.1060504099706350, 282.3210983108598384, -18.18000168485860257 ) ) ;
#74521 = CARTESIAN_POINT ( 'NONE',  ( 203.3041373168503299, 278.5139001086923827, -16.61929732091214973 ) ) ;
#74522 = ORIENTED_EDGE ( 'NONE', *, *, #29949, .T. ) ;
#74523 = CARTESIAN_POINT ( 'NONE',  ( 86.70911053808110580, 46.89117940024963360, 10.21290512048939547 ) ) ;
#74524 = CARTESIAN_POINT ( 'NONE',  ( 76.10495001321383768, 51.13391335127094095, -16.08818559945424198 ) ) ;
#74525 = CARTESIAN_POINT ( 'NONE',  ( 174.0330057339203336, 253.5070743419241523, -7.570545654136764391 ) ) ;
#74526 = CARTESIAN_POINT ( 'NONE',  ( 165.7625844681755325, 272.7524946119172569, 16.99070308655728923 ) ) ;
#74527 = CARTESIAN_POINT ( 'NONE',  ( 164.7762319088960794, 245.2461897844768828, 2.994040459560653122 ) ) ;
#74528 = EDGE_CURVE ( 'NONE', #8947, #2862, #45681, .T. ) ;
#74529 = CARTESIAN_POINT ( 'NONE',  ( 196.2293283710122012, 290.7678286567270902, -17.07152402978540096 ) ) ;
#74530 = CARTESIAN_POINT ( 'NONE',  ( 45.19978347827786536, 190.2365022471902023, 10.00000000000009948 ) ) ;
#74531 = CARTESIAN_POINT ( 'NONE',  ( 208.0045976720423084, 270.3724639545367836, 2.002128742561712471 ) ) ;
#74532 = CARTESIAN_POINT ( 'NONE',  ( 135.5734031224162663, 239.8923013555409796, 4.594050593750050204 ) ) ;
#74533 = ORIENTED_EDGE ( 'NONE', *, *, #46625, .T. ) ;
#74534 = PLANE ( 'NONE',  #40005 ) ;
#74535 = CARTESIAN_POINT ( 'NONE',  ( 183.5087089432283278, 257.8196472444194569, 6.855898145921591968 ) ) ;
#74536 = EDGE_CURVE ( 'NONE', #94434, #98779, #39572, .T. ) ;
#74537 = CARTESIAN_POINT ( 'NONE',  ( 44.18794977381975286, 118.5901545549086791, -10.00000000000000000 ) ) ;
#74538 = CARTESIAN_POINT ( 'NONE',  ( 163.9587364689194260, 246.6621334214722481, 5.816126667419880825 ) ) ;
#74539 = CARTESIAN_POINT ( 'NONE',  ( 74.77989834281638082, 61.09922272559126100, 15.34499820422063010 ) ) ;
#74540 = LINE ( 'NONE', #98327, #3335 ) ;
#74541 = EDGE_LOOP ( 'NONE', ( #16407, #98420, #18195, #95217 ) ) ;
#74542 = CARTESIAN_POINT ( 'NONE',  ( 77.37106971737360084, 59.79005663912887059, 15.99722322042923928 ) ) ;
#74543 = CARTESIAN_POINT ( 'NONE',  ( 182.0998708099376131, 275.6965794993143390, -16.43372495111283627 ) ) ;
#74544 = DIRECTION ( 'NONE',  ( -0.3473448497826262527, 0.9377374661009790779, 0.000000000000000000 ) ) ;
#74545 = CARTESIAN_POINT ( 'NONE',  ( 36.81016237556819704, 185.3927522451417929, -10.00000000000009237 ) ) ;
#74546 = CARTESIAN_POINT ( 'NONE',  ( 202.5541353527785873, 267.6455170340615268, 0.8630784805652055303 ) ) ;
#74547 = EDGE_CURVE ( 'NONE', #29146, #88681, #93873, .T. ) ;
#74548 = CARTESIAN_POINT ( 'NONE',  ( 199.0384395528189430, 265.2940482796883543, 0.1310837649599854438 ) ) ;
#74549 = B_SPLINE_CURVE_WITH_KNOTS ( 'NONE', 3,
 ( #45325, #76259, #14444, #6344 ),
 .UNSPECIFIED., .F., .F.,
 ( 4, 4 ),
 ( 0.008293070909132364485, 0.01460849775743500514 ),
 .UNSPECIFIED. ) ;
#74550 = CARTESIAN_POINT ( 'NONE',  ( 190.4976253092930278, 300.6954295735222900, -5.764807383508308902 ) ) ;
#74551 = FACE_OUTER_BOUND ( 'NONE', #48034, .T. ) ;
#74552 = CARTESIAN_POINT ( 'NONE',  ( 204.7242223814549504, 276.0542406257275161, -13.93608974681376189 ) ) ;
#74553 = CARTESIAN_POINT ( 'NONE',  ( 196.3531155526046632, 270.6521786943779375, 11.87296120750966466 ) ) ;
#74554 = EDGE_CURVE ( 'NONE', #40233, #25756, #96687, .T. ) ;
#74555 = CARTESIAN_POINT ( 'NONE',  ( 16.27523747222386774, 28.13478043621388025, 8.090169943749478065 ) ) ;
#74556 = EDGE_CURVE ( 'NONE', #87380, #92014, #16298, .T. ) ;
#74557 = CARTESIAN_POINT ( 'NONE',  ( 190.0259678364800493, 301.5123642802043946, 4.004183174499006626 ) ) ;
#74558 = CARTESIAN_POINT ( 'NONE',  ( 205.0967303340277681, 274.5205728753008430, 11.66379712794152645 ) ) ;
#74559 = CARTESIAN_POINT ( 'NONE',  ( 26.50804481403195467, 15.70852965304480087, 1.583844403245364907 ) ) ;
#74560 = CYLINDRICAL_SURFACE ( 'NONE', #70578, 10.00000000000010658 ) ;
#74561 = CARTESIAN_POINT ( 'NONE',  ( 72.13721715224981779, 71.83272178494776483, -3.912550702485382281 ) ) ;
#74562 = CARTESIAN_POINT ( 'NONE',  ( 139.3620039403754731, 251.2677522451418497, 10.00000000000009592 ) ) ;
#74563 = CARTESIAN_POINT ( 'NONE',  ( 172.5346649401163290, 284.2238562735757910, -12.87557711212363110 ) ) ;
#74564 = ORIENTED_EDGE ( 'NONE', *, *, #6401, .F. ) ;
#74565 = CARTESIAN_POINT ( 'NONE',  ( -19.65312891409030271, 93.06504152958497400, 59.99999999999999289 ) ) ;
#74566 = CARTESIAN_POINT ( 'NONE',  ( 198.5511052797322975, 286.7463930869835167, -17.24711022262289006 ) ) ;
#74567 = CARTESIAN_POINT ( 'NONE',  ( -12.81524457486244550, 175.6589784336661637, -6.496448406907676862E-16 ) ) ;
#74568 = CARTESIAN_POINT ( 'NONE',  ( 56.08842225738448661, 197.0643266524160140, 9.188101187500095079 ) ) ;
#74569 = CARTESIAN_POINT ( 'NONE',  ( 176.0198054981916869, 257.3513611390321216, -10.51569790059619791 ) ) ;
#74570 = CARTESIAN_POINT ( 'NONE',  ( 19.47506710560450571, 33.01751292744055633, 6.180339887498949913 ) ) ;
#74571 = LINE ( 'NONE', #5149, #75628 ) ;
#74572 = CARTESIAN_POINT ( 'NONE',  ( 205.4029933437358295, 274.8785748323546159, -13.50815392427034922 ) ) ;
#74573 = CARTESIAN_POINT ( 'NONE',  ( 192.5606481657753761, 292.4750250043705933, -14.28755835911418082 ) ) ;
#74574 = CARTESIAN_POINT ( 'NONE',  ( 150.0363948880720102, 276.4654116368551513, 3.707458508793961993 ) ) ;
#74575 = EDGE_CURVE ( 'NONE', #79277, #86358, #16339, .T. ) ;
#74576 = CARTESIAN_POINT ( 'NONE',  ( 167.4736906045900184, 256.7023835675479972, 14.85217472785100945 ) ) ;
#74577 = CARTESIAN_POINT ( 'NONE',  ( 75.26053270681407525, 66.77963801587817727, 12.92466396265848871 ) ) ;
#74578 = CARTESIAN_POINT ( 'NONE',  ( 150.4319008355389542, 270.0913000041206260, 13.83804576328048697 ) ) ;
#74579 = ADVANCED_FACE ( 'NONE', ( #65398 ), #57289, .T. ) ;
#74580 = CARTESIAN_POINT ( 'NONE',  ( 65.04619898167126735, 198.3615022471901739, 5.000000000000051514 ) ) ;
#74581 = CARTESIAN_POINT ( 'NONE',  ( 181.9590579474959213, 291.6908273499842039, 9.324365134751094075 ) ) ;
#74582 = CARTESIAN_POINT ( 'NONE',  ( 202.6551236945213361, 279.6380246773706517, 15.55476940527561425 ) ) ;
#74583 = CARTESIAN_POINT ( 'NONE',  ( 13.16551753867071461, 190.6589784336661921, -6.496448406907675876E-16 ) ) ;
#74584 = CARTESIAN_POINT ( 'NONE',  ( 167.8811029522163096, 286.0887665112138052, 4.087334010221439939 ) ) ;
#74585 = CARTESIAN_POINT ( 'NONE',  ( 2.672015980952107572, 183.8967562850347122, -4.648177544792955347E-16 ) ) ;
#74586 = EDGE_CURVE ( 'NONE', #29855, #88281, #56160, .T. ) ;
#74587 = CARTESIAN_POINT ( 'NONE',  ( 44.43411998782967487, 26.44966523072497822, -2.296566073217252530E-15 ) ) ;
#74588 = CARTESIAN_POINT ( 'NONE',  ( 144.8954975894293682, 242.9155109091896065, 2.679491924311254714 ) ) ;
#74589 = CARTESIAN_POINT ( 'NONE',  ( 179.8745906151779081, 276.9455922838650395, 16.30155377088923885 ) ) ;
#74590 = EDGE_CURVE ( 'NONE', #71916, #32467, #51706, .T. ) ;
#74591 = CARTESIAN_POINT ( 'NONE',  ( 24.15577373785222193, 19.11029122506294797, -8.090169943749478065 ) ) ;
#74592 = CARTESIAN_POINT ( 'NONE',  ( 148.9776469710554920, 275.4404107866210438, 7.585097431987186667 ) ) ;
#74593 = B_SPLINE_CURVE_WITH_KNOTS ( 'NONE', 3,
 ( #40264, #56479, #1796, #33701, #95546, #24080, #54976, #85954, #32680, #39750, #1293, #32178 ),
 .UNSPECIFIED., .F., .F.,
 ( 4, 2, 2, 2, 2, 4 ),
 ( 0.001410800830378118077, 0.001612464706955823394, 0.001814128583533528927, 0.002217456336688934139, 0.002620784089844339568, 0.003024111842999744563 ),
 .UNSPECIFIED. ) ;
#74594 = B_SPLINE_CURVE_WITH_KNOTS ( 'NONE', 3,
 ( #8408, #47395, #77824, #9921 ),
 .UNSPECIFIED., .F., .F.,
 ( 4, 4 ),
 ( 0.007261002233767476638, 0.01303800565229685030 ),
 .UNSPECIFIED. ) ;
#74595 = CARTESIAN_POINT ( 'NONE',  ( 176.7509313491396483, 260.7307399239896313, -13.19623395499003848 ) ) ;
#74596 = APPLICATION_PROTOCOL_DEFINITION ( 'draft international standard', 'automotive_design', 1998, #65412 ) ;
#74597 = CARTESIAN_POINT ( 'NONE',  ( 11.61360469066603507, 28.74646525600389069, 2.839279412974139660 ) ) ;
#74598 = CARTESIAN_POINT ( 'NONE',  ( 71.92952260767447115, 72.55458961131337503, 1.705568256100836066 ) ) ;
#74599 = DIRECTION ( 'NONE',  ( 0.000000000000000000, 0.000000000000000000, -1.000000000000000000 ) ) ;
#74600 = CARTESIAN_POINT ( 'NONE',  ( 159.5946725794669021, 258.6821552202987391, 17.29432174323186189 ) ) ;
#74601 = EDGE_CURVE ( 'NONE', #76651, #69911, #59819, .T. ) ;
#74602 = CARTESIAN_POINT ( 'NONE',  ( 193.7275870247597425, 295.1009717758319084, 14.48058678254265885 ) ) ;
#74603 = ORIENTED_EDGE ( 'NONE', *, *, #78197, .F. ) ;
#74604 = CARTESIAN_POINT ( 'NONE',  ( 181.5287477823910365, 289.3008137216033333, 12.67257242005390161 ) ) ;
#74605 = CARTESIAN_POINT ( 'NONE',  ( 16.56913029798217352, 168.8262482093458061, 3.021315404115420679E-15 ) ) ;
#74606 = EDGE_CURVE ( 'NONE', #30217, #49074, #94982, .T. ) ;
#74607 = CARTESIAN_POINT ( 'NONE',  ( 81.10605299805037305, 42.47174888764966738, 7.802073681796036553 ) ) ;
#74608 = CARTESIAN_POINT ( 'NONE',  ( 169.5608527833963421, 251.6396950762901952, -9.960993533446050208 ) ) ;
#74609 = ORIENTED_EDGE ( 'NONE', *, *, #98839, .T. ) ;
#74610 = CARTESIAN_POINT ( 'NONE',  ( 196.3934922554618936, 290.0189000700918314, -16.29075131761187478 ) ) ;
#74611 = LINE ( 'NONE', #59862, #54641 ) ;
#74612 = CARTESIAN_POINT ( 'NONE',  ( 66.77373092297933965, 68.40140739384713697, 4.464727344145090981 ) ) ;
#74613 = CARTESIAN_POINT ( 'NONE',  ( 203.2369479875374623, 278.6302754407888074, -16.66242713208754367 ) ) ;
#74614 = VERTEX_POINT ( 'NONE', #58773 ) ;
#74615 = ORIENTED_EDGE ( 'NONE', *, *, #23716, .T. ) ;
#74617 = CARTESIAN_POINT ( 'NONE',  ( 163.8990931530087494, 246.7654386749614162, 5.873176884778091633 ) ) ;
#74616 = CARTESIAN_POINT ( 'NONE',  ( 21.15788363470973366, 37.74176219324818504, -10.00000000000000000 ) ) ;
#74618 = CARTESIAN_POINT ( 'NONE',  ( 153.4389798490260262, 264.8828863703868137, 16.68923469758090761 ) ) ;
#74619 = ORIENTED_EDGE ( 'NONE', *, *, #6227, .F. ) ;
#74620 = CARTESIAN_POINT ( 'NONE',  ( 150.6431064791187850, 269.7254810985950257, 15.11064854015152470 ) ) ;
#74621 = CARTESIAN_POINT ( 'NONE',  ( 80.19807517511665651, 58.11859141470634427, 16.26539701942824578 ) ) ;
#74622 = CARTESIAN_POINT ( 'NONE',  ( 176.7010738378296253, 263.4434962957928406, 14.45361317776263910 ) ) ;
#74623 = ORIENTED_EDGE ( 'NONE', *, *, #16964, .T. ) ;
#74624 = CARTESIAN_POINT ( 'NONE',  ( -36.26652983198114555, 26.35523046909639788, 10.00000000000000000 ) ) ;
#74625 = CARTESIAN_POINT ( 'NONE',  ( 80.74266887835153739, 43.44699442419332769, 9.418154823084309513 ) ) ;
#74626 = VERTEX_POINT ( 'NONE', #67385 ) ;
#74627 = CARTESIAN_POINT ( 'NONE',  ( 206.5479446040613141, 272.8954610772809133, 10.74757481123993230 ) ) ;
#74628 = DIRECTION ( 'NONE',  ( 0.4999999999999992784, -0.8660254037844390407, 0.000000000000000000 ) ) ;
#74629 = ORIENTED_EDGE ( 'NONE', *, *, #15630, .T. ) ;
#74630 = CARTESIAN_POINT ( 'NONE',  ( 177.6723615241578216, 279.4491075471210593, -16.59050672443976282 ) ) ;
#74631 = CARTESIAN_POINT ( 'NONE',  ( 168.9826911834654481, 261.4415967181243445, -16.13406239319744984 ) ) ;
#74632 = ORIENTED_EDGE ( 'NONE', *, *, #54003, .T. ) ;
#74633 = PLANE ( 'NONE',  #88775 ) ;
#74634 = CARTESIAN_POINT ( 'NONE',  ( 146.8153075009282134, 276.3554234099810287, -4.113808735271278216 ) ) ;
#74635 = ORIENTED_EDGE ( 'NONE', *, *, #23514, .T. ) ;
#74636 = CARTESIAN_POINT ( 'NONE',  ( 157.4146825304236188, 269.0645323469553318, 15.58493267419004624 ) ) ;
#74637 = CIRCLE ( 'NONE', #30918, 70.00000000000001421 ) ;
#74638 = VERTEX_POINT ( 'NONE', #98312 ) ;
#74639 = CARTESIAN_POINT ( 'NONE',  ( 79.09745926769026880, 51.74933575859580515, -15.81631569581207941 ) ) ;
#74640 = CARTESIAN_POINT ( 'NONE',  ( 169.0638155539396905, 272.3808001447700917, 16.48807445323233623 ) ) ;
#74641 = CARTESIAN_POINT ( 'NONE',  ( 147.3154503175461514, 275.4891506405583073, 3.671329888160011823 ) ) ;
#74642 = CARTESIAN_POINT ( 'NONE',  ( 188.5163790307635168, 298.7479289875233235, -5.009957144413234253 ) ) ;
#74643 = CARTESIAN_POINT ( 'NONE',  ( 190.0340467409721441, 301.4983712071542641, 4.077645795029533282 ) ) ;
#74644 = CARTESIAN_POINT ( 'NONE',  ( 192.5049767439991513, 297.2185948999652965, 12.57567268027295881 ) ) ;
#74645 = CARTESIAN_POINT ( 'NONE',  ( 178.4788175059835567, 291.5611646558071470, 6.106669723458193033 ) ) ;
#74646 = CARTESIAN_POINT ( 'NONE',  ( 191.7934382699952494, 298.4510156884799699, -8.680100145728863126 ) ) ;
#74647 = ORIENTED_EDGE ( 'NONE', *, *, #75166, .F. ) ;
#74648 = CARTESIAN_POINT ( 'NONE',  ( 78.69766452942040758, 56.36335943523778269, -16.19347606039230669 ) ) ;
#74649 = CARTESIAN_POINT ( 'NONE',  ( 39.85783382567782951, 23.41603393254329291, -1.583844403245396437 ) ) ;
#74650 = CARTESIAN_POINT ( 'NONE',  ( 164.9171241593586217, 245.0021572482830550, 1.622680932994367220 ) ) ;
#74651 = CARTESIAN_POINT ( 'NONE',  ( 159.6898930778639283, 254.0559870643349143, 16.90891900388599822 ) ) ;
#74652 = CARTESIAN_POINT ( 'NONE',  ( 171.5288823711526334, 289.0286466264677756, 4.266081008705642219 ) ) ;
#74653 = CARTESIAN_POINT ( 'NONE',  ( 35.39012114306879653, 16.59285393851897084, -10.00000000000000000 ) ) ;
#74654 = EDGE_LOOP ( 'NONE', ( #96122, #73977, #95976, #52399 ) ) ;
#74655 = CARTESIAN_POINT ( 'NONE',  ( 71.88093039901364989, 69.29925688614676460, 8.664886389715691806 ) ) ;
#74656 = CARTESIAN_POINT ( 'NONE',  ( 202.7310286658811265, 277.6365180286925352, 15.39425154460195699 ) ) ;
#74657 = CARTESIAN_POINT ( 'NONE',  ( 126.3716228836089215, 233.7677522451417929, -5.000000000000041744 ) ) ;
#74658 = B_SPLINE_CURVE_WITH_KNOTS ( 'NONE', 3,
 ( #20146, #81968, #36315, #4427, #13541, #73837, #67219, #82967, #5924, #35323, #43913, #12544, #74852, #43417, #5433, #97654, #98144, #75343, #67726, #29233, #60100, #33674, #56455, #10873, #10372, #66058, #35149, #97008, #96010, #87447, #42244, #64063, #88936, #11877, #64569, #72181, #18986, #34168, #3772, #18475, #19497, #41750, #73180, #34652, #11391, #65553, #96501, #65060, #95526, #27070 ),
 .UNSPECIFIED., .F., .F.,
 ( 4, 2, 2, 2, 2, 2, 2, 2, 2, 2, 2, 2, 2, 2, 2, 2, 2, 2, 2, 2, 2, 2, 2, 2, 4 ),
 ( 0.0003971087438474241605, 0.0008548896376937187465, 0.001083780084616804565, 0.001312670531539890384, 0.001427115755001357074, 0.001541560978462823764, 0.001656006201924290454, 0.001770451425385757144, 0.001999341872308679248, 0.002228232319231601352, 0.003143794106923289769, 0.004059355894614978186, 0.004974917682306666603, 0.005432698576152548975, 0.005661589023075452864, 0.005776034246536909146, 0.005833256858267558791, 0.005890479469998209303, 0.005947702081728858947, 0.006004924693459509459, 0.006119369916920820891, 0.006348260363843550441, 0.006806041257688862089, 0.007263822151534174605, 0.007721603045379487121 ),
 .UNSPECIFIED. ) ;
#74659 = CARTESIAN_POINT ( 'NONE',  ( 199.4147421703242173, 285.2505301131875513, -17.63954444317369763 ) ) ;
#74660 = CARTESIAN_POINT ( 'NONE',  ( 101.4192659406176915, 219.3615022471902023, 5.000000000000051514 ) ) ;
#74661 = ORIENTED_EDGE ( 'NONE', *, *, #12679, .T. ) ;
#74662 = CARTESIAN_POINT ( 'NONE',  ( 162.9111474110223412, 248.4766108952035211, -9.702990628959184960 ) ) ;
#74663 = CARTESIAN_POINT ( 'NONE',  ( 188.3784916956350344, 286.3721210266486992, -16.81851773412965301 ) ) ;
#74664 = CARTESIAN_POINT ( 'NONE',  ( 152.7691010214056462, 266.0431505347400503, -16.40662330462167162 ) ) ;
#74665 = CARTESIAN_POINT ( 'NONE',  ( 207.4764081617721843, 271.2873150223495600, 6.359972247200924578 ) ) ;
#74666 = CARTESIAN_POINT ( 'NONE',  ( 28.14990833772381151, 180.3927522451418213, 10.00000000000009592 ) ) ;
#74667 = CARTESIAN_POINT ( 'NONE',  ( 116.3854409958760385, 231.8768266524159856, -9.188101187500093303 ) ) ;
#74668 = EDGE_CURVE ( 'NONE', #43732, #32399, #36984, .T. ) ;
#74669 = CARTESIAN_POINT ( 'NONE',  ( 183.7317734547368673, 297.0731768695540040, -2.820923390534820996 ) ) ;
#74670 = CARTESIAN_POINT ( 'NONE',  ( 164.5864525486781531, 281.0963845696900307, -11.76674143703315600 ) ) ;
#74671 = CARTESIAN_POINT ( 'NONE',  ( 96.65612621980318409, 236.6115022471902876, -5.000000000000047962 ) ) ;
#74672 = CARTESIAN_POINT ( 'NONE',  ( 208.1583869480885483, 270.1060931147653719, 3.025867354224990979 ) ) ;
#74673 = CARTESIAN_POINT ( 'NONE',  ( 44.31597619863101301, 187.2048013555409796, 4.594050593750051981 ) ) ;
#74674 = CARTESIAN_POINT ( 'NONE',  ( 82.66777534753497036, 40.88273136530058594, 3.288167606880417981 ) ) ;
#74676 = VERTEX_POINT ( 'NONE', #44570 ) ;
#74675 = B_SPLINE_CURVE_WITH_KNOTS ( 'NONE', 3,
 ( #25922, #41590, #87780, #3620, #80650, #26412, #89745, #89266, #64406, #57290, #11227, #42094, #80148, #10714, #33510, #34497, #26908, #81150, #73511, #34987, #20310, #51182, #65890, #96844, #50684, #12719, #67895, #90243, #91221, #21788, #37471, #14196, #75012, #99801, #68381, #98818, #92241, #29396, #53669, #36986 ),
 .UNSPECIFIED., .F., .F.,
 ( 4, 2, 2, 2, 2, 2, 2, 2, 2, 2, 2, 2, 2, 2, 2, 2, 2, 2, 2, 4 ),
 ( 0.0009206193881831178276, 0.001016370969008163153, 0.001112122549833208371, 0.001303625711483349329, 0.001495128873133490504, 0.001686632034783631679, 0.002452644681384161685, 0.003984669974585218662, 0.004750682621185713106, 0.005133688944485916526, 0.005325192106135940608, 0.005420943686960917086, 0.005516695267785893565, 0.005564571058198422571, 0.005612446848610951576, 0.005708198429435867340, 0.005899701591085861063, 0.006282707914385812081, 0.006665714237685763099, 0.007048720560985714118 ),
 .UNSPECIFIED. ) ;
#74677 = FACE_OUTER_BOUND ( 'NONE', #44680, .T. ) ;
#74678 = CARTESIAN_POINT ( 'NONE',  ( 74.09798493915437234, 67.86634104065885253, -11.62737576625272418 ) ) ;
#74679 = ADVANCED_FACE ( 'NONE', ( #35982 ), #90746, .F. ) ;
#74680 = CARTESIAN_POINT ( 'NONE',  ( -22.42236680055709641, 157.8615022471902591, 0.000000000000000000 ) ) ;
#74681 = EDGE_CURVE ( 'NONE', #90285, #100061, #27428, .T. ) ;
#74682 = CARTESIAN_POINT ( 'NONE',  ( 147.1249913145849177, 275.8190353104462815, 3.637773609013635223 ) ) ;
#74683 = CARTESIAN_POINT ( 'NONE',  ( 81.65711888479437164, 41.53726941426280206, -5.387001511484587724 ) ) ;
#74684 = CARTESIAN_POINT ( 'NONE',  ( 207.8575108622103755, 270.6272257822888037, -6.381720258959569847 ) ) ;
#74685 = CARTESIAN_POINT ( 'NONE',  ( 68.07728789491679322, 200.1115022471901739, -5.000000000000041744 ) ) ;
#74686 = DIRECTION ( 'NONE',  ( 0.000000000000000000, 0.000000000000000000, 1.000000000000000000 ) ) ;
#74687 = CARTESIAN_POINT ( 'NONE',  ( 92.16361943412358926, 214.0177522451417929, 5.000000000000051514 ) ) ;
#74688 = ORIENTED_EDGE ( 'NONE', *, *, #4337, .T. ) ;
#74689 = CARTESIAN_POINT ( 'NONE',  ( 198.1704809733372770, 267.8414693299324654, -7.977924972520448854 ) ) ;
#74690 = CARTESIAN_POINT ( 'NONE',  ( 158.7268290693951087, 282.0671554313083789, -1.622909239661974423 ) ) ;
#74691 = CARTESIAN_POINT ( 'NONE',  ( 207.9328781051891042, 270.4966858882232259, -0.8820402142964423042 ) ) ;
#74692 = CARTESIAN_POINT ( 'NONE',  ( 10.35128207213630169, 176.7833772461660544, -9.188101187500095079 ) ) ;
#74693 = CARTESIAN_POINT ( 'NONE',  ( 3.124773676633713748, 24.73705186507751463, -3.090169943749475845 ) ) ;
#74694 = CARTESIAN_POINT ( 'NONE',  ( -69.42519150082246426, 45.64199051378594874, 10.00000000000000000 ) ) ;
#74695 = FACE_OUTER_BOUND ( 'NONE', #19928, .T. ) ;
#74696 = CARTESIAN_POINT ( 'NONE',  ( 73.63435323750927353, 69.71791780730768551, 10.06421556446032461 ) ) ;
#74697 = CARTESIAN_POINT ( 'NONE',  ( 53.21953955946602122, 201.5333772461660544, 9.188101187500095079 ) ) ;
#74698 = CARTESIAN_POINT ( 'NONE',  ( 207.5230514910949182, 271.2065264061283756, 2.678931747975364708 ) ) ;
#74699 = CARTESIAN_POINT ( 'NONE',  ( 204.8762144138505903, 275.7909827032724479, 14.60855957933206817 ) ) ;
#74700 = CARTESIAN_POINT ( 'NONE',  ( 68.57836030477737665, 67.22337045858328963, 8.752937159126823019 ) ) ;
#74701 = CARTESIAN_POINT ( 'NONE',  ( 66.11933821713674320, 68.48733517449421981, -4.787403750998837637 ) ) ;
#74702 = VERTEX_POINT ( 'NONE', #83126 ) ;
#74703 = AXIS2_PLACEMENT_3D ( 'NONE', #26617, #34215, #65110 ) ;
#74704 = EDGE_CURVE ( 'NONE', #78719, #96205, #28385, .T. ) ;
#74705 = CARTESIAN_POINT ( 'NONE',  ( -13.11024591527734628, 15.00000000000000000, 25.00000000000000000 ) ) ;
#74706 = CARTESIAN_POINT ( 'NONE',  ( 12.14648056717172686, 184.4865022471903444, -10.00000000000009415 ) ) ;
#74707 = CARTESIAN_POINT ( 'NONE',  ( 84.80475637890920382, 46.66516897523420937, 11.11621779752075945 ) ) ;
#74708 = CARTESIAN_POINT ( 'NONE',  ( 147.5084024922618084, 243.7202760586659736, -5.415160957724236172E-17 ) ) ;
#74709 = CARTESIAN_POINT ( 'NONE',  ( 32.30976433484754295, 19.44966523072496045, -2.296566073217252530E-15 ) ) ;
#74710 = CARTESIAN_POINT ( 'NONE',  ( 164.4444695124895475, 245.8208191110937548, 1.054989284641946412 ) ) ;
#74711 = CARTESIAN_POINT ( 'NONE',  ( 83.42542119994750749, 51.64995580955420706, -14.90072893730332027 ) ) ;
#74712 = LINE ( 'NONE', #37656, #52974 ) ;
#74714 = CARTESIAN_POINT ( 'NONE',  ( 74.99160476570628475, 67.13646269190913074, 13.03024426091169019 ) ) ;
#74713 = CARTESIAN_POINT ( 'NONE',  ( 23.64814127513158937, 118.0650415295850451, 20.00000000000000355 ) ) ;
#74715 = EDGE_CURVE ( 'NONE', #81514, #14058, #6090, .T. ) ;
#74716 = CARTESIAN_POINT ( 'NONE',  ( 68.43300413790026937, 64.44848761198993259, 12.21846621112735853 ) ) ;
#74717 = ORIENTED_EDGE ( 'NONE', *, *, #81928, .F. ) ;
#74718 = CARTESIAN_POINT ( 'NONE',  ( 159.0543278146147088, 283.1686167836548975, 1.246070035154647204 ) ) ;
#74719 = CARTESIAN_POINT ( 'NONE',  ( 208.0240523230475276, 270.3387675105520884, -1.833813267351394494 ) ) ;
#74720 = CARTESIAN_POINT ( 'NONE',  ( 173.9987591681438914, 277.1956714198441887, 17.06944903275143588 ) ) ;
#74721 = DIRECTION ( 'NONE',  ( 0.5000000000000014433, -0.8660254037844378194, 0.000000000000000000 ) ) ;
#74722 = CARTESIAN_POINT ( 'NONE',  ( 12.70933400901951416, 9.198606405272903075, 2.839279412974134775 ) ) ;
#74723 = VERTEX_POINT ( 'NONE', #35492 ) ;
#74724 = CARTESIAN_POINT ( 'NONE',  ( 70.64415969017909447, 69.81928975612606791, 6.580201901691414612 ) ) ;
#74725 = CARTESIAN_POINT ( 'NONE',  ( 83.67528194178203194, 41.54745686406482008, -3.633279836990721989 ) ) ;
#74726 = ADVANCED_FACE ( 'NONE', ( #66395 ), #97323, .T. ) ;
#74727 = CARTESIAN_POINT ( 'NONE',  ( 84.53232711715837411, 43.64540581557137955, 6.477393172473421501 ) ) ;
#74728 = CARTESIAN_POINT ( 'NONE',  ( 196.2046261908255929, 270.9293328135447041, 13.03164479674023291 ) ) ;
#74729 = CARTESIAN_POINT ( 'NONE',  ( 182.4644955539734497, 295.0573375002295506, 4.739987455525070281 ) ) ;
#74730 = CARTESIAN_POINT ( 'NONE',  ( 68.54312381459287451, 69.80873064283493079, 3.292911436909311096 ) ) ;
#74731 = CARTESIAN_POINT ( 'NONE',  ( 148.6717005876752182, 274.8950821652439345, -7.961084883142776292 ) ) ;
#74732 = CARTESIAN_POINT ( 'NONE',  ( 72.58111491857235364, 57.29791513365444189, -16.33754921798919213 ) ) ;
#74733 = DIRECTION ( 'NONE',  ( -0.9302793824855948301, 0.3668518372888711077, 0.000000000000000000 ) ) ;
#74734 = CARTESIAN_POINT ( 'NONE',  ( 19.05068821614581864, 13.12755873383625449, -6.180339887498949025 ) ) ;
#74735 = CARTESIAN_POINT ( 'NONE',  ( 82.09686517919956827, 43.36415878988843531, 9.196185934937616935 ) ) ;
#74736 = ORIENTED_EDGE ( 'NONE', *, *, #76532, .F. ) ;
#74737 = CARTESIAN_POINT ( 'NONE',  ( 74.09260619880180343, 55.08812674012290245, 16.60422476838407846 ) ) ;
#74738 = CARTESIAN_POINT ( 'NONE',  ( 86.30773806088525646, 46.95517243064260526, -10.53307507464018755 ) ) ;
#74739 = PLANE ( 'NONE',  #53203 ) ;
#74740 = EDGE_LOOP ( 'NONE', ( #61717, #50935, #27453, #23367 ) ) ;
#74741 = CARTESIAN_POINT ( 'NONE',  ( -169.5327448629461742, 46.94652375874896677, -30.52142883766498116 ) ) ;
#74742 = CARTESIAN_POINT ( 'NONE',  ( 204.7817976169119163, 273.0227149632294754, -9.758020631165562619 ) ) ;
#74743 = CARTESIAN_POINT ( 'NONE',  ( 164.0741338217690668, 246.4622593432776796, 7.359073626423302983 ) ) ;
#74744 = CARTESIAN_POINT ( 'NONE',  ( 53.78786873247351252, 201.8615022471902307, -10.00000000000009592 ) ) ;
#74745 = ORIENTED_EDGE ( 'NONE', *, *, #21336, .T. ) ;
#74746 = CARTESIAN_POINT ( 'NONE',  ( 82.58295308470839302, 227.6744531367911293, 4.594050593750047540 ) ) ;
#74747 = CARTESIAN_POINT ( 'NONE',  ( 155.3983691713044664, 261.4891245123925501, 17.00489288030859569 ) ) ;
#74748 = CARTESIAN_POINT ( 'NONE',  ( 147.7917198021585534, 275.6304213403500398, -3.790807063116589770 ) ) ;
#74749 = CARTESIAN_POINT ( 'NONE',  ( 185.0693321002852372, 259.9792428912778064, -5.919411351415631906 ) ) ;
#74750 = ORIENTED_EDGE ( 'NONE', *, *, #66566, .T. ) ;
#74751 = VERTEX_POINT ( 'NONE', #51181 ) ;
#74752 = CARTESIAN_POINT ( 'NONE',  ( 207.3719924741569400, 270.9203590968859316, 1.937085497212718943 ) ) ;
#74753 = VERTEX_POINT ( 'NONE', #12718 ) ;
#74754 = CARTESIAN_POINT ( 'NONE',  ( 80.52412688334953828, 46.96905098241762744, 12.74129133586520091 ) ) ;
#74755 = ORIENTED_EDGE ( 'NONE', *, *, #26886, .F. ) ;
#74756 = CARTESIAN_POINT ( 'NONE',  ( 75.08869305417201190, 59.14893459762363648, 15.81684554694788503 ) ) ;
#74757 = CARTESIAN_POINT ( 'NONE',  ( 203.1526193585190470, 278.7763369107815379, -16.67658907091021447 ) ) ;
#74758 = ORIENTED_EDGE ( 'NONE', *, *, #47342, .F. ) ;
#74759 = FACE_OUTER_BOUND ( 'NONE', #93561, .T. ) ;
#74760 = CARTESIAN_POINT ( 'NONE',  ( 82.41914487369291464, 41.31337197830497132, 3.340431838514233753 ) ) ;
#74761 = B_SPLINE_CURVE_WITH_KNOTS ( 'NONE', 3,
 ( #13405, #74720, #52873, #60966 ),
 .UNSPECIFIED., .F., .F.,
 ( 4, 4 ),
 ( 0.008890319171618900340, 0.01510497574151875924 ),
 .UNSPECIFIED. ) ;
#74763 = EDGE_CURVE ( 'NONE', #27651, #85116, #79184, .T. ) ;
#74762 = LINE ( 'NONE', #28130, #67301 ) ;
#74764 = CARTESIAN_POINT ( 'NONE',  ( 10.35021921122761945, 188.3297689869269789, -2.679491924311252493 ) ) ;
#74765 = CARTESIAN_POINT ( 'NONE',  ( 76.61888230025124358, 51.35972145274618583, 16.07233720520855158 ) ) ;
#74766 = CARTESIAN_POINT ( 'NONE',  ( 157.0064891765866832, 258.7037789585758105, -18.42258229807105963 ) ) ;
#74767 = ORIENTED_EDGE ( 'NONE', *, *, #78116, .T. ) ;
#74768 = CARTESIAN_POINT ( 'NONE',  ( 76.07649505321222705, 56.58890100330362571, 16.14652101205965806 ) ) ;
#74769 = CARTESIAN_POINT ( 'NONE',  ( 11.83670304002995266, 9.760047579820874120, 5.678558825948272215 ) ) ;
#74770 = VERTEX_POINT ( 'NONE', #64223 ) ;
#74771 = CARTESIAN_POINT ( 'NONE',  ( 166.1232698191040527, 284.0209118141528961, 9.548314520813702799 ) ) ;
#74773 = ORIENTED_EDGE ( 'NONE', *, *, #77997, .T. ) ;
#74772 = CARTESIAN_POINT ( 'NONE',  ( 199.9280821859048274, 270.2386370741994597, 9.410868133784870082 ) ) ;
#74774 = CARTESIAN_POINT ( 'NONE',  ( 163.2442700311756596, 247.8996255919473697, 11.14021925110252020 ) ) ;
#74775 = CARTESIAN_POINT ( 'NONE',  ( 159.9770824720811220, 253.5585604421560788, -16.42166711341322483 ) ) ;
#74776 = CARTESIAN_POINT ( 'NONE',  ( 161.3512806983480914, 281.4835825935907110, -6.508326206231584976 ) ) ;
#74777 = CARTESIAN_POINT ( 'NONE',  ( 164.8310825586143835, 246.4510164509542847, -1.875124838255799675 ) ) ;
#74778 =( BOUNDED_CURVE ( )  B_SPLINE_CURVE ( 2, ( #99838, #92274, #34, #92755, #30423, #38000, #14724, #16222, #62812 ),
 .UNSPECIFIED., .F., .T. ) 
 B_SPLINE_CURVE_WITH_KNOTS ( ( 3, 2, 2, 2, 3 ),
 ( 0.5604838709677418818, 0.5618279569892472569, 0.5645161290322581182, 0.5672043010752688685, 0.5685483870967742437 ),
 .UNSPECIFIED. ) 
 CURVE ( )  GEOMETRIC_REPRESENTATION_ITEM ( )  RATIONAL_B_SPLINE_CURVE ( ( 0.9330127018922194093, 0.9330127018922194093, 1.000000000000000000, 0.8660254037844387076, 1.000000000000000000, 0.8660254037844387076, 1.000000000000000000, 0.9330127018922194093, 0.9330127018922194093 ) ) 
 REPRESENTATION_ITEM ( '' )  );
#74779 = LINE ( 'NONE', #4872, #81956 ) ;
#74780 = CARTESIAN_POINT ( 'NONE',  ( 168.0664690830419659, 253.0840726306553563, 11.72824221947031731 ) ) ;
#74781 = FACE_OUTER_BOUND ( 'NONE', #55391, .T. ) ;
#74782 = ORIENTED_EDGE ( 'NONE', *, *, #34079, .F. ) ;
#74783 = LINE ( 'NONE', #43844, #78528 ) ;
#74784 = CARTESIAN_POINT ( 'NONE',  ( 73.65583987803587718, 62.70152398185310716, -14.53858387021961107 ) ) ;
#74785 = ORIENTED_EDGE ( 'NONE', *, *, #84398, .T. ) ;
#74786 = CARTESIAN_POINT ( 'NONE',  ( 160.0562591974253337, 276.7040562812561006, 12.99130222948419267 ) ) ;
#74787 = EDGE_CURVE ( 'NONE', #47085, #85740, #48534, .T. ) ;
#74788 = B_SPLINE_CURVE_WITH_KNOTS ( 'NONE', 3,
 ( #46312, #38212, #61019, #53913 ),
 .UNSPECIFIED., .F., .F.,
 ( 4, 4 ),
 ( 0.01381869335794279167, 0.02017999936437927730 ),
 .UNSPECIFIED. ) ;
#74789 = CARTESIAN_POINT ( 'NONE',  ( 171.3497015292133199, 279.8280180079489696, -15.00511433428560437 ) ) ;
#74790 = CARTESIAN_POINT ( 'NONE',  ( 194.1260014150849145, 282.7392756228211397, -17.82763711395031692 ) ) ;
#74791 = CARTESIAN_POINT ( 'NONE',  ( 83.95136718548498322, 44.65165793737095612, -8.662646615273729367 ) ) ;
#74792 = CARTESIAN_POINT ( 'NONE',  ( 164.7277326422747024, 274.2652274994892423, 16.02158536651776188 ) ) ;
#74794 = CARTESIAN_POINT ( 'NONE',  ( 88.25905654664580879, 44.35750191947202126, 2.523739344444579480 ) ) ;
#74793 = CARTESIAN_POINT ( 'NONE',  ( -11.70556275232237908, 173.2369531367911293, -4.594050593750048428 ) ) ;
#74795 = FACE_OUTER_BOUND ( 'NONE', #27623, .T. ) ;
#74796 = VERTEX_POINT ( 'NONE', #18131 ) ;
#74797 = VERTEX_POINT ( 'NONE', #17633 ) ;
#74798 = LINE ( 'NONE', #82912, #56516 ) ;
#74799 = CARTESIAN_POINT ( 'NONE',  ( 80.37423141194477694, 58.00578747994902074, 16.25890986437170938 ) ) ;
#74800 = EDGE_CURVE ( 'NONE', #5467, #31605, #89096, .T. ) ;
#74801 = CARTESIAN_POINT ( 'NONE',  ( 85.55579313808955533, 48.95319673495580304, -12.20343581778852915 ) ) ;
#74802 = CARTESIAN_POINT ( 'NONE',  ( 175.5603300037018073, 290.9356092034950620, 2.583691617998545187 ) ) ;
#74803 = FACE_OUTER_BOUND ( 'NONE', #51793, .T. ) ;
#74804 = ADVANCED_FACE ( 'NONE', ( #40899 ), #2958, .F. ) ;
#74805 = CARTESIAN_POINT ( 'NONE',  ( 69.50667547386485978, 68.39943198049301998, 8.745776950494660085 ) ) ;
#74806 = CARTESIAN_POINT ( 'NONE',  ( 44.18942050719596182, 202.9865022471903160, 10.00000000000009415 ) ) ;
#74807 = CARTESIAN_POINT ( 'NONE',  ( -4.696256414383327638, 180.3464784336661637, 1.353441290958777525E-15 ) ) ;
#74808 = CARTESIAN_POINT ( 'NONE',  ( 104.0717290597573026, 221.7048013555409796, 4.594050593750051981 ) ) ;
#74809 = CARTESIAN_POINT ( 'NONE',  ( 87.81919554331292943, 44.17710153608190637, -4.445631852975253651 ) ) ;
#74810 = CARTESIAN_POINT ( 'NONE',  ( 181.6546199514925206, 256.8291319412630855, -2.317892941361705095 ) ) ;
#74811 = CARTESIAN_POINT ( 'NONE',  ( 79.03035308903145051, 56.41680147193460471, 16.17228969028650454 ) ) ;
#74812 = CARTESIAN_POINT ( 'NONE',  ( 178.0467244306524890, 283.8085580107421038, -15.17727061845414660 ) ) ;
#74813 = CIRCLE ( 'NONE', #34292, 17.82106496071138224 ) ;
#74814 = CARTESIAN_POINT ( 'NONE',  ( 79.11408761357685648, 53.92110988754666323, -15.85693396780485642 ) ) ;
#74815 = DIRECTION ( 'NONE',  ( 0.3940053768033583426, -0.6824373310787393843, 0.6156614753256619554 ) ) ;
#74816 = CARTESIAN_POINT ( 'NONE',  ( 180.4555112726659445, 273.0096557832494568, 16.95796759167777523 ) ) ;
#74817 = CARTESIAN_POINT ( 'NONE',  ( 194.6782745185928434, 293.4543327343926080, -14.56555309295305634 ) ) ;
#74818 = CARTESIAN_POINT ( 'NONE',  ( 84.73763152763326900, 50.49395269109753315, 13.54719052834833093 ) ) ;
#74819 = CARTESIAN_POINT ( 'NONE',  ( 186.7579786969028817, 299.0471994399743494, -0.6060533366661751131 ) ) ;
#74820 = CARTESIAN_POINT ( 'NONE',  ( 168.8563211758018099, 286.0187424789903048, -9.056861680415359217 ) ) ;
#74821 = CARTESIAN_POINT ( 'NONE',  ( 184.3926338455641769, 268.4995540244821655, -15.66566532612987217 ) ) ;
#74822 = CARTESIAN_POINT ( 'NONE',  ( 27.58098951138967436, 43.10352854649765675, -10.00000000000000000 ) ) ;
#74823 = EDGE_CURVE ( 'NONE', #44698, #12428, #50509, .T. ) ;
#74824 = CARTESIAN_POINT ( 'NONE',  ( 172.8992021874003342, 262.9442772269209740, -15.72255003995701195 ) ) ;
#74825 = CARTESIAN_POINT ( 'NONE',  ( 88.29356841273579448, 221.7833772461660544, -9.188101187500095079 ) ) ;
#74826 = CARTESIAN_POINT ( 'NONE',  ( 6.569006713621681648, 25.83396525600388216, -2.839279412974133887 ) ) ;
#74827 = DIRECTION ( 'NONE',  ( -0.4999999999999987788, 0.8660254037844392627, 0.000000000000000000 ) ) ;
#74828 = DIRECTION ( 'NONE',  ( -0.5000000000000014433, 0.8660254037844379305, 0.000000000000000000 ) ) ;
#74830 = CARTESIAN_POINT ( 'NONE',  ( 152.4190720221992308, 266.6494185454878334, 15.69722907698042924 ) ) ;
#74829 = CARTESIAN_POINT ( 'NONE',  ( 157.1606030646430554, 258.4368458743103361, 17.96998724893680688 ) ) ;
#74831 = CARTESIAN_POINT ( 'NONE',  ( 8.106622824862185439, 30.17147933776454494, -10.00000000000000000 ) ) ;
#74832 = CARTESIAN_POINT ( 'NONE',  ( 198.9832789858017463, 285.9978462703757600, -18.55676541969546278 ) ) ;
#74833 = CARTESIAN_POINT ( 'NONE',  ( 204.0672213060390163, 276.0394433563056396, -13.55990476547925283 ) ) ;
#74834 = CARTESIAN_POINT ( 'NONE',  ( 34.65648599653719941, 40.98502408145595410, -5.678558825948271327 ) ) ;
#74835 = CARTESIAN_POINT ( 'NONE',  ( 146.8153075009282134, 276.3554234099810287, -4.113808735271278216 ) ) ;
#74836 = CARTESIAN_POINT ( 'NONE',  ( -71.61465314115659453, 63.06504152958490295, 25.00000000000000000 ) ) ;
#74837 = EDGE_LOOP ( 'NONE', ( #9857, #58897, #95610, #58812, #88420 ) ) ;
#74838 = CARTESIAN_POINT ( 'NONE',  ( 26.97531487256933858, 21.28920272979927830, -7.433330006724141015 ) ) ;
#74839 = CARTESIAN_POINT ( 'NONE',  ( 6.475147923497964086, 27.23654200823201066, 1.583844403245363353 ) ) ;
#74840 = CARTESIAN_POINT ( 'NONE',  ( 116.4326846683273544, 226.4824982072973683, 3.021315404115420679E-15 ) ) ;
#74841 = CARTESIAN_POINT ( 'NONE',  ( 189.9416213258632808, 286.8907125026590847, -15.86853789214096011 ) ) ;
#74842 = ORIENTED_EDGE ( 'NONE', *, *, #39847, .T. ) ;
#74843 = CARTESIAN_POINT ( 'NONE',  ( 70.99909089399695006, 61.09348569631758608, 14.50421621802051675 ) ) ;
#74844 = CARTESIAN_POINT ( 'NONE',  ( 75.75493378409400691, 65.86437009324527025, -14.07593894684413804 ) ) ;
#74845 = CARTESIAN_POINT ( 'NONE',  ( 157.4612664356622815, 268.7406194900779610, 15.65006598224691281 ) ) ;
#74846 = CARTESIAN_POINT ( 'NONE',  ( 169.9469112398214747, 250.9785751410766750, -8.718312767540300712 ) ) ;
#74847 = CARTESIAN_POINT ( 'NONE',  ( 148.1846377449773513, 246.3615022471901739, 5.000000000000051514 ) ) ;
#74848 = CARTESIAN_POINT ( 'NONE',  ( 205.2391015854675516, 275.1624436846170738, -14.01434138479280911 ) ) ;
#74849 = ORIENTED_EDGE ( 'NONE', *, *, #49267, .F. ) ;
#74850 = CARTESIAN_POINT ( 'NONE',  ( 189.9879251633717558, 299.5782561228834879, -6.671532329245590809 ) ) ;
#74851 = ORIENTED_EDGE ( 'NONE', *, *, #21840, .T. ) ;
#74852 = CARTESIAN_POINT ( 'NONE',  ( 196.9033078495128279, 265.2933406070572460, -4.538647946727325078 ) ) ;
#74853 = CARTESIAN_POINT ( 'NONE',  ( 81.82036482989325066, 42.35048943672428834, -7.944650131338358179 ) ) ;
#74854 = ORIENTED_EDGE ( 'NONE', *, *, #59683, .T. ) ;
#74855 = CARTESIAN_POINT ( 'NONE',  ( 181.6377726600393316, 290.8352285560014252, -10.98690006892555004 ) ) ;
#74856 = ORIENTED_EDGE ( 'NONE', *, *, #49055, .T. ) ;
#74857 = DIRECTION ( 'NONE',  ( -0.1654779384134469067, 0.9862134920484689760, 0.000000000000000000 ) ) ;
#74858 = CARTESIAN_POINT ( 'NONE',  ( 158.9711380693753711, 255.3009072572319269, 16.19938186386990608 ) ) ;
#74859 = CARTESIAN_POINT ( 'NONE',  ( 140.7960114214023974, 264.3464784336661637, 1.353441290958777327E-15 ) ) ;
#74860 = CARTESIAN_POINT ( 'NONE',  ( 204.0783642268031031, 272.7229525204484162, 11.17834187752937325 ) ) ;
#74861 = DIRECTION ( 'NONE',  ( -0.8653701635463872943, 0.5011331959107268030, 0.000000000000000000 ) ) ;
#74862 = EDGE_CURVE ( 'NONE', #76483, #78218, #10534, .T. ) ;
#74863 = CARTESIAN_POINT ( 'NONE',  ( 32.94608582406294062, 39.99752408145594984, 5.678558825948276656 ) ) ;
#74864 = CARTESIAN_POINT ( 'NONE',  ( -22.42236680055709641, 157.8615022471902591, 0.000000000000000000 ) ) ;
#74865 = CARTESIAN_POINT ( 'NONE',  ( 164.3152942664659690, 274.9982970269645648, 14.72102722954017118 ) ) ;
#74866 = CARTESIAN_POINT ( 'NONE',  ( 189.3423859142968695, 300.6963629005612120, 0.4146017780601669589 ) ) ;
#74867 = ORIENTED_EDGE ( 'NONE', *, *, #41670, .F. ) ;
#74868 = ORIENTED_EDGE ( 'NONE', *, *, #83291, .F. ) ;
#74869 = CARTESIAN_POINT ( 'NONE',  ( 87.08174047714162214, 46.31017841404310786, -9.261312696178791271 ) ) ;
#74871 = CARTESIAN_POINT ( 'NONE',  ( 162.6368345399827433, 272.7197526209740772, -16.33568937601149784 ) ) ;
#74870 = CARTESIAN_POINT ( 'NONE',  ( 204.9768178125733016, 275.6167325052707611, 13.98665089523138505 ) ) ;
#74872 = CARTESIAN_POINT ( 'NONE',  ( 206.0977829604818510, 273.6751639155793896, -9.820003938885891515 ) ) ;
#74873 = CARTESIAN_POINT ( 'NONE',  ( 43.16562282991919375, 123.9487658730721904, 10.00000000000000000 ) ) ;
#74874 = CARTESIAN_POINT ( 'NONE',  ( 71.06528275231133307, 61.93773232536235440, -14.16138117441405520 ) ) ;
#74875 = CARTESIAN_POINT ( 'NONE',  ( 82.34797793138363886, 40.36079106117341553, 1.103604957399969111 ) ) ;
#74876 = CARTESIAN_POINT ( 'NONE',  ( 171.0255721845828418, 287.7745651417276349, -4.514413061350604828 ) ) ;
#74877 = CARTESIAN_POINT ( 'NONE',  ( 77.06991968482392963, 62.91017430212377093, -15.27451705560989126 ) ) ;
#74878 = CARTESIAN_POINT ( 'NONE',  ( 178.3425427631553077, 255.6075038009615810, 4.888047764587837740 ) ) ;
#74879 = CARTESIAN_POINT ( 'NONE',  ( -36.70227853217910763, 37.68578735097466392, 59.99999999999999289 ) ) ;
#74880 = CARTESIAN_POINT ( 'NONE',  ( 190.9928235942860795, 292.9214909438621817, -14.57390052809859249 ) ) ;
#74881 = ORIENTED_EDGE ( 'NONE', *, *, #24790, .T. ) ;
#74882 = AXIS2_PLACEMENT_3D ( 'NONE', #42876, #25727, #42390 ) ;
#74883 = CIRCLE ( 'NONE', #18242, 17.82106496071138935 ) ;
#74884 = ORIENTED_EDGE ( 'NONE', *, *, #38972, .F. ) ;
#74885 = CARTESIAN_POINT ( 'NONE',  ( 87.15344218626839279, 46.31686449193668409, -8.569727620351585529 ) ) ;
#74887 = CARTESIAN_POINT ( 'NONE',  ( 194.6050500505458842, 285.5465367126718093, -17.70104686455487553 ) ) ;
#74886 = B_SPLINE_SURFACE_WITH_KNOTS ( 'NONE', 3, 1, ( 
 ( #25447, #87824 ),
 ( #18363, #49258 ),
 ( #80702, #19864 ),
 ( #63946, #80194 ),
 ( #10762, #21344 ),
 ( #52720, #90292 ),
 ( #37032, #76065 ),
 ( #12259, #43117 ),
 ( #51228, #13261 ),
 ( #81686, #98360 ),
 ( #20862, #74061 ),
 ( #21835, #67940 ),
 ( #13735, #29931 ),
 ( #60808, #44615 ),
 ( #59827, #4650 ),
 ( #58820, #6645 ),
 ( #83680, #66930 ),
 ( #60312, #75058 ),
 ( #12767, #35543 ),
 ( #75550, #51753 ),
 ( #43632, #27938 ),
 ( #97860, #45127 ),
 ( #89782, #28431 ),
 ( #20358, #14241 ),
 ( #82196, #59313 ),
 ( #98861, #66444 ),
 ( #37520, #29438 ),
 ( #82695, #91768 ),
 ( #97372, #91270 ),
 ( #90792, #68425 ),
 ( #50731, #99353 ) ),
 .UNSPECIFIED., .F., .F., .F.,
 ( 4, 3, 3, 3, 3, 3, 3, 3, 3, 3, 4 ),
 ( 2, 2 ),
 ( 0.000000000000000000, 0.1333490885032305451, 0.3007194338854253246, 0.4699862290244986029, 0.5844252810809236198, 0.6686540514502520294, 0.7354980260655306079, 0.8028463152565280536, 0.8633854507756927310, 0.9437142632666988273, 1.000000000000000000 ),
 ( 0.000000000000000000, 1.000000000000000000 ),
 .UNSPECIFIED. ) ;
#74888 = CARTESIAN_POINT ( 'NONE',  ( 195.8947060313465443, 291.3474115503753410, 16.07878593000791767 ) ) ;
#74889 = CARTESIAN_POINT ( 'NONE',  ( 159.5221561062548972, 254.3465160214695118, -16.91023001054109542 ) ) ;
#74890 = CARTESIAN_POINT ( 'NONE',  ( 195.6395968400605341, 272.4316657006998526, -14.88132701375339906 ) ) ;
#74891 = ORIENTED_EDGE ( 'NONE', *, *, #7775, .F. ) ;
#74892 = ORIENTED_EDGE ( 'NONE', *, *, #63303, .T. ) ;
#74893 = CARTESIAN_POINT ( 'NONE',  ( -21.44506416300749407, 94.09961582791768819, 54.99999999999999289 ) ) ;
#74894 = EDGE_LOOP ( 'NONE', ( #71131, #12316, #8419, #19210 ) ) ;
#74895 = AXIS2_PLACEMENT_3D ( 'NONE', #91989, #53426, #56922 ) ;
#74896 = CARTESIAN_POINT ( 'NONE',  ( 195.0706027375981080, 265.7742591254879017, -8.915832648898723178 ) ) ;
#74897 = CARTESIAN_POINT ( 'NONE',  ( -80.08603253397792798, 57.73992072201551906, -10.00000000000000000 ) ) ;
#74898 = CARTESIAN_POINT ( 'NONE',  ( 66.47089632795841396, 68.63383729509693865, -3.041274391255982756 ) ) ;
#74900 = CARTESIAN_POINT ( 'NONE',  ( 69.40172078258943600, 62.86412582178058273, -13.69687571282228511 ) ) ;
#74899 = CARTESIAN_POINT ( 'NONE',  ( 127.1021582719434662, 250.3149278399161233, -9.188101187500095079 ) ) ;
#74901 = CARTESIAN_POINT ( 'NONE',  ( 27.76992210170819675, 43.29297894285233639, 10.00000000000000000 ) ) ;
#74902 = ORIENTED_EDGE ( 'NONE', *, *, #43091, .T. ) ;
#74903 = CARTESIAN_POINT ( 'NONE',  ( 157.4843645388753544, 257.8760745514064183, 17.70049730742206862 ) ) ;
#74904 = CARTESIAN_POINT ( 'NONE',  ( 82.45205179438404741, 51.63644557190858819, 14.69498684280020662 ) ) ;
#74905 = CARTESIAN_POINT ( 'NONE',  ( 82.13437940688061190, 41.17851433583147269, -3.455252894430590249 ) ) ;
#74906 = CARTESIAN_POINT ( 'NONE',  ( 170.8421116289723045, 249.9010192475012673, -0.2585453712269101811 ) ) ;
#74907 = CARTESIAN_POINT ( 'NONE',  ( 121.4100190113084636, 234.2365022471901739, -10.00000000000009237 ) ) ;
#74908 = ADVANCED_FACE ( 'NONE', ( #41409 ), #81460, .F. ) ;
#74909 = PLANE ( 'NONE',  #28973 ) ;
#74910 = CARTESIAN_POINT ( 'NONE',  ( 82.27124186229274017, 40.74952593748430019, -3.675396864436865307 ) ) ;
#74911 = ADVANCED_FACE ( 'NONE', ( #64735 ), #12034, .F. ) ;
#74912 = FACE_OUTER_BOUND ( 'NONE', #23872, .T. ) ;
#74913 = CARTESIAN_POINT ( 'NONE',  ( 155.6276701977099890, 261.0919634844306643, 17.49722577287685255 ) ) ;
#74914 = CARTESIAN_POINT ( 'NONE',  ( 79.17142675679626507, 47.23956432523275595, 13.38762579824775223 ) ) ;
#74915 = CARTESIAN_POINT ( 'NONE',  ( 67.23123923419436210, 69.37383865658286197, -0.9211790948078316665 ) ) ;
#74916 = ADVANCED_FACE ( 'NONE', ( #26232 ), #38523, .T. ) ;
#74917 = CARTESIAN_POINT ( 'NONE',  ( 66.64328041388984047, 197.0327760586659736, 1.948934522072303157E-15 ) ) ;
#74918 = CARTESIAN_POINT ( 'NONE',  ( 206.0930919633010774, 273.6832889610345774, -9.866500005465628220 ) ) ;
#74919 = CARTESIAN_POINT ( 'NONE',  ( 178.1281481821618797, 292.9991590599575488, -6.064681374715556572 ) ) ;
#74920 = CARTESIAN_POINT ( 'NONE',  ( 208.3863431123642727, 269.7112614563416173, -1.693909372230378851 ) ) ;
#74921 = EDGE_CURVE ( 'NONE', #14677, #19304, #5423, .T. ) ;
#74922 = CARTESIAN_POINT ( 'NONE',  ( 66.47763888052396908, 67.99612994702233948, 6.463816604053789661 ) ) ;
#74923 = CARTESIAN_POINT ( 'NONE',  ( 67.07005509396013565, 69.31304007049533311, 0.5152274618438157372 ) ) ;
#74924 = CARTESIAN_POINT ( 'NONE',  ( 85.47913374364790684, 42.62622548008751266, 0.2499991700750583967 ) ) ;
#74925 = CARTESIAN_POINT ( 'NONE',  ( 71.30684095964828373, 218.6427522451419065, 10.00000000000009415 ) ) ;
#74926 = CARTESIAN_POINT ( 'NONE',  ( 41.03800390905408335, 35.64441083166263979, -10.00000000000000533 ) ) ;
#74927 = CARTESIAN_POINT ( 'NONE',  ( 79.21668578049593634, 56.34399116799300344, -16.56718607364530627 ) ) ;
#74928 = CARTESIAN_POINT ( 'NONE',  ( 157.7698537200534190, 270.6225848554070126, -15.38064719042920103 ) ) ;
#74929 = CARTESIAN_POINT ( 'NONE',  ( 72.28225989300379695, 72.02129029449646680, 3.461803769446522239 ) ) ;
#74930 = CARTESIAN_POINT ( 'NONE',  ( 29.48529115882250551, 178.6423013555409796, -4.594050593750043987 ) ) ;
#74931 = B_SPLINE_CURVE_WITH_KNOTS ( 'NONE', 3,
 ( #40512, #70945, #32432, #78546 ),
 .UNSPECIFIED., .F., .F.,
 ( 4, 4 ),
 ( 0.008410254777844634877, 0.01479413815379926507 ),
 .UNSPECIFIED. ) ;
#74932 = DIRECTION ( 'NONE',  ( 0.000000000000000000, 0.000000000000000000, 1.000000000000000000 ) ) ;
#74933 = CARTESIAN_POINT ( 'NONE',  ( 185.0107362994922937, 259.8037357443623705, -8.917975770776131128 ) ) ;
#74934 = CARTESIAN_POINT ( 'NONE',  ( 199.2838428981942229, 277.8941618483122511, 16.22077298392192191 ) ) ;
#74935 = CARTESIAN_POINT ( 'NONE',  ( 78.23057914463134921, 51.11287733427894864, -15.28606483983534936 ) ) ;
#74936 = CARTESIAN_POINT ( 'NONE',  ( 71.63329245445480353, 72.42139875791372106, -1.350275132429440861 ) ) ;
#74937 = CARTESIAN_POINT ( 'NONE',  ( 46.39958950466356669, 197.5958772461660544, -9.188101187500095079 ) ) ;
#74938 = CARTESIAN_POINT ( 'NONE',  ( 27.11361191214091804, 16.44966523072495335, -2.296566073217252530E-15 ) ) ;
#74939 = CARTESIAN_POINT ( 'NONE',  ( 170.6536247108341513, 287.7753904406291667, 7.365555831541199971 ) ) ;
#74940 = CARTESIAN_POINT ( 'NONE',  ( 149.7109319212262051, 271.3400547943878109, -12.38605961032017433 ) ) ;
#74941 = CARTESIAN_POINT ( 'NONE',  ( 3.104905098483929482, 23.83396525600387506, -2.839279412974133887 ) ) ;
#74942 = CARTESIAN_POINT ( 'NONE',  ( 203.0033695482938185, 269.9821257774704009, -7.166763272130794782 ) ) ;
#74943 = CARTESIAN_POINT ( 'NONE',  ( 175.8519086042108199, 291.1168019899661203, 2.550567897145465501 ) ) ;
#74944 = CARTESIAN_POINT ( 'NONE',  ( 179.7328860548953458, 276.7974806922320568, 16.30745684656992722 ) ) ;
#74945 = CARTESIAN_POINT ( 'NONE',  ( 182.2373335159190901, 280.9600371166583841, -17.30031729693378040 ) ) ;
#74946 = CARTESIAN_POINT ( 'NONE',  ( 73.28832484065085850, 67.50848624533098530, -11.46336223192518844 ) ) ;
#74947 = CARTESIAN_POINT ( 'NONE',  ( 192.9510928534456298, 267.2000408598793797, 11.21941862815989488 ) ) ;
#74948 = AXIS2_PLACEMENT_3D ( 'NONE', #58713, #49632, #97755 ) ;
#74949 = DIRECTION ( 'NONE',  ( 0.000000000000000000, 0.000000000000000000, 1.000000000000000000 ) ) ;
#74950 = CARTESIAN_POINT ( 'NONE',  ( 91.89298649898879034, 233.8615022471903160, 5.000000000000046185 ) ) ;
#74951 = CARTESIAN_POINT ( 'NONE',  ( 200.4116241316243645, 283.5238799070667142, 18.37703770054986663 ) ) ;
#74952 = CARTESIAN_POINT ( 'NONE',  ( 194.7281770665802867, 285.5812223991454744, -17.42918990626452924 ) ) ;
#74953 = VERTEX_POINT ( 'NONE', #52017 ) ;
#74954 = CARTESIAN_POINT ( 'NONE',  ( 54.73473692032377613, 214.6589784336661637, -6.496448406907675876E-16 ) ) ;
#74955 = EDGE_LOOP ( 'NONE', ( #7060, #10035, #6098, #67121 ) ) ;
#74956 = LINE ( 'NONE', #67842, #82144 ) ;
#74957 = CARTESIAN_POINT ( 'NONE',  ( 190.8957779480239765, 300.0058089740729770, -4.541438514207768229 ) ) ;
#74958 = CYLINDRICAL_SURFACE ( 'NONE', #58041, 70.00000000000002842 ) ;
#74959 = VERTEX_POINT ( 'NONE', #44399 ) ;
#74961 = FACE_OUTER_BOUND ( 'NONE', #45536, .T. ) ;
#74960 = VECTOR ( 'NONE', #31332, 1000.000000000000114 ) ;
#74962 = CARTESIAN_POINT ( 'NONE',  ( 79.11321178432963563, 45.92345112123121709, -12.55202503363903155 ) ) ;
#74963 = CYLINDRICAL_SURFACE ( 'NONE', #78280, 70.00000000000002842 ) ;
#74964 = B_SPLINE_CURVE_WITH_KNOTS ( 'NONE', 3,
 ( #67124, #97563, #13451, #58522 ),
 .UNSPECIFIED., .F., .F.,
 ( 4, 4 ),
 ( 0.01376344692898578796, 0.02004488622147810803 ),
 .UNSPECIFIED. ) ;
#74965 = CARTESIAN_POINT ( 'NONE',  ( -28.78582490886478240, 40.83341904737610406, 59.99999999999999289 ) ) ;
#74966 = CARTESIAN_POINT ( 'NONE',  ( 86.53679916633876701, 47.27946550500259804, -10.19252361861625111 ) ) ;
#74967 = EDGE_CURVE ( 'NONE', #14070, #72951, #7919, .T. ) ;
#74968 = CARTESIAN_POINT ( 'NONE',  ( 205.0993130461165777, 275.4045645370890156, 13.92529057593422337 ) ) ;
#74969 = ORIENTED_EDGE ( 'NONE', *, *, #62898, .F. ) ;
#74970 = CARTESIAN_POINT ( 'NONE',  ( 20.38389956778225809, 29.95586893147755703, 7.433330006724141015 ) ) ;
#74971 = CARTESIAN_POINT ( 'NONE',  ( 76.39152921487998071, 62.56948907837542606, 15.23512175509495137 ) ) ;
#74972 = CARTESIAN_POINT ( 'NONE',  ( 164.8705138155180521, 286.2009910768602481, -3.373684704351256780 ) ) ;
#74973 = CARTESIAN_POINT ( 'NONE',  ( 6.156471524329347744, 184.3615022471903160, 5.000000000000046185 ) ) ;
#74974 = ORIENTED_EDGE ( 'NONE', *, *, #18531, .F. ) ;
#74975 = DIRECTION ( 'NONE',  ( -1.000000000000000000, 0.000000000000000000, -0.000000000000000000 ) ) ;
#74976 = CARTESIAN_POINT ( 'NONE',  ( 167.3443243822065654, 261.7894444419548563, 16.27081549069046318 ) ) ;
#74977 = CARTESIAN_POINT ( 'NONE',  ( 206.8317058779879574, 272.4039721336197317, -10.41591514895975834 ) ) ;
#74978 = ORIENTED_EDGE ( 'NONE', *, *, #88443, .F. ) ;
#74980 = LINE ( 'NONE', #98282, #18405 ) ;
#74979 = CARTESIAN_POINT ( 'NONE',  ( 159.7396088078454852, 282.2794754784105749, -3.211990912219383709 ) ) ;
#74981 = CARTESIAN_POINT ( 'NONE',  ( 70.46175891972434613, 71.28076662974713429, -3.876972208410735199 ) ) ;
#74982 = CARTESIAN_POINT ( 'NONE',  ( 65.88300657315410547, 69.00302489017140317, -2.153913200402058248 ) ) ;
#74983 = PLANE ( 'NONE',  #5981 ) ;
#74984 = CARTESIAN_POINT ( 'NONE',  ( -57.46197106626858186, 34.15416430719361074, -10.00000000000000000 ) ) ;
#74985 = CARTESIAN_POINT ( 'NONE',  ( 163.5043721629895117, 264.4363120689758944, -16.70418041949503873 ) ) ;
#74986 = ADVANCED_FACE ( 'NONE', ( #94419 ), #48289, .F. ) ;
#74987 = CARTESIAN_POINT ( 'NONE',  ( 136.0064158243085046, 240.1423013555409796, -4.594050593750043987 ) ) ;
#74988 = CARTESIAN_POINT ( 'NONE',  ( 10.46624461501205872, 188.3967562850346837, -4.648177544792955347E-16 ) ) ;
#74989 = ORIENTED_EDGE ( 'NONE', *, *, #23936, .T. ) ;
#74990 = CARTESIAN_POINT ( 'NONE',  ( 170.1385426601652568, 264.1995677655418149, 16.47783103859512721 ) ) ;
#74991 = LINE ( 'NONE', #65377, #28533 ) ;
#74992 = VERTEX_POINT ( 'NONE', #33082 ) ;
#74993 = B_SPLINE_CURVE_WITH_KNOTS ( 'NONE', 3,
 ( #53036, #52051, #99658, #14556 ),
 .UNSPECIFIED., .F., .F.,
 ( 4, 4 ),
 ( 2.780973288783981667E-17, 0.002844266532014441858 ),
 .UNSPECIFIED. ) ;
#74994 = CARTESIAN_POINT ( 'NONE',  ( 83.21237853290490705, 230.3967562850347122, -4.648177544792955347E-16 ) ) ;
#74995 = ORIENTED_EDGE ( 'NONE', *, *, #63540, .T. ) ;
#74996 = VERTEX_POINT ( 'NONE', #64487 ) ;
#74997 = CARTESIAN_POINT ( 'NONE',  ( 198.6742831389107096, 286.5330427765190393, 17.60232614297041565 ) ) ;
#74998 = DIRECTION ( 'NONE',  ( -0.8492021815265757834, 0.5280678506503729830, 0.000000000000000000 ) ) ;
#74999 = CARTESIAN_POINT ( 'NONE',  ( 77.36034478572226192, 203.2202760586659167, -5.415160957724236172E-17 ) ) ;
#75000 = DIRECTION ( 'NONE',  ( -0.8660254037844382635, -0.5000000000000005551, 0.000000000000000000 ) ) ;
#75001 = CARTESIAN_POINT ( 'NONE',  ( 120.4921787521148246, 228.8262482093457777, 3.021315404115420679E-15 ) ) ;
#75002 = CARTESIAN_POINT ( 'NONE',  ( 155.6435836392643637, 261.0644005951349982, 17.58841156286628049 ) ) ;
#75003 = B_SPLINE_CURVE_WITH_KNOTS ( 'NONE', 3,
 ( #86634, #33374, #16673, #23763, #17169, #32375, #64278, #48069, #31861, #15665, #56157, #94216, #79010, #87152, #55156, #62761, #980, #78495, #70370, #9081, #40459, #79525, #9597, #71395, #1985, #8584, #32870, #63776, #48584, #17684, #95229, #63274, #10086, #94708, #47567, #62253, #40949, #24280, #2492, #93719, #39951, #54151, #85113, #38961, #46559, #77494 ),
 .UNSPECIFIED., .F., .F.,
 ( 4, 1, 2, 2, 1, 2, 2, 1, 1, 2, 2, 1, 1, 2, 2, 1, 1, 2, 2, 1, 1, 1, 2, 2, 1, 1, 1, 2, 2, 4 ),
 ( 0.000000000000000000, 0.06250000000000068001, 0.09374999999999913958, 0.1249999999999976130, 0.1874999999999949485, 0.2187499999999950040, 0.2499999999999950318, 0.3124999999999953926, 0.3437499999999953371, 0.3593749999999956701, 0.3749999999999960032, 0.4374999999999978351, 0.4687499999999970024, 0.4843749999999983902, 0.4999999999999997780, 0.5624999999999968914, 0.5937499999999937828, 0.6093749999999906741, 0.6249999999999874545, 0.6874999999999754641, 0.7187499999999714673, 0.7343749999999694689, 0.7421874999999681366, 0.7499999999999666933, 0.8124999999999791278, 0.8437499999999833467, 0.8593749999999868994, 0.8671874999999871214, 0.8749999999999873435, 1.000000000000000000 ),
 .UNSPECIFIED. ) ;
#75004 = CARTESIAN_POINT ( 'NONE',  ( 138.1418008908465822, 79.75620593067000641, -17.47570218321536473 ) ) ;
#75005 = CARTESIAN_POINT ( 'NONE',  ( 183.3097982497011174, 257.4453907524014085, -6.291681649002233812 ) ) ;
#75006 = VERTEX_POINT ( 'NONE', #24973 ) ;
#75007 = CARTESIAN_POINT ( 'NONE',  ( 119.9486011388743236, 233.3927522451417360, -10.00000000000009237 ) ) ;
#75008 = CARTESIAN_POINT ( 'NONE',  ( 152.9607371460978129, 265.7112270302071124, -16.17698032818104537 ) ) ;
#75009 = CARTESIAN_POINT ( 'NONE',  ( 155.3513572141771704, 261.5705516107003064, -17.00592413546589299 ) ) ;
#75010 = ORIENTED_EDGE ( 'NONE', *, *, #31526, .T. ) ;
#75011 = CARTESIAN_POINT ( 'NONE',  ( 36.25628400652970384, 53.06077264917335867, 10.00000000000000000 ) ) ;
#75012 = CARTESIAN_POINT ( 'NONE',  ( 163.8698660330890959, 260.7705462234230254, -16.30966607616605657 ) ) ;
#75013 = CARTESIAN_POINT ( 'NONE',  ( 24.86884376670136021, 66.72197582601074828, 59.99999999999999289 ) ) ;
#75014 = CARTESIAN_POINT ( 'NONE',  ( 199.9852625142306977, 283.3066338628505036, -17.10789104304789277 ) ) ;
#75015 = CARTESIAN_POINT ( 'NONE',  ( 164.5648480107187197, 245.6123174360222094, 3.015887571020871238 ) ) ;
#75016 = CARTESIAN_POINT ( 'NONE',  ( 86.70911053808110580, 46.89117940024963360, 10.21290512048939902 ) ) ;
#75017 = CARTESIAN_POINT ( 'NONE',  ( 195.1869371033206164, 279.2024320103926129, 16.32474613100176342 ) ) ;
#75018 = ORIENTED_EDGE ( 'NONE', *, *, #27574, .T. ) ;
#75019 = CARTESIAN_POINT ( 'NONE',  ( 207.5290616128274337, 271.1961165699281651, 2.604679844609484984 ) ) ;
#75020 = CARTESIAN_POINT ( 'NONE',  ( 132.4608640057421667, 247.2833772461660544, -9.188101187500095079 ) ) ;
#75021 = VERTEX_POINT ( 'NONE', #79234 ) ;
#75022 = CARTESIAN_POINT ( 'NONE',  ( -7.720288864461156919, 177.8967562850347122, -4.648177544792955347E-16 ) ) ;
#75023 = CARTESIAN_POINT ( 'NONE',  ( 85.34796002485173005, 43.47219069357272758, 5.045432809274035257 ) ) ;
#75024 = EDGE_CURVE ( 'NONE', #31137, #40803, #44132, .T. ) ;
#75025 = CARTESIAN_POINT ( 'NONE',  ( 80.32560484147226987, 44.93948968179056180, -11.21518412823304800 ) ) ;
#75026 = B_SPLINE_CURVE_WITH_KNOTS ( 'NONE', 3,
 ( #86697, #93271, #24833, #31925, #87219, #70956, #63340, #94278, #62828, #56225, #87718, #10152, #41018, #17754, #79588, #55707, #71956, #2560, #63837, #17230, #56736, #9143, #39019, #24345, #69927, #2051, #93785, #1559, #544, #39511, #40525, #70436, #16239, #31426, #1046, #55219, #71460, #16739, #47628, #32933, #94775, #25335, #65339, #66336, #33964, #88702 ),
 .UNSPECIFIED., .F., .F.,
 ( 4, 1, 1, 1, 2, 2, 1, 1, 1, 2, 2, 1, 1, 2, 2, 1, 1, 2, 2, 1, 1, 2, 2, 1, 2, 2, 1, 2, 2, 4 ),
 ( 0.000000000000000000, 0.06250000000002643719, 0.09375000000003808065, 0.1093750000000423134, 0.1171875000000460465, 0.1250000000000497657, 0.1875000000000617562, 0.2187500000000678624, 0.2343750000000710543, 0.2421875000000724976, 0.2500000000000739409, 0.3125000000000892064, 0.3437500000000967004, 0.3593750000000985878, 0.3750000000001004752, 0.4375000000001050271, 0.4687500000001074141, 0.4843750000001070255, 0.5000000000001065814, 0.5625000000000948130, 0.5937500000000873746, 0.6093750000000841549, 0.6250000000000808242, 0.6875000000000719425, 0.7187500000000656142, 0.7500000000000592859, 0.8125000000000435207, 0.8437500000000360822, 0.8750000000000286438, 1.000000000000000000 ),
 .UNSPECIFIED. ) ;
#75027 = CARTESIAN_POINT ( 'NONE',  ( 72.82976588666879536, 70.83552076258160923, 7.211487186626502677 ) ) ;
#75028 = DIRECTION ( 'NONE',  ( -0.8660254037844387076, -0.4999999999999998890, -0.000000000000000000 ) ) ;
#75029 = VECTOR ( 'NONE', #75198, 1000.000000000000114 ) ;
#75030 = CYLINDRICAL_SURFACE ( 'NONE', #4913, 70.00000000000002842 ) ;
#75031 = ORIENTED_EDGE ( 'NONE', *, *, #79719, .F. ) ;
#75032 = CARTESIAN_POINT ( 'NONE',  ( 76.16009226555104306, 53.07303640036436576, 15.95681292398955264 ) ) ;
#75033 = CARTESIAN_POINT ( 'NONE',  ( 182.4489905826245888, 275.9573809634798636, -16.44186478306133736 ) ) ;
#75034 = VECTOR ( 'NONE', #98635, 1000.000000000000114 ) ;
#75035 = CARTESIAN_POINT ( 'NONE',  ( 167.2918192146199772, 248.9981393517354320, -5.482138639605560471 ) ) ;
#75036 = CARTESIAN_POINT ( 'NONE',  ( 81.32851801649849222, 53.07575169590482744, 15.40321648735625004 ) ) ;
#75037 = CARTESIAN_POINT ( 'NONE',  ( 73.64475323345853042, 69.68564092398970899, -9.517716319079164933 ) ) ;
#75038 = EDGE_CURVE ( 'NONE', #66534, #2736, #31193, .T. ) ;
#75039 = AXIS2_PLACEMENT_3D ( 'NONE', #94889, #77678, #9262 ) ;
#75040 = LINE ( 'NONE', #14216, #61056 ) ;
#75041 = CARTESIAN_POINT ( 'NONE',  ( 183.2023180053008673, 280.9201651122064618, 17.20581014854919744 ) ) ;
#75042 = CARTESIAN_POINT ( 'NONE',  ( 193.1374568794722393, 268.2848186726958488, 12.69397648171735860 ) ) ;
#75043 = CARTESIAN_POINT ( 'NONE',  ( 27.71094225399020061, 18.12755873383627403, -6.180339887498949025 ) ) ;
#75044 = DIRECTION ( 'NONE',  ( -0.4972609476841356457, 0.8612812260087758798, 0.1045284632676436315 ) ) ;
#75045 = CARTESIAN_POINT ( 'NONE',  ( 80.05961770938091604, 205.4824982072973967, 3.021315404115420679E-15 ) ) ;
#75046 = CARTESIAN_POINT ( 'NONE',  ( 72.76074090227031377, 69.17543318582201550, -10.12738290133669850 ) ) ;
#75047 = FACE_OUTER_BOUND ( 'NONE', #78541, .T. ) ;
#75048 = CARTESIAN_POINT ( 'NONE',  ( 207.2597638908594604, 271.6625539067387649, 6.169660687298267554 ) ) ;
#75049 =( BOUNDED_CURVE ( )  B_SPLINE_CURVE ( 2, ( #48369, #15956, #47352, #78274, #16455, #70656, #1268, #70142, #38749 ),
 .UNSPECIFIED., .F., .T. ) 
 B_SPLINE_CURVE_WITH_KNOTS ( ( 3, 2, 2, 2, 3 ),
 ( 0.6411290322580645018, 0.6424731182795698770, 0.6451612903225806273, 0.6478494623655913776, 0.6491935483870967527 ),
 .UNSPECIFIED. ) 
 CURVE ( )  GEOMETRIC_REPRESENTATION_ITEM ( )  RATIONAL_B_SPLINE_CURVE ( ( 0.9330127018922194093, 0.9330127018922194093, 1.000000000000000000, 0.8660254037844387076, 1.000000000000000000, 0.8660254037844387076, 1.000000000000000000, 0.9330127018922194093, 0.9330127018922194093 ) ) 
 REPRESENTATION_ITEM ( '' )  );
#75050 = CARTESIAN_POINT ( 'NONE',  ( 140.6610420460521311, 252.0177522451418213, -10.00000000000009592 ) ) ;
#75051 = DIRECTION ( 'NONE',  ( -0.4635919272833941562, 0.8029647720336182681, 0.3746065934159032440 ) ) ;
#75052 = ORIENTED_EDGE ( 'NONE', *, *, #58561, .F. ) ;
#75053 = CARTESIAN_POINT ( 'NONE',  ( 66.74093763034696281, 68.12488142277693726, -6.511293142817978996 ) ) ;
#75054 = CARTESIAN_POINT ( 'NONE',  ( 198.8194531333411419, 286.2816009704309863, -17.01510935557533344 ) ) ;
#75055 = CARTESIAN_POINT ( 'NONE',  ( 5.777845730223497789, 164.9548013555410080, -4.594050593750042211 ) ) ;
#75056 = CARTESIAN_POINT ( 'NONE',  ( 178.5612894430947790, 259.1195402287601723, -10.32338363706679019 ) ) ;
#75057 = CARTESIAN_POINT ( 'NONE',  ( 25.88782454542109335, 20.11029122506295153, -8.090169943749478065 ) ) ;
#75058 = CARTESIAN_POINT ( 'NONE',  ( 85.26413132878788304, 49.08502152628110338, 12.44825952561157578 ) ) ;
#75059 = CARTESIAN_POINT ( 'NONE',  ( 157.1002372043759010, 258.5414026113353430, -17.73553732786789539 ) ) ;
#75060 = CARTESIAN_POINT ( 'NONE',  ( 71.73704408672971056, 72.08698097738312072, -3.607164568159269891 ) ) ;
#75061 = CARTESIAN_POINT ( 'NONE',  ( 124.7297830591487724, 249.4865022471903160, 10.00000000000009415 ) ) ;
#75063 = CARTESIAN_POINT ( 'NONE',  ( 67.84273934451053378, 216.6427522451418781, -10.00000000000009415 ) ) ;
#75062 = CARTESIAN_POINT ( 'NONE',  ( 200.1492870304027178, 271.0868101810378903, -11.33151401369217659 ) ) ;
#75064 = CARTESIAN_POINT ( 'NONE',  ( 75.07870810345070822, 67.14405870075098903, 12.61863177765487620 ) ) ;
#75065 = CARTESIAN_POINT ( 'NONE',  ( 150.9158774466703221, 269.2530279239659308, 15.11407781020157515 ) ) ;
#75066 = CARTESIAN_POINT ( 'NONE',  ( 179.0995391845479503, 294.3117743827021400, 1.062652647630369485 ) ) ;
#75067 = CARTESIAN_POINT ( 'NONE',  ( 54.58172535260923297, 208.9865022471903160, 10.00000000000009237 ) ) ;
#75068 = DIRECTION ( 'NONE',  ( 0.4999999999999998890, -0.8660254037844385966, 0.000000000000000000 ) ) ;
#75069 = CARTESIAN_POINT ( 'NONE',  ( 148.3837145175834280, 273.6388627701866767, 8.841971351370922605 ) ) ;
#75070 = CARTESIAN_POINT ( 'NONE',  ( 11.32556065139379875, 177.3458772461660544, 9.188101187500095079 ) ) ;
#75071 = CARTESIAN_POINT ( 'NONE',  ( 168.2809673467089624, 286.2893536684765081, 4.380497092391412828 ) ) ;
#75072 = CARTESIAN_POINT ( 'NONE',  ( 13.85502868284443068, 167.2592609112379876, 2.679491924311228512 ) ) ;
#75073 = CARTESIAN_POINT ( 'NONE',  ( 38.63056705113294953, 37.70171378149921537, -9.188101187500004485 ) ) ;
#75074 = CARTESIAN_POINT ( 'NONE',  ( 201.6770223052710946, 280.5522444021153206, -16.20575782718176328 ) ) ;
#75075 = LINE ( 'NONE', #98876, #83969 ) ;
#75076 = CARTESIAN_POINT ( 'NONE',  ( 188.2111106237954630, 267.2351608166093797, 14.29806277360018996 ) ) ;
#75077 = CARTESIAN_POINT ( 'NONE',  ( 114.5053184729291189, 248.4637435831425023, 2.679491924311251605 ) ) ;
#75078 = CARTESIAN_POINT ( 'NONE',  ( 160.1491107143660884, 280.2713282481162764, 9.384238864439979011 ) ) ;
#75079 = SHAPE_REPRESENTATION_RELATIONSHIP ( 'NONE' , 'NONE' ,  #7571, #69379 ) ;
#75080 = CARTESIAN_POINT ( 'NONE',  ( 12.86511499041763074, 19.37878583063839244, 9.188101187500006262 ) ) ;
#75081 = CARTESIAN_POINT ( 'NONE',  ( 71.85326037870231630, 72.57223462184857965, 1.067429543862033814 ) ) ;
#75082 = LINE ( 'NONE', #92666, #66173 ) ;
#75083 = CARTESIAN_POINT ( 'NONE',  ( 159.5589503240031206, 258.7431445789238751, 17.10287526337421227 ) ) ;
#75084 = EDGE_CURVE ( 'NONE', #45792, #3742, #87854, .T. ) ;
#75085 = CARTESIAN_POINT ( 'NONE',  ( 194.1011995340913074, 294.4538559273262877, 13.93949783759920713 ) ) ;
#75086 = EDGE_LOOP ( 'NONE', ( #55880, #78772, #54502, #11187 ) ) ;
#75087 = CARTESIAN_POINT ( 'NONE',  ( 182.0723377230381743, 289.3047168942152325, 12.38573695971384048 ) ) ;
#75088 = CARTESIAN_POINT ( 'NONE',  ( -0.01211276271276956473, 139.0458036431182620, 21.50000000000008527 ) ) ;
#75089 = CARTESIAN_POINT ( 'NONE',  ( 74.99952688636028597, 53.39440814940449798, -16.04976397322502990 ) ) ;
#75090 = CARTESIAN_POINT ( 'NONE',  ( 81.12531108467926799, 42.43832548245816838, 7.730292043048938133 ) ) ;
#75091 = EDGE_CURVE ( 'NONE', #99571, #15352, #53818, .T. ) ;
#75092 = EDGE_LOOP ( 'NONE', ( #14971, #89813, #59210, #85596, #55384, #23491, #81748, #44719, #15388, #91322, #30482, #25230, #79597, #10049, #711, #1682, #4806, #92864, #94412, #38546 ) ) ;
#75093 = CARTESIAN_POINT ( 'NONE',  ( -19.65312891409030271, 93.06504152958497400, -10.00000000000000888 ) ) ;
#75094 = CARTESIAN_POINT ( 'NONE',  ( 82.32736432458936804, 40.35218285420588558, 1.148310913625198104 ) ) ;
#75095 = CYLINDRICAL_SURFACE ( 'NONE', #68746, 16.60714546451156792 ) ;
#75096 = CARTESIAN_POINT ( 'NONE',  ( 155.1398527401465230, 261.9368881057492899, -17.02245700497956449 ) ) ;
#75097 = CIRCLE ( 'NONE', #47516, 70.00000000000001421 ) ;
#75098 = ORIENTED_EDGE ( 'NONE', *, *, #68953, .T. ) ;
#75099 = ORIENTED_EDGE ( 'NONE', *, *, #75481, .T. ) ;
#75101 = CARTESIAN_POINT ( 'NONE',  ( 204.3276935076901850, 276.7410487817560920, 13.46217427333259309 ) ) ;
#75100 = CARTESIAN_POINT ( 'NONE',  ( 159.4050015888674920, 279.2435389297123152, -9.491234884881382783 ) ) ;
#75102 = CARTESIAN_POINT ( 'NONE',  ( 192.0523540417460993, 298.0025604169266558, 12.03387399082417275 ) ) ;
#75103 = VERTEX_POINT ( 'NONE', #74605 ) ;
#75104 = CARTESIAN_POINT ( 'NONE',  ( 151.4327733764141612, 268.3577379114237829, 14.90862905801242100 ) ) ;
#75105 = CARTESIAN_POINT ( 'NONE',  ( 80.56183422562187957, 57.64990364647651688, 16.23776005631657426 ) ) ;
#75106 = CARTESIAN_POINT ( 'NONE',  ( 160.6574774401344428, 259.8181007787099475, -17.52623987902137515 ) ) ;
#75108 = EDGE_CURVE ( 'NONE', #75612, #65702, #64993, .T. ) ;
#75107 = ORIENTED_EDGE ( 'NONE', *, *, #82056, .T. ) ;
#75109 = CARTESIAN_POINT ( 'NONE',  ( 87.48484950937405813, 45.04520271710788393, -6.098260242492822059 ) ) ;
#75110 = AXIS2_PLACEMENT_3D ( 'NONE', #17748, #70950, #25330 ) ;
#75111 = CARTESIAN_POINT ( 'NONE',  ( 196.5475899070771675, 290.2165835061676944, -17.89382743182097002 ) ) ;
#75112 = ORIENTED_EDGE ( 'NONE', *, *, #10578, .F. ) ;
#75113 = CARTESIAN_POINT ( 'NONE',  ( 206.0041637419966776, 273.8373171585603814, 11.66586596407113596 ) ) ;
#75114 = DIRECTION ( 'NONE',  ( 0.5000000000000001110, -0.8660254037844384856, -0.000000000000000000 ) ) ;
#75115 = B_SPLINE_SURFACE_WITH_KNOTS ( 'NONE', 3, 1, ( 
 ( #73958, #50635 ),
 ( #20763, #19766 ),
 ( #88712, #58238 ),
 ( #19281, #12157 ),
 ( #42530, #50148 ),
 ( #18763, #10662 ),
 ( #89699, #41538 ),
 ( #97765, #72483 ),
 ( #3085, #73463 ),
 ( #74477, #33976 ),
 ( #82095, #12668 ),
 ( #57237, #65831 ),
 ( #96797, #64860 ),
 ( #43536, #95807 ),
 ( #4046, #43019 ),
 ( #81588, #5055 ),
 ( #4543, #26361 ),
 ( #3569, #35444 ),
 ( #81101, #66346 ),
 ( #88212, #49641 ),
 ( #97279, #27356 ),
 ( #26856, #57732 ),
 ( #11668, #27846 ),
 ( #51133, #80599 ),
 ( #11177, #58724 ),
 ( #42044, #34450 ),
 ( #65348, #20258 ),
 ( #35935, #28335 ),
 ( #59212, #90187 ),
 ( #21740, #29351 ),
 ( #7531, #92673 ),
 ( #30841, #99753 ),
 ( #90698, #7034 ),
 ( #37916, #30338 ) ),
 .UNSPECIFIED., .T., .F., .F.,
 ( 4, 2, 2, 2, 2, 2, 2, 2, 2, 2, 2, 2, 2, 2, 2, 2, 4 ),
 ( 2, 2 ),
 ( 0.000000000000000000, 0.06250000000000000000, 0.1250000000000000000, 0.1875000000000000000, 0.2500000000000000000, 0.3125000000000000000, 0.3750000000000000000, 0.4375000000000000000, 0.5000000000000000000, 0.5625000000000000000, 0.6250000000000000000, 0.6875000000000000000, 0.7500000000000000000, 0.8125000000000000000, 0.8750000000000000000, 0.9375000000000000000, 1.000000000000000000 ),
 ( 0.000000000000000000, 1.000000000000000000 ),
 .UNSPECIFIED. ) ;
#75116 = ORIENTED_EDGE ( 'NONE', *, *, #93643, .F. ) ;
#75117 = CARTESIAN_POINT ( 'NONE',  ( 174.5871134489742076, 276.7843657037444132, -16.02992603658275073 ) ) ;
#75118 = CARTESIAN_POINT ( 'NONE',  ( 168.9751777291785402, 261.3521787389587985, -16.33135548124933223 ) ) ;
#75119 = EDGE_LOOP ( 'NONE', ( #73996, #80782, #95874, #53174 ) ) ;
#75120 = CARTESIAN_POINT ( 'NONE',  ( 158.6609831669983635, 274.8501997329411779, -12.75851027878984745 ) ) ;
#75121 = EDGE_CURVE ( 'NONE', #52122, #19903, #75359, .T. ) ;
#75122 = LINE ( 'NONE', #5208, #40162 ) ;
#75123 = CARTESIAN_POINT ( 'NONE',  ( 45.57373283677818421, 114.7827874512443032, -10.00000000000000000 ) ) ;
#75124 = ORIENTED_EDGE ( 'NONE', *, *, #82629, .T. ) ;
#75125 = ORIENTED_EDGE ( 'NONE', *, *, #37203, .T. ) ;
#75126 = CARTESIAN_POINT ( 'NONE',  ( 73.63577410123313882, 69.72805253716678919, 9.466241435726317377 ) ) ;
#75127 = CARTESIAN_POINT ( 'NONE',  ( 87.24693701583447591, 43.60182921170479631, 0.4518306138544891382 ) ) ;
#75128 = CARTESIAN_POINT ( 'NONE',  ( 190.9380839614473473, 299.9325328093580652, -5.232187664503159752 ) ) ;
#75129 = CARTESIAN_POINT ( 'NONE',  ( 82.62974588365311490, 53.86145749464596122, 15.83045060744369614 ) ) ;
#75130 = DIRECTION ( 'NONE',  ( -1.000000000000000000, 0.000000000000000000, 0.000000000000000000 ) ) ;
#75131 = CARTESIAN_POINT ( 'NONE',  ( 192.5254593562406171, 297.1831179748913314, 11.00703791256144015 ) ) ;
#75132 = CARTESIAN_POINT ( 'NONE',  ( 191.7079280567292017, 298.5991237224230304, 9.677592105567574876 ) ) ;
#75133 = CARTESIAN_POINT ( 'NONE',  ( 147.1447476476323004, 275.7848163378367872, 0.6373001129109078233 ) ) ;
#75134 = ORIENTED_EDGE ( 'NONE', *, *, #14689, .T. ) ;
#75135 = CARTESIAN_POINT ( 'NONE',  ( 75.96267333776768282, 57.39029935918532033, -16.11942128475391911 ) ) ;
#75136 = DIRECTION ( 'NONE',  ( 0.4330127018922192983, 0.2500000000000001110, -0.8660254037844387076 ) ) ;
#75137 = CARTESIAN_POINT ( 'NONE',  ( 67.14419364460526651, 66.64754800388041645, 8.362635188899179894 ) ) ;
#75138 = DIRECTION ( 'NONE',  ( -0.9607486656258038549, -0.2774202615135334948, 0.000000000000000000 ) ) ;
#75139 = CYLINDRICAL_SURFACE ( 'NONE', #88438, 17.82106496071139645 ) ;
#75140 = VERTEX_POINT ( 'NONE', #72613 ) ;
#75141 = CARTESIAN_POINT ( 'NONE',  ( 190.4155215753448829, 300.8376374122118477, -3.221041461475324219 ) ) ;
#75142 = EDGE_CURVE ( 'NONE', #35859, #43346, #26493, .T. ) ;
#75143 = CARTESIAN_POINT ( 'NONE',  ( 71.02572423326354567, 67.25701790933874236, 10.42884077080723237 ) ) ;
#75144 = CARTESIAN_POINT ( 'NONE',  ( 202.8550299997861259, 277.8130222402279514, 15.22080692779638511 ) ) ;
#75145 = CARTESIAN_POINT ( 'NONE',  ( 79.68566563166257311, 45.96296481709465809, 12.95737312212979297 ) ) ;
#75146 = CARTESIAN_POINT ( 'NONE',  ( 199.3292086366563467, 285.3986785392510797, -17.29754939996516683 ) ) ;
#75147 = CARTESIAN_POINT ( 'NONE',  ( 80.91936912787150504, 54.12794304082212449, -16.13542988847117954 ) ) ;
#75148 = VERTEX_POINT ( 'NONE', #88345 ) ;
#75150 = ADVANCED_FACE ( 'NONE', ( #18903 ), #65974, .F. ) ;
#75149 = CARTESIAN_POINT ( 'NONE',  ( 163.4178923001155681, 247.5989030008181260, -10.38047187240561442 ) ) ;
#75151 = LINE ( 'NONE', #50333, #54839 ) ;
#75152 = CARTESIAN_POINT ( 'NONE',  ( 155.6368094659423207, 263.0761338075079721, 17.69820953191020152 ) ) ;
#75153 = CARTESIAN_POINT ( 'NONE',  ( 43.23318412030271674, 205.7677522451419350, -5.000000000000047962 ) ) ;
#75155 = CARTESIAN_POINT ( 'NONE',  ( 120.1739550416679378, 246.3149278399160949, 9.188101187500093303 ) ) ;
#75154 = B_SPLINE_CURVE_WITH_KNOTS ( 'NONE', 3,
 ( #77508, #16190, #39459, #54163 ),
 .UNSPECIFIED., .F., .F.,
 ( 4, 4 ),
 ( 0.04853114605566435924, 0.04887120950165265570 ),
 .UNSPECIFIED. ) ;
#75156 = CARTESIAN_POINT ( 'NONE',  ( 198.9590707264871412, 286.0397762054715827, -17.05306195936250191 ) ) ;
#75157 = ADVANCED_FACE ( 'NONE', ( #61349 ), #45641, .F. ) ;
#75158 = CARTESIAN_POINT ( 'NONE',  ( 87.62133583293774564, 45.31115884160845297, -7.293173845241971875 ) ) ;
#75159 = CARTESIAN_POINT ( 'NONE',  ( 97.88299554183114992, 233.9865022471902876, -10.00000000000009592 ) ) ;
#75160 = CARTESIAN_POINT ( 'NONE',  ( 175.7329799467893849, 253.0876820653997186, -4.805701136885333291 ) ) ;
#75161 = B_SPLINE_CURVE_WITH_KNOTS ( 'NONE', 3,
 ( #86790, #17323, #40614, #56317 ),
 .UNSPECIFIED., .F., .F.,
 ( 4, 4 ),
 ( 0.000000000000000000, 0.0003410592472882656044 ),
 .UNSPECIFIED. ) ;
#75162 = CARTESIAN_POINT ( 'NONE',  ( 34.35668405510998724, 181.4548013555409796, -4.594050593750042211 ) ) ;
#75163 = CARTESIAN_POINT ( 'NONE',  ( 27.58098951138967436, 43.10352854649765675, -10.00000000000000000 ) ) ;
#75164 = ORIENTED_EDGE ( 'NONE', *, *, #97028, .T. ) ;
#75166 = EDGE_CURVE ( 'NONE', #57534, #78966, #91299, .T. ) ;
#75165 = LINE ( 'NONE', #90897, #12288 ) ;
#75167 = CARTESIAN_POINT ( 'NONE',  ( 178.9149973514854537, 265.8180992141078605, 16.19802902779107967 ) ) ;
#75168 = EDGE_CURVE ( 'NONE', #43311, #62454, #3102, .T. ) ;
#75169 = CARTESIAN_POINT ( 'NONE',  ( 69.42787255574388894, 70.69812650043003543, 0.7215327683271423043 ) ) ;
#75170 = CARTESIAN_POINT ( 'NONE',  ( 81.66892272557473120, 41.49682992153503136, -5.273621467921760342 ) ) ;
#75171 = AXIS2_PLACEMENT_3D ( 'NONE', #40651, #56355, #1688 ) ;
#75172 = CARTESIAN_POINT ( 'NONE',  ( 207.1019571622349815, 271.9358831784929293, -5.989975140547304733 ) ) ;
#75173 = CARTESIAN_POINT ( 'NONE',  ( 177.2370279623645501, 286.0837832704111179, -12.08136213241702350 ) ) ;
#75174 = CARTESIAN_POINT ( 'NONE',  ( 164.2180702684029825, 250.0262507739865043, 10.22535470056666540 ) ) ;
#75175 = CARTESIAN_POINT ( 'NONE',  ( 91.22542524669036368, 230.1427522451419065, -10.00000000000009415 ) ) ;
#75176 = B_SPLINE_SURFACE_WITH_KNOTS ( 'NONE', 3, 1, ( 
 ( #97388, #80217 ),
 ( #35057, #11790 ),
 ( #27956, #81707 ),
 ( #3688, #2692 ),
 ( #34567, #57861 ),
 ( #42647, #73579 ),
 ( #4161, #65964 ),
 ( #96916, #58353 ),
 ( #12279, #89331 ),
 ( #43140, #74083 ),
 ( #35563, #76085 ),
 ( #5656, #38537 ),
 ( #69934, #69444 ),
 ( #62838, #16247 ),
 ( #61832, #23334 ),
 ( #47138, #83529 ),
 ( #83031, #84036 ),
 ( #98718, #75916 ),
 ( #68280, #99202 ),
 ( #37866, #74913 ),
 ( #99699, #30286 ),
 ( #61173, #84527 ),
 ( #92141, #22694 ),
 ( #45960, #33281 ),
 ( #55559, #77901 ),
 ( #62162, #8981 ),
 ( #71806, #54063 ),
 ( #93111, #69777 ),
 ( #7997, #386 ),
 ( #8488, #63683 ),
 ( #9497, #77395 ),
 ( #23663, #31274 ),
 ( #40363, #93617 ),
 ( #1396, #54555 ) ),
 .UNSPECIFIED., .T., .F., .F.,
 ( 4, 2, 2, 2, 2, 2, 2, 2, 2, 2, 2, 2, 2, 2, 2, 2, 4 ),
 ( 2, 2 ),
 ( 0.000000000000000000, 0.06250000000000000000, 0.1250000000000000000, 0.1875000000000000000, 0.2500000000000000000, 0.3125000000000000000, 0.3750000000000000000, 0.4375000000000000000, 0.5000000000000000000, 0.5625000000000000000, 0.6250000000000000000, 0.6875000000000000000, 0.7500000000000000000, 0.8125000000000000000, 0.8750000000000000000, 0.9375000000000000000, 1.000000000000000000 ),
 ( 0.000000000000000000, 1.000000000000000000 ),
 .UNSPECIFIED. ) ;
#75177 = ORIENTED_EDGE ( 'NONE', *, *, #41107, .F. ) ;
#75178 = CARTESIAN_POINT ( 'NONE',  ( 79.08643767721621032, 59.41746268492352101, -16.53334974603827945 ) ) ;
#75179 = VECTOR ( 'NONE', #81257, 999.9999999999998863 ) ;
#75180 = CARTESIAN_POINT ( 'NONE',  ( 157.3607188712925620, 280.8594552850489663, -1.588514201417627669 ) ) ;
#75181 = CARTESIAN_POINT ( 'NONE',  ( 154.1399373542834326, 265.3127017963294634, 16.98476250194385884 ) ) ;
#75182 = CARTESIAN_POINT ( 'NONE',  ( 5.317335864756744357, 180.0024278399160949, -9.188101187500093303 ) ) ;
#75183 = CARTESIAN_POINT ( 'NONE',  ( 72.24948267320672812, 68.65699682331809584, -10.35566155590062465 ) ) ;
#75184 = CARTESIAN_POINT ( 'NONE',  ( 196.0836447532441014, 273.4668328341180654, 15.15126769363194015 ) ) ;
#75185 = CARTESIAN_POINT ( 'NONE',  ( 71.63279429240235174, 59.10062218824842972, -15.33079785499452896 ) ) ;
#75186 = CARTESIAN_POINT ( 'NONE',  ( 71.99907712171530250, 72.20780430811404926, -1.638790099443578674 ) ) ;
#75187 = CARTESIAN_POINT ( 'NONE',  ( 54.00411475982191689, 211.1744531367911293, 4.594050593750047540 ) ) ;
#75188 = CARTESIAN_POINT ( 'NONE',  ( 163.7085541710205234, 247.0954618725873217, -6.713544974106887331 ) ) ;
#75189 = CARTESIAN_POINT ( 'NONE',  ( 72.51691088610790814, 57.43791320888536234, 16.30873706240645049 ) ) ;
#75190 = DIRECTION ( 'NONE',  ( -0.000000000000000000, 0.000000000000000000, -1.000000000000000000 ) ) ;
#75191 = CARTESIAN_POINT ( 'NONE',  ( 165.0156970625405108, 244.8314239717225007, -1.890480716182876719 ) ) ;
#75192 = ORIENTED_EDGE ( 'NONE', *, *, #94621, .F. ) ;
#75193 = CARTESIAN_POINT ( 'NONE',  ( 164.7396270603856294, 269.0037874151494179, 17.61975801440670608 ) ) ;
#75194 = CARTESIAN_POINT ( 'NONE',  ( 13.01250597095616612, 184.9865022471903160, 10.00000000000009237 ) ) ;
#75195 = CARTESIAN_POINT ( 'NONE',  ( 164.4678285797544106, 245.7803600197737524, -6.875991496205872799 ) ) ;
#75196 = CARTESIAN_POINT ( 'NONE',  ( 126.7502486777147794, 253.1744531367911009, 4.594050593750047540 ) ) ;
#75197 = CARTESIAN_POINT ( 'NONE',  ( 22.00287929847174695, 28.10171378149919263, 9.188101187500008038 ) ) ;
#75198 = DIRECTION ( 'NONE',  ( -0.3653410243663964274, -0.9308737486442036912, 0.000000000000000000 ) ) ;
#75199 = CARTESIAN_POINT ( 'NONE',  ( 83.77593207218663451, 52.15966500954240104, -15.02877900679588130 ) ) ;
#75201 = CARTESIAN_POINT ( 'NONE',  ( 189.4106793247880489, 289.8710049031299150, 14.49873233045173571 ) ) ;
#75200 = CARTESIAN_POINT ( 'NONE',  ( 81.80775818236242003, 41.72624112066809943, -5.623390783372381740 ) ) ;
#75202 = CARTESIAN_POINT ( 'NONE',  ( 68.43883904695194076, 64.41866838014503571, 12.24487134208069783 ) ) ;
#75203 = ORIENTED_EDGE ( 'NONE', *, *, #57683, .T. ) ;
#75204 = CARTESIAN_POINT ( 'NONE',  ( 79.84392966380758594, 46.37903614055092305, 13.18172969020267793 ) ) ;
#75205 = CARTESIAN_POINT ( 'NONE',  ( 163.6302915796623267, 247.2310166571519687, 7.393723215219985434 ) ) ;
#75206 = DIRECTION ( 'NONE',  ( -0.9874733399847777093, -0.1577859398657163736, 0.000000000000000000 ) ) ;
#75207 = CARTESIAN_POINT ( 'NONE',  ( 169.9431595906827113, 266.1794658690906203, -17.47759505517880285 ) ) ;
#75208 = CARTESIAN_POINT ( 'NONE',  ( 197.3266261510635786, 273.2354618366890691, -13.41124827380268236 ) ) ;
#75209 = VERTEX_POINT ( 'NONE', #52747 ) ;
#75210 = FACE_OUTER_BOUND ( 'NONE', #93907, .T. ) ;
#75211 = CARTESIAN_POINT ( 'NONE',  ( -27.15312891409035601, 106.0554225863516109, 0.000000000000000000 ) ) ;
#75212 = CARTESIAN_POINT ( 'NONE',  ( 79.14312167556931854, 57.64441083166269664, 0.000000000000000000 ) ) ;
#75213 = CARTESIAN_POINT ( 'NONE',  ( 20.85854946042532276, 194.3967562850347122, -4.648177544792955347E-16 ) ) ;
#75214 = CARTESIAN_POINT ( 'NONE',  ( 181.9860418187968492, 295.0310787814198079, 4.802745342729399347 ) ) ;
#75215 = CARTESIAN_POINT ( 'NONE',  ( 69.17578128875754828, 70.38967932611143397, 2.324284992333389699 ) ) ;
#75216 = CARTESIAN_POINT ( 'NONE',  ( 73.93519270231455209, 68.56589142993286146, -10.88456953958179518 ) ) ;
#75217 = CARTESIAN_POINT ( 'NONE',  ( 154.4470374439381146, 277.6591429590598068, -9.115886381272481742 ) ) ;
#75218 = CARTESIAN_POINT ( 'NONE',  ( 16.00201260034520345, 10.20801979619927380, -3.090169943749474069 ) ) ;
#75219 = CARTESIAN_POINT ( 'NONE',  ( 73.00396795756827828, 57.62093675928252878, -16.32480838619500219 ) ) ;
#75220 = ORIENTED_EDGE ( 'NONE', *, *, #46920, .T. ) ;
#75221 = CARTESIAN_POINT ( 'NONE',  ( 58.10966550219799132, 178.3759306620403606, -18.47570218321542868 ) ) ;
#75222 = CARTESIAN_POINT ( 'NONE',  ( 86.55235766077406367, 47.22292317728852140, -10.66532192617878749 ) ) ;
#75223 = CARTESIAN_POINT ( 'NONE',  ( 159.6056220676521207, 264.0888561691485279, -17.76186630473194938 ) ) ;
#75225 = ADVANCED_FACE ( 'NONE', ( #61842 ), #14266, .F. ) ;
#75224 = ORIENTED_EDGE ( 'NONE', *, *, #93275, .F. ) ;
#75226 = CARTESIAN_POINT ( 'NONE',  ( 191.6823192895500370, 298.6434794082964572, -8.424208857102787107 ) ) ;
#75227 = CYLINDRICAL_SURFACE ( 'NONE', #50785, 70.00000000000002842 ) ;
#75228 = CARTESIAN_POINT ( 'NONE',  ( 163.8990931530087494, 246.7654386749614162, 5.873176884778091633 ) ) ;
#75229 = DIRECTION ( 'NONE',  ( -0.8660254037844387076, -0.4999999999999998890, -0.000000000000000000 ) ) ;
#75230 = EDGE_LOOP ( 'NONE', ( #25771, #69545, #87532, #49546 ) ) ;
#75231 = CARTESIAN_POINT ( 'NONE',  ( 89.86341300497758766, 216.5643266524160140, 9.188101187500095079 ) ) ;
#75232 = CARTESIAN_POINT ( 'NONE',  ( 203.2845477157559060, 278.5478302930881682, 14.95601347903707889 ) ) ;
#75233 = CARTESIAN_POINT ( 'NONE',  ( 73.14143739346300777, 69.59972439283021117, -9.872010100564622803 ) ) ;
#75234 = CARTESIAN_POINT ( 'NONE',  ( 177.9267046042368179, 268.9789068694544767, -16.81798070278933821 ) ) ;
#75235 = CARTESIAN_POINT ( 'NONE',  ( 81.32406911314680542, 42.50972318262807192, -7.655652106578362037 ) ) ;
#75236 = VERTEX_POINT ( 'NONE', #67464 ) ;
#75237 = EDGE_CURVE ( 'NONE', #7831, #81147, #92455, .T. ) ;
#75238 = ORIENTED_EDGE ( 'NONE', *, *, #67122, .T. ) ;
#75239 = CARTESIAN_POINT ( 'NONE',  ( -5.625082409869304634, 160.8927522451418213, 10.00000000000009948 ) ) ;
#75240 = EDGE_CURVE ( 'NONE', #56390, #99391, #69594, .T. ) ;
#75241 = ORIENTED_EDGE ( 'NONE', *, *, #48586, .T. ) ;
#75242 = CYLINDRICAL_SURFACE ( 'NONE', #30412, 17.82106496071139645 ) ;
#75243 = VECTOR ( 'NONE', #34503, 1000.000000000000000 ) ;
#75244 = EDGE_LOOP ( 'NONE', ( #15151, #87404, #62215, #25869 ) ) ;
#75245 = CARTESIAN_POINT ( 'NONE',  ( 75.35497918779043403, 60.43207667070393541, 15.59439205038279574 ) ) ;
#75246 = ORIENTED_EDGE ( 'NONE', *, *, #84816, .F. ) ;
#75247 = LINE ( 'NONE', #90484, #23285 ) ;
#75248 = LINE ( 'NONE', #6329, #59494 ) ;
#75249 = LINE ( 'NONE', #68120, #64061 ) ;
#75250 = CARTESIAN_POINT ( 'NONE',  ( 14.81672556217377235, 179.3615022471902591, -10.00000000000009592 ) ) ;
#75251 = VECTOR ( 'NONE', #24845, 1000.000000000000227 ) ;
#75252 = CARTESIAN_POINT ( 'NONE',  ( 82.61003618271377036, 54.05539744841610172, -15.51395791714448968 ) ) ;
#75253 = CARTESIAN_POINT ( 'NONE',  ( 168.2183573306309086, 267.1390863016062553, -17.06247922714877063 ) ) ;
#75254 = EDGE_LOOP ( 'NONE', ( #73951, #96581 ) ) ;
#75255 = FACE_OUTER_BOUND ( 'NONE', #87981, .T. ) ;
#75256 = CARTESIAN_POINT ( 'NONE',  ( 2.953350652821653988, 23.74646525600387648, 2.839279412974139660 ) ) ;
#75257 = ORIENTED_EDGE ( 'NONE', *, *, #43624, .F. ) ;
#75258 = CARTESIAN_POINT ( 'NONE',  ( 166.2739464712248321, 282.9472121807791609, 8.907762031810820602 ) ) ;
#75260 = EDGE_LOOP ( 'NONE', ( #95507, #50465, #95331, #3092, #83013 ) ) ;
#75259 = DIRECTION ( 'NONE',  ( 0.5000000000000013323, -0.8660254037844378194, 0.000000000000000000 ) ) ;
#75261 = CARTESIAN_POINT ( 'NONE',  ( 162.6220573360242270, 248.9773295930640131, 10.49878733418918486 ) ) ;
#75262 = CARTESIAN_POINT ( 'NONE',  ( 188.2323859076021222, 260.7681868484680763, 2.706230261455492059 ) ) ;
#75263 = CARTESIAN_POINT ( 'NONE',  ( 149.5706976103993782, 276.2301179004945197, -5.400069381014914960 ) ) ;
#75264 = DIRECTION ( 'NONE',  ( -0.8660254037844387076, -0.4999999999999998890, -0.000000000000000000 ) ) ;
#75265 = CARTESIAN_POINT ( 'NONE',  ( 27.76992210170820030, 43.29297894285232928, -10.00000000000000000 ) ) ;
#75266 = CARTESIAN_POINT ( 'NONE',  ( 168.1614549503004525, 252.8790457503890536, 11.93473075534227057 ) ) ;
#75267 = LINE ( 'NONE', #74290, #1152 ) ;
#75268 = VERTEX_POINT ( 'NONE', #13766 ) ;
#75270 = EDGE_CURVE ( 'NONE', #18761, #31643, #93722, .T. ) ;
#75269 = CARTESIAN_POINT ( 'NONE',  ( 181.8129518053731033, 270.5384970965435514, -17.23398818032472946 ) ) ;
#75271 = CARTESIAN_POINT ( 'NONE',  ( 74.74960108721565177, 62.34916436530387784, -14.94383104034243814 ) ) ;
#75272 = ORIENTED_EDGE ( 'NONE', *, *, #46143, .F. ) ;
#75273 = CARTESIAN_POINT ( 'NONE',  ( 11.37297787527554327, 165.8262482093457777, 3.021315404115420679E-15 ) ) ;
#75274 = CARTESIAN_POINT ( 'NONE',  ( -3.532187684056895538, 158.7677522451418213, -5.000000000000041744 ) ) ;
#75275 = EDGE_CURVE ( 'NONE', #100037, #99756, #90131, .T. ) ;
#75276 = CARTESIAN_POINT ( 'NONE',  ( 193.1480066626644714, 267.5100469937302137, -10.98767188462725386 ) ) ;
#75277 = EDGE_CURVE ( 'NONE', #7578, #59740, #22361, .T. ) ;
#75278 = CARTESIAN_POINT ( 'NONE',  ( 204.2488672143813346, 276.8775799267394291, -15.19253025301563831 ) ) ;
#75279 = CARTESIAN_POINT ( 'NONE',  ( 172.0775005200765406, 286.7165937425170341, -10.58237651954697078 ) ) ;
#75280 = CARTESIAN_POINT ( 'NONE',  ( 161.3261849411383650, 273.2032229615781489, 15.91718547624222957 ) ) ;
#75282 = CARTESIAN_POINT ( 'NONE',  ( 24.50477583610994259, 37.08080186712593473, -3.090169943749475845 ) ) ;
#75281 = CARTESIAN_POINT ( 'NONE',  ( -9.107486540969064848, 174.7369531367911293, -4.594050593750048428 ) ) ;
#75283 = AXIS2_PLACEMENT_3D ( 'NONE', #93045, #53515, #54493 ) ;
#75284 = CARTESIAN_POINT ( 'NONE',  ( 185.0535551050948868, 295.3960374749880771, 8.450267053739612066 ) ) ;
#75285 = EDGE_LOOP ( 'NONE', ( #44787, #98798, #46003, #69485 ) ) ;
#75286 = EDGE_CURVE ( 'NONE', #61039, #96078, #70701, .T. ) ;
#75287 = ORIENTED_EDGE ( 'NONE', *, *, #56923, .F. ) ;
#75288 = DIRECTION ( 'NONE',  ( -0.000000000000000000, 0.000000000000000000, -1.000000000000000000 ) ) ;
#75289 = LINE ( 'NONE', #69650, #82049 ) ;
#75290 = EDGE_CURVE ( 'NONE', #75472, #97425, #85758, .T. ) ;
#75291 = CARTESIAN_POINT ( 'NONE',  ( 185.2824853868734181, 297.7695098558858149, 4.231266468330407093 ) ) ;
#75292 = CARTESIAN_POINT ( 'NONE',  ( 175.4037125437872362, 291.3959072482493298, 3.423790665827645352 ) ) ;
#75293 = CARTESIAN_POINT ( 'NONE',  ( 85.18020382826158254, 42.46978738886356552, 0.9382811178248954276 ) ) ;
#75294 = CARTESIAN_POINT ( 'NONE',  ( 163.2084678683261814, 247.9616367570234559, -11.19269778657885972 ) ) ;
#75295 = CARTESIAN_POINT ( 'NONE',  ( 83.36075103893979588, 44.36208028417300397, 8.738630005962992442 ) ) ;
#75296 = CARTESIAN_POINT ( 'NONE',  ( 153.5742155153078272, 278.9749726662499825, 3.791783021084301097 ) ) ;
#75297 = CARTESIAN_POINT ( 'NONE',  ( 30.59497298136257726, 176.2202760586659736, -5.415160957724236172E-17 ) ) ;
#75298 = CARTESIAN_POINT ( 'NONE',  ( 118.1982478153434357, 248.2369531367911293, -4.594050593750048428 ) ) ;
#75299 = CARTESIAN_POINT ( 'NONE',  ( 87.75630041960181416, 44.40081992046322057, -3.969603809391093474 ) ) ;
#75300 = CARTESIAN_POINT ( 'NONE',  ( 182.9052583267165915, 257.6403021703982290, -2.314827183511977360 ) ) ;
#75301 = CARTESIAN_POINT ( 'NONE',  ( 78.65335153445595040, 54.31254791370685098, 15.95818423819602216 ) ) ;
#75302 = CARTESIAN_POINT ( 'NONE',  ( 175.7813307086614714, 281.8375084945754452, -14.19557829653598979 ) ) ;
#75303 = CARTESIAN_POINT ( 'NONE',  ( 83.61754957953866096, 52.24592005514148951, -14.70745080183156972 ) ) ;
#75304 = CARTESIAN_POINT ( 'NONE',  ( 182.7190055043868142, 259.1992038300794547, 9.912833159430794794 ) ) ;
#75305 = CARTESIAN_POINT ( 'NONE',  ( 183.9464132997153456, 275.0587871046172950, 16.36209078982390963 ) ) ;
#75306 = CARTESIAN_POINT ( 'NONE',  ( 194.1789525331299728, 294.3191837825503967, -15.34533909744314961 ) ) ;
#75307 = CARTESIAN_POINT ( 'NONE',  ( 70.56051678902534263, 60.79552409407079949, -14.52389266189133998 ) ) ;
#75308 = CARTESIAN_POINT ( 'NONE',  ( 84.64741752562134991, 50.25350151326510684, 13.85721388315136693 ) ) ;
#75309 = DIRECTION ( 'NONE',  ( 1.000000000000000000, 0.000000000000000000, 0.000000000000000000 ) ) ;
#75310 = CARTESIAN_POINT ( 'NONE',  ( 51.18979252112020362, 200.3615022471902307, -10.00000000000009592 ) ) ;
#75311 = CARTESIAN_POINT ( 'NONE',  ( 183.2174363127404320, 268.2244215103378338, -14.94466466708451158 ) ) ;
#75312 = LINE ( 'NONE', #82935, #20598 ) ;
#75313 = CARTESIAN_POINT ( 'NONE',  ( 172.5095176311965872, 263.6581028672348452, -15.42591371060134264 ) ) ;
#75314 = EDGE_CURVE ( 'NONE', #38232, #54274, #6102, .T. ) ;
#75315 = CARTESIAN_POINT ( 'NONE',  ( 104.3964885861764600, 221.8923013555410080, 4.594050593750050204 ) ) ;
#75316 = CARTESIAN_POINT ( 'NONE',  ( 8.584303441219292452, 23.14336893147753571, 7.433330006724141015 ) ) ;
#75318 = CARTESIAN_POINT ( 'NONE',  ( 190.8094645593471341, 300.1553081486349015, 8.399847186519689757 ) ) ;
#75317 = AXIS2_PLACEMENT_3D ( 'NONE', #28455, #49774, #81710 ) ;
#75319 = DIRECTION ( 'NONE',  ( 0.3400251696390308997, -0.9404163354663445107, 0.000000000000000000 ) ) ;
#75321 = CARTESIAN_POINT ( 'NONE',  ( 84.43425781732527469, 42.39747773327804481, -3.149235988505898476 ) ) ;
#75320 = CARTESIAN_POINT ( 'NONE',  ( 196.1613785401733878, 290.8855212161054737, 15.98157687694135021 ) ) ;
#75322 = DIRECTION ( 'NONE',  ( 0.4999999999999992784, -0.8660254037844390407, 0.000000000000000000 ) ) ;
#75323 = CARTESIAN_POINT ( 'NONE',  ( 151.2964716097791325, 268.5938194963972592, -15.66250187539618111 ) ) ;
#75324 = CARTESIAN_POINT ( 'NONE',  ( 162.9254136962317148, 277.9293967287522946, 13.77390558128574760 ) ) ;
#75325 = CARTESIAN_POINT ( 'NONE',  ( 43.77620770598743150, 30.98920272979930601, 7.433330006724137462 ) ) ;
#75326 = CARTESIAN_POINT ( 'NONE',  ( -19.79170892150624894, 93.03488659321679677, 59.99999999999999289 ) ) ;
#75327 = CARTESIAN_POINT ( 'NONE',  ( 48.43557798863805886, 76.81918075477977936, 10.00000000000000000 ) ) ;
#75328 = ORIENTED_EDGE ( 'NONE', *, *, #21916, .F. ) ;
#75329 = CARTESIAN_POINT ( 'NONE',  ( 20.05074681235918277, 34.68290643055188127, 3.479690158560446702E-15 ) ) ;
#75330 = PLANE ( 'NONE',  #49113 ) ;
#75331 = CARTESIAN_POINT ( 'NONE',  ( 196.8537322840589070, 267.5011318901352411, 9.757633572797876909 ) ) ;
#75332 = CARTESIAN_POINT ( 'NONE',  ( 191.6653133782924670, 287.8825534954372642, -15.84478586218862262 ) ) ;
#75333 = CARTESIAN_POINT ( 'NONE',  ( 70.47930578771455146, 60.95205399099343424, 14.96696578811553735 ) ) ;
#75334 = CARTESIAN_POINT ( 'NONE',  ( 159.6978881494930249, 254.0421391940632532, 15.34888828951022610 ) ) ;
#75335 = CARTESIAN_POINT ( 'NONE',  ( 73.67706877977251168, 59.42851455646710690, 16.04744940023546818 ) ) ;
#75336 = CARTESIAN_POINT ( 'NONE',  ( 169.4318521445344174, 252.1923235025763574, -8.759566905232736289 ) ) ;
#75338 =( BOUNDED_CURVE ( )  B_SPLINE_CURVE ( 2, ( #68469, #22870, #69471, #46151, #99397, #29975, #91816, #14775, #91315, #53755, #61857, #90838, #21389 ),
 .UNSPECIFIED., .F., .T. ) 
 B_SPLINE_CURVE_WITH_KNOTS ( ( 3, 2, 2, 2, 2, 2, 3 ),
 ( 0.5625000000000000000, 0.5649999999999999467, 0.5699999999999999512, 0.5749999999999999556, 0.5799999999999999600, 0.5849999999999999645, 0.5875000000000000222 ),
 .UNSPECIFIED. ) 
 CURVE ( )  GEOMETRIC_REPRESENTATION_ITEM ( )  RATIONAL_B_SPLINE_CURVE ( ( 0.9755282581475768211, 0.9755282581475768211, 1.000000000000000000, 0.9510565162951535312, 1.000000000000000000, 0.9510565162951535312, 1.000000000000000000, 0.9510565162951535312, 1.000000000000000000, 0.9510565162951535312, 1.000000000000000000, 0.9755282581475761550, 0.9755282581475767101 ) ) 
 REPRESENTATION_ITEM ( '' )  );
#75337 = CARTESIAN_POINT ( 'NONE',  ( 129.2042476453683264, 258.7365022471903444, 2.944929066748280225E-16 ) ) ;
#75339 = DIRECTION ( 'NONE',  ( -0.8660254037844359321, -0.5000000000000051070, -0.000000000000000000 ) ) ;
#75340 = ORIENTED_EDGE ( 'NONE', *, *, #40958, .F. ) ;
#75341 = CARTESIAN_POINT ( 'NONE',  ( 70.98573842219099106, 65.83761980621460452, 12.30238249020369423 ) ) ;
#75342 = EDGE_LOOP ( 'NONE', ( #46170, #51642, #8297, #21628 ) ) ;
#75343 = CARTESIAN_POINT ( 'NONE',  ( 196.4555699717270159, 265.3045897231015147, -4.475125793179218547 ) ) ;
#75344 = CARTESIAN_POINT ( 'NONE',  ( 85.17037076274338858, 42.84250995736751833, 3.387596126962762355 ) ) ;
#75345 = ORIENTED_EDGE ( 'NONE', *, *, #55656, .T. ) ;
#75346 = CARTESIAN_POINT ( 'NONE',  ( 181.5586684916292199, 291.2330295745708781, -11.30866533355154857 ) ) ;
#75348 = ADVANCED_FACE ( 'NONE', ( #63122 ), #54495, .T. ) ;
#75347 = ORIENTED_EDGE ( 'NONE', *, *, #30973, .T. ) ;
#75349 = FACE_OUTER_BOUND ( 'NONE', #91184, .T. ) ;
#75350 = CARTESIAN_POINT ( 'NONE',  ( 205.7652784884614618, 274.2510785548626586, 10.78649346335630632 ) ) ;
#75351 = CARTESIAN_POINT ( 'NONE',  ( 190.8346167705416292, 278.0885925990914984, -16.91238342368501080 ) ) ;
#75352 = CARTESIAN_POINT ( 'NONE',  ( 153.9376410758373197, 264.0191797897847437, -17.98316443701128264 ) ) ;
#75353 = CARTESIAN_POINT ( 'NONE',  ( 200.9521687275011175, 282.5876292032514243, -18.16013154125647944 ) ) ;
#75354 = AXIS2_PLACEMENT_3D ( 'NONE', #61151, #12212, #12723 ) ;
#75355 = CARTESIAN_POINT ( 'NONE',  ( 39.71190250773520347, 34.87878583063844928, -9.188101187500006262 ) ) ;
#75356 = CARTESIAN_POINT ( 'NONE',  ( 78.31430634746025987, 58.80323091815131420, -16.15417916714726587 ) ) ;
#75358 = EDGE_CURVE ( 'NONE', #18338, #34850, #84961, .T. ) ;
#75357 = DIRECTION ( 'NONE',  ( -1.000000000000000000, 0.000000000000000000, 0.000000000000000000 ) ) ;
#75359 =( BOUNDED_CURVE ( )  B_SPLINE_CURVE ( 2, ( #89815, #20390, #51261, #82225, #26988, #96928, #19415, #41668, #73590, #95933, #12799, #12291, #4170 ),
 .UNSPECIFIED., .F., .T. ) 
 B_SPLINE_CURVE_WITH_KNOTS ( ( 3, 2, 2, 2, 2, 2, 3 ),
 ( 0.4375000000000000000, 0.4400000000000000022, 0.4450000000000000067, 0.4500000000000000111, 0.4550000000000000155, 0.4600000000000000200, 0.4625000000000000222 ),
 .UNSPECIFIED. ) 
 CURVE ( )  GEOMETRIC_REPRESENTATION_ITEM ( )  RATIONAL_B_SPLINE_CURVE ( ( 0.9755282581475768211, 0.9755282581475768211, 1.000000000000000000, 0.9510565162951535312, 1.000000000000000000, 0.9510565162951535312, 1.000000000000000000, 0.9510565162951535312, 1.000000000000000000, 0.9510565162951535312, 1.000000000000000000, 0.9755282581475768211, 0.9755282581475768211 ) ) 
 REPRESENTATION_ITEM ( '' )  );
#75361 = VECTOR ( 'NONE', #10583, 1000.000000000000114 ) ;
#75360 = DIRECTION ( 'NONE',  ( 1.082076799516502080E-16, 0.000000000000000000, 1.000000000000000000 ) ) ;
#75362 = EDGE_CURVE ( 'NONE', #1759, #35085, #32219, .T. ) ;
#75363 = VERTEX_POINT ( 'NONE', #40303 ) ;
#75364 = ORIENTED_EDGE ( 'NONE', *, *, #14892, .T. ) ;
#75365 = CARTESIAN_POINT ( 'NONE',  ( 87.22108034532067222, 46.19249316086605006, -9.000540691006557736 ) ) ;
#75367 = CARTESIAN_POINT ( 'NONE',  ( 164.9505546126307820, 273.5171455901430591, -15.23424786856183211 ) ) ;
#75366 = CARTESIAN_POINT ( 'NONE',  ( 174.5008544261717134, 257.2940615678410268, -12.04793888739825114 ) ) ;
#75368 = CARTESIAN_POINT ( 'NONE',  ( 179.3609674101392670, 270.6429099854789229, -17.53201452148147865 ) ) ;
#75369 = CARTESIAN_POINT ( 'NONE',  ( 197.4318886344639168, 273.2323872680082104, -13.37235133448358582 ) ) ;
#75370 = CARTESIAN_POINT ( 'NONE',  ( 82.10283259859586735, 40.80311082331518691, 1.497507696010887512 ) ) ;
#75371 = CARTESIAN_POINT ( 'NONE',  ( 167.5062897759243867, 286.2136144727477927, -4.753602936323340522 ) ) ;
#75372 = CARTESIAN_POINT ( 'NONE',  ( 77.00910850481052705, 63.69207575539577704, -14.97815254220546954 ) ) ;
#75373 = CARTESIAN_POINT ( 'NONE',  ( 181.8753390830952981, 257.0193592213445868, 5.050065929983023949 ) ) ;
#75374 = CARTESIAN_POINT ( 'NONE',  ( 111.1892885731694065, 228.8768266524159856, -9.188101187500091527 ) ) ;
#75375 = ORIENTED_EDGE ( 'NONE', *, *, #16957, .T. ) ;
#75376 = DIRECTION ( 'NONE',  ( -1.000000000000000000, 0.000000000000000000, 0.000000000000000000 ) ) ;
#75377 = CARTESIAN_POINT ( 'NONE',  ( 191.5502192675250797, 274.9178017426596057, 16.83841206479500840 ) ) ;
#75378 = VERTEX_POINT ( 'NONE', #32718 ) ;
#75379 = AXIS2_PLACEMENT_3D ( 'NONE', #19488, #27063, #4763 ) ;
#75380 = CARTESIAN_POINT ( 'NONE',  ( 74.06641568892433725, 68.90029856846140888, -11.17356148674937444 ) ) ;
#75381 = CARTESIAN_POINT ( 'NONE',  ( 164.4115384698665423, 246.2497411554974178, -2.154666020448770425 ) ) ;
#75382 = CARTESIAN_POINT ( 'NONE',  ( 196.4677418905696129, 290.3548843276421394, 17.08610552292358520 ) ) ;
#75383 = CARTESIAN_POINT ( 'NONE',  ( 68.83415823943913381, 70.27335860090030906, 4.117195521840038452 ) ) ;
#75384 = CARTESIAN_POINT ( 'NONE',  ( 74.24029763082349120, 55.47955095029949746, -16.12046342301015756 ) ) ;
#75385 = ORIENTED_EDGE ( 'NONE', *, *, #50876, .F. ) ;
#75386 = VECTOR ( 'NONE', #55500, 999.9999999999998863 ) ;
#75387 = ORIENTED_EDGE ( 'NONE', *, *, #15980, .F. ) ;
#75388 = ADVANCED_FACE ( 'NONE', ( #77842 ), #63620, .T. ) ;
#75389 = CARTESIAN_POINT ( 'NONE',  ( 37.58366506746438773, 204.0530062829863027, 1.101618078115930403E-13 ) ) ;
#75390 = ORIENTED_EDGE ( 'NONE', *, *, #48031, .F. ) ;
#75391 = CARTESIAN_POINT ( 'NONE',  ( 192.1803104008425009, 263.7327182331824815, -8.277698982533909344 ) ) ;
#75392 = CARTESIAN_POINT ( 'NONE',  ( 156.0770925354950407, 262.0035003640769560, 17.00396438526712828 ) ) ;
#75393 = CARTESIAN_POINT ( 'NONE',  ( 83.70131808852121935, 48.44858958261185933, 12.58427742406832905 ) ) ;
#75395 = DIRECTION ( 'NONE',  ( -0.7299047266382303611, 0.6835488936653839609, 0.000000000000000000 ) ) ;
#75394 = CARTESIAN_POINT ( 'NONE',  ( 132.0211419364472363, 235.4824982072973683, 3.021315404115420679E-15 ) ) ;
#75396 = CARTESIAN_POINT ( 'NONE',  ( 201.1060504099706350, 282.3210983108598384, -18.18000168485860257 ) ) ;
#75397 = VERTEX_POINT ( 'NONE', #38310 ) ;
#75398 = CARTESIAN_POINT ( 'NONE',  ( 147.2494378675467033, 275.6034875578896504, 3.639370109197119341 ) ) ;
#75399 = CARTESIAN_POINT ( 'NONE',  ( 81.78459505290653908, 48.88907504212919974, 13.50450084590696953 ) ) ;
#75400 = CARTESIAN_POINT ( 'NONE',  ( 82.40024631258233967, 41.31310794220259197, -3.382981533264477036 ) ) ;
#75401 = EDGE_CURVE ( 'NONE', #7307, #37182, #88911, .T. ) ;
#75402 = CARTESIAN_POINT ( 'NONE',  ( 73.27328646083023500, 70.16270934360544231, -9.274526489422585840 ) ) ;
#75403 = CARTESIAN_POINT ( 'NONE',  ( 192.8280828621116143, 271.6925081571723695, -14.86971951722050989 ) ) ;
#75404 = LINE ( 'NONE', #92138, #37054 ) ;
#75405 = CARTESIAN_POINT ( 'NONE',  ( 84.00948332465746660, 44.55099784152547215, 8.476636100854188172 ) ) ;
#75406 = CARTESIAN_POINT ( 'NONE',  ( 122.0674962994202275, 252.8297689869269504, -2.679491924311252493 ) ) ;
#75407 = CARTESIAN_POINT ( 'NONE',  ( 191.3433485266361060, 283.5098745242009386, -16.59037939125511230 ) ) ;
#75408 = CARTESIAN_POINT ( 'NONE',  ( 66.79485077809044924, 69.14189238270698468, -0.3922495213730473607 ) ) ;
#75409 = CARTESIAN_POINT ( 'NONE',  ( 83.72013207082297015, 209.9548013555409796, -4.594050593750042211 ) ) ;
#75410 = CARTESIAN_POINT ( 'NONE',  ( 159.2713554375903300, 254.7809155221686410, -15.70062444474382168 ) ) ;
#75411 = CARTESIAN_POINT ( 'NONE',  ( 77.84925963432132789, 61.76067837358136359, 16.06420508523131474 ) ) ;
#75412 = CARTESIAN_POINT ( 'NONE',  ( 162.7738416911812180, 248.7144313781379310, -11.09964294874192525 ) ) ;
#75413 = ADVANCED_FACE ( 'NONE', ( #8922 ), #70721, .T. ) ;
#75414 = VECTOR ( 'NONE', #100205, 999.9999999999998863 ) ;
#75415 = CARTESIAN_POINT ( 'NONE',  ( 207.7320178805681508, 270.8445860024863237, -5.379955943374661764 ) ) ;
#75416 = DIRECTION ( 'NONE',  ( -1.000000000000000000, 0.000000000000000000, 0.000000000000000000 ) ) ;
#75417 = CARTESIAN_POINT ( 'NONE',  ( 185.9122197414204720, 265.5112680014551074, 13.45063299295054016 ) ) ;
#75418 = CARTESIAN_POINT ( 'NONE',  ( 118.8119427999551476, 232.7365022471901739, -10.00000000000009237 ) ) ;
#75419 = CARTESIAN_POINT ( 'NONE',  ( 43.54162044069033755, 26.10801979619932567, 3.090169943749476733 ) ) ;
#75420 = CARTESIAN_POINT ( 'NONE',  ( 73.38975662564067193, 58.44531319176417128, -16.23198634866734125 ) ) ;
#75421 = CARTESIAN_POINT ( 'NONE',  ( 157.7367892284080995, 270.6845674506320165, -15.10799881823672131 ) ) ;
#75422 = VECTOR ( 'NONE', #52921, 1000.000000000000114 ) ;
#75423 = CARTESIAN_POINT ( 'NONE',  ( 72.08446838866018425, 72.31872904169155447, 3.483634709754487080 ) ) ;
#75424 = EDGE_CURVE ( 'NONE', #33343, #91371, #56656, .T. ) ;
#75425 = EDGE_CURVE ( 'NONE', #98025, #8702, #56586, .T. ) ;
#75426 = CARTESIAN_POINT ( 'NONE',  ( -19.65312891409030271, 93.06504152958497400, -10.00000000000000888 ) ) ;
#75427 = DIRECTION ( 'NONE',  ( 0.000000000000000000, -0.000000000000000000, -1.000000000000000000 ) ) ;
#75428 = FACE_OUTER_BOUND ( 'NONE', #7457, .T. ) ;
#75429 = CARTESIAN_POINT ( 'NONE',  ( 71.81907866082414671, 72.09960760913652678, -1.684840435608867759 ) ) ;
#75430 = CARTESIAN_POINT ( 'NONE',  ( 56.62968813474974894, 197.3768266524159856, -9.188101187500093303 ) ) ;
#75431 = CARTESIAN_POINT ( 'NONE',  ( 24.63222838094502265, 17.14754757982090538, -5.678558825948275768 ) ) ;
#75432 = CARTESIAN_POINT ( 'NONE',  ( 171.3915261951946150, 286.6500415720103092, 7.434736897587270299 ) ) ;
#75433 = CARTESIAN_POINT ( 'NONE',  ( -12.46307465703604400, 163.6115022471902591, 10.00000000000009592 ) ) ;
#75434 = CARTESIAN_POINT ( 'NONE',  ( 36.46445469440066489, 39.79103043416552055, 8.090169943749478065 ) ) ;
#75435 = CARTESIAN_POINT ( 'NONE',  ( 202.9485587013432450, 270.0648872230868278, -6.527258153556268816 ) ) ;
#75436 = CARTESIAN_POINT ( 'NONE',  ( 76.37262670668393127, 61.51550187027301320, 15.91785308945339494 ) ) ;
#75437 = AXIS2_PLACEMENT_3D ( 'NONE', #20949, #82279, #72283 ) ;
#75438 = CARTESIAN_POINT ( 'NONE',  ( 176.4777781830643733, 275.0219395333674584, 16.71559492492674437 ) ) ;
#75439 = CARTESIAN_POINT ( 'NONE',  ( 182.1775460995084188, 281.0620400832397081, -16.66492851291912203 ) ) ;
#75440 = CARTESIAN_POINT ( 'NONE',  ( 68.30469270138026161, 67.85665571424478060, -7.560265020520116508 ) ) ;
#75441 = CARTESIAN_POINT ( 'NONE',  ( 192.1779685593947420, 266.1842805242176269, 11.64530923862864142 ) ) ;
#75442 = CARTESIAN_POINT ( 'NONE',  ( 82.30057295520377636, 41.22186192095817603, 3.240003865797013383 ) ) ;
#75443 = CARTESIAN_POINT ( 'NONE',  ( 87.76310869853918462, 45.07707962072153407, -6.704660406813174767 ) ) ;
#75444 = CARTESIAN_POINT ( 'NONE',  ( 103.0791479645378814, 216.9865022471901455, 1.119607411625061291E-15 ) ) ;
#75445 = CARTESIAN_POINT ( 'NONE',  ( 200.7079229450794173, 283.0106753079404029, 16.90512463913211505 ) ) ;
#75446 = CARTESIAN_POINT ( 'NONE',  ( 165.2257725011909599, 269.6626922470395016, -16.28745125698258889 ) ) ;
#75447 = ORIENTED_EDGE ( 'NONE', *, *, #29165, .F. ) ;
#75448 = CARTESIAN_POINT ( 'NONE',  ( 55.49285624440017273, 202.8458772461660260, 9.188101187500095079 ) ) ;
#75449 = ORIENTED_EDGE ( 'NONE', *, *, #26886, .T. ) ;
#75450 = CARTESIAN_POINT ( 'NONE',  ( 166.2024314945517744, 265.3097119368810581, 16.55270856133939006 ) ) ;
#75451 = CARTESIAN_POINT ( 'NONE',  ( -32.86949478547433046, 94.43171332246730287, 43.89948692389422291 ) ) ;
#75452 = PLANE ( 'NONE',  #54761 ) ;
#75453 = ORIENTED_EDGE ( 'NONE', *, *, #80226, .T. ) ;
#75454 = CARTESIAN_POINT ( 'NONE',  ( 175.5738744261513773, 288.6452583002058532, 10.69039192277817207 ) ) ;
#75455 = CARTESIAN_POINT ( 'NONE',  ( 79.23893794663464973, 46.12127630347242757, -13.23827507291852434 ) ) ;
#75456 = B_SPLINE_CURVE_WITH_KNOTS ( 'NONE', 3,
 ( #9979, #41349, #8466, #25678 ),
 .UNSPECIFIED., .F., .F.,
 ( 4, 4 ),
 ( 0.006801831041879702333, 0.01491549308688025835 ),
 .UNSPECIFIED. ) ;
#75457 = CARTESIAN_POINT ( 'NONE',  ( 23.75126848931443746, 37.21091486745861943, 7.012934429366973338E-14 ) ) ;
#75458 = CARTESIAN_POINT ( 'NONE',  ( 175.8941769947522005, 273.9942606850552238, -16.49495549152694451 ) ) ;
#75459 = CARTESIAN_POINT ( 'NONE',  ( 206.7093368940924449, 271.6371694531807748, -6.526174084559485777 ) ) ;
#75460 = CARTESIAN_POINT ( 'NONE',  ( 204.2992694100975939, 276.7902807629455992, 13.99537586056731620 ) ) ;
#75461 = ORIENTED_EDGE ( 'NONE', *, *, #86860, .F. ) ;
#75462 = CARTESIAN_POINT ( 'NONE',  ( 17.35762855594305520, 30.99752408145591431, 5.678558825948276656 ) ) ;
#75463 = CARTESIAN_POINT ( 'NONE',  ( 76.24236140527241901, 61.49608671980659835, 15.50578537986026539 ) ) ;
#75464 = CARTESIAN_POINT ( 'NONE',  ( 68.55793687630249167, 69.78307366813099577, -3.432291385973068820 ) ) ;
#75465 = CARTESIAN_POINT ( 'NONE',  ( 75.32733269473096982, 66.70192330152532634, -13.01492205759767629 ) ) ;
#75466 = ORIENTED_EDGE ( 'NONE', *, *, #68274, .T. ) ;
#75468 = EDGE_CURVE ( 'NONE', #22518, #6816, #18100, .T. ) ;
#75467 = CARTESIAN_POINT ( 'NONE',  ( 182.1942909992290254, 284.0346785242947476, 14.95718866600176966 ) ) ;
#75469 = CARTESIAN_POINT ( 'NONE',  ( 33.30115378465513487, 95.78395070760240060, 59.99999999999999289 ) ) ;
#75470 = EDGE_CURVE ( 'NONE', #39284, #79412, #5402, .T. ) ;
#75471 = ORIENTED_EDGE ( 'NONE', *, *, #85667, .T. ) ;
#75472 = VERTEX_POINT ( 'NONE', #73786 ) ;
#75474 = CARTESIAN_POINT ( 'NONE',  ( 60.19284827774804114, 198.8927522451417644, -10.00000000000009237 ) ) ;
#75473 = CARTESIAN_POINT ( 'NONE',  ( 159.2847755103654777, 282.3438696241352659, -3.266643173123188415 ) ) ;
#75475 = CARTESIAN_POINT ( 'NONE',  ( 162.7459776558209228, 248.7626933030860812, -9.895605163646791880 ) ) ;
#75476 = CARTESIAN_POINT ( 'NONE',  ( 164.1224127655298730, 246.3786377597482158, 7.356982420601481998 ) ) ;
#75477 = EDGE_CURVE ( 'NONE', #38318, #60221, #79337, .T. ) ;
#75478 = CARTESIAN_POINT ( 'NONE',  ( 159.9307118030769175, 253.6388767968520881, 16.60600887889890487 ) ) ;
#75479 = CARTESIAN_POINT ( 'NONE',  ( 81.89559477234445239, 55.33976261442212774, 16.26127046582525892 ) ) ;
#75480 = CARTESIAN_POINT ( 'NONE',  ( 161.0194789840985550, 262.9636063602296758, -17.49589281607644864 ) ) ;
#75481 = EDGE_CURVE ( 'NONE', #77239, #68127, #77899, .T. ) ;
#75482 = CARTESIAN_POINT ( 'NONE',  ( 125.6141109788952122, 234.1423013555409796, -4.594050593750043987 ) ) ;
#75483 = CARTESIAN_POINT ( 'NONE',  ( 75.14063404487711750, 220.3149278399160664, -9.188101187500095079 ) ) ;
#75484 = ORIENTED_EDGE ( 'NONE', *, *, #31894, .F. ) ;
#75485 = CARTESIAN_POINT ( 'NONE',  ( 170.5242561500533895, 263.7951878494171183, 15.83046558349961863 ) ) ;
#75486 = CARTESIAN_POINT ( 'NONE',  ( 79.70677143361787387, 46.01134058561531504, 12.98241517792750699 ) ) ;
#75487 = AXIS2_PLACEMENT_3D ( 'NONE', #54251, #85222, #46674 ) ;
#75488 = CARTESIAN_POINT ( 'NONE',  ( 160.3453973192849276, 253.3356115996859899, 14.63839832439733968 ) ) ;
#75489 = VECTOR ( 'NONE', #52062, 1000.000000000000114 ) ;
#75490 = VERTEX_POINT ( 'NONE', #76757 ) ;
#75491 = ORIENTED_EDGE ( 'NONE', *, *, #89260, .T. ) ;
#75492 = CARTESIAN_POINT ( 'NONE',  ( 76.25214315863026115, 65.18377266038437767, 14.56725100193072109 ) ) ;
#75493 = CARTESIAN_POINT ( 'NONE',  ( 195.2631479605611560, 291.6323043634218379, -15.73646530299744839 ) ) ;
#75494 = CARTESIAN_POINT ( 'NONE',  ( -6.583630525541995127, 178.5530062829863027, -4.648177544792955347E-16 ) ) ;
#75495 = CARTESIAN_POINT ( 'NONE',  ( 147.2405539530007559, 275.6188749492528132, 0.4306668706573002492 ) ) ;
#75496 = PLANE ( 'NONE',  #54688 ) ;
#75497 = CARTESIAN_POINT ( 'NONE',  ( 193.9844289374573520, 294.6561085335266625, 15.49818881749970245 ) ) ;
#75498 = VECTOR ( 'NONE', #73378, 999.9999999999998863 ) ;
#75499 = CARTESIAN_POINT ( 'NONE',  ( 71.91558025072355065, 67.94660262428635633, 10.25156427071338605 ) ) ;
#75500 = CARTESIAN_POINT ( 'NONE',  ( 87.77058453035330388, 45.11289234403166404, 6.766180878992243741 ) ) ;
#75501 = ORIENTED_EDGE ( 'NONE', *, *, #66557, .T. ) ;
#75502 = CARTESIAN_POINT ( 'NONE',  ( 153.3544108199959908, 265.0293642254135307, -17.49105661178601423 ) ) ;
#75503 = CARTESIAN_POINT ( 'NONE',  ( 185.0684497205900527, 286.3477220876792444, 16.15350733335134237 ) ) ;
#75504 = ORIENTED_EDGE ( 'NONE', *, *, #52812, .F. ) ;
#75505 = CARTESIAN_POINT ( 'NONE',  ( -17.09196077473970021, 172.4860189848785410, -2.679491924311252049 ) ) ;
#75506 = CARTESIAN_POINT ( 'NONE',  ( 76.06558573277115443, 51.36628043362249230, -15.65277118209960250 ) ) ;
#75507 = DIRECTION ( 'NONE',  ( 0.000000000000000000, 0.000000000000000000, 1.000000000000000000 ) ) ;
#75508 = CARTESIAN_POINT ( 'NONE',  ( 165.0538309624641613, 244.7653741195639157, 2.311334310144196547 ) ) ;
#75509 = CARTESIAN_POINT ( 'NONE',  ( 198.9303151507368170, 281.1112718272049165, 17.08711449059368803 ) ) ;
#75510 = CARTESIAN_POINT ( 'NONE',  ( -64.94778771796556782, 41.33875607593970614, -10.00000000000000000 ) ) ;
#75511 = CARTESIAN_POINT ( 'NONE',  ( 136.3579783227721691, 249.5333772461660544, 9.188101187500095079 ) ) ;
#75512 = ORIENTED_EDGE ( 'NONE', *, *, #795, .F. ) ;
#75513 = VECTOR ( 'NONE', #90237, 1000.000000000000000 ) ;
#75514 = CARTESIAN_POINT ( 'NONE',  ( 88.27143343078938642, 44.36575123808635368, 4.213746458969102271 ) ) ;
#75515 = CARTESIAN_POINT ( 'NONE',  ( 182.0583737030646319, 257.8139296662238280, 6.555026806704957743 ) ) ;
#75516 = DIRECTION ( 'NONE',  ( -1.000000000000000000, 0.000000000000000000, 0.000000000000000000 ) ) ;
#75517 = PRODUCT_RELATED_PRODUCT_CATEGORY ( 'part', '', ( #13637 ) ) ;
#75518 = AXIS2_PLACEMENT_3D ( 'NONE', #68673, #99105, #99598 ) ;
#75519 = DIRECTION ( 'NONE',  ( -0.7957378174433876739, 0.6056412518070690698, 0.000000000000000000 ) ) ;
#75520 = CARTESIAN_POINT ( 'NONE',  ( 67.53205783091016201, 67.39954269358065631, -7.583584584872256507 ) ) ;
#75521 = VERTEX_POINT ( 'NONE', #92984 ) ;
#75522 = CARTESIAN_POINT ( 'NONE',  ( 76.24083095996626014, 53.42879034202049837, 15.99957989301804062 ) ) ;
#75523 = CARTESIAN_POINT ( 'NONE',  ( 185.1300216526354063, 277.5058458126731580, -16.84358915254627576 ) ) ;
#75524 = CARTESIAN_POINT ( 'NONE',  ( 167.5907823061452291, 249.2350603960721855, -5.636120817613099909 ) ) ;
#75525 = CARTESIAN_POINT ( 'NONE',  ( 81.64670028806227720, 55.20916848805968158, 15.89581094406439554 ) ) ;
#75526 = CARTESIAN_POINT ( 'NONE',  ( 73.61548149140467956, 69.27229284252211983, -9.996823136999276826 ) ) ;
#75527 = CARTESIAN_POINT ( 'NONE',  ( 195.1671348588630508, 263.5382602011624158, 0.8553596245369967654 ) ) ;
#75528 = FACE_OUTER_BOUND ( 'NONE', #70744, .T. ) ;
#75529 = CARTESIAN_POINT ( 'NONE',  ( 185.8834930517967337, 282.2059964265092162, 16.17713989960437360 ) ) ;
#75530 = ADVANCED_FACE ( 'NONE', ( #37747 ), #7351, .T. ) ;
#75531 = CARTESIAN_POINT ( 'NONE',  ( 205.0994677818405023, 275.4042965269534307, -14.14519517703424789 ) ) ;
#75532 = CARTESIAN_POINT ( 'NONE',  ( 193.3472389827650204, 268.3320133866042170, 12.76089158629410747 ) ) ;
#75533 = CARTESIAN_POINT ( 'NONE',  ( 19.40821860046903069, 26.90829794293880539, 10.00000000000000355 ) ) ;
#75534 = CARTESIAN_POINT ( 'NONE',  ( -86.81108781737714253, 10.00000000000000178, -14.21260523776213347 ) ) ;
#75535 = CARTESIAN_POINT ( 'NONE',  ( 205.4925884257800988, 274.0740247280971857, 10.80283695292349222 ) ) ;
#75536 = CARTESIAN_POINT ( 'NONE',  ( 21.11941962201201051, 24.14441083166261137, 10.00000000000000533 ) ) ;
#75537 = CARTESIAN_POINT ( 'NONE',  ( 159.7953104873542145, 253.8733987550956783, 15.41928249285404107 ) ) ;
#75538 = CARTESIAN_POINT ( 'NONE',  ( 161.7101054567844187, 250.5568765819650707, 14.25969465237331235 ) ) ;
#75539 = CARTESIAN_POINT ( 'NONE',  ( -2.124636079309504488, 160.3923013555410080, 4.594050593750050204 ) ) ;
#75540 = CARTESIAN_POINT ( 'NONE',  ( 175.4324593603440974, 286.4533427740436196, -12.30467070008952213 ) ) ;
#75541 = VERTEX_POINT ( 'NONE', #68654 ) ;
#75542 = EDGE_CURVE ( 'NONE', #35189, #95819, #12590, .T. ) ;
#75543 = CARTESIAN_POINT ( 'NONE',  ( 66.89753708227109996, 68.17595765912082584, -6.590651905259176324 ) ) ;
#75544 = PLANE ( 'NONE',  #4709 ) ;
#75545 = CARTESIAN_POINT ( 'NONE',  ( 202.4876139799157500, 274.1054391224496953, -12.98901669480548016 ) ) ;
#75546 = CARTESIAN_POINT ( 'NONE',  ( 199.0773057068961123, 285.8349872121713702, -17.17316764978006560 ) ) ;
#75547 = CARTESIAN_POINT ( 'NONE',  ( 9.485603764116874004, 164.0327760586659451, 1.948934522072302763E-15 ) ) ;
#75548 = VECTOR ( 'NONE', #98310, 1000.000000000000000 ) ;
#75549 = CARTESIAN_POINT ( 'NONE',  ( 24.85415417228448121, 26.30066082961422680, -10.00000000000000533 ) ) ;
#75550 = CARTESIAN_POINT ( 'NONE',  ( 85.46201571263348740, 48.63304775035897620, 12.47391791266364791 ) ) ;
#75551 = CARTESIAN_POINT ( 'NONE',  ( 172.4538997260322617, 272.0033172842936438, -16.41376745784389968 ) ) ;
#75553 = AXIS2_PLACEMENT_3D ( 'NONE', #19790, #51676, #12693 ) ;
#75552 = CARTESIAN_POINT ( 'NONE',  ( 72.01505508543084488, 71.76016648463198067, -3.920346449359661367 ) ) ;
#75554 = CARTESIAN_POINT ( 'NONE',  ( 150.0749816411065183, 276.6459287350622844, 4.378659120374928548 ) ) ;
#75555 = CARTESIAN_POINT ( 'NONE',  ( 178.4558349409154232, 255.0179201197129828, -3.920679784167997894 ) ) ;
#75556 = CARTESIAN_POINT ( 'NONE',  ( 150.3774144590728952, 270.1856731764797814, 13.91914410364283938 ) ) ;
#75557 = AXIS2_PLACEMENT_3D ( 'NONE', #18813, #65891, #12210 ) ;
#75558 = CARTESIAN_POINT ( 'NONE',  ( 58.91185237153143106, 211.4865022471903444, -10.00000000000009415 ) ) ;
#75559 = DIRECTION ( 'NONE',  ( 0.1039558454088763267, -0.1800568059919503139, 0.9781476007338069101 ) ) ;
#75560 = CARTESIAN_POINT ( 'NONE',  ( 190.3049670482083684, 301.0291234702190764, 0.2225066852051815758 ) ) ;
#75561 = CARTESIAN_POINT ( 'NONE',  ( 14.19444334931225349, 172.8768266524160140, 9.188101187500098632 ) ) ;
#75562 = CARTESIAN_POINT ( 'NONE',  ( 168.1019601029094019, 286.2093627858199056, 4.093480230534757069 ) ) ;
#75563 = FACE_BOUND ( 'NONE', #65266, .T. ) ;
#75564 = FACE_OUTER_BOUND ( 'NONE', #71384, .T. ) ;
#75565 = CARTESIAN_POINT ( 'NONE',  ( 202.1602617260373336, 279.5841831652249425, -15.84922531218295383 ) ) ;
#75566 = CARTESIAN_POINT ( 'NONE',  ( 164.9971748156432056, 244.8635054444190757, -1.825016704039769788 ) ) ;
#75567 = CARTESIAN_POINT ( 'NONE',  ( 185.1770359163484159, 266.8001431404497907, 13.86940662139324765 ) ) ;
#75568 = DIRECTION ( 'NONE',  ( 0.5000000000000013323, -0.8660254037844378194, 0.000000000000000000 ) ) ;
#75569 = CARTESIAN_POINT ( 'NONE',  ( 163.9630091648389509, 281.4969130715203960, 8.857997127697792905 ) ) ;
#75570 = PRODUCT_CONTEXT ( 'NONE', #62128, 'mechanical' ) ;
#75571 = CARTESIAN_POINT ( 'NONE',  ( 18.60133699236122595, 19.24335787977762990, -9.188101187500008038 ) ) ;
#75572 = DIRECTION ( 'NONE',  ( 0.5000000000000048850, -0.8660254037844358210, 0.000000000000000000 ) ) ;
#75573 = CARTESIAN_POINT ( 'NONE',  ( 82.70618072881376293, 53.83593579450208466, 15.81121719814038151 ) ) ;
#75574 = CARTESIAN_POINT ( 'NONE',  ( 71.73982542038400823, 59.04037670598220444, 15.86454711389505334 ) ) ;
#75575 = CARTESIAN_POINT ( 'NONE',  ( -51.42721978966704910, 42.16899896210639298, 54.99999999999999289 ) ) ;
#75576 = ORIENTED_EDGE ( 'NONE', *, *, #47299, .F. ) ;
#75577 = VECTOR ( 'NONE', #78007, 1000.000000000000000 ) ;
#75578 = CARTESIAN_POINT ( 'NONE',  ( 183.2126764927348290, 289.7799306247588333, 12.21646338406959842 ) ) ;
#75579 = CARTESIAN_POINT ( 'NONE',  ( 163.0804386853320125, 262.7275182220299712, -17.72388574752874746 ) ) ;
#75580 = CARTESIAN_POINT ( 'NONE',  ( 81.48503363143359479, 41.97952132416679660, 7.656029848638611135 ) ) ;
#75581 = CARTESIAN_POINT ( 'NONE',  ( 35.92001165216885994, 44.23654200823204974, 1.583844403245397769 ) ) ;
#75582 = ORIENTED_EDGE ( 'NONE', *, *, #69508, .T. ) ;
#75583 = CARTESIAN_POINT ( 'NONE',  ( 196.0587100571994483, 289.0633482449420626, -17.27351923437598913 ) ) ;
#75584 = CARTESIAN_POINT ( 'NONE',  ( 67.78283758264466030, 69.71839983238106697, 0.6266629628056711310 ) ) ;
#75585 = DIRECTION ( 'NONE',  ( 0.000000000000000000, 0.000000000000000000, 1.000000000000000000 ) ) ;
#75586 = CARTESIAN_POINT ( 'NONE',  ( 155.2193237801463113, 261.7992402267395846, -18.58295809893692407 ) ) ;
#75587 = EDGE_LOOP ( 'NONE', ( #40126, #13332, #94544, #67274 ) ) ;
#75588 = EDGE_LOOP ( 'NONE', ( #46287, #95252, #90205, #19897 ) ) ;
#75589 = AXIS2_PLACEMENT_3D ( 'NONE', #69931, #70964, #85185 ) ;
#75591 = CARTESIAN_POINT ( 'NONE',  ( 1.813001633210440833, 27.74720351945396857, -10.00000000000000000 ) ) ;
#75590 = CARTESIAN_POINT ( 'NONE',  ( 202.3522217946735111, 279.7792213403169512, 15.59347206985308709 ) ) ;
#75592 = ORIENTED_EDGE ( 'NONE', *, *, #79610, .F. ) ;
#75593 = CARTESIAN_POINT ( 'NONE',  ( 88.45040933577318754, 44.05593677119288287, -2.476488480078137933 ) ) ;
#75594 = CARTESIAN_POINT ( 'NONE',  ( 46.32860941106299890, 116.4404604047837779, -10.00000000000000000 ) ) ;
#75595 = CARTESIAN_POINT ( 'NONE',  ( 80.44596413951620661, 57.92004253751065335, -16.60216415864725903 ) ) ;
#75596 = LINE ( 'NONE', #98903, #58059 ) ;
#75597 = ORIENTED_EDGE ( 'NONE', *, *, #83416, .F. ) ;
#75599 = ADVANCED_FACE ( 'NONE', ( #85927 ), #1265, .T. ) ;
#75598 = CARTESIAN_POINT ( 'NONE',  ( -17.42236680055705023, 149.2012482093457777, 0.000000000000000000 ) ) ;
#75600 = EDGE_LOOP ( 'NONE', ( #38965, #49825, #11596, #17512 ) ) ;
#75601 = CARTESIAN_POINT ( 'NONE',  ( 205.8379285891498682, 274.1252448892948905, 10.44730901608240181 ) ) ;
#75602 = CARTESIAN_POINT ( 'NONE',  ( -56.23827824165702793, 48.13106613502690578, 59.99999999999999289 ) ) ;
#75603 = ORIENTED_EDGE ( 'NONE', *, *, #38605, .T. ) ;
#75604 = CARTESIAN_POINT ( 'NONE',  ( 148.9719199701866899, 272.6200610409887872, 12.59512981512031438 ) ) ;
#75605 = CARTESIAN_POINT ( 'NONE',  ( 172.3369791656317034, 263.9050024373092924, -16.81851492143085025 ) ) ;
#75606 = ORIENTED_EDGE ( 'NONE', *, *, #35387, .T. ) ;
#75607 = CARTESIAN_POINT ( 'NONE',  ( 158.5161842154787166, 275.0912836277667566, -13.81901676271391466 ) ) ;
#75608 = CARTESIAN_POINT ( 'NONE',  ( 32.19481522723634725, 40.36126292948897287, 6.180339887498949913 ) ) ;
#75609 = FACE_OUTER_BOUND ( 'NONE', #2604, .T. ) ;
#75610 = CARTESIAN_POINT ( 'NONE',  ( -4.065086259125790136, 119.3853102282570120, 36.50000000000000000 ) ) ;
#75611 = VERTEX_POINT ( 'NONE', #30158 ) ;
#75612 = VERTEX_POINT ( 'NONE', #23537 ) ;
#75613 = CARTESIAN_POINT ( 'NONE',  ( 156.6195539527090546, 266.7731622753219654, -16.18964406384344912 ) ) ;
#75614 = CARTESIAN_POINT ( 'NONE',  ( 190.9441801652054096, 299.9219738747156043, -4.765040093794296716 ) ) ;
#75615 = CARTESIAN_POINT ( 'NONE',  ( 82.38367100173057622, 53.80119691343342936, 15.85271891126490473 ) ) ;
#75616 = CARTESIAN_POINT ( 'NONE',  ( -22.09748208295713567, 35.17237849129525529, 59.99999999999999289 ) ) ;
#75617 = CARTESIAN_POINT ( 'NONE',  ( 192.8132846206021611, 296.6845899933152850, 11.53748932578252351 ) ) ;
#75618 = CARTESIAN_POINT ( 'NONE',  ( 191.1932856887581522, 299.4905104514762684, 9.694084360102674935 ) ) ;
#75619 = CARTESIAN_POINT ( 'NONE',  ( 146.5502055023624735, 276.8145935406849389, 0.3770461397900869427 ) ) ;
#75620 = CARTESIAN_POINT ( 'NONE',  ( 74.54785486515559967, 57.86623053792277460, -15.96777695429060806 ) ) ;
#75621 = VECTOR ( 'NONE', #43881, 1000.000000000000000 ) ;
#75622 = CARTESIAN_POINT ( 'NONE',  ( 165.0297293518065658, 244.8071193337670195, 2.517333243890161665 ) ) ;
#75624 = CARTESIAN_POINT ( 'NONE',  ( 42.16454434324482747, 125.9067112960471349, 10.00000000000000000 ) ) ;
#75623 = CARTESIAN_POINT ( 'NONE',  ( 196.8363552541316324, 289.7164272536036265, -17.80258609350122967 ) ) ;
#75625 = CARTESIAN_POINT ( 'NONE',  ( 71.22129689212546566, 72.22986999219065751, -0.8113714082787989446 ) ) ;
#75626 = CARTESIAN_POINT ( 'NONE',  ( 171.5288298918311511, 288.9004815652406251, 4.237906360154932273 ) ) ;
#75627 = FACE_OUTER_BOUND ( 'NONE', #9901, .T. ) ;
#75628 = VECTOR ( 'NONE', #5635, 1000.000000000000227 ) ;
#75629 = ORIENTED_EDGE ( 'NONE', *, *, #49148, .F. ) ;
#75630 = CARTESIAN_POINT ( 'NONE',  ( 149.7482486646325412, 271.2754202988347743, -12.05835948757660958 ) ) ;
#75631 = CARTESIAN_POINT ( 'NONE',  ( 78.21076945151075677, 53.49648267122271506, -15.87264874329164677 ) ) ;
#75632 = CARTESIAN_POINT ( 'NONE',  ( 149.3018356595837588, 273.4567121134075478, 10.20698179752245949 ) ) ;
#75633 = LINE ( 'NONE', #6219, #78062 ) ;
#75634 = CARTESIAN_POINT ( 'NONE',  ( 179.6164226443064535, 282.7900583135175339, -15.54602365610343107 ) ) ;
#75635 = CARTESIAN_POINT ( 'NONE',  ( 189.9455075854687323, 301.6517255229458101, -1.253142702374338002 ) ) ;
#75636 = EDGE_LOOP ( 'NONE', ( #85227, #10693, #75375, #68207 ) ) ;
#75637 = CARTESIAN_POINT ( 'NONE',  ( 208.3829315663354862, 269.7171704273955015, -1.768817828503133072 ) ) ;
#75638 = CIRCLE ( 'NONE', #82184, 1.449999999999994627 ) ;
#75639 =( BOUNDED_CURVE ( )  B_SPLINE_CURVE ( 2, ( #67676, #89542, #13007, #43867, #5387, #36273, #20103, #67172, #91019 ),
 .UNSPECIFIED., .F., .T. ) 
 B_SPLINE_CURVE_WITH_KNOTS ( ( 3, 2, 2, 2, 3 ),
 ( 0.3508064516129032473, 0.3521505376344086224, 0.3548387096774193727, 0.3575268817204301230, 0.3588709677419354982 ),
 .UNSPECIFIED. ) 
 CURVE ( )  GEOMETRIC_REPRESENTATION_ITEM ( )  RATIONAL_B_SPLINE_CURVE ( ( 0.9330127018922194093, 0.9330127018922194093, 1.000000000000000000, 0.8660254037844387076, 1.000000000000000000, 0.8660254037844387076, 1.000000000000000000, 0.9330127018922194093, 0.9330127018922194093 ) ) 
 REPRESENTATION_ITEM ( '' )  );
#75640 = CARTESIAN_POINT ( 'NONE',  ( 85.93470712620026575, 48.23248545518190866, 11.93606436224419376 ) ) ;
#75641 = DIRECTION ( 'NONE',  ( 0.2473641778533817170, 0.9689225787001356505, 0.000000000000000000 ) ) ;
#75642 = CARTESIAN_POINT ( 'NONE',  ( 36.81016237556811177, 205.3927522451419350, 2.944929066748280225E-16 ) ) ;
#75643 = CARTESIAN_POINT ( 'NONE',  ( 105.6408794604690797, 240.9869531367911293, 4.594050593750046652 ) ) ;
#75644 = CARTESIAN_POINT ( 'NONE',  ( 72.26538907532096800, 200.9824982072973967, 3.021315404115420679E-15 ) ) ;
#75645 = DIRECTION ( 'NONE',  ( -0.000000000000000000, -0.000000000000000000, -1.000000000000000000 ) ) ;
#75646 = CARTESIAN_POINT ( 'NONE',  ( 157.2168982216852555, 258.3393398020932636, 18.09635675623264106 ) ) ;
#75647 = CARTESIAN_POINT ( 'NONE',  ( 175.2741237188109551, 253.4266919301918506, -3.879795126654972393 ) ) ;
#75648 = B_SPLINE_CURVE_WITH_KNOTS ( 'NONE', 3,
 ( #548, #45140, #29944, #62321, #53243, #62832, #22346, #38533, #47133, #31430, #84198, #14253, #31928, #93274, #23831, #14745 ),
 .UNSPECIFIED., .F., .F.,
 ( 4, 1, 2, 2, 2, 1, 2, 2, 4 ),
 ( 0.000000000000000000, 0.1250000000000026368, 0.1875000000000034972, 0.2500000000000043854, 0.5000000000000066613, 0.6250000000000064393, 0.6875000000000063283, 0.7500000000000061062, 1.000000000000000000 ),
 .UNSPECIFIED. ) ;
#75649 = CARTESIAN_POINT ( 'NONE',  ( 36.54820344085055694, 204.1589784336661637, -6.496448406907675876E-16 ) ) ;
#75650 = EDGE_CURVE ( 'NONE', #48026, #36578, #8855, .T. ) ;
#75651 = LINE ( 'NONE', #90397, #68901 ) ;
#75652 = AXIS2_PLACEMENT_3D ( 'NONE', #31598, #69615, #85888 ) ;
#75653 = ORIENTED_EDGE ( 'NONE', *, *, #78939, .F. ) ;
#75654 = CARTESIAN_POINT ( 'NONE',  ( 72.93625488370378207, 69.25789689889019485, 9.544539825114355835 ) ) ;
#75655 = CARTESIAN_POINT ( 'NONE',  ( 179.7777640920925535, 266.8932340374666978, 15.06726368060596144 ) ) ;
#75656 = CARTESIAN_POINT ( 'NONE',  ( 72.18990340680744566, 72.03918383723207342, -3.149060597287207219 ) ) ;
#75657 = CARTESIAN_POINT ( 'NONE',  ( 147.1199024702499969, 275.8278494473859723, 5.224467159276165340 ) ) ;
#75658 = CARTESIAN_POINT ( 'NONE',  ( 205.7872507830675204, 272.2130214242461079, -9.506855900917111413 ) ) ;
#75659 = EDGE_CURVE ( 'NONE', #66853, #81845, #84399, .T. ) ;
#75660 = LINE ( 'NONE', #45237, #5873 ) ;
#75661 = CARTESIAN_POINT ( 'NONE',  ( 177.5073464959093315, 286.2605698986350831, -12.10074426044735674 ) ) ;
#75662 = CARTESIAN_POINT ( 'NONE',  ( 68.91022223105564137, 64.71151235087043574, -12.22836756590942464 ) ) ;
#75663 = VECTOR ( 'NONE', #51473, 1000.000000000000000 ) ;
#75664 = CARTESIAN_POINT ( 'NONE',  ( 108.6902708896766114, 226.8927522451418213, 10.00000000000009592 ) ) ;
#75665 = ORIENTED_EDGE ( 'NONE', *, *, #18904, .F. ) ;
#75666 = EDGE_CURVE ( 'NONE', #65627, #59009, #77778, .T. ) ;
#75667 = CARTESIAN_POINT ( 'NONE',  ( 79.29973261757051262, 59.57579620614538385, -16.53044932756547425 ) ) ;
#75668 = CARTESIAN_POINT ( 'NONE',  ( 202.2603678735342214, 280.3217618159037556, 16.49712126737133744 ) ) ;
#75669 = CARTESIAN_POINT ( 'NONE',  ( 207.6523394534040392, 270.9825930866021508, -2.115019688068903392 ) ) ;
#75670 = CARTESIAN_POINT ( 'NONE',  ( 3.097972219676621730, 184.8464784336661637, 1.353441290958777327E-15 ) ) ;
#75671 = B_SPLINE_CURVE_WITH_KNOTS ( 'NONE', 3,
 ( #45382, #75818, #83433, #90039 ),
 .UNSPECIFIED., .F., .F.,
 ( 4, 4 ),
 ( 0.009406675354063229882, 0.01769731902523580952 ),
 .UNSPECIFIED. ) ;
#75672 = CARTESIAN_POINT ( 'NONE',  ( 4.441398484865463736, 26.65659080271448289, -1.878358725466461243E-16 ) ) ;
#75673 = CARTESIAN_POINT ( 'NONE',  ( -15.98639401305193175, 105.8318875400968011, 44.17750287558818911 ) ) ;
#75674 = CARTESIAN_POINT ( 'NONE',  ( 71.50716427137886910, 59.09066120637785247, -15.81421025005064607 ) ) ;
#75675 = DIRECTION ( 'NONE',  ( -0.8660254037844387076, -0.4999999999999998890, -0.000000000000000000 ) ) ;
#75677 = CARTESIAN_POINT ( 'NONE',  ( 58.68649846873780263, 198.5643266524160140, 9.188101187500095079 ) ) ;
#75676 = CARTESIAN_POINT ( 'NONE',  ( 175.3741314181362725, 286.6665286446898904, 10.50185128592887018 ) ) ;
#75678 = CARTESIAN_POINT ( 'NONE',  ( 207.6932907333322191, 270.9116633891313199, 2.120963121341169710 ) ) ;
#75679 = CARTESIAN_POINT ( 'NONE',  ( 72.97550374175638410, 57.18490168260592554, 15.90463394248157947 ) ) ;
#75680 = CARTESIAN_POINT ( 'NONE',  ( 70.37206268826852806, 70.13158196118115484, 5.629252521285986077 ) ) ;
#75681 = CARTESIAN_POINT ( 'NONE',  ( 207.6860335175200589, 270.9242332556395922, 6.913225035677485586 ) ) ;
#75682 = VERTEX_POINT ( 'NONE', #85405 ) ;
#75683 = CARTESIAN_POINT ( 'NONE',  ( 207.0624025450594843, 270.0043937851150417, -2.644299678167422840 ) ) ;
#75684 = CARTESIAN_POINT ( 'NONE',  ( 8.754547735682661980, 185.8615022471903160, 5.000000000000046185 ) ) ;
#75685 = FACE_OUTER_BOUND ( 'NONE', #47695, .T. ) ;
#75686 = VECTOR ( 'NONE', #75519, 1000.000000000000000 ) ;
#75687 = CARTESIAN_POINT ( 'NONE',  ( 138.1714793337695824, 241.3923013555409796, 4.594050593750050204 ) ) ;
#75688 = CARTESIAN_POINT ( 'NONE',  ( 24.12224894148702248, 22.43085787977763701, -9.188101187500008038 ) ) ;
#75689 = CARTESIAN_POINT ( 'NONE',  ( 207.1023286545539861, 271.9352397349218791, -8.358798036041973134 ) ) ;
#75690 = CARTESIAN_POINT ( 'NONE',  ( 83.68493280611274088, 51.65299594367198210, -14.83749715326822205 ) ) ;
#75691 = CARTESIAN_POINT ( 'NONE',  ( 69.21394623383592659, 210.7677522451418497, 10.00000000000009592 ) ) ;
#75693 = CARTESIAN_POINT ( 'NONE',  ( 188.5998214029316102, 289.4849150055601399, 14.43259912634508524 ) ) ;
#75692 = CARTESIAN_POINT ( 'NONE',  ( 82.28003896795380001, 40.62557011406286733, -3.142018250819525793 ) ) ;
#75694 = CARTESIAN_POINT ( 'NONE',  ( 68.62869117346340886, 64.12329276949824930, 11.92149815895183096 ) ) ;
#75695 = ORIENTED_EDGE ( 'NONE', *, *, #49962, .F. ) ;
#75696 = CARTESIAN_POINT ( 'NONE',  ( 150.7530568467738590, 269.5350414755053521, 15.60317050893315916 ) ) ;
#75697 = CYLINDRICAL_SURFACE ( 'NONE', #4073, 10.00000000000010658 ) ;
#75698 = AXIS2_PLACEMENT_3D ( 'NONE', #9608, #25279, #56165 ) ;
#75699 = CARTESIAN_POINT ( 'NONE',  ( 67.44257088943838596, 67.25355904234817217, -8.657396272410824878 ) ) ;
#75700 = CARTESIAN_POINT ( 'NONE',  ( 169.6285385964465604, 266.0829471737013705, -16.93693285811728799 ) ) ;
#75701 = CARTESIAN_POINT ( 'NONE',  ( 5.721601707324311725, 18.70171378149916919, -9.188101187500004485 ) ) ;
#75702 = ORIENTED_EDGE ( 'NONE', *, *, #3598, .F. ) ;
#75703 = CARTESIAN_POINT ( 'NONE',  ( 74.56414817410228579, 187.8759306620403322, -18.47570218321542157 ) ) ;
#75704 = AXIS2_PLACEMENT_3D ( 'NONE', #53508, #14530, #62093 ) ;
#75705 = LINE ( 'NONE', #21497, #21517 ) ;
#75706 = EDGE_CURVE ( 'NONE', #7688, #35964, #58485, .T. ) ;
#75707 = EDGE_CURVE ( 'NONE', #75268, #7831, #33013, .T. ) ;
#75708 = CARTESIAN_POINT ( 'NONE',  ( 71.48480579176155914, 72.35852322450824659, 1.080755764661565754 ) ) ;
#75709 = B_SPLINE_SURFACE_WITH_KNOTS ( 'NONE', 3, 1, ( 
 ( #70276, #86548 ),
 ( #93622, #24189 ),
 ( #55072, #47480 ),
 ( #78404, #94127 ),
 ( #17079, #71306 ),
 ( #32778, #72312 ),
 ( #25701, #96133 ),
 ( #34288, #87568 ),
 ( #66188, #10491 ),
 ( #41373, #40863 ),
 ( #50475, #48995 ),
 ( #79931, #58085 ),
 ( #19114, #33285 ),
 ( #95647, #33810 ),
 ( #3414, #18602 ),
 ( #19617, #80945 ),
 ( #26194, #57073 ),
 ( #49481, #49990 ),
 ( #80437, #65185 ),
 ( #27701, #89541 ),
 ( #26687, #48495 ),
 ( #57575, #88548 ),
 ( #42367, #11513 ),
 ( #73301, #3892 ),
 ( #71810, #34774 ),
 ( #65675, #27196 ),
 ( #89065, #81428 ),
 ( #79436, #20102 ),
 ( #23046, #25310 ),
 ( #89661, #57199 ),
 ( #41503, #34413 ),
 ( #57699, #3537 ),
 ( #18725, #19249 ),
 ( #50114, #33938 ) ),
 .UNSPECIFIED., .T., .F., .F.,
 ( 4, 2, 2, 2, 2, 2, 2, 2, 2, 2, 2, 2, 2, 2, 2, 2, 4 ),
 ( 2, 2 ),
 ( 0.000000000000000000, 0.06250000000000000000, 0.1250000000000000000, 0.1875000000000000000, 0.2500000000000000000, 0.3125000000000000000, 0.3750000000000000000, 0.4375000000000000000, 0.5000000000000000000, 0.5625000000000000000, 0.6250000000000000000, 0.6875000000000000000, 0.7500000000000000000, 0.8125000000000000000, 0.8750000000000000000, 0.9375000000000000000, 1.000000000000000000 ),
 ( 0.000000000000000000, 1.000000000000000000 ),
 .UNSPECIFIED. ) ;
#75710 = CARTESIAN_POINT ( 'NONE',  ( 200.6634772367119410, 281.5104481654628898, -17.03558376807434271 ) ) ;
#75711 = CARTESIAN_POINT ( 'NONE',  ( 196.2305329650964723, 270.9041150931136031, 12.09698969586446538 ) ) ;
#75712 = CARTESIAN_POINT ( 'NONE',  ( 98.36217659263859048, 216.0494855054051868, -2.679491924311248496 ) ) ;
#75713 = CARTESIAN_POINT ( 'NONE',  ( 67.36253031349440334, 68.54163467477879124, 5.081825066198372376 ) ) ;
#75714 = CARTESIAN_POINT ( 'NONE',  ( 153.1983976505312626, 265.2995869615763809, -17.69657798691567763 ) ) ;
#75715 = ORIENTED_EDGE ( 'NONE', *, *, #81366, .F. ) ;
#75716 = DIRECTION ( 'NONE',  ( 0.9999986627203610867, -0.001635407438361276495, 0.000000000000000000 ) ) ;
#75717 = CARTESIAN_POINT ( 'NONE',  ( 10.05514423959709447, 21.50829794293879260, -10.00000000000000355 ) ) ;
#75718 = CARTESIAN_POINT ( 'NONE',  ( -31.49356256989596758, 94.88921800892812541, 36.50000000000000000 ) ) ;
#75719 = ORIENTED_EDGE ( 'NONE', *, *, #61527, .F. ) ;
#75720 = CARTESIAN_POINT ( 'NONE',  ( 149.6036070299368532, 271.5259469590175740, 11.63513718912356865 ) ) ;
#75721 = CARTESIAN_POINT ( 'NONE',  ( 86.42645758268480449, 47.01732744055364321, -10.52632212332717998 ) ) ;
#75722 = CARTESIAN_POINT ( 'NONE',  ( 82.81350700933505493, 45.30993475200613574, -10.24506358842424270 ) ) ;
#75723 = ORIENTED_EDGE ( 'NONE', *, *, #35055, .F. ) ;
#75725 = ADVANCED_FACE ( 'NONE', ( #96008 ), #47835, .T. ) ;
#75724 = CARTESIAN_POINT ( 'NONE',  ( 191.7247331938518187, 298.5700163710982338, -9.650650827884682315 ) ) ;
#75726 = CARTESIAN_POINT ( 'NONE',  ( 181.4930680486588699, 260.3623518102999697, -11.98802389789063660 ) ) ;
#75727 = CARTESIAN_POINT ( 'NONE',  ( 163.7136804588959649, 247.0865828815331042, 6.783386239354816105 ) ) ;
#75728 = CARTESIAN_POINT ( 'NONE',  ( 69.42144788871627270, 62.89730317705431872, 13.10748580973936761 ) ) ;
#75729 = ORIENTED_EDGE ( 'NONE', *, *, #30530, .T. ) ;
#75730 = CARTESIAN_POINT ( 'NONE',  ( 97.03527265400872182, 217.6423013555409796, -4.594050593750043987 ) ) ;
#75731 = CARTESIAN_POINT ( 'NONE',  ( 202.9416383086232543, 279.1417668086349977, 15.32562689463440364 ) ) ;
#75732 = CARTESIAN_POINT ( 'NONE',  ( 177.9014365079093807, 268.9747928436916595, -16.77994175735417670 ) ) ;
#75733 = CARTESIAN_POINT ( 'NONE',  ( 81.38720151904264810, 42.05902438066944171, -7.878585452988780879 ) ) ;
#75734 = EDGE_CURVE ( 'NONE', #73618, #69104, #80259, .T. ) ;
#75735 = B_SPLINE_SURFACE_WITH_KNOTS ( 'NONE', 3, 1, ( 
 ( #22525, #45801 ),
 ( #4856, #35738 ),
 ( #29143, #66633 ),
 ( #51939, #97564 ),
 ( #28131, #20553 ),
 ( #51431, #82396 ),
 ( #62493, #15914 ),
 ( #31107, #25011 ),
 ( #24517, #61514 ),
 ( #85892, #8817 ),
 ( #39686, #55394 ),
 ( #78237, #84859 ),
 ( #100043, #92947 ),
 ( #86381, #715 ),
 ( #222, #78734 ),
 ( #1227, #77741 ),
 ( #69617, #61995 ),
 ( #31601, #24015 ),
 ( #38709, #15403 ),
 ( #94457, #23500 ),
 ( #92462, #93463 ),
 ( #16912, #47801 ),
 ( #70614, #9325 ),
 ( #32109, #55890 ),
 ( #86884, #69117 ),
 ( #38198, #46295 ),
 ( #54392, #63018 ),
 ( #40198, #47311 ),
 ( #85368, #46819 ),
 ( #23007, #8326 ),
 ( #54912, #39191 ),
 ( #77223, #30629 ),
 ( #71142, #1742 ),
 ( #70106, #17417 ) ),
 .UNSPECIFIED., .T., .F., .F.,
 ( 4, 2, 2, 2, 2, 2, 2, 2, 2, 2, 2, 2, 2, 2, 2, 2, 4 ),
 ( 2, 2 ),
 ( 0.000000000000000000, 0.06250000000000000000, 0.1250000000000000000, 0.1875000000000000000, 0.2500000000000000000, 0.3125000000000000000, 0.3750000000000000000, 0.4375000000000000000, 0.5000000000000000000, 0.5625000000000000000, 0.6250000000000000000, 0.6875000000000000000, 0.7500000000000000000, 0.8125000000000000000, 0.8750000000000000000, 0.9375000000000000000, 1.000000000000000000 ),
 ( 0.000000000000000000, 1.000000000000000000 ),
 .UNSPECIFIED. ) ;
#75736 = ORIENTED_EDGE ( 'NONE', *, *, #33722, .F. ) ;
#75737 = EDGE_CURVE ( 'NONE', #54050, #75363, #89938, .T. ) ;
#75738 = VERTEX_POINT ( 'NONE', #66551 ) ;
#75739 = ORIENTED_EDGE ( 'NONE', *, *, #79862, .T. ) ;
#75740 = CARTESIAN_POINT ( 'NONE',  ( 81.53437377926626084, 50.59759334475508297, 14.46997207384287343 ) ) ;
#75741 = VERTEX_POINT ( 'NONE', #28539 ) ;
#75742 = CARTESIAN_POINT ( 'NONE',  ( 69.41547982834435970, 69.97450927703960133, 4.531412641460686785 ) ) ;
#75743 = ORIENTED_EDGE ( 'NONE', *, *, #54935, .T. ) ;
#75744 = CARTESIAN_POINT ( 'NONE',  ( 208.3057440179679531, 269.8508631828800617, 2.969924427282375046 ) ) ;
#75745 = VECTOR ( 'NONE', #10552, 1000.000000000000000 ) ;
#75746 = LINE ( 'NONE', #91975, #44890 ) ;
#75747 = CARTESIAN_POINT ( 'NONE',  ( 200.7694952279801157, 282.9040289856181403, -17.94628235092568502 ) ) ;
#75748 = CARTESIAN_POINT ( 'NONE',  ( -23.57584832053852963, 99.66285025437392164, 45.19938011207119644 ) ) ;
#75749 = CARTESIAN_POINT ( 'NONE',  ( 69.33709985148358612, 68.43352380735160523, -7.655773901753416766 ) ) ;
#75750 = CARTESIAN_POINT ( 'NONE',  ( 171.2743479101317234, 254.4242377521371736, -11.94796457435898951 ) ) ;
#75751 = VERTEX_POINT ( 'NONE', #90401 ) ;
#75752 = DIRECTION ( 'NONE',  ( -0.8660254037844387076, -0.4999999999999998890, -0.000000000000000000 ) ) ;
#75753 = CARTESIAN_POINT ( 'NONE',  ( 9.708348802340269756, 27.64646525600388571, -2.839279412974133887 ) ) ;
#75754 = EDGE_LOOP ( 'NONE', ( #74469, #6465, #19672, #56180 ) ) ;
#75755 = CARTESIAN_POINT ( 'NONE',  ( 164.2963363950948690, 281.6989409824586801, 8.833678480319404613 ) ) ;
#75756 = CARTESIAN_POINT ( 'NONE',  ( 85.69780903665139249, 48.74868904809778059, 11.98201799417179991 ) ) ;
#75758 = ORIENTED_EDGE ( 'NONE', *, *, #40455, .T. ) ;
#75757 = LINE ( 'NONE', #91984, #15318 ) ;
#75759 = CARTESIAN_POINT ( 'NONE',  ( -16.71725632976956888, 104.6388057647513961, 12.47619570403008105 ) ) ;
#75760 = CARTESIAN_POINT ( 'NONE',  ( 203.0535368433499457, 278.9479528611958585, 16.46202213522710167 ) ) ;
#75761 = FACE_OUTER_BOUND ( 'NONE', #84734, .T. ) ;
#75762 = CARTESIAN_POINT ( 'NONE',  ( 161.3205084827974076, 281.4276874649026468, -6.572659893739726478 ) ) ;
#75763 = CARTESIAN_POINT ( 'NONE',  ( 165.5366541472494362, 246.9067919256106620, -2.119420010412345956 ) ) ;
#75764 = DIRECTION ( 'NONE',  ( -1.000000000000000000, 0.000000000000000000, 0.000000000000000000 ) ) ;
#75765 = CARTESIAN_POINT ( 'NONE',  ( 200.1782072557437857, 283.9281697954355650, 18.05177561285849208 ) ) ;
#75766 = CARTESIAN_POINT ( 'NONE',  ( 157.9927698565683727, 281.0302174119535721, 1.994413190729223739 ) ) ;
#75767 = ORIENTED_EDGE ( 'NONE', *, *, #83875, .T. ) ;
#75768 = CARTESIAN_POINT ( 'NONE',  ( 181.5151252095495806, 271.0695012673220390, -15.95595848548451023 ) ) ;
#75769 = CARTESIAN_POINT ( 'NONE',  ( 71.40813930945712684, 63.30437739610238168, -13.57462368570346278 ) ) ;
#75770 = AXIS2_PLACEMENT_3D ( 'NONE', #48140, #61822, #54215 ) ;
#75771 = CARTESIAN_POINT ( 'NONE',  ( 3.125382611083808104, 182.6115022471903160, -5.000000000000047962 ) ) ;
#75772 = CARTESIAN_POINT ( 'NONE',  ( 4.767222435543961190, 166.8927522451418213, 10.00000000000009592 ) ) ;
#75773 = CARTESIAN_POINT ( 'NONE',  ( 82.78552022943677002, 53.33943766691666610, -15.29229482101202109 ) ) ;
#75774 = VECTOR ( 'NONE', #68418, 1000.000000000000000 ) ;
#75775 = CARTESIAN_POINT ( 'NONE',  ( 188.1018771210319471, 260.4230313274653099, 6.875771660441075461 ) ) ;
#75776 =( REPRESENTATION_RELATIONSHIP ('NONE','NONE', #67038, #87244 ) REPRESENTATION_RELATIONSHIP_WITH_TRANSFORMATION ( #54226 )SHAPE_REPRESENTATION_RELATIONSHIP( ) );
#75777 = CARTESIAN_POINT ( 'NONE',  ( 163.3365390452323425, 247.7398109716368424, -8.140084928332512959 ) ) ;
#75778 = CARTESIAN_POINT ( 'NONE',  ( 72.08805153644932773, 72.27453658898816968, 1.326354783638816315 ) ) ;
#75779 = AXIS2_PLACEMENT_3D ( 'NONE', #63543, #94484, #1257 ) ;
#75780 = CARTESIAN_POINT ( 'NONE',  ( 164.5539697625973190, 274.3695635373503023, 14.76467764503104441 ) ) ;
#75782 = CARTESIAN_POINT ( 'NONE',  ( 76.19586783375881112, 65.24272250020374031, 14.11841093771251643 ) ) ;
#75781 = CARTESIAN_POINT ( 'NONE',  ( -7.645548028435306342, 157.2048013555409796, 4.594050593750051981 ) ) ;
#75783 = ADVANCED_FACE ( 'NONE', ( #88934 ), #6241, .T. ) ;
#75784 = CARTESIAN_POINT ( 'NONE',  ( 162.8386403195304410, 249.0994062285972461, 10.29435687412694911 ) ) ;
#75785 = ORIENTED_EDGE ( 'NONE', *, *, #13908, .T. ) ;
#75786 = AXIS2_PLACEMENT_3D ( 'NONE', #83756, #75138, #20948 ) ;
#75787 = VERTEX_POINT ( 'NONE', #35148 ) ;
#75788 = DIRECTION ( 'NONE',  ( -0.4621356007560363244, 0.8868092729070087277, 0.000000000000000000 ) ) ;
#75789 = DIRECTION ( 'NONE',  ( -0.5000000000000003331, 0.8660254037844383745, 0.000000000000000000 ) ) ;
#75790 = EDGE_CURVE ( 'NONE', #1578, #62347, #75638, .T. ) ;
#75791 = DIRECTION ( 'NONE',  ( -0.8495546651763560275, -0.5275005885087612478, 0.000000000000000000 ) ) ;
#75792 = CARTESIAN_POINT ( 'NONE',  ( 202.0980293819432916, 280.6029403313636408, -17.25107598010587751 ) ) ;
#75793 = CARTESIAN_POINT ( 'NONE',  ( 84.36168211171367659, 46.55299321218482334, 10.66842414931385541 ) ) ;
#75794 = CARTESIAN_POINT ( 'NONE',  ( 153.5378496954705270, 279.2422976570009610, 3.847913014617606375 ) ) ;
#75795 = CARTESIAN_POINT ( 'NONE',  ( 21.69106252476256458, 174.1423013555409796, -4.594050593750043987 ) ) ;
#75796 = CARTESIAN_POINT ( 'NONE',  ( 108.2389556718223673, 242.4869531367911009, 4.594050593750046652 ) ) ;
#75797 = DIRECTION ( 'NONE',  ( -0.9172102815912978047, -0.3984034379159046568, 0.000000000000000000 ) ) ;
#75798 = CARTESIAN_POINT ( 'NONE',  ( 65.83444237920811304, 68.98881161217069291, 2.061071955463292138 ) ) ;
#75799 = EDGE_CURVE ( 'NONE', #48468, #2734, #20976, .T. ) ;
#75800 = CARTESIAN_POINT ( 'NONE',  ( 206.5615526473034151, 272.3516689047157229, -7.512841850187674808 ) ) ;
#75801 = VECTOR ( 'NONE', #94965, 1000.000000000000114 ) ;
#75802 = CARTESIAN_POINT ( 'NONE',  ( 175.5675097156527613, 281.7075564011171309, -14.18956677121689403 ) ) ;
#75803 = CARTESIAN_POINT ( 'NONE',  ( 81.93876147804334664, 52.90231730716391922, -15.25894681625440974 ) ) ;
#75804 = CARTESIAN_POINT ( 'NONE',  ( 155.0303156110108489, 262.1266119787277944, 17.11986653161320859 ) ) ;
#75805 = CARTESIAN_POINT ( 'NONE',  ( 184.0348397922024901, 275.0104453757304555, 16.36204107713549050 ) ) ;
#75806 = CARTESIAN_POINT ( 'NONE',  ( 83.07104351211755500, 49.91350363301629045, 14.17192785442602876 ) ) ;
#75807 = EDGE_CURVE ( 'NONE', #49470, #57417, #54005, .T. ) ;
#75808 = CARTESIAN_POINT ( 'NONE',  ( 84.80230723680845983, 50.33593218185897911, 13.42795335988696870 ) ) ;
#75809 = CARTESIAN_POINT ( 'NONE',  ( 195.5982822146934836, 266.5867291171349507, 7.946036122846243721 ) ) ;
#75810 = DIRECTION ( 'NONE',  ( -0.01068548594337170865, 0.9999429085653609439, 0.000000000000000000 ) ) ;
#75811 = CARTESIAN_POINT ( 'NONE',  ( 162.3854161007234609, 251.6213552765262875, -12.80540064494198838 ) ) ;
#75812 = EDGE_CURVE ( 'NONE', #78693, #55881, #83278, .T. ) ;
#75813 = PLANE ( 'NONE',  #60989 ) ;
#75814 = VECTOR ( 'NONE', #21329, 999.9999999999998863 ) ;
#75815 = CARTESIAN_POINT ( 'NONE',  ( 181.6067143826203676, 267.9940397974941675, 15.00604427482618242 ) ) ;
#75816 = CARTESIAN_POINT ( 'NONE',  ( 101.2839494695023603, 229.2833772461660544, -9.188101187500095079 ) ) ;
#75817 = CARTESIAN_POINT ( 'NONE',  ( 12.50787272796288896, 10.14754757982087874, -5.678558825948276656 ) ) ;
#75818 = CARTESIAN_POINT ( 'NONE',  ( 162.5189332652596761, 275.0194079713638189, -15.39703335036588250 ) ) ;
#75819 = CARTESIAN_POINT ( 'NONE',  ( 162.8751945631634612, 272.8900720096677333, -16.40198242748087054 ) ) ;
#75821 = CARTESIAN_POINT ( 'NONE',  ( 83.12755468652130730, 42.05662557703112014, -4.534451112896598524 ) ) ;
#75820 = CARTESIAN_POINT ( 'NONE',  ( 17.30334773395576775, 15.15404122711132651, 8.090169943749479842 ) ) ;
#75822 = CARTESIAN_POINT ( 'NONE',  ( 201.5036534377215958, 270.3153034880852488, -10.25451236307256409 ) ) ;
#75823 = CARTESIAN_POINT ( 'NONE',  ( 198.6894790592683080, 286.5067226703918095, -17.06774375037124614 ) ) ;
#75824 = CARTESIAN_POINT ( 'NONE',  ( 173.5155000508206911, 267.4844645354696127, -16.73009763236219172 ) ) ;
#75825 = AXIS2_PLACEMENT_3D ( 'NONE', #52090, #83036, #21698 ) ;
#75826 = CARTESIAN_POINT ( 'NONE',  ( 42.70206918026079990, 25.44966523072497822, -2.296566073217252530E-15 ) ) ;
#75827 = LINE ( 'NONE', #75326, #11144 ) ;
#75828 = CARTESIAN_POINT ( 'NONE',  ( -78.57153713424663977, 57.64153020465174393, -10.00000000000000000 ) ) ;
#75829 = EDGE_LOOP ( 'NONE', ( #99638, #56235 ) ) ;
#75830 = CARTESIAN_POINT ( 'NONE',  ( 30.57771352727866443, 18.44966523072494979, -2.296566073217252530E-15 ) ) ;
#75831 = B_SPLINE_CURVE_WITH_KNOTS ( 'NONE', 3,
 ( #39518, #54219, #61828, #25340, #15227, #32938, #16744, #93277, #2056, #8647, #63345, #17237, #24838, #93790, #70442, #23833, #94781, #85708, #47632, #39025, #38534, #77037, #54727, #7643, #78059, #78564, #46637, #30942, #9149, #24350, #47135, #55223 ),
 .UNSPECIFIED., .F., .F.,
 ( 4, 2, 2, 2, 2, 2, 2, 2, 2, 2, 2, 2, 2, 2, 2, 4 ),
 ( 0.001523115973120424535, 0.002198702639335023152, 0.002874289305549621986, 0.004225462637978878201, 0.004901049304193506526, 0.005238842637300820254, 0.005407739303854516150, 0.005449963470492883745, 0.005492187637131250473, 0.005534411803769618068, 0.005576635970407985664, 0.005745532636961396197, 0.005914429303514805863, 0.006252222636621627798, 0.006590015969728450600, 0.006927809302835272534 ),
 .UNSPECIFIED. ) ;
#75832 = FACE_OUTER_BOUND ( 'NONE', #39045, .T. ) ;
#75833 = CARTESIAN_POINT ( 'NONE',  ( 147.4824818982269790, 275.1998434563504929, -4.972419998968698351 ) ) ;
#75834 = CARTESIAN_POINT ( 'NONE',  ( 196.5806080813426888, 290.1593943507663766, -16.31912166233602690 ) ) ;
#75835 = ADVANCED_FACE ( 'NONE', ( #37136 ), #43736, .T. ) ;
#75836 = VERTEX_POINT ( 'NONE', #81304 ) ;
#75837 = CARTESIAN_POINT ( 'NONE',  ( 70.32997052007365824, 61.22580503597990287, 14.81304146787438114 ) ) ;
#75838 = CARTESIAN_POINT ( 'NONE',  ( 159.6898930778639283, 254.0559870643349143, 16.90891900388599822 ) ) ;
#75839 = CARTESIAN_POINT ( 'NONE',  ( 153.6675463778983612, 266.9416252070789142, 16.49262662605783092 ) ) ;
#75840 = CARTESIAN_POINT ( 'NONE',  ( -13.42108286626701386, 23.34301056334149038, -10.00000000000000000 ) ) ;
#75841 = CARTESIAN_POINT ( 'NONE',  ( 140.8234218128096131, 252.1115022471902591, 10.00000000000009592 ) ) ;
#75842 = EDGE_CURVE ( 'NONE', #24595, #6796, #58442, .T. ) ;
#75843 = EDGE_LOOP ( 'NONE', ( #59230, #61983, #3458, #99996 ) ) ;
#75844 = CARTESIAN_POINT ( 'NONE',  ( 73.59537120146498523, 69.79291368717997557, 9.952181187355030545 ) ) ;
#75845 = AXIS2_PLACEMENT_3D ( 'NONE', #21422, #6715, #98935 ) ;
#75846 = VERTEX_POINT ( 'NONE', #42730 ) ;
#75847 = CARTESIAN_POINT ( 'NONE',  ( 202.9093905060991005, 279.1976216410395182, 16.97070083370504179 ) ) ;
#75848 = CARTESIAN_POINT ( 'NONE',  ( 77.99518601148065500, 61.05539905302716619, -15.87786080876372274 ) ) ;
#75850 = EDGE_CURVE ( 'NONE', #29132, #47356, #99600, .T. ) ;
#75849 = CARTESIAN_POINT ( 'NONE',  ( 182.6217066138594305, 291.1375281399239157, -10.79417329231678302 ) ) ;
#75851 = ORIENTED_EDGE ( 'NONE', *, *, #95301, .F. ) ;
#75852 = AXIS2_PLACEMENT_3D ( 'NONE', #52621, #37913, #83579 ) ;
#75854 = ADVANCED_FACE ( 'NONE', ( #22439 ), #45234, .F. ) ;
#75853 = CARTESIAN_POINT ( 'NONE',  ( 44.69460199273692069, 196.6115022471902591, 10.00000000000009592 ) ) ;
#75855 = CARTESIAN_POINT ( 'NONE',  ( 158.6991807772081415, 256.2500756557278692, 16.19856017798593939 ) ) ;
#75856 = CARTESIAN_POINT ( 'NONE',  ( 192.8453312832112090, 280.1102836227724424, -16.77340966031070835 ) ) ;
#75857 = CARTESIAN_POINT ( 'NONE',  ( 153.4976680152657877, 264.7812354846562926, -17.98840356897177273 ) ) ;
#75858 = B_SPLINE_CURVE_WITH_KNOTS ( 'NONE', 3,
 ( #98509, #23456, #21487, #52871 ),
 .UNSPECIFIED., .F., .F.,
 ( 4, 4 ),
 ( 0.04629403814142867696, 0.04887066958154943908 ),
 .UNSPECIFIED. ) ;
#75859 = CARTESIAN_POINT ( 'NONE',  ( 152.6740002182599767, 266.2078699576288159, -17.16212636348624088 ) ) ;
#75860 = VECTOR ( 'NONE', #41345, 1000.000000000000114 ) ;
#75861 = EDGE_CURVE ( 'NONE', #56977, #88596, #16450, .T. ) ;
#75862 = CARTESIAN_POINT ( 'NONE',  ( 41.11799749075662191, 32.24335787977766898, -9.188101187500008038 ) ) ;
#75863 = DIRECTION ( 'NONE',  ( 1.000000000000000000, 0.000000000000000000, 0.000000000000000000 ) ) ;
#75864 = EDGE_CURVE ( 'NONE', #44309, #68820, #67593, .T. ) ;
#75865 = CARTESIAN_POINT ( 'NONE',  ( -72.30469571560091424, 48.86078274006646183, -10.00000000000000000 ) ) ;
#75866 = CARTESIAN_POINT ( 'NONE',  ( 87.65988181639181676, 45.35027930547009589, 6.479635358970763370 ) ) ;
#75867 = ORIENTED_EDGE ( 'NONE', *, *, #20309, .F. ) ;
#75868 = ORIENTED_EDGE ( 'NONE', *, *, #78116, .F. ) ;
#75869 = CARTESIAN_POINT ( 'NONE',  ( 72.04834849415195208, 72.28436413801230742, -0.8995985284803106330 ) ) ;
#75870 = DIRECTION ( 'NONE',  ( -0.000000000000000000, -0.000000000000000000, -1.000000000000000000 ) ) ;
#75872 = CARTESIAN_POINT ( 'NONE',  ( 79.73371708168252781, 56.78064988272082303, 16.21239358597816604 ) ) ;
#75871 = VECTOR ( 'NONE', #41179, 1000.000000000000000 ) ;
#75874 = CARTESIAN_POINT ( 'NONE',  ( 147.7112127936102866, 274.8036699242858276, -9.124700685424272706 ) ) ;
#75873 = FACE_OUTER_BOUND ( 'NONE', #19426, .T. ) ;
#75875 = DIRECTION ( 'NONE',  ( 1.000000000000000000, 0.000000000000000000, 0.000000000000000000 ) ) ;
#75876 = CARTESIAN_POINT ( 'NONE',  ( 201.0150177425703077, 274.8767133061161303, -13.89391286736939612 ) ) ;
#75877 = CARTESIAN_POINT ( 'NONE',  ( 75.82000616564076267, 60.49516838392244011, -15.67118054971322572 ) ) ;
#75878 = CARTESIAN_POINT ( 'NONE',  ( 82.08371825655493126, 40.78504432597228657, 1.422816544139647199 ) ) ;
#75879 = CARTESIAN_POINT ( 'NONE',  ( 187.7710022618638277, 277.0665775429750397, -17.72351784843695555 ) ) ;
#75880 = CARTESIAN_POINT ( 'NONE',  ( 77.25314033157172844, 63.01322228697468830, -15.27545204580677485 ) ) ;
#75881 = CARTESIAN_POINT ( 'NONE',  ( 178.0655552872740088, 255.4621687460560508, 4.946877401895048543 ) ) ;
#75882 = CARTESIAN_POINT ( 'NONE',  ( 111.3514947884964670, 235.0958772461660544, -9.188101187500095079 ) ) ;
#75883 = ORIENTED_EDGE ( 'NONE', *, *, #55817, .T. ) ;
#75884 = CARTESIAN_POINT ( 'NONE',  ( 183.4307448953204300, 260.0939146214054745, -9.483231343634749066 ) ) ;
#75885 = CARTESIAN_POINT ( 'NONE',  ( 43.73469409959700016, 27.11110640527295956, -2.839279412974138328 ) ) ;
#75886 = CARTESIAN_POINT ( 'NONE',  ( 191.7218012215406304, 275.0451209121254124, 16.76516018751371107 ) ) ;
#75887 = ORIENTED_EDGE ( 'NONE', *, *, #91423, .F. ) ;
#75888 = AXIS2_PLACEMENT_3D ( 'NONE', #97885, #58841, #59337 ) ;
#75889 = CARTESIAN_POINT ( 'NONE',  ( 73.80638704669732419, 68.31061168272384521, -11.57820046455322149 ) ) ;
#75890 = CARTESIAN_POINT ( 'NONE',  ( 180.1168005803277481, 295.2192856762299016, -2.191971455912026467 ) ) ;
#75891 = CARTESIAN_POINT ( 'NONE',  ( 157.2744851780909414, 258.2395962677452985, 18.17792129701959070 ) ) ;
#75892 = CARTESIAN_POINT ( 'NONE',  ( 206.0930919633010774, 273.6832889610345774, -9.866500005465628220 ) ) ;
#75893 = B_SPLINE_CURVE_WITH_KNOTS ( 'NONE', 3,
 ( #15627, #55126, #46526, #38932 ),
 .UNSPECIFIED., .F., .F.,
 ( 4, 4 ),
 ( 0.004991743399790857412, 0.009976538136425933123 ),
 .UNSPECIFIED. ) ;
#75894 = CARTESIAN_POINT ( 'NONE',  ( 170.8463542321686077, 287.4393069310528972, -8.645854640182026429 ) ) ;
#75895 = ORIENTED_EDGE ( 'NONE', *, *, #2786, .T. ) ;
#75896 = CARTESIAN_POINT ( 'NONE',  ( 195.0933678165431502, 292.7353700524613487, 15.12141487717723365 ) ) ;
#75897 = VERTEX_POINT ( 'NONE', #69029 ) ;
#75898 = CARTESIAN_POINT ( 'NONE',  ( -105.0000000000000000, 4.999999999999999112, -14.21260523776212281 ) ) ;
#75899 = ORIENTED_EDGE ( 'NONE', *, *, #99840, .T. ) ;
#75900 = CARTESIAN_POINT ( 'NONE',  ( 23.45662567177863167, 195.8967562850347122, -4.648177544792955347E-16 ) ) ;
#75901 = CARTESIAN_POINT ( 'NONE',  ( 195.7200744708509887, 265.3358093963507827, 4.285174003455722413 ) ) ;
#75902 = CARTESIAN_POINT ( 'NONE',  ( -11.77978294824862893, 175.5530062829863311, 1.347971487989956912E-14 ) ) ;
#75903 = CARTESIAN_POINT ( 'NONE',  ( 83.03413861592977696, 46.38630032584844542, 11.19405999254725437 ) ) ;
#75905 = CARTESIAN_POINT ( 'NONE',  ( 69.79485179726921729, 63.14629169217509030, -13.66398113955644789 ) ) ;
#75904 = DIRECTION ( 'NONE',  ( 0.4999999999999992784, -0.8660254037844390407, 0.000000000000000000 ) ) ;
#75906 = CARTESIAN_POINT ( 'NONE',  ( 201.3053499423511425, 281.9759013948520874, -16.75960365258566398 ) ) ;
#75907 = VERTEX_POINT ( 'NONE', #60922 ) ;
#75908 = CARTESIAN_POINT ( 'NONE',  ( 190.5653282632609091, 300.5781646174276602, -5.775635208185608604 ) ) ;
#75909 = CARTESIAN_POINT ( 'NONE',  ( 71.40961132680497769, 62.47877890195463380, 13.99073973727416842 ) ) ;
#75910 = CARTESIAN_POINT ( 'NONE',  ( 190.5837197087969912, 264.0079844486248817, -9.604741279133001797 ) ) ;
#75911 = CARTESIAN_POINT ( 'NONE',  ( 171.4692916405222718, 250.4214803585759626, -0.2564616657247425491 ) ) ;
#75912 = CARTESIAN_POINT ( 'NONE',  ( 192.7848161478432303, 271.7584063516355855, -14.73987874102306961 ) ) ;
#75913 = CARTESIAN_POINT ( 'NONE',  ( 71.76780065431621836, 72.18842372171909005, 3.264426277842164659 ) ) ;
#75914 = CARTESIAN_POINT ( 'NONE',  ( 84.35478657919151146, 45.19241756715437930, 9.088159741279909554 ) ) ;
#75915 = DIRECTION ( 'NONE',  ( -0.2575544297740129385, 0.9662637919863205083, 0.000000000000000000 ) ) ;
#75916 = CARTESIAN_POINT ( 'NONE',  ( 155.5660013421004919, 261.1987770755905558, 17.28709111629370199 ) ) ;
#75917 = CARTESIAN_POINT ( 'NONE',  ( 70.63918758082388649, 61.42057648183527618, -14.80585868731052024 ) ) ;
#75918 = CARTESIAN_POINT ( 'NONE',  ( 112.9278751967105450, 247.5530062829863311, -4.648177544792955347E-16 ) ) ;
#75919 = AXIS2_PLACEMENT_3D ( 'NONE', #85390, #83894, #30142 ) ;
#75920 = CARTESIAN_POINT ( 'NONE',  ( 85.20852645963621796, 213.8768266524159856, -9.188101187500091527 ) ) ;
#75921 = CARTESIAN_POINT ( 'NONE',  ( 159.2122473525774069, 254.8832937285494609, -16.22689353966294590 ) ) ;
#75922 = CARTESIAN_POINT ( 'NONE',  ( 197.5333837132704673, 287.4243462569709209, 17.22026250574119288 ) ) ;
#75923 = DIRECTION ( 'NONE',  ( 0.6544109481086042290, 0.7561390817803280706, 0.000000000000000000 ) ) ;
#75924 = B_SPLINE_CURVE_WITH_KNOTS ( 'NONE', 3,
 ( #75784, #99078, #60538, #69145, #99570, #22558, #21570, #68649, #44352, #60042 ),
 .UNSPECIFIED., .F., .F.,
 ( 4, 2, 2, 2, 4 ),
 ( 0.001272943234969431620, 0.001710735386977082009, 0.002148527538984732616, 0.002586319690992383222, 0.003024111843000033394 ),
 .UNSPECIFIED. ) ;
#75925 = EDGE_CURVE ( 'NONE', #62719, #17777, #60420, .T. ) ;
#75927 = CARTESIAN_POINT ( 'NONE',  ( 196.1749740761792111, 288.8619730569873809, -17.33086882175758703 ) ) ;
#75926 = AXIS2_PLACEMENT_3D ( 'NONE', #93631, #24198, #86065 ) ;
#75928 = CARTESIAN_POINT ( 'NONE',  ( 207.1432938686257046, 271.8642859028066141, -6.405155839440290322 ) ) ;
#75929 = DIRECTION ( 'NONE',  ( 0.3103181967972122313, -0.9506327454577433445, 0.000000000000000000 ) ) ;
#75931 = LINE ( 'NONE', #52588, #88513 ) ;
#75930 = CARTESIAN_POINT ( 'NONE',  ( 73.07600783879472317, 69.60248043393922046, -9.824339152688605026 ) ) ;
#75932 = CARTESIAN_POINT ( 'NONE',  ( 120.6082041558992586, 228.8932355074535394, -2.679491924311248496 ) ) ;
#75933 = ADVANCED_FACE ( 'NONE', ( #39111 ), #78151, .T. ) ;
#75934 = CARTESIAN_POINT ( 'NONE',  ( 38.43992769770077444, 34.14441083166263979, 10.00000000000000533 ) ) ;
#75935 = DIRECTION ( 'NONE',  ( -0.8660254037844387076, -0.4999999999999998890, -0.000000000000000000 ) ) ;
#75936 = CARTESIAN_POINT ( 'NONE',  ( 82.18797279649203347, 54.21966230526519581, 15.63691867135833036 ) ) ;
#75937 = CARTESIAN_POINT ( 'NONE',  ( 72.27517474642483819, 72.00281888946810227, 3.513552353559626251 ) ) ;
#75938 = EDGE_CURVE ( 'NONE', #43464, #4742, #22929, .T. ) ;
#75939 = VECTOR ( 'NONE', #6182, 1000.000000000000114 ) ;
#75940 =( BOUNDED_CURVE ( )  B_SPLINE_CURVE ( 1, ( #60527, #1250 ),
 .UNSPECIFIED., .F., .T. ) 
 B_SPLINE_CURVE_WITH_KNOTS ( ( 2, 2 ),
 ( 0.000000000000000000, 0.0009374999959032195417 ),
 .UNSPECIFIED. ) 
 CURVE ( )  GEOMETRIC_REPRESENTATION_ITEM ( )  RATIONAL_B_SPLINE_CURVE ( ( 0.9368410486966849415, 0.9368410486966849415 ) ) 
 REPRESENTATION_ITEM ( '' )  );
#75941 = CARTESIAN_POINT ( 'NONE',  ( 28.53781555160951555, 187.2833772461660544, -9.188101187500095079 ) ) ;
#75942 = CARTESIAN_POINT ( 'NONE',  ( 166.0506673010352472, 274.1027903476490337, -16.62009509085023851 ) ) ;
#75943 = CARTESIAN_POINT ( 'NONE',  ( 199.5396699312275928, 277.5950600280153822, 15.20170681613290142 ) ) ;
#75944 = CARTESIAN_POINT ( 'NONE',  ( 81.09727246379429744, 50.28454668112130577, -14.41009495042581712 ) ) ;
#75945 = CARTESIAN_POINT ( 'NONE',  ( 71.72790558683757922, 72.47596629505412125, -1.350878852920679662 ) ) ;
#75946 = CARTESIAN_POINT ( 'NONE',  ( 43.80151329331025067, 196.0958772461660544, -9.188101187500095079 ) ) ;
#75947 = VECTOR ( 'NONE', #83189, 1000.000000000000000 ) ;
#75948 = CARTESIAN_POINT ( 'NONE',  ( 24.72364882272980324, 19.98920272979926693, 7.433330006724137462 ) ) ;
#75949 = FACE_OUTER_BOUND ( 'NONE', #43462, .T. ) ;
#75950 = CARTESIAN_POINT ( 'NONE',  ( 149.6564118588553924, 271.4344863124460971, -11.76165597393390172 ) ) ;
#75951 = CARTESIAN_POINT ( 'NONE',  ( 5.721601707324312613, 18.70171378149916563, -9.188101187500004485 ) ) ;
#75952 = CARTESIAN_POINT ( 'NONE',  ( 204.6475128369918082, 276.1871054541632020, -13.72068618491070779 ) ) ;
#75953 = CARTESIAN_POINT ( 'NONE',  ( 202.8126086360731222, 269.9569268784645146, -6.432707174703383046 ) ) ;
#75954 = CARTESIAN_POINT ( 'NONE',  ( 32.18695666311190706, 46.02670049433633181, 10.00000000000000000 ) ) ;
#75955 = CARTESIAN_POINT ( 'NONE',  ( 178.1538850474519506, 275.9401529576537087, 16.36541506392882539 ) ) ;
#75956 = CARTESIAN_POINT ( 'NONE',  ( 72.74023158506105347, 61.92935225774390773, 14.60112725577257820 ) ) ;
#75957 = CARTESIAN_POINT ( 'NONE',  ( 153.5689166488172646, 264.6578292313752740, 18.05965550300112099 ) ) ;
#75958 =( BOUNDED_CURVE ( )  B_SPLINE_CURVE ( 2, ( #28301, #22583, #90154, #82568, #13131, #89666, #12633, #11638, #42989 ),
 .UNSPECIFIED., .F., .T. ) 
 B_SPLINE_CURVE_WITH_KNOTS ( ( 3, 2, 2, 2, 3 ),
 ( 0.3669354838709677491, 0.3682795698924731242, 0.3709677419354838745, 0.3736559139784946248, 0.3750000000000000000 ),
 .UNSPECIFIED. ) 
 CURVE ( )  GEOMETRIC_REPRESENTATION_ITEM ( )  RATIONAL_B_SPLINE_CURVE ( ( 0.9330127018922194093, 0.9330127018922194093, 1.000000000000000000, 0.8660254037844387076, 1.000000000000000000, 0.8660254037844387076, 1.000000000000000000, 0.9330127018922194093, 0.9330127018922194093 ) ) 
 REPRESENTATION_ITEM ( '' )  );
#75959 = CARTESIAN_POINT ( 'NONE',  ( 153.0305350670531936, 277.3750776671890890, 8.290292975357761662 ) ) ;
#75960 = CARTESIAN_POINT ( 'NONE',  ( 87.69397940208136788, 45.37340796770510565, -6.500714127684745769 ) ) ;
#75961 = CARTESIAN_POINT ( 'NONE',  ( 104.0173421519710217, 220.8615022471902023, 5.000000000000051514 ) ) ;
#75962 = CARTESIAN_POINT ( 'NONE',  ( 161.4469036912142599, 251.0127554125742222, 12.93933463576739307 ) ) ;
#75963 = EDGE_CURVE ( 'NONE', #11410, #36862, #91887, .T. ) ;
#75964 = CARTESIAN_POINT ( 'NONE',  ( 164.6958324620632368, 269.3431737359563272, -16.31609373033956345 ) ) ;
#75965 = ORIENTED_EDGE ( 'NONE', *, *, #46768, .F. ) ;
#75966 = CARTESIAN_POINT ( 'NONE',  ( 56.79189435007682363, 203.5958772461660544, -9.188101187500095079 ) ) ;
#75967 = VERTEX_POINT ( 'NONE', #8738 ) ;
#75968 = DIRECTION ( 'NONE',  ( 0.8660254037844395958, 0.4999999999999985567, 0.000000000000000000 ) ) ;
#75969 = FACE_OUTER_BOUND ( 'NONE', #68588, .T. ) ;
#75970 = CARTESIAN_POINT ( 'NONE',  ( -19.65312891409030271, 93.06504152958497400, 59.99999999999999289 ) ) ;
#75971 = ORIENTED_EDGE ( 'NONE', *, *, #11169, .T. ) ;
#75972 = CARTESIAN_POINT ( 'NONE',  ( 198.2505066714982149, 285.2670451491296149, 0.000000000000000000 ) ) ;
#75974 = EDGE_CURVE ( 'NONE', #32652, #87428, #76644, .T. ) ;
#75973 = CARTESIAN_POINT ( 'NONE',  ( 79.18282792688175675, 45.86070727306254469, -12.48096782606623734 ) ) ;
#75975 = B_SPLINE_CURVE_WITH_KNOTS ( 'NONE', 3,
 ( #76547, #22831, #99849, #61322 ),
 .UNSPECIFIED., .F., .F.,
 ( 4, 4 ),
 ( 0.01071166683732669572, 0.01632733781203283066 ),
 .UNSPECIFIED. ) ;
#75976 = DIRECTION ( 'NONE',  ( 1.000000000000000000, 0.000000000000000000, 0.000000000000000000 ) ) ;
#75977 = CARTESIAN_POINT ( 'NONE',  ( 176.3483583558151508, 274.3708778633847487, -17.64881272765552822 ) ) ;
#75978 = CYLINDRICAL_SURFACE ( 'NONE', #11743, 45.00000000000000000 ) ;
#75979 = CARTESIAN_POINT ( 'NONE',  ( 156.6938127249734976, 259.2453504591003934, 17.44495368413245728 ) ) ;
#75980 = ORIENTED_EDGE ( 'NONE', *, *, #75799, .F. ) ;
#75981 = CARTESIAN_POINT ( 'NONE',  ( 19.25324864145614967, 26.51421378149919761, -9.188101187500004485 ) ) ;
#75982 = CARTESIAN_POINT ( 'NONE',  ( 69.60857895278438434, 70.05621065339627762, -4.634882221859216500 ) ) ;
#75983 = CARTESIAN_POINT ( 'NONE',  ( 40.60966550219796289, 208.6868197944957330, 17.47570218321535762 ) ) ;
#75984 = EDGE_CURVE ( 'NONE', #78709, #95321, #6748, .T. ) ;
#75985 = EDGE_LOOP ( 'NONE', ( #70401, #35952, #12252, #26358 ) ) ;
#75986 = CARTESIAN_POINT ( 'NONE',  ( 135.6272693901030095, 249.1115022471902591, 10.00000000000009592 ) ) ;
#75987 = CARTESIAN_POINT ( 'NONE',  ( 159.2713554375903300, 254.7809155221686410, -15.70062444474382168 ) ) ;
#75988 = ORIENTED_EDGE ( 'NONE', *, *, #1627, .F. ) ;
#75990 = CARTESIAN_POINT ( 'NONE',  ( 47.89168550319194395, 74.68847913791599069, 10.00000000000000000 ) ) ;
#75989 = CARTESIAN_POINT ( 'NONE',  ( 159.2990852460085023, 282.6395706699606762, -3.314431380743207978 ) ) ;
#75991 = CARTESIAN_POINT ( 'NONE',  ( 67.78902524216930203, 70.26539227734573956, -0.4897883682968208752 ) ) ;
#75992 = CARTESIAN_POINT ( 'NONE',  ( 204.6780326111993986, 276.1342436545999703, 14.85609018352459287 ) ) ;
#75993 = CARTESIAN_POINT ( 'NONE',  ( -40.67952639183666008, 27.60432558407080350, -10.00000000000000000 ) ) ;
#75994 = CARTESIAN_POINT ( 'NONE',  ( 81.17232691891706509, 55.55242957854174080, 16.36487835605630536 ) ) ;
#75995 = CARTESIAN_POINT ( 'NONE',  ( 204.1656981441084611, 271.5570760979641136, 9.881240885324146461 ) ) ;
#75996 = CARTESIAN_POINT ( 'NONE',  ( 134.0307085979839883, 242.0643266524160140, 9.188101187500095079 ) ) ;
#75997 = AXIS2_PLACEMENT_3D ( 'NONE', #91919, #69569, #91410 ) ;
#75998 = CARTESIAN_POINT ( 'NONE',  ( 177.5865089022509551, 268.7852845103913069, 17.37969943402860906 ) ) ;
#75999 = CARTESIAN_POINT ( 'NONE',  ( 182.2689230490940986, 259.9811410596485075, 9.155893851718131415 ) ) ;
#76000 = CARTESIAN_POINT ( 'NONE',  ( 68.83479979963041728, 219.7369531367911293, -4.594050593750048428 ) ) ;
#76001 = ORIENTED_EDGE ( 'NONE', *, *, #13925, .F. ) ;
#76002 = CARTESIAN_POINT ( 'NONE',  ( 170.1373231016024477, 264.2063840763735243, 16.55828558264352424 ) ) ;
#76003 = DIRECTION ( 'NONE',  ( -0.2502735827033040761, -0.9681751565707790164, 0.000000000000000000 ) ) ;
#76004 = EDGE_LOOP ( 'NONE', ( #14408, #92613, #14438, #42409 ) ) ;
#76005 = AXIS2_PLACEMENT_3D ( 'NONE', #91758, #22322, #53224 ) ;
#76006 = VERTEX_POINT ( 'NONE', #39609 ) ;
#76007 = ORIENTED_EDGE ( 'NONE', *, *, #52189, .F. ) ;
#76008 = FACE_BOUND ( 'NONE', #37165, .T. ) ;
#76009 = CARTESIAN_POINT ( 'NONE',  ( 66.47155029869672660, 67.83944574720587184, 6.769174700624444263 ) ) ;
#76010 = CARTESIAN_POINT ( 'NONE',  ( 197.9367325884184083, 286.8643941967906130, 16.93519219127947295 ) ) ;
#76011 = CARTESIAN_POINT ( 'NONE',  ( 82.84795146572012925, 42.04542452314480272, -6.343602513311916269 ) ) ;
#76012 = CARTESIAN_POINT ( 'NONE',  ( 81.45345171730303946, 56.09117390121627977, 16.06974809975275420 ) ) ;
#76013 = CARTESIAN_POINT ( 'NONE',  ( 194.4889937320412230, 293.7821766735966662, 14.99892588346621380 ) ) ;
#76014 = CARTESIAN_POINT ( 'NONE',  ( 71.93069005840953878, 67.98409351856226124, 10.22207861052760158 ) ) ;
#76015 = EDGE_LOOP ( 'NONE', ( #3590, #46210, #54946, #3283 ) ) ;
#76016 = AXIS2_PLACEMENT_3D ( 'NONE', #39420, #70338, #69345 ) ;
#76017 = PLANE ( 'NONE',  #17104 ) ;
#76018 = VERTEX_POINT ( 'NONE', #61427 ) ;
#76019 = ADVANCED_FACE ( 'NONE', ( #61919, #14833 ), #45721, .F. ) ;
#76020 = CARTESIAN_POINT ( 'NONE',  ( 76.26909101152743631, 50.98313773053103404, -15.54286448327743742 ) ) ;
#76021 = FACE_OUTER_BOUND ( 'NONE', #6473, .T. ) ;
#76022 = CARTESIAN_POINT ( 'NONE',  ( 164.9356397357043704, 244.9700873293209042, 2.799217332519396972 ) ) ;
#76023 = VECTOR ( 'NONE', #16004, 1000.000000000000114 ) ;
#76024 = CARTESIAN_POINT ( 'NONE',  ( -29.37075727991403440, 94.88921800892813962, 44.57229221387616036 ) ) ;
#76025 = CARTESIAN_POINT ( 'NONE',  ( 195.0437424211503412, 279.4124847088495471, 16.44665416634688171 ) ) ;
#76026 = CARTESIAN_POINT ( 'NONE',  ( 162.9364957791611630, 261.5460700938506875, 17.26453991925339082 ) ) ;
#76027 = CARTESIAN_POINT ( 'NONE',  ( 144.4230134433972239, 248.0643266524160140, 9.188101187500095079 ) ) ;
#76028 = ORIENTED_EDGE ( 'NONE', *, *, #93985, .T. ) ;
#76029 = CARTESIAN_POINT ( 'NONE',  ( 88.16762080519842470, 44.42520534355205797, 4.589585637743891944 ) ) ;
#76030 = CARTESIAN_POINT ( 'NONE',  ( 85.75643568251058468, 43.97353779226914838, 5.730478947345492458 ) ) ;
#76031 = DIRECTION ( 'NONE',  ( -0.000000000000000000, -0.000000000000000000, -1.000000000000000000 ) ) ;
#76032 = CIRCLE ( 'NONE', #35579, 11.89249999999999652 ) ;
#76033 = CARTESIAN_POINT ( 'NONE',  ( 73.01638763941097920, 70.78844651441271196, 7.463027675286954654 ) ) ;
#76034 = CARTESIAN_POINT ( 'NONE',  ( 68.96171688564015767, 67.43038479987662015, -8.781394817860746826 ) ) ;
#76035 = ORIENTED_EDGE ( 'NONE', *, *, #37222, .F. ) ;
#76036 = CARTESIAN_POINT ( 'NONE',  ( 199.1379133944519424, 266.8226340275038524, 4.550351456204111855 ) ) ;
#76037 = DIRECTION ( 'NONE',  ( -0.000000000000000000, 1.000000000000000000, -0.000000000000000000 ) ) ;
#76038 = CARTESIAN_POINT ( 'NONE',  ( -110.0000000000000000, 0.000000000000000000, 59.99999999999999289 ) ) ;
#76039 = CARTESIAN_POINT ( 'NONE',  ( 186.2798660816079632, 264.0713031700501006, -12.82791401631097550 ) ) ;
#76040 = CARTESIAN_POINT ( 'NONE',  ( 202.6574465548223145, 267.4804609884895967, 0.8726363535044180386 ) ) ;
#76041 = ORIENTED_EDGE ( 'NONE', *, *, #75963, .T. ) ;
#76042 = CARTESIAN_POINT ( 'NONE',  ( 88.06269261788010283, 43.61796610520789841, 0.05835779599787610517 ) ) ;
#76043 = CARTESIAN_POINT ( 'NONE',  ( 183.3250138703919561, 280.8103892703075530, 16.49174253902363674 ) ) ;
#76044 = CARTESIAN_POINT ( 'NONE',  ( 164.4781197247689306, 245.7625352337404649, -1.511762618280499515 ) ) ;
#76045 = CARTESIAN_POINT ( 'NONE',  ( 193.0673848936551735, 268.2732046201192020, 12.66768335688180436 ) ) ;
#76046 = EDGE_CURVE ( 'NONE', #40956, #99081, #46533, .T. ) ;
#76047 = CARTESIAN_POINT ( 'NONE',  ( 27.95316317257044858, 17.10801979619929725, 3.090169943749476733 ) ) ;
#76048 = CARTESIAN_POINT ( 'NONE',  ( 41.50249547274756878, 124.4848494355456836, -10.00000000000000000 ) ) ;
#76049 = CARTESIAN_POINT ( 'NONE',  ( 204.7200661083698776, 274.0614395018808978, 12.25436898028725530 ) ) ;
#76050 = CARTESIAN_POINT ( 'NONE',  ( 151.3511865740561007, 278.6745403919405248, -1.693856907688049862 ) ) ;
#76051 = CARTESIAN_POINT ( 'NONE',  ( 159.9014600375868440, 253.6895423408921886, 15.57825579621527368 ) ) ;
#76052 = EDGE_CURVE ( 'NONE', #45778, #45450, #7715, .T. ) ;
#76053 = CARTESIAN_POINT ( 'NONE',  ( 71.91872812886755639, 71.71754829396212472, -3.869976083996915506 ) ) ;
#76054 = CARTESIAN_POINT ( 'NONE',  ( -15.46727382606978374, 168.0024278399160664, -9.188101187500093303 ) ) ;
#76055 = CARTESIAN_POINT ( 'NONE',  ( 3.113790753877909712, 26.87087736965101570, -10.00000000000000000 ) ) ;
#76057 = ORIENTED_EDGE ( 'NONE', *, *, #22610, .T. ) ;
#76056 = MANIFOLD_SOLID_BREP ( 'Cut-Extrude16', #2199 ) ;
#76058 = VECTOR ( 'NONE', #70495, 1000.000000000000114 ) ;
#76059 = CARTESIAN_POINT ( 'NONE',  ( 178.2112680352368272, 255.9238100178365869, 8.848909479073256534 ) ) ;
#76060 = CARTESIAN_POINT ( 'NONE',  ( 72.90882467353794993, 70.31776273714770298, -8.127408542227577470 ) ) ;
#76061 = CARTESIAN_POINT ( 'NONE',  ( 202.5775937153526627, 273.9552816370790538, -13.18159814775432181 ) ) ;
#76062 = CARTESIAN_POINT ( 'NONE',  ( 151.1811967613751335, 268.7934813906678642, -15.79361349403328418 ) ) ;
#76063 = CARTESIAN_POINT ( 'NONE',  ( 2.394500126984267840, 178.3149278399160949, -9.188101187500095079 ) ) ;
#76064 = CARTESIAN_POINT ( 'NONE',  ( 32.55392312662736032, 19.76426979415091267, 3.090169943749476733 ) ) ;
#76065 = CARTESIAN_POINT ( 'NONE',  ( 85.63659005182417161, 48.93691085330170409, 12.16422113781264969 ) ) ;
#76066 = B_SPLINE_CURVE_WITH_KNOTS ( 'NONE', 3,
 ( #96773, #14126, #59711, #83059 ),
 .UNSPECIFIED., .F., .F.,
 ( 4, 4 ),
 ( 0.009172812625567213288, 0.01512212324709697256 ),
 .UNSPECIFIED. ) ;
#76067 = CARTESIAN_POINT ( 'NONE',  ( 184.7894305693181138, 292.1317680087225881, 12.52679022050396895 ) ) ;
#76068 = CARTESIAN_POINT ( 'NONE',  ( 81.53115339410011586, 41.92267797703283350, -7.515177224638169839 ) ) ;
#76069 = CYLINDRICAL_SURFACE ( 'NONE', #39979, 70.00000000000002842 ) ;
#76070 = CARTESIAN_POINT ( 'NONE',  ( 149.9444379511524517, 276.8732903533755803, 4.578473933676738383 ) ) ;
#76071 = CARTESIAN_POINT ( 'NONE',  ( 178.7534805286849178, 255.1052391757385749, -3.938431664117528541 ) ) ;
#76072 = CARTESIAN_POINT ( 'NONE',  ( 151.0171360864231644, 269.0776428152087760, 14.21401713093731267 ) ) ;
#76073 = AXIS2_PLACEMENT_3D ( 'NONE', #51105, #43994, #59186 ) ;
#76074 = CARTESIAN_POINT ( 'NONE',  ( 182.3197145248164190, 295.2660807675984529, 1.016087631068208097 ) ) ;
#76075 = CARTESIAN_POINT ( 'NONE',  ( 49.89075441544350298, 209.6115022471903160, -5.000000000000047962 ) ) ;
#76076 = CARTESIAN_POINT ( 'NONE',  ( 40.48539884740146277, 126.3902902409112556, 10.00000000000000000 ) ) ;
#76077 = EDGE_CURVE ( 'NONE', #44339, #78746, #74127, .T. ) ;
#76078 = CARTESIAN_POINT ( 'NONE',  ( 189.9925954911225290, 301.5701668779311717, 0.1154287172046158938 ) ) ;
#76079 = CARTESIAN_POINT ( 'NONE',  ( 22.85469738715664434, 177.8768266524160140, -9.188101187500091527 ) ) ;
#76080 = LINE ( 'NONE', #7134, #77938 ) ;
#76081 = CARTESIAN_POINT ( 'NONE',  ( 79.20158430517960824, 60.00302764608026251, 16.13772425423236356 ) ) ;
#76082 = CARTESIAN_POINT ( 'NONE',  ( 38.02916716989017942, 40.14336893147758900, 7.433330006724141015 ) ) ;
#76083 = CARTESIAN_POINT ( 'NONE',  ( 118.1240276194171770, 250.5530062829863311, -4.648177544792955347E-16 ) ) ;
#76084 = DIRECTION ( 'NONE',  ( 0.4999999999999998890, -0.8660254037844385966, 0.000000000000000000 ) ) ;
#76085 = CARTESIAN_POINT ( 'NONE',  ( 155.0898745997320134, 262.0234527842152374, 17.05457557403769542 ) ) ;
#76086 = CARTESIAN_POINT ( 'NONE',  ( 186.5969764575044394, 267.2136708933791169, 13.23504358057708430 ) ) ;
#76087 = CARTESIAN_POINT ( 'NONE',  ( 120.0388121219830708, 240.1115022471902307, 10.00000000000009592 ) ) ;
#76088 = CARTESIAN_POINT ( 'NONE',  ( 164.0149191615929851, 281.5227187913443458, 8.861377439193347527 ) ) ;
#76089 = SHAPE_DEFINITION_REPRESENTATION ( #82432, #77412 ) ;
#76090 = CARTESIAN_POINT ( 'NONE',  ( 10.42942532566755354, 26.99752408145590721, 5.678558825948277544 ) ) ;
#76091 = CARTESIAN_POINT ( 'NONE',  ( 15.60912251971356213, 9.416033932543239615, -1.583844403245366905 ) ) ;
#76092 = CARTESIAN_POINT ( 'NONE',  ( 71.96630278948212833, 59.14415382642645369, 15.87175206068406830 ) ) ;
#76093 = CARTESIAN_POINT ( 'NONE',  ( 194.5047661587782386, 293.7548580291293092, 14.86680123054176583 ) ) ;
#76094 = ORIENTED_EDGE ( 'NONE', *, *, #76964, .F. ) ;
#76095 = CARTESIAN_POINT ( 'NONE',  ( 182.4138193503314653, 289.4190845564540950, 12.30891238242875829 ) ) ;
#76096 = CARTESIAN_POINT ( 'NONE',  ( 161.0972336787313282, 260.9823377472601464, -17.65804059120327452 ) ) ;
#76097 = CARTESIAN_POINT ( 'NONE',  ( 81.64979810624366507, 42.63530321562527803, 7.555915214504083544 ) ) ;
#76098 = DIRECTION ( 'NONE',  ( -0.7226656227773308183, -0.6911977992267138715, 0.000000000000000000 ) ) ;
#76099 = ORIENTED_EDGE ( 'NONE', *, *, #90386, .T. ) ;
#76100 = CARTESIAN_POINT ( 'NONE',  ( -68.37628875030422648, 42.44405361048389125, -10.00000000000000000 ) ) ;
#76101 = CARTESIAN_POINT ( 'NONE',  ( 82.35828269511283395, 40.36336379056105272, 1.060027914477761568 ) ) ;
#76102 = CARTESIAN_POINT ( 'NONE',  ( 76.52571587298459121, 63.66138771598714641, 14.90242614926261311 ) ) ;
#76103 = CARTESIAN_POINT ( 'NONE',  ( 203.5258219653775313, 278.1299310341851765, -16.21052911601769608 ) ) ;
#76104 = ORIENTED_EDGE ( 'NONE', *, *, #23068, .F. ) ;
#76105 = ORIENTED_EDGE ( 'NONE', *, *, #83815, .T. ) ;
#76107 = FACE_OUTER_BOUND ( 'NONE', #73233, .T. ) ;
#76106 = LINE ( 'NONE', #91811, #64846 ) ;
#76108 = EDGE_LOOP ( 'NONE', ( #19208, #92877, #100014, #97097 ) ) ;
#76109 = CARTESIAN_POINT ( 'NONE',  ( 151.3883635558152321, 268.4346579770563608, 15.44343517165679103 ) ) ;
#76110 = DIRECTION ( 'NONE',  ( -0.8660254037844379305, -0.5000000000000014433, -0.000000000000000000 ) ) ;
#76111 = CARTESIAN_POINT ( 'NONE',  ( 80.29526846451028632, 57.41841621455482425, -16.58920233904881414 ) ) ;
#76112 = CARTESIAN_POINT ( 'NONE',  ( 170.3127733705114224, 263.9010670580030364, 17.23448983536806622 ) ) ;
#76114 = ORIENTED_EDGE ( 'NONE', *, *, #76769, .T. ) ;
#76113 = B_SPLINE_CURVE_WITH_KNOTS ( 'NONE', 3,
 ( #34711, #96565, #58017, #99523, #53880, #91956, #91443, #45783, #53398, #23482 ),
 .UNSPECIFIED., .F., .F.,
 ( 4, 2, 2, 2, 4 ),
 ( 0.000000000000000000, 0.0002622400424272684142, 0.0005244800848545368285, 0.0007867201272818051885, 0.001048960169709073657 ),
 .UNSPECIFIED. ) ;
#76115 = CARTESIAN_POINT ( 'NONE',  ( 87.56962886756771525, 45.10300061070547173, -6.116038350875187213 ) ) ;
#76116 = EDGE_CURVE ( 'NONE', #23265, #9880, #71802, .T. ) ;
#76117 = EDGE_LOOP ( 'NONE', ( #36435, #97406 ) ) ;
#76118 = CARTESIAN_POINT ( 'NONE',  ( 206.5571822944673670, 272.8794609281530938, 10.95833005210827515 ) ) ;
#76119 = CARTESIAN_POINT ( 'NONE',  ( 74.52124453458169739, 63.30200860632920268, 14.49837560861971397 ) ) ;
#76120 = ORIENTED_EDGE ( 'NONE', *, *, #94321, .F. ) ;
#76121 = CARTESIAN_POINT ( 'NONE',  ( 190.1519139143167081, 301.2942192743771557, 4.481136594690903863 ) ) ;
#76122 = CARTESIAN_POINT ( 'NONE',  ( 78.26215446592701142, 47.40418697570542861, -14.30981545185047565 ) ) ;
#76123 = ORIENTED_EDGE ( 'NONE', *, *, #50822, .T. ) ;
#76124 = CARTESIAN_POINT ( 'NONE',  ( -38.61298035630893111, 26.97617139035147460, -10.00000000000000000 ) ) ;
#76125 = DIRECTION ( 'NONE',  ( 1.235257323912246174E-15, 1.000000000000000000, 0.000000000000000000 ) ) ;
#76126 = CARTESIAN_POINT ( 'NONE',  ( 170.5373622343556690, 269.7751423367952270, 17.81562764448176850 ) ) ;
#76127 = DIRECTION ( 'NONE',  ( 0.9681751565707763518, -0.2502735827033140681, 0.000000000000000000 ) ) ;
#76128 = VERTEX_POINT ( 'NONE', #68290 ) ;
#76129 = ORIENTED_EDGE ( 'NONE', *, *, #60755, .T. ) ;
#76130 = CARTESIAN_POINT ( 'NONE',  ( 156.3761965727711356, 267.2017284797204866, -16.34692893795439161 ) ) ;
#76131 = CARTESIAN_POINT ( 'NONE',  ( 83.32561943262588500, 42.79751196862224560, -6.107886559562847317 ) ) ;
#76132 = CARTESIAN_POINT ( 'NONE',  ( 162.7435819479956933, 250.7668427907593411, -13.06080741167749082 ) ) ;
#76133 = CARTESIAN_POINT ( 'NONE',  ( 190.4841013044967042, 300.7188538369516095, 4.682298117523464143 ) ) ;
#76134 = DIRECTION ( 'NONE',  ( -0.8660254037844387076, -0.4999999999999998890, -0.000000000000000000 ) ) ;
#76136 = CARTESIAN_POINT ( 'NONE',  ( 146.5665812168672915, 276.7862299711523519, -0.4280630669697406687 ) ) ;
#76135 = VECTOR ( 'NONE', #38037, 1000.000000000000000 ) ;
#76137 = CARTESIAN_POINT ( 'NONE',  ( 191.0481192767711036, 299.7419460525905492, -9.103377665618040737 ) ) ;
#76138 = CARTESIAN_POINT ( 'NONE',  ( 163.9896819828944672, 256.9390232144978086, 16.08371068233360290 ) ) ;
#76139 = CARTESIAN_POINT ( 'NONE',  ( 70.39753563717141560, 68.48327457168743138, 8.534146841718333931 ) ) ;
#76141 = CARTESIAN_POINT ( 'NONE',  ( 49.04287251715432205, 95.72274150194785136, 10.00000000000000000 ) ) ;
#76140 = CARTESIAN_POINT ( 'NONE',  ( 197.0226655822963551, 289.3937282992477549, -17.28982543158101493 ) ) ;
#76142 = CARTESIAN_POINT ( 'NONE',  ( 70.70420039156243774, 71.94848598797803163, 6.061257734329015641E-06 ) ) ;
#76143 = CARTESIAN_POINT ( 'NONE',  ( 171.0488218253813386, 288.2608493535105367, 4.157149925330108964 ) ) ;
#76144 = CARTESIAN_POINT ( 'NONE',  ( 78.08372258140214228, 47.78081774239645796, 14.00095081412197473 ) ) ;
#76145 = CARTESIAN_POINT ( 'NONE',  ( 98.17141035282828909, 236.6744531367911293, 4.594050593750047540 ) ) ;
#76146 = EDGE_LOOP ( 'NONE', ( #75715, #21285, #70763, #46522 ) ) ;
#76147 = CARTESIAN_POINT ( 'NONE',  ( 190.7616931697327516, 300.2380506225948125, -4.491414918766103881 ) ) ;
#76148 = CARTESIAN_POINT ( 'NONE',  ( 79.26202630790012904, 53.12952634897852278, -15.69712025940643230 ) ) ;
#76149 = CARTESIAN_POINT ( 'NONE',  ( 84.54826043205098074, 42.30827120018470566, 4.527376015812757615 ) ) ;
#76150 = CARTESIAN_POINT ( 'NONE',  ( 79.26278427487086731, 46.15226300323974584, 12.64627858079322742 ) ) ;
#76151 = CARTESIAN_POINT ( 'NONE',  ( 191.2278159864466431, 297.4307022214792937, -10.96893880474589267 ) ) ;
#76152 = CARTESIAN_POINT ( 'NONE',  ( 83.62455065227555906, 52.34512318633653649, -15.13772682721065621 ) ) ;
#76153 = VECTOR ( 'NONE', #78517, 1000.000000000000000 ) ;
#76154 = CARTESIAN_POINT ( 'NONE',  ( 165.5142259937072993, 283.5901604647961562, -8.273349223471056391 ) ) ;
#76155 = VERTEX_POINT ( 'NONE', #82559 ) ;
#76156 = CARTESIAN_POINT ( 'NONE',  ( 208.3863431123642727, 269.7112614563416173, -1.693909372230378851 ) ) ;
#76157 = CARTESIAN_POINT ( 'NONE',  ( 160.0081047537594543, 253.5048282741223602, -16.11956848123596941 ) ) ;
#76158 = CARTESIAN_POINT ( 'NONE',  ( 72.60043212129588142, 71.47019982953712258, 5.638345928473151858 ) ) ;
#76159 = CARTESIAN_POINT ( 'NONE',  ( 43.23318412030279489, 185.7677522451417929, -5.000000000000041744 ) ) ;
#76160 = CARTESIAN_POINT ( 'NONE',  ( 111.3514947884964670, 235.0958772461660544, -9.188101187500095079 ) ) ;
#76161 = CYLINDRICAL_SURFACE ( 'NONE', #91519, 70.00000000000002842 ) ;
#76162 = DIRECTION ( 'NONE',  ( -0.8660254037844378194, -0.5000000000000014433, -0.000000000000000000 ) ) ;
#76163 = CARTESIAN_POINT ( 'NONE',  ( 189.4827547918471851, 297.7068139993613727, 9.374012235039304031 ) ) ;
#76164 = CARTESIAN_POINT ( 'NONE',  ( 173.5466779927756704, 252.2311758790288252, -3.912256498803678095 ) ) ;
#76165 = CARTESIAN_POINT ( 'NONE',  ( 28.37526224051743284, 193.3149278399160949, -9.188101187500095079 ) ) ;
#76166 = CARTESIAN_POINT ( 'NONE',  ( 147.6787290359179110, 275.8338687843527168, -2.569013399972302381 ) ) ;
#76167 = ORIENTED_EDGE ( 'NONE', *, *, #28011, .T. ) ;
#76168 = CARTESIAN_POINT ( 'NONE',  ( 72.70715679364579387, 68.59801517648534741, 10.11885734070592413 ) ) ;
#76169 = CARTESIAN_POINT ( 'NONE',  ( 178.3855741922590994, 265.9601407903336394, 15.32162025640515068 ) ) ;
#76170 = EDGE_CURVE ( 'NONE', #41092, #12902, #81513, .T. ) ;
#76171 = DIRECTION ( 'NONE',  ( -0.000000000000000000, -0.000000000000000000, -1.000000000000000000 ) ) ;
#76172 = CARTESIAN_POINT ( 'NONE',  ( 147.2443490232117256, 275.6123016948292275, 5.226063659459642352 ) ) ;
#76173 = DIRECTION ( 'NONE',  ( -0.8660254037844357100, -0.5000000000000049960, -0.000000000000000000 ) ) ;
#76174 = ADVANCED_FACE ( 'NONE', ( #67294 ), #97723, .F. ) ;
#76175 = LINE ( 'NONE', #13371, #82314 ) ;
#76176 = CARTESIAN_POINT ( 'NONE',  ( 115.5463053363034476, 227.5177522451418213, 5.000000000000051514 ) ) ;
#76177 = EDGE_CURVE ( 'NONE', #43169, #92570, #39092, .T. ) ;
#76178 = EDGE_LOOP ( 'NONE', ( #65900, #81872, #78888, #69692 ) ) ;
#76179 = DIRECTION ( 'NONE',  ( -1.000000000000000000, 0.000000000000000000, 0.000000000000000000 ) ) ;
#76180 = EDGE_CURVE ( 'NONE', #34316, #35306, #13122, .T. ) ;
#76181 = CARTESIAN_POINT ( 'NONE',  ( 158.7695631051096257, 282.4121657607714155, -1.649238854537537158 ) ) ;
#76182 = LINE ( 'NONE', #30046, #62530 ) ;
#76183 = CARTESIAN_POINT ( 'NONE',  ( 10.89220085373657376, 189.3464784336661353, 1.353441290958777327E-15 ) ) ;
#76184 = CARTESIAN_POINT ( 'NONE',  ( 72.56357867676685203, 68.60059663970191934, -10.60869006465324205 ) ) ;
#76185 = CARTESIAN_POINT ( 'NONE',  ( 196.2123514992661057, 273.6774763844528024, 14.95493983070488930 ) ) ;
#76186 = CARTESIAN_POINT ( 'NONE',  ( 71.51902242164648271, 59.42281871825910144, -15.72106062734085086 ) ) ;
#76187 = DIRECTION ( 'NONE',  ( 0.5000000000000014433, -0.8660254037844378194, 0.000000000000000000 ) ) ;
#76189 = CARTESIAN_POINT ( 'NONE',  ( 74.76226857436894591, 201.7202760586659167, -5.415160957724236172E-17 ) ) ;
#76188 = CARTESIAN_POINT ( 'NONE',  ( 195.1313828796571386, 275.4209514540651185, -15.57016190239770914 ) ) ;
#76190 = CARTESIAN_POINT ( 'NONE',  ( 207.8725590214046406, 270.6011616060040410, 1.988011721677743093 ) ) ;
#76191 = CARTESIAN_POINT ( 'NONE',  ( 74.17656091806652796, 55.29306353059418910, 16.12363719729034983 ) ) ;
#76192 = CARTESIAN_POINT ( 'NONE',  ( 54.13067045125697518, 195.3927522451418213, 10.00000000000009948 ) ) ;
#76193 = CARTESIAN_POINT ( 'NONE',  ( 66.36286506768924198, 68.17188559719302532, -4.442151567769474951 ) ) ;
#76194 = VERTEX_POINT ( 'NONE', #28803 ) ;
#76195 = CARTESIAN_POINT ( 'NONE',  ( 13.51768745649715697, 168.6115022471901739, -5.000000000000041744 ) ) ;
#76196 = CARTESIAN_POINT ( 'NONE',  ( 163.7038023771459052, 247.1036922210055025, -6.448491958542482472 ) ) ;
#76197 = CARTESIAN_POINT ( 'NONE',  ( 137.1425535231280151, 259.1744531367911009, 4.594050593750047540 ) ) ;
#76198 = CARTESIAN_POINT ( 'NONE',  ( 29.82838080365165112, 20.14754757982091249, -5.678558825948276656 ) ) ;
#76199 = CARTESIAN_POINT ( 'NONE',  ( 207.5386549290987546, 271.1795004587326048, -7.943787175633387321 ) ) ;
#76200 = CARTESIAN_POINT ( 'NONE',  ( 83.70911819089758410, 52.26791303372475994, -15.08805761434582848 ) ) ;
#76201 = FACE_OUTER_BOUND ( 'NONE', #63097, .T. ) ;
#76203 = DIRECTION ( 'NONE',  ( -0.1860369090531061032, -0.9825427565607341984, 0.000000000000000000 ) ) ;
#76202 = CARTESIAN_POINT ( 'NONE',  ( 88.03161368674544462, 43.80918251920727613, 2.446934266190726959 ) ) ;
#76204 = CARTESIAN_POINT ( 'NONE',  ( 68.61953357195196190, 64.26322109196938470, 12.44723069995015408 ) ) ;
#76205 = VERTEX_POINT ( 'NONE', #29310 ) ;
#76206 = CARTESIAN_POINT ( 'NONE',  ( 64.47116044126103418, 196.4824982072973683, 3.021315404115420679E-15 ) ) ;
#76207 =( LENGTH_UNIT ( ) NAMED_UNIT ( * ) SI_UNIT ( .MILLI., .METRE. ) );
#76208 = LINE ( 'NONE', #29102, #36163 ) ;
#76209 = CARTESIAN_POINT ( 'NONE',  ( -0.2492734796364602656, 27.10516647459198225, 10.00000000000000000 ) ) ;
#76210 = CARTESIAN_POINT ( 'NONE',  ( 194.1563733927635838, 270.7326105280735078, -14.10882362769777743 ) ) ;
#76211 = ORIENTED_EDGE ( 'NONE', *, *, #18130, .F. ) ;
#76212 = CARTESIAN_POINT ( 'NONE',  ( 160.0940723892081223, 253.3559279617186917, 16.15485901636618138 ) ) ;
#76213 = LINE ( 'NONE', #44771, #84662 ) ;
#76214 = FACE_OUTER_BOUND ( 'NONE', #3378, .T. ) ;
#76215 = CARTESIAN_POINT ( 'NONE',  ( 206.1823507212516802, 271.5286882572439140, -8.119960357998227352 ) ) ;
#76216 = CARTESIAN_POINT ( 'NONE',  ( 89.54518929453067244, 234.0530062829863027, -4.648177544792955347E-16 ) ) ;
#76217 = CARTESIAN_POINT ( 'NONE',  ( 208.3863431123642727, 269.7112614563416173, -1.693909372230378851 ) ) ;
#76218 = VECTOR ( 'NONE', #30965, 1000.000000000000114 ) ;
#76219 = CARTESIAN_POINT ( 'NONE',  ( 200.8665851640556070, 282.7358642834317948, -16.69422397739980823 ) ) ;
#76220 = VERTEX_POINT ( 'NONE', #90658 ) ;
#76221 = CARTESIAN_POINT ( 'NONE',  ( 192.0331336666972391, 281.5685065300137353, 16.72509162371795099 ) ) ;
#76222 = CARTESIAN_POINT ( 'NONE',  ( 14.17036660571061546, 16.38052372038639604, 10.00000000000000533 ) ) ;
#76223 = FACE_OUTER_BOUND ( 'NONE', #2501, .T. ) ;
#76224 = ORIENTED_EDGE ( 'NONE', *, *, #6148, .F. ) ;
#76225 = CARTESIAN_POINT ( 'NONE',  ( 149.6877696051026305, 271.3801731027346591, 11.89134584187677390 ) ) ;
#76226 = DIRECTION ( 'NONE',  ( -0.4897629171537585258, 0.8718556560469402639, 0.000000000000000000 ) ) ;
#76227 = CARTESIAN_POINT ( 'NONE',  ( 189.0590152237434154, 297.0845166239263335, 8.082612471021599632 ) ) ;
#76228 = B_SPLINE_CURVE_WITH_KNOTS ( 'NONE', 3,
 ( #63173, #70266, #69272, #93101, #8481, #62659, #93611, #86044, #47469, #1391, #38865, #32270, #94117, #57063, #65666, #25692 ),
 .UNSPECIFIED., .F., .F.,
 ( 4, 1, 2, 2, 2, 1, 2, 2, 4 ),
 ( 0.000000000000000000, 0.1250000000000010547, 0.1875000000000006384, 0.2500000000000002220, 0.4999999999999973355, 0.6249999999999953371, 0.6874999999999966693, 0.7499999999999980016, 1.000000000000000000 ),
 .UNSPECIFIED. ) ;
#76229 = VERTEX_POINT ( 'NONE', #52094 ) ;
#76230 = CARTESIAN_POINT ( 'NONE',  ( 146.6363376198206652, 276.6654083370839885, -0.5879280619134327202 ) ) ;
#76231 = DIRECTION ( 'NONE',  ( -0.2702110370271922357, -0.9515975153008174869, 0.1464519181916024981 ) ) ;
#76232 = CARTESIAN_POINT ( 'NONE',  ( 204.6427704787179493, 276.1953194596412118, 13.28850621060895953 ) ) ;
#76233 = EDGE_CURVE ( 'NONE', #77324, #74259, #78909, .T. ) ;
#76234 = CARTESIAN_POINT ( 'NONE',  ( 69.53918912477176661, 62.67033094902271984, 13.85614356406449943 ) ) ;
#76235 = ORIENTED_EDGE ( 'NONE', *, *, #58254, .F. ) ;
#76236 = CARTESIAN_POINT ( 'NONE',  ( 107.4275774994220001, 223.6423013555409796, -4.594050593750043987 ) ) ;
#76237 = CARTESIAN_POINT ( 'NONE',  ( 155.2031798843469232, 261.8272022744961873, 18.50448283576785968 ) ) ;
#76238 = CARTESIAN_POINT ( 'NONE',  ( 73.34339640511194602, 69.67785411864186074, -9.916893174164222557 ) ) ;
#76239 = CARTESIAN_POINT ( 'NONE',  ( 178.4381536407659894, 269.1936824936634594, -17.11615640515828574 ) ) ;
#76240 = CARTESIAN_POINT ( 'NONE',  ( 81.52667467699143344, 42.23108980399940293, -8.023880245682178725 ) ) ;
#76241 = ORIENTED_EDGE ( 'NONE', *, *, #174, .T. ) ;
#76242 = ORIENTED_EDGE ( 'NONE', *, *, #62298, .T. ) ;
#76243 = VERTEX_POINT ( 'NONE', #13612 ) ;
#76244 = FACE_OUTER_BOUND ( 'NONE', #84852, .T. ) ;
#76246 = EDGE_CURVE ( 'NONE', #51127, #33408, #16149, .T. ) ;
#76245 = ORIENTED_EDGE ( 'NONE', *, *, #58080, .T. ) ;
#76247 = CARTESIAN_POINT ( 'NONE',  ( 68.87408322772347447, 69.31020849774787962, 5.424133776871966184 ) ) ;
#76248 = ORIENTED_EDGE ( 'NONE', *, *, #6359, .T. ) ;
#76249 = CARTESIAN_POINT ( 'NONE',  ( 163.7423057141168385, 247.0370024851108610, -6.909410042141566066 ) ) ;
#76251 = ADVANCED_FACE ( 'NONE', ( #6990 ), #83040, .T. ) ;
#76250 = CARTESIAN_POINT ( 'NONE',  ( 167.9307537431739661, 281.1416098987750729, 11.64201043039908434 ) ) ;
#76252 = CARTESIAN_POINT ( 'NONE',  ( -23.57130163085902552, 99.65262297949493586, 45.19937752447436452 ) ) ;
#76253 = CARTESIAN_POINT ( 'NONE',  ( 82.81311453349250939, 53.82731390497905721, -15.42448983893086734 ) ) ;
#76254 = ORIENTED_EDGE ( 'NONE', *, *, #72268, .T. ) ;
#76255 = CARTESIAN_POINT ( 'NONE',  ( 196.6195079739135849, 274.6088269242578690, -15.71717729878580094 ) ) ;
#76256 = CARTESIAN_POINT ( 'NONE',  ( 14.74991654177707723, 23.91421378149918198, 9.188101187500008038 ) ) ;
#76257 = CARTESIAN_POINT ( 'NONE',  ( 191.6779092374860625, 276.1752509429691145, -17.22939886907964890 ) ) ;
#76258 = CARTESIAN_POINT ( 'NONE',  ( 84.42663183290279960, 49.91580812419739743, -13.73522929182741059 ) ) ;
#76260 = ORIENTED_EDGE ( 'NONE', *, *, #46988, .T. ) ;
#76259 = CARTESIAN_POINT ( 'NONE',  ( 180.7701619213715958, 282.8660957359396093, 16.53338994692317954 ) ) ;
#76261 = CARTESIAN_POINT ( 'NONE',  ( 163.1691520398773321, 248.0297337694385931, 11.21816141384514331 ) ) ;
#76262 = CARTESIAN_POINT ( 'NONE',  ( 184.9627711092587674, 258.1544921998163318, 2.978903034762152124 ) ) ;
#76263 = DIRECTION ( 'NONE',  ( 0.4999999999999992784, -0.8660254037844390407, 0.000000000000000000 ) ) ;
#76264 = CARTESIAN_POINT ( 'NONE',  ( 147.1270795744234476, 264.4111747905818675, -1.822351119449947324E-15 ) ) ;
#76265 = CARTESIAN_POINT ( 'NONE',  ( 171.4292241046584877, 255.5488744981172431, 11.14177367849849887 ) ) ;
#76266 = CARTESIAN_POINT ( 'NONE',  ( 159.9665222620925817, 282.2299347244568253, 2.085082827276235395 ) ) ;
#76267 = VERTEX_POINT ( 'NONE', #60174 ) ;
#76268 = CARTESIAN_POINT ( 'NONE',  ( 182.6715392610496735, 271.9296818901224242, -16.02872276298343834 ) ) ;
#76269 = CARTESIAN_POINT ( 'NONE',  ( 70.75662654094317361, 63.45050265575406456, -13.26425860699792914 ) ) ;
#76270 = CARTESIAN_POINT ( 'NONE',  ( 160.1969820541083607, 255.1776831935258372, -16.37528374203482073 ) ) ;
#76271 = CARTESIAN_POINT ( 'NONE',  ( 10.68506269473765258, 163.6427522451417644, 1.119607411625061291E-15 ) ) ;
#76272 = CARTESIAN_POINT ( 'NONE',  ( 193.6071458082581955, 267.8835467034379008, -10.90750982005068259 ) ) ;
#76273 = CARTESIAN_POINT ( 'NONE',  ( 201.4660993003597582, 266.8443734887555365, -2.250696924963314416 ) ) ;
#76274 = CARTESIAN_POINT ( 'NONE',  ( 203.6076779758675741, 277.9881522651116370, -14.46320369641031256 ) ) ;
#76275 = CARTESIAN_POINT ( 'NONE',  ( 86.90280484423139740, 44.67138223063114566, -5.898473692909979249 ) ) ;
#76276 = CARTESIAN_POINT ( 'NONE',  ( 161.5029716424245407, 251.3413373469583973, -13.00020995489466458 ) ) ;
#76278 = CARTESIAN_POINT ( 'NONE',  ( 106.4790390313002888, 243.8297689869268936, -2.679491924311252493 ) ) ;
#76277 = CARTESIAN_POINT ( 'NONE',  ( -13.19395714113563045, 169.3149278399160949, -9.188101187500095079 ) ) ;
#76279 = CARTESIAN_POINT ( 'NONE',  ( 185.5618062172021894, 295.3137494393371298, 8.271460040209413833 ) ) ;
#76280 = ORIENTED_EDGE ( 'NONE', *, *, #12128, .F. ) ;
#76281 = ORIENTED_EDGE ( 'NONE', *, *, #57987, .F. ) ;
#76282 = DIRECTION ( 'NONE',  ( -0.6303371332823576312, -0.7763215174174805666, 0.000000000000000000 ) ) ;
#76283 = DIRECTION ( 'NONE',  ( -0.5000000000000012212, 0.8660254037844380415, 0.000000000000000000 ) ) ;
#76284 = EDGE_CURVE ( 'NONE', #73229, #18285, #59168, .T. ) ;
#76285 = B_SPLINE_CURVE_WITH_KNOTS ( 'NONE', 3,
 ( #15965, #77791, #78283, #39242 ),
 .UNSPECIFIED., .F., .F.,
 ( 4, 4 ),
 ( 0.02265161601259375185, 0.02890507703157969843 ),
 .UNSPECIFIED. ) ;
#76286 = DIRECTION ( 'NONE',  ( 0.5000000000000013323, -0.8660254037844378194, 0.000000000000000000 ) ) ;
#76287 = CARTESIAN_POINT ( 'NONE',  ( -40.67952639183666008, 27.60432558407080350, 10.00000000000000000 ) ) ;
#76288 = CARTESIAN_POINT ( 'NONE',  ( 162.5387916653087927, 249.1215499652694234, -10.44916066063070126 ) ) ;
#76289 = CARTESIAN_POINT ( 'NONE',  ( 83.98545619398112194, 45.63022158774919745, 9.896021495624898634 ) ) ;
#76290 = CARTESIAN_POINT ( 'NONE',  ( 150.1473662157767990, 276.5461327245939742, 3.629510331267637557 ) ) ;
#76291 = CARTESIAN_POINT ( 'NONE',  ( 17.19803509898326510, 189.9244531367911293, -4.594050593750046652 ) ) ;
#76292 = CARTESIAN_POINT ( 'NONE',  ( 127.8874276638293850, 235.4548013555409796, -4.594050593750042211 ) ) ;
#76293 = CARTESIAN_POINT ( 'NONE',  ( 181.8839543305726068, 294.0754964817877521, -6.330318412758383140 ) ) ;
#76294 = CARTESIAN_POINT ( 'NONE',  ( 172.0728039219370658, 285.9831811572526021, 11.38650458882361427 ) ) ;
#76295 = EDGE_CURVE ( 'NONE', #38684, #30963, #5015, .T. ) ;
#76296 = FACE_OUTER_BOUND ( 'NONE', #53043, .T. ) ;
#76297 = ADVANCED_FACE ( 'NONE', ( #99212 ), #90142, .F. ) ;
#76298 = CARTESIAN_POINT ( 'NONE',  ( 178.1976719649161964, 283.8584802497103396, -15.12167059147577675 ) ) ;
#76299 = CARTESIAN_POINT ( 'NONE',  ( 61.41971759977592171, 216.2677522451419065, -5.000000000000047962 ) ) ;
#76300 = CARTESIAN_POINT ( 'NONE',  ( 63.72375369157849434, 192.0095308348468564, 0.000000000000000000 ) ) ;
#76301 = CARTESIAN_POINT ( 'NONE',  ( 207.8792014703394671, 270.5896565469619759, -5.780233892547864905 ) ) ;
#76302 = CARTESIAN_POINT ( 'NONE',  ( 41.85954357502988898, 126.4744881464662001, 177.5919119679930134 ) ) ;
#76303 = CARTESIAN_POINT ( 'NONE',  ( 70.57238475796081900, 60.71229067232671639, -14.56237343984944665 ) ) ;
#76304 = CARTESIAN_POINT ( 'NONE',  ( 167.7842790755206011, 278.3773043237077331, 14.72622960804143766 ) ) ;
#76305 = CARTESIAN_POINT ( 'NONE',  ( 188.3964383979925401, 299.2957869059246718, -0.5852346544794374550 ) ) ;
#76306 = CARTESIAN_POINT ( 'NONE',  ( 68.68578350440056113, 68.40580704404837320, 7.012371262790892956 ) ) ;
#76307 = CARTESIAN_POINT ( 'NONE',  ( 162.9294686138450459, 252.2324572554889812, -12.93311691499258309 ) ) ;
#76308 = ORIENTED_EDGE ( 'NONE', *, *, #73193, .F. ) ;
#76309 = CARTESIAN_POINT ( 'NONE',  ( 48.73804053012794668, 107.9864336245683631, -10.00000000000000000 ) ) ;
#76310 = CARTESIAN_POINT ( 'NONE',  ( 189.7838259857693686, 299.9317662682615833, -5.554424272425116271 ) ) ;
#76311 = CARTESIAN_POINT ( 'NONE',  ( 89.94416901687610277, 231.9244531367911009, -4.594050593750046652 ) ) ;
#76312 = CARTESIAN_POINT ( 'NONE',  ( 207.7666684749232786, 270.7845694125510931, -6.630926507062123498 ) ) ;
#76313 = CARTESIAN_POINT ( 'NONE',  ( 151.2455280670316711, 268.6820563007532314, 14.35914944935941229 ) ) ;
#76314 = DIRECTION ( 'NONE',  ( -0.8660254037844384856, -0.5000000000000002220, -3.252519625699449945E-16 ) ) ;
#76316 = CARTESIAN_POINT ( 'NONE',  ( 83.76485939058579788, 42.20955296087365127, -3.876374748171139029 ) ) ;
#76315 = CYLINDRICAL_SURFACE ( 'NONE', #20966, 10.00000000000010658 ) ;
#76317 = CARTESIAN_POINT ( 'NONE',  ( 201.1763559185644112, 270.5295643278437865, -10.00885884882298704 ) ) ;
#76318 = CARTESIAN_POINT ( 'NONE',  ( 184.8303046393444049, 287.3399108598079579, -15.67031930442813348 ) ) ;
#76319 = FACE_OUTER_BOUND ( 'NONE', #36447, .T. ) ;
#76320 = CARTESIAN_POINT ( 'NONE',  ( 44.43411998782967487, 26.44966523072498177, -2.296566073217252530E-15 ) ) ;
#76321 = CARTESIAN_POINT ( 'NONE',  ( 123.7735466722555202, 252.2677522451419065, -5.000000000000047962 ) ) ;
#76322 = FACE_BOUND ( 'NONE', #13104, .T. ) ;
#76323 = ORIENTED_EDGE ( 'NONE', *, *, #77682, .T. ) ;
#76324 = CARTESIAN_POINT ( 'NONE',  ( 22.15746398174156440, 34.83396525600390703, -2.839279412974133887 ) ) ;
#76325 = CARTESIAN_POINT ( 'NONE',  ( 178.9095197733313114, 280.6377396294411710, 15.96141144708081860 ) ) ;
#76326 = CARTESIAN_POINT ( 'NONE',  ( 193.2053309019613891, 296.0055459150826778, -12.79465285318189061 ) ) ;
#76327 = FACE_OUTER_BOUND ( 'NONE', #52661, .T. ) ;
#76328 = VERTEX_POINT ( 'NONE', #14104 ) ;
#76329 = B_SPLINE_SURFACE_WITH_KNOTS ( 'NONE', 3, 1, ( 
 ( #31841, #9065 ),
 ( #39932, #71379 ),
 ( #1968, #63762 ),
 ( #93700, #53645 ),
 ( #24263, #84600 ),
 ( #18673, #80002 ),
 ( #89130, #19682 ),
 ( #56655, #64771 ),
 ( #40934, #94694 ),
 ( #33360, #87640 ),
 ( #41446, #42437 ),
 ( #64260, #81500 ),
 ( #50543, #95211 ),
 ( #18168, #34842 ),
 ( #96201, #49554 ),
 ( #12068, #95720 ),
 ( #10571, #25256 ),
 ( #73372, #25780 ),
 ( #88621, #80507 ),
 ( #49068, #34359 ),
 ( #87137, #56139 ),
 ( #41957, #26763 ),
 ( #57645, #73865 ),
 ( #42925, #35352 ),
 ( #3959, #72386 ),
 ( #17669, #2996 ),
 ( #33886, #26268 ),
 ( #65745, #57144 ),
 ( #88126, #48567 ),
 ( #11081, #10069 ),
 ( #96699, #72892 ),
 ( #3484, #65256 ),
 ( #19189, #79508 ),
 ( #27267, #50060 ) ),
 .UNSPECIFIED., .T., .F., .F.,
 ( 4, 2, 2, 2, 2, 2, 2, 2, 2, 2, 2, 2, 2, 2, 2, 2, 4 ),
 ( 2, 2 ),
 ( 0.000000000000000000, 0.06250000000000000000, 0.1250000000000000000, 0.1875000000000000000, 0.2500000000000000000, 0.3125000000000000000, 0.3750000000000000000, 0.4375000000000000000, 0.5000000000000000000, 0.5625000000000000000, 0.6250000000000000000, 0.6875000000000000000, 0.7500000000000000000, 0.8125000000000000000, 0.8750000000000000000, 0.9375000000000000000, 1.000000000000000000 ),
 ( 0.000000000000000000, 1.000000000000000000 ),
 .UNSPECIFIED. ) ;
#76330 = B_SPLINE_CURVE_WITH_KNOTS ( 'NONE', 3,
 ( #71989, #55251, #64378, #56769, #54756, #85742, #1082, #47163, #87751, #80122, #32966, #10684, #41562, #72506, #63873, #9179, #93307, #8676, #24869, #23864, #16270, #39546, #1597, #70468, #31960, #86233, #16768, #47660, #78594, #32480, #63376 ),
 .UNSPECIFIED., .F., .F.,
 ( 4, 3, 3, 3, 3, 3, 3, 3, 3, 3, 4 ),
 ( 0.000000000000000000, 0.1333490885032340423, 0.3007194338854312643, 0.4699862290245129803, 0.5844252810809342780, 0.6686540514502644639, 0.7354980260655447077, 0.8028463152565625816, 0.8633854507757121599, 0.9437142632667110398, 1.000000000000000000 ),
 .UNSPECIFIED. ) ;
#76331 = CARTESIAN_POINT ( 'NONE',  ( 70.85940962530331433, 60.99147867796299494, 15.04089833736761328 ) ) ;
#76332 = CARTESIAN_POINT ( 'NONE',  ( 75.98901751930753790, 65.25029023645535631, -14.46192986472697584 ) ) ;
#76333 = PLANE ( 'NONE',  #86603 ) ;
#76334 = CARTESIAN_POINT ( 'NONE',  ( 173.2590479799806928, 253.7630292489582757, -9.109924965339219582 ) ) ;
#76335 = CARTESIAN_POINT ( 'NONE',  ( 75.13052455607011382, 52.91100154115419230, -15.99857184472472760 ) ) ;
#76336 = CARTESIAN_POINT ( 'NONE',  ( 152.7618747630824885, 266.0556667813044101, 16.41480086888796919 ) ) ;
#76337 = VERTEX_POINT ( 'NONE', #44986 ) ;
#76338 = CARTESIAN_POINT ( 'NONE',  ( 187.2731080186762256, 278.8154626391448119, 17.13899673958438186 ) ) ;
#76339 = CARTESIAN_POINT ( 'NONE',  ( 33.64972468124413751, 31.37878583063843152, 9.188101187500006262 ) ) ;
#76340 = EDGE_LOOP ( 'NONE', ( #11601, #95724, #44411, #74854 ) ) ;
#76341 = CARTESIAN_POINT ( 'NONE',  ( 167.7069825692313429, 249.7662905202334969, 6.717005362718047934 ) ) ;
#76342 = CARTESIAN_POINT ( 'NONE',  ( 184.5595156642797008, 292.1222730993646906, -10.69555203441723457 ) ) ;
#76343 = EDGE_LOOP ( 'NONE', ( #62106, #41677, #49932, #26259 ) ) ;
#76344 = CARTESIAN_POINT ( 'NONE',  ( -21.31413092498267048, 24.33771760303831755, -10.00000000000000000 ) ) ;
#76345 = DIRECTION ( 'NONE',  ( -0.3402761906661271873, -0.9403255362191060840, 0.000000000000000000 ) ) ;
#76346 = CARTESIAN_POINT ( 'NONE',  ( 193.8837194332558056, 280.6698792847660684, -17.10338268821150720 ) ) ;
#76347 = CARTESIAN_POINT ( 'NONE',  ( 153.9313804520737961, 264.0300235082304425, -16.64903060835773374 ) ) ;
#76348 = CARTESIAN_POINT ( 'NONE',  ( 200.9445292274600092, 282.6008612054670266, -16.62830946367346741 ) ) ;
#76349 = CARTESIAN_POINT ( 'NONE',  ( 169.0898264877448014, 257.6955085404131296, 15.20712983902550341 ) ) ;
#76350 = ADVANCED_FACE ( 'NONE', ( #51605 ), #6508, .T. ) ;
#76351 = CARTESIAN_POINT ( 'NONE',  ( 34.33172647011804202, 40.79752408145594700, -5.678558825948271327 ) ) ;
#76352 = CARTESIAN_POINT ( 'NONE',  ( 81.49529596843051138, 56.10236560196279498, -16.41626961062114631 ) ) ;
#76353 = EDGE_CURVE ( 'NONE', #38635, #90112, #85086, .T. ) ;
#76354 = CARTESIAN_POINT ( 'NONE',  ( 68.68909986782581711, 64.16576715805911135, -12.55144644517788421 ) ) ;
#76355 = VERTEX_POINT ( 'NONE', #55569 ) ;
#76356 = CARTESIAN_POINT ( 'NONE',  ( 176.2398559119413051, 258.8095549018042334, 13.22354805979146697 ) ) ;
#76357 = VERTEX_POINT ( 'NONE', #93629 ) ;
#76358 = VERTEX_POINT ( 'NONE', #63693 ) ;
#76359 = CARTESIAN_POINT ( 'NONE',  ( 198.0258880569907376, 286.7261629195996875, 16.96262172508392041 ) ) ;
#76360 = CARTESIAN_POINT ( 'NONE',  ( 169.4301234034413426, 269.1242964454818889, 17.39485978491103069 ) ) ;
#76362 = FACE_OUTER_BOUND ( 'NONE', #38680, .T. ) ;
#76361 = CARTESIAN_POINT ( 'NONE',  ( 86.18027666378029039, 49.75620593066999220, -22.49999999999982592 ) ) ;
#76363 = CARTESIAN_POINT ( 'NONE',  ( -19.65312891409030271, 93.06504152958497400, 54.99999999999999289 ) ) ;
#76364 = CARTESIAN_POINT ( 'NONE',  ( 201.1914266341661630, 274.9083111069574556, -13.97515993586548610 ) ) ;
#76365 = CARTESIAN_POINT ( 'NONE',  ( 78.21946184288361792, 59.52378438228485180, -16.11278392467423970 ) ) ;
#76366 = CARTESIAN_POINT ( 'NONE',  ( 148.2159754900428936, 273.9293952882992471, 9.267836332806297150 ) ) ;
#76368 = EDGE_CURVE ( 'NONE', #30353, #68986, #47976, .T. ) ;
#76367 = CARTESIAN_POINT ( 'NONE',  ( 167.0874653007571169, 286.5168870136799910, -4.892502125562864457 ) ) ;
#76369 = CARTESIAN_POINT ( 'NONE',  ( 165.8866640751390094, 265.8956478032751534, 17.81115609982314751 ) ) ;
#76370 = CARTESIAN_POINT ( 'NONE',  ( 183.5371895774011364, 284.7566254381118824, -15.01286450311582144 ) ) ;
#76371 = CARTESIAN_POINT ( 'NONE',  ( 102.6097905472235539, 239.2369531367911009, -4.594050593750048428 ) ) ;
#76372 = ORIENTED_EDGE ( 'NONE', *, *, #18772, .T. ) ;
#76373 = CARTESIAN_POINT ( 'NONE',  ( 31.15319227796116053, 18.39040679176984128, -6.890680421881970419E-14 ) ) ;
#76374 = CARTESIAN_POINT ( 'NONE',  ( 45.09207854535236493, 28.96004757982094446, -5.678558825948276656 ) ) ;
#76375 = CARTESIAN_POINT ( 'NONE',  ( 191.4296719636011517, 274.8339350444337583, 16.87517489376925539 ) ) ;
#76376 = ORIENTED_EDGE ( 'NONE', *, *, #14781, .F. ) ;
#76377 = ORIENTED_EDGE ( 'NONE', *, *, #10755, .F. ) ;
#76378 = CARTESIAN_POINT ( 'NONE',  ( 73.92441827737660276, 68.29833774401778612, -11.64939612493447996 ) ) ;
#76379 = CARTESIAN_POINT ( 'NONE',  ( 180.7260405409376745, 294.0588039200300159, -2.607966119977916275 ) ) ;
#76380 = CARTESIAN_POINT ( 'NONE',  ( 192.0670538266147958, 297.9770996426736929, 11.54736252216878256 ) ) ;
#76381 = CARTESIAN_POINT ( 'NONE',  ( 206.7680519836501958, 272.5142239127119979, -10.57935479673322021 ) ) ;
#76382 = CARTESIAN_POINT ( 'NONE',  ( 97.10949284993499475, 215.3262482093457493, 3.021315404115420679E-15 ) ) ;
#76383 = ADVANCED_FACE ( 'NONE', ( #54565 ), #78921, .T. ) ;
#76384 = ORIENTED_EDGE ( 'NONE', *, *, #33054, .T. ) ;
#76385 = CARTESIAN_POINT ( 'NONE',  ( -36.56673362314461428, 37.64405826905806407, 59.99999999999999289 ) ) ;
#76386 = ORIENTED_EDGE ( 'NONE', *, *, #74231, .F. ) ;
#76387 = CARTESIAN_POINT ( 'NONE',  ( -4.653128914090328472, 78.77562236714182120, 59.99999999999999289 ) ) ;
#76388 = ORIENTED_EDGE ( 'NONE', *, *, #87323, .F. ) ;
#76389 = MANIFOLD_SOLID_BREP ( 'Split Line2', #36149 ) ;
#76390 = CARTESIAN_POINT ( 'NONE',  ( 191.8829787380248604, 267.6708518110137334, -12.49840204580878478 ) ) ;
#76391 = CARTESIAN_POINT ( 'NONE',  ( 192.6073437551183645, 263.2194025587710939, 4.509002015703135413 ) ) ;
#76392 = CARTESIAN_POINT ( 'NONE',  ( 15.77038241084232517, 34.14663330942826747, 10.00000000000000000 ) ) ;
#76393 = CARTESIAN_POINT ( 'NONE',  ( 163.1008115941903895, 248.1481028935802442, 11.25332017433677834 ) ) ;
#76395 = CARTESIAN_POINT ( 'NONE',  ( 156.9006073532037817, 280.5407770597218473, 5.988227030271738194 ) ) ;
#76394 = CARTESIAN_POINT ( 'NONE',  ( 187.3716705114872809, 291.0127574213985895, -13.61402146762525334 ) ) ;
#76396 = CIRCLE ( 'NONE', #63434, 17.82106496071138224 ) ;
#76397 = CARTESIAN_POINT ( 'NONE',  ( -22.42236680055709641, 157.8615022471902591, 0.000000000000000000 ) ) ;
#76398 = VERTEX_POINT ( 'NONE', #45970 ) ;
#76399 = CARTESIAN_POINT ( 'NONE',  ( 147.0670278774466908, 275.9194309285509235, 3.666898409139099257 ) ) ;
#76400 = CARTESIAN_POINT ( 'NONE',  ( 72.44101633376520510, 65.82767294218574250, 12.36625408228399259 ) ) ;
#76401 = EDGE_CURVE ( 'NONE', #91080, #61231, #77287, .T. ) ;
#76402 = CARTESIAN_POINT ( 'NONE',  ( 82.41127205671455158, 40.84167155264970006, -3.717692515266792341 ) ) ;
#76403 = CARTESIAN_POINT ( 'NONE',  ( 172.7994643787747293, 251.3630591998880561, -0.2565247822977752556 ) ) ;
#76404 = CARTESIAN_POINT ( 'NONE',  ( 192.5117867804768252, 271.3415924289031409, -15.10878263095346696 ) ) ;
#76405 = DIRECTION ( 'NONE',  ( 0.8575671445351807920, -0.5143720371616018472, 0.000000000000000000 ) ) ;
#76406 = CARTESIAN_POINT ( 'NONE',  ( 82.70173776682830180, 42.57814917962534196, 6.376911687432284204 ) ) ;
#76407 = CARTESIAN_POINT ( 'NONE',  ( 29.73762157799522399, 194.6427522451419065, 10.00000000000009415 ) ) ;
#76408 = ADVANCED_FACE ( 'NONE', ( #61681 ), #36878, .F. ) ;
#76409 = CARTESIAN_POINT ( 'NONE',  ( -75.18208942163933273, 50.44421862632484022, 177.5919119679930134 ) ) ;
#76410 = CARTESIAN_POINT ( 'NONE',  ( 71.65769282842789778, 70.70965056591087716, -6.033769676015556804 ) ) ;
#76411 = CARTESIAN_POINT ( 'NONE',  ( 81.74442484449845381, 211.8768266524159856, 9.188101187500098632 ) ) ;
#76412 = PLANE ( 'NONE',  #34654 ) ;
#76413 = CARTESIAN_POINT ( 'NONE',  ( 147.5749551500760788, 275.0396750858066639, -4.254929048021584670 ) ) ;
#76414 = DIRECTION ( 'NONE',  ( -0.8660254037844387076, -0.4999999999999998890, -0.000000000000000000 ) ) ;
#76415 = CARTESIAN_POINT ( 'NONE',  ( 196.8357460615746675, 288.9375519056556527, -16.76664714252133948 ) ) ;
#76416 = EDGE_CURVE ( 'NONE', #87878, #8862, #43539, .T. ) ;
#76417 = CARTESIAN_POINT ( 'NONE',  ( 207.1019571622349815, 271.9358831784929293, -5.989975140547304733 ) ) ;
#76418 = CARTESIAN_POINT ( 'NONE',  ( 167.5421813246326792, 287.5986610761024167, 3.969292590682533373 ) ) ;
#76420 = CARTESIAN_POINT ( 'NONE',  ( 76.54298794630824432, 51.21710260455724040, 16.04984378097219633 ) ) ;
#76419 = CARTESIAN_POINT ( 'NONE',  ( 100.3908607700756619, 238.7677522451419065, -5.000000000000047962 ) ) ;
#76421 = EDGE_CURVE ( 'NONE', #75268, #57662, #24574, .T. ) ;
#76422 = CARTESIAN_POINT ( 'NONE',  ( 189.2845499996045930, 259.5340837477176024, -0.8149847707460528001 ) ) ;
#76423 = CARTESIAN_POINT ( 'NONE',  ( 44.68504016816519453, 27.92755873383629606, 6.180339887498953466 ) ) ;
#76424 = CARTESIAN_POINT ( 'NONE',  ( 161.3697451762201922, 251.5394009270540607, 13.17726145763740853 ) ) ;
#76425 = CARTESIAN_POINT ( 'NONE',  ( 189.7838259857693686, 299.9317662682615833, -5.554424272425116271 ) ) ;
#76426 = CARTESIAN_POINT ( 'NONE',  ( 72.14611019483686505, 72.30310738408833515, 3.684292749196578232 ) ) ;
#76427 = CARTESIAN_POINT ( 'NONE',  ( 53.21953955946602122, 201.5333772461660544, 9.188101187500095079 ) ) ;
#76428 = CARTESIAN_POINT ( 'NONE',  ( 196.2048238403250764, 290.8102717488927169, 17.53926796892840656 ) ) ;
#76429 = CARTESIAN_POINT ( 'NONE',  ( 199.2752819598239000, 277.9111509360756145, 15.64615381322591681 ) ) ;
#76430 = DIRECTION ( 'NONE',  ( -0.8660254037844387076, -0.4999999999999998890, -0.000000000000000000 ) ) ;
#76431 = CARTESIAN_POINT ( 'NONE',  ( -18.88609640177068627, 173.2365022471903160, 2.944929066748280225E-16 ) ) ;
#76432 = CARTESIAN_POINT ( 'NONE',  ( 50.02589733512838421, 205.8149278399161233, 9.188101187500093303 ) ) ;
#76433 = CARTESIAN_POINT ( 'NONE',  ( 20.70865909420142259, 30.14336893147755703, 7.433330006724141015 ) ) ;
#76434 = CARTESIAN_POINT ( 'NONE',  ( 198.7829547491859330, 286.3448180261817129, -18.59838968157616179 ) ) ;
#76435 = CARTESIAN_POINT ( 'NONE',  ( 196.8363552541316324, 289.7164272536036265, -17.80258609350122967 ) ) ;
#76436 = CARTESIAN_POINT ( 'NONE',  ( 16.06339478488542127, 14.98920272979925272, 7.433330006724137462 ) ) ;
#76437 = CARTESIAN_POINT ( 'NONE',  ( 157.6500260163024620, 257.5891404556457474, -18.23450497588216379 ) ) ;
#76438 = CARTESIAN_POINT ( 'NONE',  ( 77.24238159045749796, 63.47610639771342278, 15.48509222746617553 ) ) ;
#76439 = CARTESIAN_POINT ( 'NONE',  ( 7.225231395932167899, 28.43104314603600358, -10.00000000000000000 ) ) ;
#76440 = CARTESIAN_POINT ( 'NONE',  ( 179.8263126347392813, 276.7214098371354680, 16.33597602842999308 ) ) ;
#76441 = CARTESIAN_POINT ( 'NONE',  ( 72.18153366120698422, 59.81188395286972082, 15.22051537925258202 ) ) ;
#76442 = CARTESIAN_POINT ( 'NONE',  ( 201.3598265928982869, 281.8815450682784558, 17.41054330225266966 ) ) ;
#76443 = CARTESIAN_POINT ( 'NONE',  ( 81.30930031418027681, 54.60213497152520290, -15.79650731256931273 ) ) ;
#76444 = CARTESIAN_POINT ( 'NONE',  ( 107.4814437671086580, 242.8615022471903160, 5.000000000000046185 ) ) ;
#76445 = CARTESIAN_POINT ( 'NONE',  ( 169.2681527202045118, 288.6954499571734800, 3.589104733571486516 ) ) ;
#76446 = CARTESIAN_POINT ( 'NONE',  ( 165.2484375929805935, 269.8046256042021582, -16.27477966519025898 ) ) ;
#76447 = ORIENTED_EDGE ( 'NONE', *, *, #70999, .T. ) ;
#76448 = CARTESIAN_POINT ( 'NONE',  ( 77.52100321733644250, 49.65180640845364479, 14.92792641300140843 ) ) ;
#76449 = ORIENTED_EDGE ( 'NONE', *, *, #62513, .F. ) ;
#76450 = CARTESIAN_POINT ( 'NONE',  ( 166.5018518098672189, 264.8202169054221145, 16.82335354330060539 ) ) ;
#76451 = CARTESIAN_POINT ( 'NONE',  ( 190.3620301733707834, 278.8805567241598169, -16.54082129631397891 ) ) ;
#76452 = LINE ( 'NONE', #21737, #48277 ) ;
#76453 = ORIENTED_EDGE ( 'NONE', *, *, #20347, .F. ) ;
#76454 = CARTESIAN_POINT ( 'NONE',  ( 162.8756881843043516, 250.5380280774768949, 12.81046238701583029 ) ) ;
#76455 = CARTESIAN_POINT ( 'NONE',  ( 79.21048608390624679, 45.84430088201565212, -12.45846168025711798 ) ) ;
#76456 = CARTESIAN_POINT ( 'NONE',  ( 194.4826705584825390, 293.7931287314651740, -16.11258321617245315 ) ) ;
#76457 = CARTESIAN_POINT ( 'NONE',  ( 72.98228618152094782, 70.36901929029048119, -8.113406466234710734 ) ) ;
#76459 = ORIENTED_EDGE ( 'NONE', *, *, #78233, .F. ) ;
#76458 = AXIS2_PLACEMENT_3D ( 'NONE', #92676, #38928, #22748 ) ;
#76460 = CARTESIAN_POINT ( 'NONE',  ( 18.92729281690869314, 22.87878583063841020, -9.188101187500006262 ) ) ;
#76461 = CARTESIAN_POINT ( 'NONE',  ( 67.72713518178136383, 69.49437377556795070, -2.463275011707438900 ) ) ;
#76462 = CYLINDRICAL_SURFACE ( 'NONE', #5225, 10.00000000000010658 ) ;
#76463 = VECTOR ( 'NONE', #83581, 1000.000000000000000 ) ;
#76464 = VERTEX_POINT ( 'NONE', #74965 ) ;
#76465 = CYLINDRICAL_SURFACE ( 'NONE', #15817, 16.60714546451156792 ) ;
#76466 = DIRECTION ( 'NONE',  ( -0.1550826972584531394, -0.9879014915521905360, 0.000000000000000000 ) ) ;
#76467 = ORIENTED_EDGE ( 'NONE', *, *, #39023, .F. ) ;
#76468 = ORIENTED_EDGE ( 'NONE', *, *, #79784, .T. ) ;
#76469 = CARTESIAN_POINT ( 'NONE',  ( 170.8501576794184587, 284.6586050162820243, 10.94124936453461849 ) ) ;
#76471 = CARTESIAN_POINT ( 'NONE',  ( 67.92772920839225037, 65.41715411821847681, -10.39043899096739665 ) ) ;
#76470 = CARTESIAN_POINT ( 'NONE',  ( 163.1241269448184710, 283.6514265758889906, -3.103922426645265187 ) ) ;
#76472 = CARTESIAN_POINT ( 'NONE',  ( 163.1096928939807924, 248.1327200311062882, -9.690381021358412283 ) ) ;
#76473 = CARTESIAN_POINT ( 'NONE',  ( 164.4761815919938215, 245.7658921781788592, 6.833796894895563412 ) ) ;
#76474 = CARTESIAN_POINT ( 'NONE',  ( -72.81784413424504976, 47.52919789448971244, -10.00000000000000000 ) ) ;
#76475 = CARTESIAN_POINT ( 'NONE',  ( 164.6266891068947587, 265.1316493055271053, -16.62685662814512710 ) ) ;
#76478 = EDGE_CURVE ( 'NONE', #77213, #76155, #26365, .T. ) ;
#76477 = CARTESIAN_POINT ( 'NONE',  ( 134.8967340017684080, 242.5643266524160424, -9.188101187500093303 ) ) ;
#76476 = B_SPLINE_CURVE_WITH_KNOTS ( 'NONE', 3,
 ( #83267, #6738, #14822, #21439 ),
 .UNSPECIFIED., .F., .F.,
 ( 4, 4 ),
 ( 0.01319540715386985363, 0.01956822373704288423 ),
 .UNSPECIFIED. ) ;
#76479 = CARTESIAN_POINT ( 'NONE',  ( 203.0230638682947699, 267.9133265956084529, 2.537566450392548134 ) ) ;
#76480 = AXIS2_PLACEMENT_3D ( 'NONE', #78954, #100242, #1438 ) ;
#76481 = CARTESIAN_POINT ( 'NONE',  ( 179.5506826250896211, 257.8340240002441988, 10.21777184434937702 ) ) ;
#76482 = CARTESIAN_POINT ( 'NONE',  ( 72.89481452351749624, 203.7048013555409796, 4.594050593750051981 ) ) ;
#76483 = VERTEX_POINT ( 'NONE', #80602 ) ;
#76484 = CARTESIAN_POINT ( 'NONE',  ( 176.4172214413987660, 252.1966103377273214, 1.934499474311637712 ) ) ;
#76485 = CARTESIAN_POINT ( 'NONE',  ( 72.82159975088246995, 72.59360798638101642, 0.000000000000000000 ) ) ;
#76486 = ORIENTED_EDGE ( 'NONE', *, *, #75142, .T. ) ;
#76487 = CARTESIAN_POINT ( 'NONE',  ( 44.95821123098110661, 116.5722627105190270, -10.00000000000000000 ) ) ;
#76488 = ORIENTED_EDGE ( 'NONE', *, *, #8360, .T. ) ;
#76489 = CARTESIAN_POINT ( 'NONE',  ( 66.92706188925286881, 68.00105104109823628, 6.962559168495445761 ) ) ;
#76490 = CARTESIAN_POINT ( 'NONE',  ( 191.4738032422262677, 260.7793432447242594, -0.2951778641931921410 ) ) ;
#76491 = EDGE_CURVE ( 'NONE', #50515, #96813, #73057, .T. ) ;
#76492 = LINE ( 'NONE', #92231, #33647 ) ;
#76493 = CARTESIAN_POINT ( 'NONE',  ( 80.96506752577832344, 55.91141337780396725, 16.08528190432093297 ) ) ;
#76494 = CARTESIAN_POINT ( 'NONE',  ( 194.5047661587782386, 293.7548580291293092, 14.86680123054176583 ) ) ;
#76495 = LINE ( 'NONE', #38462, #20483 ) ;
#76496 = EDGE_CURVE ( 'NONE', #75612, #52858, #47891, .T. ) ;
#76497 = ORIENTED_EDGE ( 'NONE', *, *, #69952, .F. ) ;
#76498 = CARTESIAN_POINT ( 'NONE',  ( 200.9621566682951652, 282.5703295823330450, -16.90446154037251958 ) ) ;
#76499 = VERTEX_POINT ( 'NONE', #7534 ) ;
#76500 = CARTESIAN_POINT ( 'NONE',  ( 73.00396795756827828, 57.62093675928252878, -16.32480838619500219 ) ) ;
#76501 = CARTESIAN_POINT ( 'NONE',  ( 76.04450315243209957, 65.42723423563565177, -13.97889933544638019 ) ) ;
#76502 = CARTESIAN_POINT ( 'NONE',  ( 149.1429535397850827, 272.3238222086447990, -12.91457852089092384 ) ) ;
#76503 = CARTESIAN_POINT ( 'NONE',  ( 194.9743901658331424, 279.5313095752043751, 16.57687009077668350 ) ) ;
#76504 = CARTESIAN_POINT ( 'NONE',  ( 161.8358879837834365, 261.0030460270972412, 16.78525318079316264 ) ) ;
#76505 = CARTESIAN_POINT ( 'NONE',  ( 140.4172988551291610, 258.0024278399160949, -9.188101187500093303 ) ) ;
#76506 = ORIENTED_EDGE ( 'NONE', *, *, #87123, .F. ) ;
#76507 = CARTESIAN_POINT ( 'NONE',  ( 87.93413682123004094, 44.35120838780621000, 4.768703809423660012 ) ) ;
#76508 = CARTESIAN_POINT ( 'NONE',  ( 42.35759689194659927, 26.58380873178790793, 6.180339887498953466 ) ) ;
#76509 = CARTESIAN_POINT ( 'NONE',  ( -110.0000000000000000, 4.999999999999999112, 14.21260523776215301 ) ) ;
#76510 = CARTESIAN_POINT ( 'NONE',  ( 153.3939648708017387, 264.9608545997728015, -16.49556533540763681 ) ) ;
#76511 = CARTESIAN_POINT ( 'NONE',  ( 72.77087662098560372, 70.82427377826435588, 7.173618689453861386 ) ) ;
#76512 = CARTESIAN_POINT ( 'NONE',  ( 71.00707024578083804, 67.28932756229654899, -10.38437885875134192 ) ) ;
#76513 = ORIENTED_EDGE ( 'NONE', *, *, #89036, .F. ) ;
#76514 = CARTESIAN_POINT ( 'NONE',  ( 199.7315608606883757, 266.8161529887717620, 4.634410026811882410 ) ) ;
#76515 =( BOUNDED_CURVE ( )  B_SPLINE_CURVE ( 2, ( #62787, #31881, #47587, #32397, #9620, #33398, #94730, #23789, #85658 ),
 .UNSPECIFIED., .F., .T. ) 
 B_SPLINE_CURVE_WITH_KNOTS ( ( 3, 2, 2, 2, 3 ),
 ( 0.7379032258064516236, 0.7392473118279569988, 0.7419354838709677491, 0.7446236559139784994, 0.7459677419354838745 ),
 .UNSPECIFIED. ) 
 CURVE ( )  GEOMETRIC_REPRESENTATION_ITEM ( )  RATIONAL_B_SPLINE_CURVE ( ( 0.9330127018922194093, 0.9330127018922194093, 1.000000000000000000, 0.8660254037844387076, 1.000000000000000000, 0.8660254037844387076, 1.000000000000000000, 0.9330127018922194093, 0.9330127018922194093 ) ) 
 REPRESENTATION_ITEM ( '' )  );
#76516 = EDGE_CURVE ( 'NONE', #8092, #22139, #52626, .T. ) ;
#76517 = CARTESIAN_POINT ( 'NONE',  ( 93.96857342517718337, -8.000000000000000000, -14.21260523776213347 ) ) ;
#76518 = CARTESIAN_POINT ( 'NONE',  ( 25.20903040758703284, 185.3615022471902591, -10.00000000000009592 ) ) ;
#76519 = CARTESIAN_POINT ( 'NONE',  ( 184.6202127605081387, 263.5949843424817800, -12.39504086723364651 ) ) ;
#76520 = CARTESIAN_POINT ( 'NONE',  ( 83.37362496471422446, 52.41223193542727898, 14.84798797970331563 ) ) ;
#76521 = EDGE_CURVE ( 'NONE', #30181, #87380, #45212, .T. ) ;
#76522 = ORIENTED_EDGE ( 'NONE', *, *, #36288, .T. ) ;
#76523 = CARTESIAN_POINT ( 'NONE',  ( 146.9376205018946848, 276.1435710778808925, 5.066564108429441937 ) ) ;
#76524 = EDGE_CURVE ( 'NONE', #79765, #3024, #14647, .T. ) ;
#76525 = CARTESIAN_POINT ( 'NONE',  ( 71.84797400569436832, 72.18106025956552685, -0.5846029390931422043 ) ) ;
#76526 = EDGE_CURVE ( 'NONE', #11680, #37254, #97126, .T. ) ;
#76527 = CARTESIAN_POINT ( 'NONE',  ( 207.3062152119541679, 271.5820978585240368, 7.879821064966149535 ) ) ;
#76529 = FACE_BOUND ( 'NONE', #8696, .T. ) ;
#76528 = CARTESIAN_POINT ( 'NONE',  ( 193.9204722154232741, 294.7668848255750049, 15.43855698596013859 ) ) ;
#76530 = ADVANCED_FACE ( 'NONE', ( #56998 ), #25102, .T. ) ;
#76531 = AXIS2_PLACEMENT_3D ( 'NONE', #86826, #63957, #79213 ) ;
#76532 = EDGE_CURVE ( 'NONE', #66560, #19653, #91190, .T. ) ;
#76533 = CARTESIAN_POINT ( 'NONE',  ( 26.98754258172029452, 23.78052372038640883, -10.00000000000000355 ) ) ;
#76534 = CARTESIAN_POINT ( 'NONE',  ( 80.56202954020663753, 57.53823600680942718, 16.23110421993949259 ) ) ;
#76535 = DIRECTION ( 'NONE',  ( 0.8599083858334038988, -0.5104483989331241034, 0.000000000000000000 ) ) ;
#76536 = CARTESIAN_POINT ( 'NONE',  ( 159.4285914931787431, 254.5085746851079023, 15.41072477910873673 ) ) ;
#76537 = CARTESIAN_POINT ( 'NONE',  ( 144.5581563630820767, 254.2677522451418781, 10.00000000000009592 ) ) ;
#76538 = CARTESIAN_POINT ( 'NONE',  ( 13.18854085237251539, 31.24736827225017777, 10.00000000000000000 ) ) ;
#76539 = ORIENTED_EDGE ( 'NONE', *, *, #46245, .T. ) ;
#76540 = CARTESIAN_POINT ( 'NONE',  ( 66.56294892191600354, 68.00698982583806185, -6.541986041792972273 ) ) ;
#76541 = CARTESIAN_POINT ( 'NONE',  ( 72.74024025722110309, 70.77703717069300637, -7.960999691682589585 ) ) ;
#76542 = CYLINDRICAL_SURFACE ( 'NONE', #53338, 17.82106496071139645 ) ;
#76543 = CARTESIAN_POINT ( 'NONE',  ( 7.590652549690900308, 181.3149278399160949, -9.188101187500095079 ) ) ;
#76544 = CARTESIAN_POINT ( 'NONE',  ( 28.50119043139558883, 18.58380873178787951, 6.180339887498953466 ) ) ;
#76545 = CARTESIAN_POINT ( 'NONE',  ( 77.12554246003209357, 53.45558293378064718, 16.40013681541701018 ) ) ;
#76546 = CARTESIAN_POINT ( 'NONE',  ( 170.7648842107952589, 271.0558799679138247, -16.70271480118435647 ) ) ;
#76547 = CARTESIAN_POINT ( 'NONE',  ( 177.8222571804544430, 286.5223583772871621, 13.77940225188420875 ) ) ;
#76548 = B_SPLINE_SURFACE_WITH_KNOTS ( 'NONE', 3, 1, ( 
 ( #50780, #13310 ),
 ( #4702, #35592 ),
 ( #91316, #75105 ),
 ( #81730, #67479 ),
 ( #58861, #12307 ),
 ( #21390, #28999 ),
 ( #83217, #44660 ),
 ( #28479, #6181 ),
 ( #12817, #37078 ),
 ( #20406, #67982 ),
 ( #21876, #43167 ),
 ( #36076, #66487 ),
 ( #43679, #74621 ),
 ( #66977, #97904 ),
 ( #59360, #16271 ),
 ( #69963, #93821 ),
 ( #84229, #47164 ),
 ( #7167, #22871 ),
 ( #53756, #15255 ),
 ( #38054, #68967 ),
 ( #84715, #70995 ),
 ( #24380, #31961 ),
 ( #69472, #77069 ),
 ( #55252, #30475 ),
 ( #91817, #86234 ),
 ( #86, #45658 ),
 ( #46152, #22377 ),
 ( #78088, #8182 ),
 ( #8677, #99890 ),
 ( #9180, #7677 ),
 ( #93308, #39547 ) ),
 .UNSPECIFIED., .F., .F., .F.,
 ( 4, 3, 3, 3, 3, 3, 3, 3, 3, 3, 4 ),
 ( 2, 2 ),
 ( 0.000000000000000000, 0.1333490885032399820, 0.3007194338854488058, 0.4699862290245400698, 0.5844252810809538179, 0.6686540514502882226, 0.7354980260655652469, 0.8028463152565959993, 0.8633854507757408037, 0.9437142632667595565, 1.000000000000000000 ),
 ( 0.000000000000000000, 1.000000000000000000 ),
 .UNSPECIFIED. ) ;
#76549 = CARTESIAN_POINT ( 'NONE',  ( 175.6999050983589541, 253.1551923919900844, -3.327328156188026131 ) ) ;
#76550 = DIRECTION ( 'NONE',  ( -0.2938926261462390666, 0.5090369604551334692, 0.8090169943749425663 ) ) ;
#76551 = CARTESIAN_POINT ( 'NONE',  ( 53.86003751612216917, 215.2365022471903444, 2.944929066748280225E-16 ) ) ;
#76552 = CARTESIAN_POINT ( 'NONE',  ( 81.83268240801082527, 41.27904705060213075, 5.916546515311264187 ) ) ;
#76553 = CARTESIAN_POINT ( 'NONE',  ( 190.3691966041315311, 300.9178746160123410, 0.1783449565851275009 ) ) ;
#76554 = CARTESIAN_POINT ( 'NONE',  ( 19.39059577201889084, 175.8768266524160140, 9.188101187500098632 ) ) ;
#76555 = DIRECTION ( 'NONE',  ( 0.000000000000000000, -0.000000000000000000, -1.000000000000000000 ) ) ;
#76556 = EDGE_CURVE ( 'NONE', #24006, #8092, #26121, .T. ) ;
#76557 = CARTESIAN_POINT ( 'NONE',  ( 45.41683807177152232, 29.14754757982093736, -5.678558825948276656 ) ) ;
#76558 = CARTESIAN_POINT ( 'NONE',  ( 164.2672861321391053, 246.1277097281173667, -2.417001679502223777 ) ) ;
#76559 = CARTESIAN_POINT ( 'NONE',  ( 189.0332475110736823, 268.2270510816296110, 13.69286421477849380 ) ) ;
#76560 = CARTESIAN_POINT ( 'NONE',  ( 160.1420032418522794, 278.6903965922204520, -9.786847659039947800 ) ) ;
#76561 = CARTESIAN_POINT ( 'NONE',  ( 179.7070423342790662, 263.0192850531631734, -13.12411453645908743 ) ) ;
#76562 = APPLICATION_PROTOCOL_DEFINITION ( 'draft international standard', 'automotive_design', 1998, #31646 ) ;
#76563 = CARTESIAN_POINT ( 'NONE',  ( 26.13094010387951371, 20.80170272979927049, 7.433330006724137462 ) ) ;
#76564 = CARTESIAN_POINT ( 'NONE',  ( 190.6036479972031259, 300.5117928913073797, -0.6824572005520307405 ) ) ;
#76565 = CARTESIAN_POINT ( 'NONE',  ( 71.62614020371384527, 59.05562564738432485, 15.34271347411686115 ) ) ;
#76566 = CARTESIAN_POINT ( 'NONE',  ( 194.4904290197884507, 293.7796906822950973, 14.50206953321744940 ) ) ;
#76567 = EDGE_LOOP ( 'NONE', ( #13680, #89519, #38303, #96837, #21996, #84461 ) ) ;
#76568 = CARTESIAN_POINT ( 'NONE',  ( 181.6021537782941948, 289.2296556448770843, 12.56736601662415787 ) ) ;
#76569 = CARTESIAN_POINT ( 'NONE',  ( 86.51254904731311512, 45.35660278255235056, -8.424040530456800013 ) ) ;
#76570 = DIRECTION ( 'NONE',  ( 0.5000000000000013323, -0.8660254037844378194, 0.000000000000000000 ) ) ;
#76571 = CARTESIAN_POINT ( 'NONE',  ( 81.49684083197098516, 42.49698986986711446, 7.471786974450515650 ) ) ;
#76572 = DIRECTION ( 'NONE',  ( -0.8503781557569336513, 0.05328141121994486862, 0.5234673661555679924 ) ) ;
#76573 = EDGE_LOOP ( 'NONE', ( #37365, #20317, #60133, #25030 ) ) ;
#76574 = CARTESIAN_POINT ( 'NONE',  ( 153.8480465357228013, 265.0660884932569843, -16.61306390558784685 ) ) ;
#76575 = CARTESIAN_POINT ( 'NONE',  ( 70.21041392557471283, 70.96369918409062905, -2.494471698684542105 ) ) ;
#76576 = CARTESIAN_POINT ( 'NONE',  ( 76.73487078864175714, 63.86935209113470080, 14.87109117981107076 ) ) ;
#76577 = CARTESIAN_POINT ( 'NONE',  ( 181.1649504240936324, 257.3422611971239462, -7.689218329250792294 ) ) ;
#76578 = ORIENTED_EDGE ( 'NONE', *, *, #64377, .F. ) ;
#76579 = DIRECTION ( 'NONE',  ( -0.5000000000000008882, 0.8660254037844381525, 0.000000000000000000 ) ) ;
#76580 = ORIENTED_EDGE ( 'NONE', *, *, #90388, .T. ) ;
#76581 = CARTESIAN_POINT ( 'NONE',  ( 153.0444155045374544, 265.5662918618958201, -16.15173036748435109 ) ) ;
#76582 = CARTESIAN_POINT ( 'NONE',  ( 72.11639660595672296, 70.09681734935580266, 8.459716556816276878 ) ) ;
#76583 = DIRECTION ( 'NONE',  ( 1.000000000000000000, 0.000000000000000000, 0.000000000000000000 ) ) ;
#76584 = FACE_OUTER_BOUND ( 'NONE', #59623, .T. ) ;
#76585 = ORIENTED_EDGE ( 'NONE', *, *, #74601, .T. ) ;
#76586 = CARTESIAN_POINT ( 'NONE',  ( 148.3519871123208986, 273.6938162480936398, 8.180046468253793890 ) ) ;
#76587 = EDGE_CURVE ( 'NONE', #82896, #74751, #98163, .T. ) ;
#76588 = ORIENTED_EDGE ( 'NONE', *, *, #88569, .T. ) ;
#76589 = CARTESIAN_POINT ( 'NONE',  ( 157.0957870390718369, 258.5491105237443321, 17.69218919045495397 ) ) ;
#76590 = CARTESIAN_POINT ( 'NONE',  ( 158.0904712413047548, 265.1349370488131854, 17.45369701028249310 ) ) ;
#76591 = VERTEX_POINT ( 'NONE', #83337 ) ;
#76592 = CARTESIAN_POINT ( 'NONE',  ( 190.2389970918280540, 301.1433867864428748, 4.601241515604689525 ) ) ;
#76593 = CARTESIAN_POINT ( 'NONE',  ( -58.10760318826260118, 36.06970723555269842, -10.00000000000000000 ) ) ;
#76594 = ORIENTED_EDGE ( 'NONE', *, *, #69077, .F. ) ;
#76595 = EDGE_CURVE ( 'NONE', #35211, #16493, #12422, .T. ) ;
#76596 = CARTESIAN_POINT ( 'NONE',  ( -6.015783505528726316, 74.68510901943744784, 14.77481591981949016 ) ) ;
#76597 = CARTESIAN_POINT ( 'NONE',  ( 159.5300091911712741, 255.0427242571105637, 15.76637448721640666 ) ) ;
#76598 = CARTESIAN_POINT ( 'NONE',  ( 48.74043828842092552, 100.0309547576005258, 10.00000000000000000 ) ) ;
#76599 = CARTESIAN_POINT ( 'NONE',  ( 36.11248442148217919, 32.80066082961424456, 10.00000000000000533 ) ) ;
#76600 = ORIENTED_EDGE ( 'NONE', *, *, #94219, .F. ) ;
#76601 = EDGE_CURVE ( 'NONE', #64000, #62590, #11141, .T. ) ;
#76602 = ORIENTED_EDGE ( 'NONE', *, *, #23058, .F. ) ;
#76603 = CARTESIAN_POINT ( 'NONE',  ( 73.08787508166213343, 59.01509672055304634, -15.57900745017619393 ) ) ;
#76604 = CARTESIAN_POINT ( 'NONE',  ( 190.1813752874636805, 301.2431906792259042, -4.710625539811892359 ) ) ;
#76605 = CARTESIAN_POINT ( 'NONE',  ( 82.29734961797252879, 53.60383310410945512, 15.81226994477779790 ) ) ;
#76606 = CARTESIAN_POINT ( 'NONE',  ( 190.3572031550745294, 300.9386478791372497, 3.093832330100951378 ) ) ;
#76607 = DIRECTION ( 'NONE',  ( 1.000000000000000000, -4.369520618346150875E-13, 0.000000000000000000 ) ) ;
#76608 = CARTESIAN_POINT ( 'NONE',  ( 191.2740899065998121, 299.3505534407085520, 8.349120108963653308 ) ) ;
#76609 = CARTESIAN_POINT ( 'NONE',  ( 191.7187529716733820, 298.5803744197520473, -8.487597704798396592 ) ) ;
#76610 = VECTOR ( 'NONE', #83220, 1000.000000000000000 ) ;
#76611 = CARTESIAN_POINT ( 'NONE',  ( -22.42236680055716036, 157.8615022471903444, 5.188172501216621122E-14 ) ) ;
#76612 = FACE_OUTER_BOUND ( 'NONE', #96445, .T. ) ;
#76614 = DIRECTION ( 'NONE',  ( -0.8660254037844387076, -0.4999999999999998890, -0.000000000000000000 ) ) ;
#76613 = CARTESIAN_POINT ( 'NONE',  ( 196.9098758191317700, 289.5890858996224324, -16.54412079817003800 ) ) ;
#76615 = CARTESIAN_POINT ( 'NONE',  ( 66.98597148399355206, 67.06197240495457379, 8.554490737669659950 ) ) ;
#76616 = CARTESIAN_POINT ( 'NONE',  ( 168.3793444054225290, 286.3781285656735349, 4.059011274220171828 ) ) ;
#76617 = CARTESIAN_POINT ( 'NONE',  ( 78.22548900086377444, 47.74579297413086465, 13.94123525276128994 ) ) ;
#76618 = CARTESIAN_POINT ( 'NONE',  ( 108.5372593219620683, 221.2202760586659167, -5.415160957724236172E-17 ) ) ;
#76619 = EDGE_LOOP ( 'NONE', ( #79140, #95463, #82881, #64999, #65265 ) ) ;
#76620 = CARTESIAN_POINT ( 'NONE',  ( 190.8137524654443666, 300.1478812774159906, -3.757822530009682804 ) ) ;
#76621 = CARTESIAN_POINT ( 'NONE',  ( 71.22012620979680264, 67.74042170150684683, 10.05071617227448044 ) ) ;
#76622 = CARTESIAN_POINT ( 'NONE',  ( 148.8152594325094640, 273.8656759551610094, 8.901672353312864772 ) ) ;
#76623 = CARTESIAN_POINT ( 'NONE',  ( 79.14837792229336344, 45.86247416287834966, 13.10094053291496508 ) ) ;
#76624 = CARTESIAN_POINT ( 'NONE',  ( 179.6503533887556046, 282.9570081633805785, -15.82271799553900848 ) ) ;
#76625 = LINE ( 'NONE', #21431, #1380 ) ;
#76626 = CARTESIAN_POINT ( 'NONE',  ( 169.1676646093989973, 285.0513320500780878, -7.948105669459880396 ) ) ;
#76627 = ORIENTED_EDGE ( 'NONE', *, *, #26577, .T. ) ;
#76628 = CARTESIAN_POINT ( 'NONE',  ( 41.47569090598247499, 209.1868197944957899, 18.47570218321542868 ) ) ;
#76629 = CARTESIAN_POINT ( 'NONE',  ( 206.7923762329701276, 272.4720930770340033, -9.496103119940368487 ) ) ;
#76630 = ADVANCED_FACE ( 'NONE', ( #67096 ), #4824, .T. ) ;
#76631 = CARTESIAN_POINT ( 'NONE',  ( 72.21801880702699350, 71.73430858976985292, 5.514776891874405784 ) ) ;
#76632 = CARTESIAN_POINT ( 'NONE',  ( 53.19247626382384908, 191.5177522451418213, 5.000000000000051514 ) ) ;
#76633 = CARTESIAN_POINT ( 'NONE',  ( 113.0020953926368037, 245.2369531367911009, -4.594050593750048428 ) ) ;
#76634 = CARTESIAN_POINT ( 'NONE',  ( 151.4188942279983223, 268.3817773016460251, -14.77302265413830895 ) ) ;
#76635 = CARTESIAN_POINT ( 'NONE',  ( 66.70421483277053198, 67.41215751505673381, -6.693045608280014491 ) ) ;
#76636 = CARTESIAN_POINT ( 'NONE',  ( 157.5710319558766344, 257.7259621817996162, 18.28704422422941533 ) ) ;
#76637 = CARTESIAN_POINT ( 'NONE',  ( 175.8738807006601235, 252.8402638148968720, -4.840734339853246304 ) ) ;
#76638 = CARTESIAN_POINT ( 'NONE',  ( 38.06444208900335013, 180.5327760586659451, 1.948934522072303157E-15 ) ) ;
#76639 = CARTESIAN_POINT ( 'NONE',  ( 82.14960936660257573, 40.66333750097311395, 3.614425481505477489 ) ) ;
#76640 = ORIENTED_EDGE ( 'NONE', *, *, #42382, .F. ) ;
#76641 = CARTESIAN_POINT ( 'NONE',  ( 9.795534599056948011, 164.9155109091896350, 2.679491924311254714 ) ) ;
#76642 = CARTESIAN_POINT ( 'NONE',  ( 177.9052955790886870, 265.4696414361982306, 15.73918422437849074 ) ) ;
#76643 = EDGE_CURVE ( 'NONE', #68532, #50939, #43288, .T. ) ;
#76644 = LINE ( 'NONE', #92868, #2914 ) ;
#76645 = CARTESIAN_POINT ( 'NONE',  ( 190.6218339396177441, 300.4802939150614520, -4.178005820806754755 ) ) ;
#76646 = CARTESIAN_POINT ( 'NONE',  ( 97.22339252480620075, 238.4860189848785410, -2.679491924311252493 ) ) ;
#76647 = CARTESIAN_POINT ( 'NONE',  ( 188.2735287570237688, 299.1710073388255751, -5.251721556916531419 ) ) ;
#76648 = CARTESIAN_POINT ( 'NONE',  ( 166.1961671434869174, 251.1444224861350563, 10.22506114935430155 ) ) ;
#76649 = CARTESIAN_POINT ( 'NONE',  ( 104.2879750871056928, 231.0177522451418781, -10.00000000000009592 ) ) ;
#76650 = CARTESIAN_POINT ( 'NONE',  ( 9.837252142675989575, 71.98620320469845524, 1.836970198720989751E-15 ) ) ;
#76651 = VERTEX_POINT ( 'NONE', #90459 ) ;
#76652 = CARTESIAN_POINT ( 'NONE',  ( 163.0683798854284703, 248.2042762609320903, 11.26611642476872710 ) ) ;
#76653 = CARTESIAN_POINT ( 'NONE',  ( 83.52484103943936589, 46.90027433733275330, -11.98971445564651717 ) ) ;
#76654 = ADVANCED_FACE ( 'NONE', ( #6302 ), #5314, .F. ) ;
#76655 = CARTESIAN_POINT ( 'NONE',  ( 14.51920287573142510, 173.0643266524160140, 9.188101187500095079 ) ) ;
#76656 = CARTESIAN_POINT ( 'NONE',  ( 10.99774771173347432, 18.30066082961419838, -10.00000000000000533 ) ) ;
#76657 = CARTESIAN_POINT ( 'NONE',  ( 192.3965733967720269, 272.0314340560001938, 14.18959370928753572 ) ) ;
#76658 = CARTESIAN_POINT ( 'NONE',  ( 71.72487096640281834, 58.74680701327284993, -15.44539912601161546 ) ) ;
#76659 = CARTESIAN_POINT ( 'NONE',  ( 49.07419501245632176, 91.40403951869188859, 10.00000000000000000 ) ) ;
#76661 = CARTESIAN_POINT ( 'NONE',  ( 56.60219097117523290, 212.6744531367911293, 4.594050593750047540 ) ) ;
#76660 = CARTESIAN_POINT ( 'NONE',  ( 174.6894609039457009, 286.3781494789058115, 10.38366818161665606 ) ) ;
#76662 = CARTESIAN_POINT ( 'NONE',  ( 200.5621507313343557, 283.2631601884785368, 16.81037192529623425 ) ) ;
#76663 = CARTESIAN_POINT ( 'NONE',  ( 72.97677987389820942, 57.10916639992058208, 16.39923404589487177 ) ) ;
#76664 = CARTESIAN_POINT ( 'NONE',  ( 69.39148564807371145, 65.38147651185532538, 11.91492136379578426 ) ) ;
#76665 = CARTESIAN_POINT ( 'NONE',  ( 66.73167312141883656, 68.39993800570366034, -4.394447365586645837 ) ) ;
#76666 = VERTEX_POINT ( 'NONE', #44290 ) ;
#76667 = AXIS2_PLACEMENT_3D ( 'NONE', #14772, #68466, #99394 ) ;
#76668 = CARTESIAN_POINT ( 'NONE',  ( 165.1220678389894090, 269.0795942023863745, 16.79297129081651363 ) ) ;
#76669 = CARTESIAN_POINT ( 'NONE',  ( 11.42479273068475010, 170.7365022471902023, 10.00000000000009592 ) ) ;
#76670 = B_SPLINE_CURVE_WITH_KNOTS ( 'NONE', 3,
 ( #43095, #33023, #44591, #75037, #43609, #13716, #29906, #82674, #82170, #5614, #6618, #36506, #51731, #37492, #45106, #59800, #12745, #75526, #14214, #36005, #98334, #97349, #14707, #6111 ),
 .UNSPECIFIED., .F., .F.,
 ( 4, 2, 2, 2, 2, 2, 2, 2, 2, 2, 2, 4 ),
 ( 0.000000000000000000, 0.1250000000000001110, 0.2500000000000002220, 0.3750000000000003331, 0.4375000000000003886, 0.5000000000000004441, 0.5625000000000004441, 0.6250000000000005551, 0.6875000000000006661, 0.7500000000000006661, 0.8750000000000003331, 1.000000000000000000 ),
 .UNSPECIFIED. ) ;
#76671 = CARTESIAN_POINT ( 'NONE',  ( 164.3890147726454813, 245.9168695380243435, -6.010262808998044548 ) ) ;
#76672 = CARTESIAN_POINT ( 'NONE',  ( 140.2550926398021147, 251.7833772461660544, -9.188101187500095079 ) ) ;
#76673 = CARTESIAN_POINT ( 'NONE',  ( 26.34264212020660167, 36.18502408145594273, 5.678558825948277544 ) ) ;
#76674 = CARTESIAN_POINT ( 'NONE',  ( 165.9273809406606688, 261.6126396426859628, -16.19544363369431750 ) ) ;
#76675 = CARTESIAN_POINT ( 'NONE',  ( 93.96857342517718337, 10.00000000000001243, 14.21260523776213347 ) ) ;
#76676 = CARTESIAN_POINT ( 'NONE',  ( 75.36487073175837281, 53.53173320265494084, -16.04382577248123809 ) ) ;
#76677 = AXIS2_PLACEMENT_3D ( 'NONE', #8800, #62473, #87871 ) ;
#76679 = LINE ( 'NONE', #6779, #8546 ) ;
#76678 = LINE ( 'NONE', #84810, #100213 ) ;
#76680 = CARTESIAN_POINT ( 'NONE',  ( 68.65765088900910484, 64.10725282940799730, 11.94679850282813938 ) ) ;
#76681 = VERTEX_POINT ( 'NONE', #43291 ) ;
#76682 = CARTESIAN_POINT ( 'NONE',  ( 190.9501423151522772, 299.9116471280854626, 8.746938802470586083 ) ) ;
#76683 = DIRECTION ( 'NONE',  ( 1.000000000000000000, -6.145877457746401150E-15, 0.000000000000000000 ) ) ;
#76684 = CARTESIAN_POINT ( 'NONE',  ( 196.6597737787374456, 289.2349992526956726, 16.68652926890371546 ) ) ;
#76685 = CARTESIAN_POINT ( 'NONE',  ( 11.38685760444945672, 12.28920272979924988, -7.433330006724141015 ) ) ;
#76686 = ORIENTED_EDGE ( 'NONE', *, *, #82448, .F. ) ;
#76687 = CARTESIAN_POINT ( 'NONE',  ( 206.9158469655446879, 272.2582354949668684, 9.541657424068484161 ) ) ;
#76688 = DIRECTION ( 'NONE',  ( -0.1172721027424030449, -0.9930998207221544138, 0.000000000000000000 ) ) ;
#76689 = CYLINDRICAL_SURFACE ( 'NONE', #23059, 10.00000000000010658 ) ;
#76690 = CARTESIAN_POINT ( 'NONE',  ( -22.42236680055709641, 157.8615022471902591, 0.000000000000000000 ) ) ;
#76691 = CARTESIAN_POINT ( 'NONE',  ( 44.35815684012577265, 67.96982248125696913, -10.00000000000000000 ) ) ;
#76692 = CARTESIAN_POINT ( 'NONE',  ( 67.63503648096795473, 68.85725524262423392, 4.671258359888055267 ) ) ;
#76693 = CARTESIAN_POINT ( 'NONE',  ( 152.6621968174709991, 266.2283140474973493, -17.02835521334403168 ) ) ;
#76694 = LINE ( 'NONE', #7287, #90781 ) ;
#76695 = CARTESIAN_POINT ( 'NONE',  ( 173.8805019302338621, 250.6242863632701585, 0.4030408839048176262 ) ) ;
#76696 = ORIENTED_EDGE ( 'NONE', *, *, #20552, .T. ) ;
#76697 = CARTESIAN_POINT ( 'NONE',  ( 190.0445576990143195, 301.4801656937889902, 4.140328216824785912 ) ) ;
#76698 = CARTESIAN_POINT ( 'NONE',  ( 70.80888052646473341, 69.64703403501997059, 8.011688916067704724 ) ) ;
#76699 = CARTESIAN_POINT ( 'NONE',  ( 84.26010284367181669, 45.15451964197480095, -9.139984135955533162 ) ) ;
#76700 = EDGE_LOOP ( 'NONE', ( #85862, #2798, #97518, #58557 ) ) ;
#76701 = CARTESIAN_POINT ( 'NONE',  ( 191.0478321355427624, 299.7424433957868928, -9.006798842970001218 ) ) ;
#76702 = CARTESIAN_POINT ( 'NONE',  ( 174.8906308118707216, 255.9997517440984893, -11.44291824309870975 ) ) ;
#76703 = B_SPLINE_CURVE_WITH_KNOTS ( 'NONE', 3,
 ( #4491, #35384, #37862, #91125 ),
 .UNSPECIFIED., .F., .F.,
 ( 4, 4 ),
 ( 0.01152314744103701688, 0.01766322936049247866 ),
 .UNSPECIFIED. ) ;
#76704 = CARTESIAN_POINT ( 'NONE',  ( 196.8363552541316324, 289.7164272536036265, -17.80258609350122967 ) ) ;
#76705 = CARTESIAN_POINT ( 'NONE',  ( 69.75493487105953250, 62.68956563894904832, 13.91594397096109503 ) ) ;
#76706 = VERTEX_POINT ( 'NONE', #27627 ) ;
#76707 = CARTESIAN_POINT ( 'NONE',  ( 111.1353355333153843, 222.7202760586659167, -5.415160957724236172E-17 ) ) ;
#76708 = DIRECTION ( 'NONE',  ( 0.000000000000000000, 0.000000000000000000, 1.000000000000000000 ) ) ;
#76709 = CARTESIAN_POINT ( 'NONE',  ( 181.1618576654650212, 271.6441367243567697, -16.30549846865705277 ) ) ;
#76710 = CARTESIAN_POINT ( 'NONE',  ( 132.0007880082076781, 257.0177522451418781, 5.000000000000046185 ) ) ;
#76711 = VERTEX_POINT ( 'NONE', #97056 ) ;
#76712 = VERTEX_POINT ( 'NONE', #89466 ) ;
#76713 = EDGE_CURVE ( 'NONE', #85978, #20151, #53448, .T. ) ;
#76714 = ORIENTED_EDGE ( 'NONE', *, *, #77280, .F. ) ;
#76715 = CARTESIAN_POINT ( 'NONE',  ( 81.33756375948632922, 49.74101304335109575, 14.11251714982108574 ) ) ;
#76716 = ORIENTED_EDGE ( 'NONE', *, *, #85842, .T. ) ;
#76717 = EDGE_CURVE ( 'NONE', #15906, #6168, #61113, .T. ) ;
#76718 = CARTESIAN_POINT ( 'NONE',  ( 68.03534369547149652, 68.16390280863178930, 6.778061388490955075 ) ) ;
#76719 = ORIENTED_EDGE ( 'NONE', *, *, #58580, .F. ) ;
#76720 = CARTESIAN_POINT ( 'NONE',  ( 208.0287371622045782, 270.3306531311065442, 3.558879245883286746 ) ) ;
#76721 = LINE ( 'NONE', #44316, #12605 ) ;
#76722 = EDGE_CURVE ( 'NONE', #26122, #26501, #51400, .T. ) ;
#76723 = CARTESIAN_POINT ( 'NONE',  ( 170.8465782694706263, 283.6086715855652187, 12.33509960992013355 ) ) ;
#76724 = EDGE_CURVE ( 'NONE', #69960, #76591, #92921, .T. ) ;
#76725 = DIRECTION ( 'NONE',  ( 0.000000000000000000, 0.000000000000000000, 1.000000000000000000 ) ) ;
#76726 = CARTESIAN_POINT ( 'NONE',  ( 67.40003082602686391, 68.24590789163552529, -5.841565263471736991 ) ) ;
#76727 = ORIENTED_EDGE ( 'NONE', *, *, #55904, .T. ) ;
#76728 = CARTESIAN_POINT ( 'NONE',  ( 201.2591206913006658, 271.2044317791411459, -11.41792222164669113 ) ) ;
#76729 = CARTESIAN_POINT ( 'NONE',  ( 12.32504541118064978, 22.51421378149917985, -9.188101187500004485 ) ) ;
#76730 = CARTESIAN_POINT ( 'NONE',  ( 202.0661878422603763, 279.1895584290143120, -16.02388874507808225 ) ) ;
#76731 = DIRECTION ( 'NONE',  ( 0.1577859398657057155, -0.9874733399847793747, 0.000000000000000000 ) ) ;
#76733 = ORIENTED_EDGE ( 'NONE', *, *, #22040, .F. ) ;
#76732 = CARTESIAN_POINT ( 'NONE',  ( 20.30386484825465132, 170.9824982072973967, 3.021315404115420679E-15 ) ) ;
#76734 = CARTESIAN_POINT ( 'NONE',  ( 202.5245888501533216, 279.8641176599742266, 15.60152447840272494 ) ) ;
#76735 = DIRECTION ( 'NONE',  ( -0.000000000000000000, -0.000000000000000000, 1.000000000000000000 ) ) ;
#76736 = DIRECTION ( 'NONE',  ( -0.8660254037844387076, -0.4999999999999998890, -0.000000000000000000 ) ) ;
#76737 = CARTESIAN_POINT ( 'NONE',  ( 67.79478323710348775, 65.59340164614276603, -10.86706726790307798 ) ) ;
#76738 = CIRCLE ( 'NONE', #71914, 70.00000000000001421 ) ;
#76739 = CARTESIAN_POINT ( 'NONE',  ( 70.62955678152277983, 60.80479719363770386, -15.06269029744276899 ) ) ;
#76740 = CARTESIAN_POINT ( 'NONE',  ( 160.9160827979327166, 283.0037893736308661, 2.110134644200618137 ) ) ;
#76741 = ORIENTED_EDGE ( 'NONE', *, *, #39187, .F. ) ;
#76742 = CARTESIAN_POINT ( 'NONE',  ( 155.7106188756215204, 260.9482921598670373, -17.31404547047129938 ) ) ;
#76743 = CARTESIAN_POINT ( 'NONE',  ( 75.07870222088889989, 67.13256391452972593, -13.06718628923150405 ) ) ;
#76744 = CARTESIAN_POINT ( 'NONE',  ( 1.663964738649655661, 181.7677522451419350, -5.000000000000047962 ) ) ;
#76745 = VECTOR ( 'NONE', #80774, 1000.000000000000114 ) ;
#76746 = CARTESIAN_POINT ( 'NONE',  ( 82.51756260356231110, 53.28320474767543402, -15.32090594621901758 ) ) ;
#76747 = CARTESIAN_POINT ( 'NONE',  ( 165.6131678205262290, 248.3344997053549434, 8.498622568436868363 ) ) ;
#76748 = CARTESIAN_POINT ( 'NONE',  ( 163.8807549990905841, 246.7972012892647626, -8.911697419588444191 ) ) ;
#76749 = CARTESIAN_POINT ( 'NONE',  ( 83.23625814710678128, 44.68616627695709553, -9.226232325800772571 ) ) ;
#76750 = CARTESIAN_POINT ( 'NONE',  ( 162.6383036806675193, 250.7589265055833323, -12.97350464324780184 ) ) ;
#76752 = CARTESIAN_POINT ( 'NONE',  ( 31.67936943677743855, 23.45404122711135386, -8.090169943749478065 ) ) ;
#76751 = CARTESIAN_POINT ( 'NONE',  ( -2.016382903836450691, 160.4548013555409796, -4.594050593750042211 ) ) ;
#76753 = LINE ( 'NONE', #7346, #949 ) ;
#76754 = ORIENTED_EDGE ( 'NONE', *, *, #84524, .F. ) ;
#76755 = ORIENTED_EDGE ( 'NONE', *, *, #82586, .F. ) ;
#76756 = LINE ( 'NONE', #38745, #98219 ) ;
#76757 = CARTESIAN_POINT ( 'NONE',  ( 64.41134571303810219, 67.16059528448873550, 0.000000000000000000 ) ) ;
#76758 = CARTESIAN_POINT ( 'NONE',  ( 84.71689455500938948, 42.18615029519279602, 0.2983201894514607710 ) ) ;
#76759 = CARTESIAN_POINT ( 'NONE',  ( 202.7081908165554296, 279.5461097257963843, -16.92338847124122481 ) ) ;
#76760 = CARTESIAN_POINT ( 'NONE',  ( 71.06207387823002364, 70.85672049742558443, 6.009000135645388596 ) ) ;
#76761 = CARTESIAN_POINT ( 'NONE',  ( 151.2757240218323886, 277.1518032949712165, 3.694889182893786650 ) ) ;
#76762 = CARTESIAN_POINT ( 'NONE',  ( 14.59995888762994554, 188.4244531367911293, -4.594050593750046652 ) ) ;
#76763 = CARTESIAN_POINT ( 'NONE',  ( 111.8924135700967355, 247.6589784336661069, -6.496448406907675876E-16 ) ) ;
#76764 = CARTESIAN_POINT ( 'NONE',  ( 182.1055966411629186, 294.5202151697680506, -6.440452032333615406 ) ) ;
#76765 = CARTESIAN_POINT ( 'NONE',  ( 196.2659867875262876, 275.2308177797455642, 16.04285008767656606 ) ) ;
#76766 = CARTESIAN_POINT ( 'NONE',  ( 27.73493783529162116, 193.4865022471903160, -10.00000000000009592 ) ) ;
#76767 = EDGE_CURVE ( 'NONE', #39680, #34226, #34104, .T. ) ;
#76768 = CARTESIAN_POINT ( 'NONE',  ( 178.4166537163541193, 283.9060778229895163, -15.00412117590805572 ) ) ;
#76769 = EDGE_CURVE ( 'NONE', #40898, #67853, #8786, .T. ) ;
#76770 = CARTESIAN_POINT ( 'NONE',  ( 190.7246925096072516, 299.7733309290570674, -5.038784231807341918 ) ) ;
#76771 = CARTESIAN_POINT ( 'NONE',  ( 195.8248271798537417, 291.4684452715354155, 17.35175160929494709 ) ) ;
#76772 = CARTESIAN_POINT ( 'NONE',  ( 194.4263876777154394, 293.8906135405502482, 15.23185943445137802 ) ) ;
#76773 = CARTESIAN_POINT ( 'NONE',  ( 161.1747502674735415, 251.4841389699472529, -13.25152330924089839 ) ) ;
#76774 = CARTESIAN_POINT ( 'NONE',  ( 80.74974841587442143, 43.27611110060701805, 10.01619596027649095 ) ) ;
#76775 = PLANE ( 'NONE',  #74073 ) ;
#76776 = CARTESIAN_POINT ( 'NONE',  ( 192.7415923820568082, 264.8708757276006622, 7.413265226357134807 ) ) ;
#76777 = CARTESIAN_POINT ( 'NONE',  ( 169.3859977840389774, 278.7875771771462610, 14.01937899539775323 ) ) ;
#76778 = CARTESIAN_POINT ( 'NONE',  ( 175.4391368986771340, 256.4972366567271251, -10.87669320986560528 ) ) ;
#76779 = CARTESIAN_POINT ( 'NONE',  ( 70.51171994387159714, 70.77651729788739488, 4.033880998964182396 ) ) ;
#76780 = CARTESIAN_POINT ( 'NONE',  ( 71.47384123275857348, 72.35069954344788812, 1.100233114707620530 ) ) ;
#76781 = CARTESIAN_POINT ( 'NONE',  ( 151.7249709189835016, 274.7820922814796631, 10.79316925266204308 ) ) ;
#76782 = ORIENTED_EDGE ( 'NONE', *, *, #68441, .T. ) ;
#76783 = DIRECTION ( 'NONE',  ( 0.000000000000000000, 0.000000000000000000, 1.000000000000000000 ) ) ;
#76784 = CARTESIAN_POINT ( 'NONE',  ( 184.7639518824382776, 269.2648697177924078, 16.06510220747506068 ) ) ;
#76785 = ADVANCED_FACE ( 'NONE', ( #692 ), #53387, .T. ) ;
#76786 = CARTESIAN_POINT ( 'NONE',  ( 85.18102929606172324, 229.1744531367911293, 4.594050593750047540 ) ) ;
#76787 = CARTESIAN_POINT ( 'NONE',  ( 12.64980493759981250, 22.70171378149918340, -9.188101187500004485 ) ) ;
#76788 = CARTESIAN_POINT ( 'NONE',  ( 72.42824182984617210, 61.00551489497025415, -15.37960674554226159 ) ) ;
#76789 = FACE_OUTER_BOUND ( 'NONE', #83968, .T. ) ;
#76791 = CARTESIAN_POINT ( 'NONE',  ( 191.7417035528519875, 277.0673726153275425, 16.68325300976718850 ) ) ;
#76790 = CARTESIAN_POINT ( 'NONE',  ( 8.758203689844268780, 28.55466486950697913, -1.111400068045478839E-16 ) ) ;
#76792 = CARTESIAN_POINT ( 'NONE',  ( 196.5464242819039384, 290.2186024281901950, 17.89341495589234654 ) ) ;
#76793 = CARTESIAN_POINT ( 'NONE',  ( 198.7136873185829984, 286.4647927352960437, -18.57144721070432070 ) ) ;
#76794 = CARTESIAN_POINT ( 'NONE',  ( 137.6559535675401094, 261.8297689869268652, -2.679491924311252493 ) ) ;
#76795 = CARTESIAN_POINT ( 'NONE',  ( 39.71070620960689723, 31.43085787977766543, -9.188101187500008038 ) ) ;
#76796 = CARTESIAN_POINT ( 'NONE',  ( 192.4212750754384160, 297.3635704425909125, -12.73704185013552248 ) ) ;
#76797 = FACE_OUTER_BOUND ( 'NONE', #84612, .T. ) ;
#76798 = EDGE_LOOP ( 'NONE', ( #10293, #297, #19089, #18442 ) ) ;
#76799 = CARTESIAN_POINT ( 'NONE',  ( 31.93509797303403630, 20.29860640527293825, -2.839279412974138328 ) ) ;
#76800 = CARTESIAN_POINT ( 'NONE',  ( 71.71174882302005926, 58.93038559421764688, -15.88944412480316259 ) ) ;
#76801 = CARTESIAN_POINT ( 'NONE',  ( 82.25857016995360027, 53.22243677109732118, 15.71245593812844632 ) ) ;
#76802 = CARTESIAN_POINT ( 'NONE',  ( 149.6890529486499872, 271.3779502865075983, -12.51465682618088593 ) ) ;
#76803 =( BOUNDED_CURVE ( )  B_SPLINE_CURVE ( 2, ( #78464, #24739, #951, #39918, #16640, #92198, #77959, #70853, #31827 ),
 .UNSPECIFIED., .F., .T. ) 
 B_SPLINE_CURVE_WITH_KNOTS ( ( 3, 2, 2, 2, 3 ),
 ( 0.2379032258064516236, 0.2392473118279569988, 0.2419354838709677491, 0.2446236559139784994, 0.2459677419354838745 ),
 .UNSPECIFIED. ) 
 CURVE ( )  GEOMETRIC_REPRESENTATION_ITEM ( )  RATIONAL_B_SPLINE_CURVE ( ( 0.9330127018922194093, 0.9330127018922194093, 1.000000000000000000, 0.8660254037844387076, 1.000000000000000000, 0.8660254037844387076, 1.000000000000000000, 0.9330127018922194093, 0.9330127018922194093 ) ) 
 REPRESENTATION_ITEM ( '' )  );
#76804 = CARTESIAN_POINT ( 'NONE',  ( 84.78734842081532008, 50.40784050611168965, -13.89907628984690113 ) ) ;
#76805 = CARTESIAN_POINT ( 'NONE',  ( -73.83803415018344651, 50.74234351129840093, 10.00000000000000000 ) ) ;
#76806 = CARTESIAN_POINT ( 'NONE',  ( 75.00216722520403323, 65.29316891282158508, 14.16376155384191904 ) ) ;
#76807 = CARTESIAN_POINT ( 'NONE',  ( 171.2194629759952988, 253.1908842429618289, -8.786472813057685016 ) ) ;
#76808 = DIRECTION ( 'NONE',  ( 0.4270171210482450741, -0.9042435392811321027, 0.000000000000000000 ) ) ;
#76809 = ORIENTED_EDGE ( 'NONE', *, *, #43684, .F. ) ;
#76810 = CARTESIAN_POINT ( 'NONE',  ( 73.25535670630372920, 69.88482930906741331, 9.609716971570463784 ) ) ;
#76811 = B_SPLINE_SURFACE_WITH_KNOTS ( 'NONE', 3, 1, ( 
 ( #99264, #38933 ),
 ( #46527, #22753 ),
 ( #68340, #98273 ),
 ( #30847, #91187 ),
 ( #28861, #59739 ),
 ( #85081, #61733 ),
 ( #92682, #90707 ),
 ( #45040, #52142 ),
 ( #37431, #83091 ),
 ( #13662, #75465 ),
 ( #450, #78465 ),
 ( #69838, #94187 ),
 ( #85606, #62225 ),
 ( #16146, #79493 ),
 ( #10055, #9049 ),
 ( #23729, #86605 ),
 ( #48553, #1463 ),
 ( #24740, #39919 ),
 ( #70339, #55622 ),
 ( #16641, #47045 ),
 ( #17139, #31341 ),
 ( #9566, #48036 ),
 ( #93687, #32839 ),
 ( #55127, #70854 ),
 ( #32343, #77960 ),
 ( #8552, #39421 ),
 ( #63246, #952 ),
 ( #47536, #31828 ),
 ( #40920, #2466 ),
 ( #93177, #78980 ),
 ( #94682, #17656 ) ),
 .UNSPECIFIED., .F., .F., .F.,
 ( 4, 3, 3, 3, 3, 3, 3, 3, 3, 3, 4 ),
 ( 2, 2 ),
 ( 0.000000000000000000, 0.1333490885032361239, 0.3007194338854258242, 0.4699862290245113705, 0.5844252810809250631, 0.6686540514502664623, 0.7354980260655568092, 0.8028463152565741279, 0.8633854507757309227, 0.9437142632667492315, 1.000000000000000000 ),
 ( 0.000000000000000000, 1.000000000000000000 ),
 .UNSPECIFIED. ) ;
#76812 = CARTESIAN_POINT ( 'NONE',  ( 38.53854167689037524, 24.11110640527295246, -2.839279412974138328 ) ) ;
#76813 = ORIENTED_EDGE ( 'NONE', *, *, #11905, .F. ) ;
#76814 = CARTESIAN_POINT ( 'NONE',  ( 168.1385646420976343, 249.0247310940818011, 6.544369751715001016 ) ) ;
#76815 = CARTESIAN_POINT ( 'NONE',  ( 181.5035962553983211, 290.8403058601051612, -11.04694206434262682 ) ) ;
#76817 = ORIENTED_EDGE ( 'NONE', *, *, #9759, .F. ) ;
#76816 = AXIS2_PLACEMENT_3D ( 'NONE', #14515, #67713, #7916 ) ;
#76818 = LINE ( 'NONE', #59101, #60306 ) ;
#76819 = DIRECTION ( 'NONE',  ( -0.8660254037844387076, -0.4999999999999998890, -0.000000000000000000 ) ) ;
#76820 = CARTESIAN_POINT ( 'NONE',  ( 85.05760017557965114, 49.81609225799626017, 13.45342997944402796 ) ) ;
#76821 = CARTESIAN_POINT ( 'NONE',  ( 200.8251833487811666, 282.8075743310126882, -16.74393672780000131 ) ) ;
#76822 = LINE ( 'NONE', #7417, #17289 ) ;
#76823 = DIRECTION ( 'NONE',  ( -0.8660254037844387076, -0.4999999999999998890, -0.000000000000000000 ) ) ;
#76824 = CARTESIAN_POINT ( 'NONE',  ( 195.8961960204858599, 266.5302481932577621, 9.552191782196176817 ) ) ;
#76825 = LINE ( 'NONE', #47786, #82189 ) ;
#76826 = ORIENTED_EDGE ( 'NONE', *, *, #47844, .T. ) ;
#76827 = DIRECTION ( 'NONE',  ( 0.9681751565707763518, -0.2502735827033140681, 0.000000000000000000 ) ) ;
#76828 = VERTEX_POINT ( 'NONE', #54365 ) ;
#76829 = ORIENTED_EDGE ( 'NONE', *, *, #20706, .F. ) ;
#76830 = CARTESIAN_POINT ( 'NONE',  ( 172.2043063819207021, 270.6962890225300953, 16.45290475606747549 ) ) ;
#76832 = DIRECTION ( 'NONE',  ( 0.06142469166373833167, 0.9981117208278915687, 0.000000000000000000 ) ) ;
#76831 = CARTESIAN_POINT ( 'NONE',  ( -19.77365603540006944, 93.13978744366448836, 59.99999999999999289 ) ) ;
#76833 = DIRECTION ( 'NONE',  ( -0.9946578707245746775, -0.1032265479692855564, 0.000000000000000000 ) ) ;
#76834 = CARTESIAN_POINT ( 'NONE',  ( 200.9558679789573148, 274.8618586551609155, -13.87171223153703004 ) ) ;
#76835 = CARTESIAN_POINT ( 'NONE',  ( 72.39542100948224856, 61.59435533500952431, -14.66294840908354402 ) ) ;
#76836 = CARTESIAN_POINT ( 'NONE',  ( 82.64100954815702949, 40.51523152100199354, 0.8905920172003339852 ) ) ;
#76837 = CARTESIAN_POINT ( 'NONE',  ( 168.9820521491120360, 250.0049531100763716, -5.469593116480293560 ) ) ;
#76838 = EDGE_CURVE ( 'NONE', #79014, #82804, #22060, .T. ) ;
#76839 = CARTESIAN_POINT ( 'NONE',  ( 77.18662672379076639, 63.56519964668829203, -15.06539499090657763 ) ) ;
#76840 = CARTESIAN_POINT ( 'NONE',  ( 178.0511205245788346, 255.4621034402314024, 4.984966428951989492 ) ) ;
#76841 = CARTESIAN_POINT ( 'NONE',  ( 122.6912752411227103, 232.4548013555409796, -4.594050593750042211 ) ) ;
#76842 = CARTESIAN_POINT ( 'NONE',  ( 70.41572640437576069, 60.98787027670521610, -14.93661785217966198 ) ) ;
#76843 = CARTESIAN_POINT ( 'NONE',  ( 43.36002773778349706, 27.96004757982094446, -5.678558825948276656 ) ) ;
#76844 = CARTESIAN_POINT ( 'NONE',  ( 187.9335791911229023, 273.9157097510401400, 16.49127241766424490 ) ) ;
#76845 = ORIENTED_EDGE ( 'NONE', *, *, #7524, .F. ) ;
#76846 = VECTOR ( 'NONE', #24119, 1000.000000000000000 ) ;
#76847 = VERTEX_POINT ( 'NONE', #39662 ) ;
#76848 = CARTESIAN_POINT ( 'NONE',  ( 36.10619739613039769, 52.83927550304669296, 10.00000000000000000 ) ) ;
#76849 = CARTESIAN_POINT ( 'NONE',  ( 69.60926776342978428, 64.26717917311120232, -12.25031856425473364 ) ) ;
#76850 = DIRECTION ( 'NONE',  ( 0.000000000000000000, 0.000000000000000000, 1.000000000000000000 ) ) ;
#76851 = EDGE_CURVE ( 'NONE', #21764, #78112, #81327, .T. ) ;
#76852 = CARTESIAN_POINT ( 'NONE',  ( 146.6727924462101669, 276.6022667255962801, 3.481050673020940511 ) ) ;
#76853 = CARTESIAN_POINT ( 'NONE',  ( 159.2651917302844993, 254.7915913763855258, -16.53922207549818424 ) ) ;
#76854 = CARTESIAN_POINT ( 'NONE',  ( 73.85566786302621267, 55.32763327914238261, -16.11774481835226069 ) ) ;
#76855 = ORIENTED_EDGE ( 'NONE', *, *, #95548, .F. ) ;
#76856 = CARTESIAN_POINT ( 'NONE',  ( 148.3925088351605552, 273.6236305653253567, 10.42437868982396054 ) ) ;
#76857 = ORIENTED_EDGE ( 'NONE', *, *, #22340, .T. ) ;
#76858 = PLANE ( 'NONE',  #75354 ) ;
#76859 = DIRECTION ( 'NONE',  ( 1.000000000000000000, 1.048764250047692355E-13, 0.000000000000000000 ) ) ;
#76860 = ORIENTED_EDGE ( 'NONE', *, *, #32493, .F. ) ;
#76861 = CYLINDRICAL_SURFACE ( 'NONE', #67795, 16.60714546451156792 ) ;
#76862 = CARTESIAN_POINT ( 'NONE',  ( 196.0526458812441035, 264.7804988895400697, 3.830367068405413189 ) ) ;
#76863 = CARTESIAN_POINT ( 'NONE',  ( 158.3700511340344121, 263.3548805506079020, 17.43552943246885789 ) ) ;
#76864 = DIRECTION ( 'NONE',  ( -0.8903844177683322147, -0.4552093898365321412, 0.000000000000000000 ) ) ;
#76866 = DIRECTION ( 'NONE',  ( -0.8660254037844387076, -0.4999999999999998890, -0.000000000000000000 ) ) ;
#76865 = CARTESIAN_POINT ( 'NONE',  ( 184.3332131814447621, 288.6360765898637624, -14.21508448381140965 ) ) ;
#76867 = CARTESIAN_POINT ( 'NONE',  ( 153.2513309553138470, 265.2079037882803618, -16.24091495603130397 ) ) ;
#76868 = VERTEX_POINT ( 'NONE', #61968 ) ;
#76869 = CARTESIAN_POINT ( 'NONE',  ( 190.1635032421960148, 301.2741459696644029, -5.047660290019184259 ) ) ;
#76870 = CARTESIAN_POINT ( 'NONE',  ( 73.65729962767424865, 69.49757902785616182, 9.740712345197151123 ) ) ;
#76871 = CARTESIAN_POINT ( 'NONE',  ( 82.50439176478489856, 40.89164830652052274, -3.703415047413355143 ) ) ;
#76872 = CARTESIAN_POINT ( 'NONE',  ( 33.41027130880567597, 178.5494855054051300, -2.679491924311248496 ) ) ;
#76873 = CARTESIAN_POINT ( 'NONE',  ( 189.5354676446069391, 270.3341974172179221, -14.09206254053018270 ) ) ;
#76874 = CARTESIAN_POINT ( 'NONE',  ( 177.9552638626009298, 260.7378092407702184, -13.94576028113082877 ) ) ;
#76875 = VECTOR ( 'NONE', #62482, 1000.000000000000114 ) ;
#76876 = CARTESIAN_POINT ( 'NONE',  ( 36.44700672854521883, 203.3967562850347122, 1.101618078115930403E-13 ) ) ;
#76877 = CARTESIAN_POINT ( 'NONE',  ( 23.08833070876649529, 13.73415679381821874, 1.333680081654574804E-15 ) ) ;
#76878 = CARTESIAN_POINT ( 'NONE',  ( 191.4168617962777148, 282.8041663340243872, -17.08726176923725149 ) ) ;
#76879 = CARTESIAN_POINT ( 'NONE',  ( -57.04299263576977097, 30.72821847190685673, 10.00000000000000000 ) ) ;
#76880 = CARTESIAN_POINT ( 'NONE',  ( 68.83479979963041728, 219.7369531367911293, -4.594050593750048428 ) ) ;
#76881 = CARTESIAN_POINT ( 'NONE',  ( 26.17072728691639583, 197.4637435831424739, 2.679491924311251605 ) ) ;
#76882 = CARTESIAN_POINT ( 'NONE',  ( 192.8607783413999073, 296.6023284558532396, -11.80574095728561446 ) ) ;
#76883 = DIRECTION ( 'NONE',  ( -0.7561390817803280706, 0.6544109481086042290, 0.000000000000000000 ) ) ;
#76884 = CARTESIAN_POINT ( 'NONE',  ( 155.3716771045260714, 261.5353565282119348, -18.54934131471355840 ) ) ;
#76885 = ADVANCED_FACE ( 'NONE', ( #76223 ), #92434, .T. ) ;
#76886 = CARTESIAN_POINT ( 'NONE',  ( 161.8153478334749877, 250.3745914384277285, -14.21120979595050215 ) ) ;
#76888 = CARTESIAN_POINT ( 'NONE',  ( 75.84856439504059722, 51.76521084193598199, 15.76359423700354689 ) ) ;
#76887 = CARTESIAN_POINT ( 'NONE',  ( -22.42236680055709641, 157.8615022471902591, 0.000000000000000000 ) ) ;
#76889 = DIRECTION ( 'NONE',  ( -0.6386832404231509441, -0.7694697644498993405, 0.000000000000000000 ) ) ;
#76890 = CARTESIAN_POINT ( 'NONE',  ( 45.03145032967896100, 28.12755873383630600, -6.180339887498949025 ) ) ;
#76891 = CARTESIAN_POINT ( 'NONE',  ( 204.8015065334591043, 275.9203805478366576, -12.93433564072899600 ) ) ;
#76892 = CARTESIAN_POINT ( 'NONE',  ( 157.4656258344471098, 257.9085309395441641, 18.30485740784190796 ) ) ;
#76893 = CARTESIAN_POINT ( 'NONE',  ( 71.68255973785201718, 72.12657461437540007, 3.318624374305799041 ) ) ;
#76894 = CARTESIAN_POINT ( 'NONE',  ( 32.43492986863949312, 189.5333772461660544, 9.188101187500095079 ) ) ;
#76895 = EDGE_CURVE ( 'NONE', #56834, #50040, #68591, .T. ) ;
#76896 = CARTESIAN_POINT ( 'NONE',  ( 60.66220569506229765, 196.6423013555410080, -4.594050593750043987 ) ) ;
#76897 = CARTESIAN_POINT ( 'NONE',  ( 157.5042325173297684, 257.8416622032797818, 16.70595240278738203 ) ) ;
#76898 = CARTESIAN_POINT ( 'NONE',  ( 81.24166145016371843, 42.23607023897516655, -7.290125548428411761 ) ) ;
#76899 = DIRECTION ( 'NONE',  ( 0.4999999999999998890, -0.8660254037844385966, 0.000000000000000000 ) ) ;
#76900 = CARTESIAN_POINT ( 'NONE',  ( 150.1604317434691325, 251.3768266524160140, -9.188101187500091527 ) ) ;
#76901 = CARTESIAN_POINT ( 'NONE',  ( -9.693023484072631035, 23.77726266618847717, 177.5919119679930134 ) ) ;
#76902 = CARTESIAN_POINT ( 'NONE',  ( 200.1288169248181816, 270.7711892690550712, -11.55673819778957956 ) ) ;
#76903 = AXIS2_PLACEMENT_3D ( 'NONE', #87429, #71669, #64547 ) ;
#76904 = CARTESIAN_POINT ( 'NONE',  ( 15.40246583222295129, 30.93396525600389424, 2.839279412974139660 ) ) ;
#76905 = CARTESIAN_POINT ( 'NONE',  ( 198.4427928769277969, 286.9339956717308837, -17.97122743692687763 ) ) ;
#76906 = CARTESIAN_POINT ( 'NONE',  ( 82.10990542498430500, 41.84899041517284957, 5.504228460268151046 ) ) ;
#76907 = CARTESIAN_POINT ( 'NONE',  ( 17.90548643172614263, 12.19860640527291373, 2.839279412974134775 ) ) ;
#76908 = CARTESIAN_POINT ( 'NONE',  ( 60.68900866710680475, 205.8458772461660544, 9.188101187500095079 ) ) ;
#76909 = CARTESIAN_POINT ( 'NONE',  ( -49.78034631855285141, 29.87998972566341749, 177.5919119679930134 ) ) ;
#76910 = B_SPLINE_CURVE_WITH_KNOTS ( 'NONE', 3,
 ( #27602, #97506, #89919, #98992, #29575, #91406 ),
 .UNSPECIFIED., .F., .F.,
 ( 4, 2, 4 ),
 ( 0.02165947195459741459, 0.02624956959626738653, 0.03083966723793735848 ),
 .UNSPECIFIED. ) ;
#76911 = CARTESIAN_POINT ( 'NONE',  ( 78.61941745410977944, 58.11157619480126613, -16.59458311719091128 ) ) ;
#76912 = CARTESIAN_POINT ( 'NONE',  ( 159.5573297132660002, 254.2855935470410031, 16.91607698584599007 ) ) ;
#76913 = CARTESIAN_POINT ( 'NONE',  ( 82.09480132358520166, 40.75487975465649271, -0.9815627762904419740 ) ) ;
#76914 = CARTESIAN_POINT ( 'NONE',  ( 153.0920794520761206, 277.2686993117134762, 8.274819790008697495 ) ) ;
#76915 = ADVANCED_FACE ( 'NONE', ( #22981 ), #61982, .T. ) ;
#76916 = VECTOR ( 'NONE', #68148, 1000.000000000000114 ) ;
#76917 = CARTESIAN_POINT ( 'NONE',  ( 76.73822351447255130, 56.29186403409720185, -16.16359082176946416 ) ) ;
#76918 = CARTESIAN_POINT ( 'NONE',  ( 111.0177141658951143, 248.2365022471903444, 2.944929066748280225E-16 ) ) ;
#76919 = CARTESIAN_POINT ( 'NONE',  ( 200.1444820856229967, 283.9865835035790269, 17.93386694781497326 ) ) ;
#76920 = CARTESIAN_POINT ( 'NONE',  ( 207.6918009085542849, 270.9142438413412037, 7.009114282139513818 ) ) ;
#76921 = VERTEX_POINT ( 'NONE', #16886 ) ;
#76922 = CARTESIAN_POINT ( 'NONE',  ( 77.08242418523479955, 49.46725263400162476, 15.46546490473176938 ) ) ;
#76923 = ORIENTED_EDGE ( 'NONE', *, *, #69056, .F. ) ;
#76924 = CARTESIAN_POINT ( 'NONE',  ( 159.9894443651313338, 253.5371490153152081, -16.36035038356864391 ) ) ;
#76925 = CARTESIAN_POINT ( 'NONE',  ( 186.8956715526903167, 276.6081854589048135, -17.33659699395019516 ) ) ;
#76926 = CARTESIAN_POINT ( 'NONE',  ( -12.56269525828471245, 104.2312461070085021, 45.19948692389422717 ) ) ;
#76927 = ORIENTED_EDGE ( 'NONE', *, *, #41114, .T. ) ;
#76928 = ORIENTED_EDGE ( 'NONE', *, *, #89860, .F. ) ;
#76929 = CARTESIAN_POINT ( 'NONE',  ( 79.21534038901880592, 46.09240496756496697, -13.22827714657437781 ) ) ;
#76930 = CARTESIAN_POINT ( 'NONE',  ( 194.1789525331299728, 294.3191837825503967, -15.34533909744314961 ) ) ;
#76931 = CARTESIAN_POINT ( 'NONE',  ( 177.0218378549533327, 274.6764583735296696, -16.80540863426473308 ) ) ;
#76932 = CARTESIAN_POINT ( 'NONE',  ( 20.76088743254790359, 12.39040679176982529, 1.333680081654574804E-15 ) ) ;
#76933 = EDGE_LOOP ( 'NONE', ( #27277, #88492, #29059, #83642 ) ) ;
#76934 = CARTESIAN_POINT ( 'NONE',  ( 18.21401815691482895, 25.91421378149918553, 9.188101187500008038 ) ) ;
#76935 = AXIS2_PLACEMENT_3D ( 'NONE', #4552, #43544, #28343 ) ;
#76936 = PLANE ( 'NONE',  #89386 ) ;
#76937 = ADVANCED_FACE ( 'NONE', ( #71112 ), #78223, .F. ) ;
#76938 = EDGE_CURVE ( 'NONE', #23598, #18450, #40985, .T. ) ;
#76939 = ORIENTED_EDGE ( 'NONE', *, *, #15028, .F. ) ;
#76940 = CARTESIAN_POINT ( 'NONE',  ( 178.8595466249924755, 265.0989930076032124, -16.03772641351113748 ) ) ;
#76941 = CARTESIAN_POINT ( 'NONE',  ( 46.43574122514301195, 74.10519008736565638, -10.00000000000000000 ) ) ;
#76942 = AXIS2_PLACEMENT_3D ( 'NONE', #2525, #18718, #95763 ) ;
#76943 = ORIENTED_EDGE ( 'NONE', *, *, #4642, .T. ) ;
#76944 = EDGE_CURVE ( 'NONE', #52938, #12952, #38506, .T. ) ;
#76945 = CARTESIAN_POINT ( 'NONE',  ( 174.7281960057983383, 286.2758036095501097, 11.50214825767278448 ) ) ;
#76947 = CARTESIAN_POINT ( 'NONE',  ( 67.71824482912023768, 65.66011283822241751, -10.75488218253084582 ) ) ;
#76946 = CARTESIAN_POINT ( 'NONE',  ( 72.61942445857775397, 68.50386890797452111, 10.74179888713238107 ) ) ;
#76948 = CARTESIAN_POINT ( 'NONE',  ( 47.66616421796181413, 112.2513067263565034, 10.00000000000000000 ) ) ;
#76949 = CARTESIAN_POINT ( 'NONE',  ( 163.7239493340838123, 247.0687966679708438, 6.286946239157660266 ) ) ;
#76950 = DIRECTION ( 'NONE',  ( -0.8660254037844379305, -0.5000000000000014433, -0.000000000000000000 ) ) ;
#76951 = CARTESIAN_POINT ( 'NONE',  ( 164.6294852917785931, 265.1817657174682381, -16.63052033780461869 ) ) ;
#76952 = CARTESIAN_POINT ( 'NONE',  ( 144.9103262809084924, 242.2202760586659167, -5.415160957724236172E-17 ) ) ;
#76953 = EDGE_CURVE ( 'NONE', #45907, #14302, #88698, .T. ) ;
#76954 = CARTESIAN_POINT ( 'NONE',  ( 177.3466669983353938, 269.1945114843388751, 16.08467660924950593 ) ) ;
#76955 = CARTESIAN_POINT ( 'NONE',  ( 181.2069392775523227, 259.9445122199059597, 9.505921896722259845 ) ) ;
#76956 = CARTESIAN_POINT ( 'NONE',  ( 63.63864737692379236, 216.7369531367911293, -4.594050593750048428 ) ) ;
#76957 = ORIENTED_EDGE ( 'NONE', *, *, #4123, .F. ) ;
#76958 = CARTESIAN_POINT ( 'NONE',  ( 173.6315150813169623, 265.4685547730397843, 16.13185304422783162 ) ) ;
#76959 = CARTESIAN_POINT ( 'NONE',  ( 73.50309919034782524, 60.00084379880728847, -15.88072908836307029 ) ) ;
#76960 = DIRECTION ( 'NONE',  ( -0.9681751565707790164, 0.2502735827033040761, 0.000000000000000000 ) ) ;
#76961 = VERTEX_POINT ( 'NONE', #88675 ) ;
#76962 = CARTESIAN_POINT ( 'NONE',  ( 157.3040537939580190, 258.1883819227538197, -18.30432891822131225 ) ) ;
#76963 = ORIENTED_EDGE ( 'NONE', *, *, #96849, .T. ) ;
#76964 = EDGE_CURVE ( 'NONE', #19465, #60481, #69255, .T. ) ;
#76965 = CARTESIAN_POINT ( 'NONE',  ( 79.15288444911743682, 228.0530062829863027, -4.648177544792955347E-16 ) ) ;
#76966 = CARTESIAN_POINT ( 'NONE',  ( 66.94906710382659298, 68.02340058291366631, 6.944469598640234942 ) ) ;
#76967 = EDGE_CURVE ( 'NONE', #27862, #63672, #4014, .T. ) ;
#76968 = CARTESIAN_POINT ( 'NONE',  ( 197.8021188482492789, 286.7634004315060565, 16.92933056012654802 ) ) ;
#76969 = CARTESIAN_POINT ( 'NONE',  ( 146.7373254022577100, 276.4904923669593586, -0.7242168585908188572 ) ) ;
#76970 = DIRECTION ( 'NONE',  ( -0.5000000000000013323, 0.8660254037844380415, 0.000000000000000000 ) ) ;
#76971 = CARTESIAN_POINT ( 'NONE',  ( 155.2098048002210930, 261.8157275836062468, 16.98811268941991059 ) ) ;
#76972 = CARTESIAN_POINT ( 'NONE',  ( 70.47523177494278457, 64.09717175604362183, 12.73376050057014197 ) ) ;
#76973 = CARTESIAN_POINT ( 'NONE',  ( 76.87303194821100760, 209.0643266524160424, 9.188101187500095079 ) ) ;
#76974 = VERTEX_POINT ( 'NONE', #3049 ) ;
#76975 = ORIENTED_EDGE ( 'NONE', *, *, #16900, .T. ) ;
#76976 = DIRECTION ( 'NONE',  ( 1.000000000000000000, 1.156482317317871331E-15, 0.000000000000000000 ) ) ;
#76977 = ORIENTED_EDGE ( 'NONE', *, *, #98597, .F. ) ;
#76978 = CARTESIAN_POINT ( 'NONE',  ( -42.18065534595050536, 68.63081177882914119, -10.00000000000000000 ) ) ;
#76979 = CARTESIAN_POINT ( 'NONE',  ( -28.04097607764120781, 24.82386083235215679, 10.00000000000000000 ) ) ;
#76980 = AXIS2_PLACEMENT_3D ( 'NONE', #57164, #3503, #88145 ) ;
#76981 = CARTESIAN_POINT ( 'NONE',  ( 163.4520133936471495, 284.3138964249058631, 0.5061738602265062337 ) ) ;
#76982 = DIRECTION ( 'NONE',  ( 0.000000000000000000, -0.000000000000000000, 1.000000000000000000 ) ) ;
#76983 = CARTESIAN_POINT ( 'NONE',  ( 162.7485557827231446, 261.3830000631959365, 17.54795403777559670 ) ) ;
#76984 = EDGE_LOOP ( 'NONE', ( #68402, #27780, #27511, #44654 ) ) ;
#76985 = CARTESIAN_POINT ( 'NONE',  ( 158.8270733235451075, 260.0119502166541565, 17.68969926203419618 ) ) ;
#76986 = CARTESIAN_POINT ( 'NONE',  ( 156.6857699971041029, 274.0622359378131137, 13.49643617979643118 ) ) ;
#76987 = DIRECTION ( 'NONE',  ( -0.8660254037844387076, -0.4999999999999998890, -0.000000000000000000 ) ) ;
#76988 = CARTESIAN_POINT ( 'NONE',  ( 153.0927037754837556, 265.4826541232073964, -16.15085267704102634 ) ) ;
#76989 = CARTESIAN_POINT ( 'NONE',  ( 72.72146555473813123, 70.80955590929056598, 7.150549449074294905 ) ) ;
#76990 = CARTESIAN_POINT ( 'NONE',  ( 187.7710022618638277, 277.0665775429750397, -17.72351784843695555 ) ) ;
#76991 = VERTEX_POINT ( 'NONE', #56711 ) ;
#76992 = CARTESIAN_POINT ( 'NONE',  ( 199.7757112945883478, 266.5330615442240401, 4.708490324072631239 ) ) ;
#76993 = CARTESIAN_POINT ( 'NONE',  ( -19.65312891409030271, 93.06504152958497400, 10.00000000000000888 ) ) ;
#76994 = CARTESIAN_POINT ( 'NONE',  ( 20.74252405664088172, 194.3297689869269220, -2.679491924311252493 ) ) ;
#76995 = CARTESIAN_POINT ( 'NONE',  ( 80.22871040234743134, 48.51986718445390778, 13.76706510026316899 ) ) ;
#76996 = CARTESIAN_POINT ( 'NONE',  ( 83.46914375417860299, 52.40757773513071527, 14.82330941673155245 ) ) ;
#76997 = CARTESIAN_POINT ( 'NONE',  ( 156.0186942281396796, 271.8450601007914997, 14.11081356587844660 ) ) ;
#76998 = VERTEX_POINT ( 'NONE', #48628 ) ;
#76999 = CARTESIAN_POINT ( 'NONE',  ( 147.5813496936708020, 275.0285994114094592, 4.516581957185684004 ) ) ;
#77000 = CARTESIAN_POINT ( 'NONE',  ( 202.8211298556536804, 279.3504935719197988, 17.07914446815911447 ) ) ;
#77001 = EDGE_CURVE ( 'NONE', #55644, #23266, #47515, .T. ) ;
#77002 = VECTOR ( 'NONE', #36131, 1000.000000000000000 ) ;
#77003 = CARTESIAN_POINT ( 'NONE',  ( 164.2600772519394923, 246.1401958748887182, -2.110785484364219311 ) ) ;
#77005 = CARTESIAN_POINT ( 'NONE',  ( 73.99094044066663400, 55.21107462180383862, 16.12321973269548536 ) ) ;
#77004 = CARTESIAN_POINT ( 'NONE',  ( 194.3799873100184641, 293.9709813348915191, 15.33105633561973669 ) ) ;
#77006 = EDGE_CURVE ( 'NONE', #71517, #76398, #18497, .T. ) ;
#77007 = CARTESIAN_POINT ( 'NONE',  ( 21.45610022030931674, 34.16126292948896293, -6.180339887498951690 ) ) ;
#77008 = LINE ( 'NONE', #52212, #30584 ) ;
#77009 = CARTESIAN_POINT ( 'NONE',  ( 165.4889794677011423, 286.4264833526404459, -3.351811820826717359 ) ) ;
#77010 = CARTESIAN_POINT ( 'NONE',  ( 129.1320788617196911, 245.3615022471902591, -10.00000000000009592 ) ) ;
#77011 = AXIS2_PLACEMENT_3D ( 'NONE', #54431, #46858, #52462 ) ;
#77012 = DIRECTION ( 'NONE',  ( -0.5000000000000002220, 0.8660254037844384856, 0.000000000000000000 ) ) ;
#77013 = CARTESIAN_POINT ( 'NONE',  ( -12.49048504844327745, 175.8464784336661353, 1.353441290958777327E-15 ) ) ;
#77014 = DIRECTION ( 'NONE',  ( -0.5000000000000014433, 0.8660254037844379305, 0.000000000000000000 ) ) ;
#77015 = ORIENTED_EDGE ( 'NONE', *, *, #89670, .T. ) ;
#77016 = EDGE_CURVE ( 'NONE', #4561, #23431, #81067, .T. ) ;
#77017 = CARTESIAN_POINT ( 'NONE',  ( 67.02157033833375976, 67.70868166164997604, -6.467237866492896892 ) ) ;
#77018 = FACE_OUTER_BOUND ( 'NONE', #80874, .T. ) ;
#77019 = CARTESIAN_POINT ( 'NONE',  ( 81.57634712059733317, 41.66383691174480930, 5.797449893469142523 ) ) ;
#77020 = CARTESIAN_POINT ( 'NONE',  ( 15.73713787374454043, 170.7048013555409796, 4.594050593750051981 ) ) ;
#77021 = CARTESIAN_POINT ( 'NONE',  ( 76.77173841120222164, 63.31185858333683569, -15.44871830894366838 ) ) ;
#77022 = CARTESIAN_POINT ( 'NONE',  ( 25.55253460671674759, 33.49103043416550918, -8.090169943749479842 ) ) ;
#77023 = CARTESIAN_POINT ( 'NONE',  ( 181.1741292703470663, 294.4598225981704331, 6.531841373275609541 ) ) ;
#77024 = CARTESIAN_POINT ( 'NONE',  ( 170.9037867558837718, 271.1323369732969013, -16.66440209927639415 ) ) ;
#77025 = CARTESIAN_POINT ( 'NONE',  ( 154.9032082715209810, 280.6326124547101699, -2.389722542998433230 ) ) ;
#77026 = CARTESIAN_POINT ( 'NONE',  ( 175.9272209172219164, 253.8149587822312014, -3.863606349031126097 ) ) ;
#77027 = ADVANCED_FACE ( 'NONE', ( #25836 ), #11630, .T. ) ;
#77028 = CARTESIAN_POINT ( 'NONE',  ( 188.6440864781562539, 260.6118655346156174, -0.7579459963146770729 ) ) ;
#77029 = EDGE_CURVE ( 'NONE', #861, #71916, #95769, .T. ) ;
#77030 = CARTESIAN_POINT ( 'NONE',  ( 182.9192744200266816, 296.0790939607076098, 1.760360045685976260 ) ) ;
#77031 = CARTESIAN_POINT ( 'NONE',  ( 69.30415721694468800, 217.4865022471902876, -10.00000000000009415 ) ) ;
#77032 = CARTESIAN_POINT ( 'NONE',  ( 44.96521122863986619, 26.36477965099644649, 1.583844403245364907 ) ) ;
#77033 = CARTESIAN_POINT ( 'NONE',  ( 148.3997536239841679, 273.6110822229926498, 8.713694244701960301 ) ) ;
#77034 = CARTESIAN_POINT ( 'NONE',  ( 39.11982377592438809, 184.2048013555409796, 4.594050593750051981 ) ) ;
#77035 = CARTESIAN_POINT ( 'NONE',  ( 67.41248320326423027, 66.37693208286884783, -8.946798147498746800 ) ) ;
#77036 = DIRECTION ( 'NONE',  ( -1.000000000000000000, -4.892646582057397676E-14, 0.000000000000000000 ) ) ;
#77037 = CARTESIAN_POINT ( 'NONE',  ( 203.0143287164872845, 269.9738428714081238, -6.283217384528930971 ) ) ;
#77038 = CARTESIAN_POINT ( 'NONE',  ( 151.2646864780760723, 268.6488729594320830, -14.38346604407754548 ) ) ;
#77039 = CARTESIAN_POINT ( 'NONE',  ( 207.6860335175200589, 270.9242332556395922, 6.913225035677485586 ) ) ;
#77040 = CARTESIAN_POINT ( 'NONE',  ( 185.1815156408660812, 266.7917036737816261, 13.95118630758742917 ) ) ;
#77041 = CARTESIAN_POINT ( 'NONE',  ( 163.1964476821512449, 280.9516185401507755, -10.10006455857531371 ) ) ;
#77042 = DIRECTION ( 'NONE',  ( -0.000000000000000000, 0.000000000000000000, -1.000000000000000000 ) ) ;
#77043 = CARTESIAN_POINT ( 'NONE',  ( 19.08967936351193373, 31.99752408145592497, 5.678558825948277544 ) ) ;
#77044 = DIRECTION ( 'NONE',  ( -0.8660254037844359321, -0.5000000000000051070, -0.000000000000000000 ) ) ;
#77045 = CARTESIAN_POINT ( 'NONE',  ( 71.81391265307100014, 59.05408711125518550, 15.87230141160151575 ) ) ;
#77046 = CARTESIAN_POINT ( 'NONE',  ( 188.7841062153288192, 270.3218309834035153, -14.49186609326428687 ) ) ;
#77047 = ORIENTED_EDGE ( 'NONE', *, *, #14843, .T. ) ;
#77048 = VECTOR ( 'NONE', #88137, 1000.000000000000000 ) ;
#77049 = CARTESIAN_POINT ( 'NONE',  ( 5.396842180905147224, 18.51421378149916208, -9.188101187500004485 ) ) ;
#77050 = CARTESIAN_POINT ( 'NONE',  ( -22.42236680055709641, 157.8615022471902591, 0.000000000000000000 ) ) ;
#77051 = CARTESIAN_POINT ( 'NONE',  ( 80.25178558894602077, 57.14685393251872370, -16.23521980932009612 ) ) ;
#77052 = CARTESIAN_POINT ( 'NONE',  ( 48.29091023345864642, 82.53782597618220507, 10.00000000000000000 ) ) ;
#77053 = EDGE_CURVE ( 'NONE', #94311, #86378, #6124, .T. ) ;
#77054 = CARTESIAN_POINT ( 'NONE',  ( 155.6483466250159893, 262.7148938034327443, -17.56146835583262344 ) ) ;
#77055 = ORIENTED_EDGE ( 'NONE', *, *, #35387, .F. ) ;
#77056 = CARTESIAN_POINT ( 'NONE',  ( 32.06367262104295435, 91.81775857601540736, 59.99999999999999289 ) ) ;
#77057 = DIRECTION ( 'NONE',  ( -0.8660254037844387076, -0.4999999999999998890, -0.000000000000000000 ) ) ;
#77058 = AXIS2_PLACEMENT_3D ( 'NONE', #33508, #57288, #95853 ) ;
#77059 = CARTESIAN_POINT ( 'NONE',  ( 72.84393339948680079, 57.07810317368846142, 16.39299656256352833 ) ) ;
#77060 = CARTESIAN_POINT ( 'NONE',  ( 87.35606880162971777, 45.77061481740688009, 8.290963297571636303 ) ) ;
#77061 = ORIENTED_EDGE ( 'NONE', *, *, #71734, .F. ) ;
#77062 = VERTEX_POINT ( 'NONE', #60675 ) ;
#77063 = EDGE_CURVE ( 'NONE', #56753, #315, #43759, .T. ) ;
#77065 = CARTESIAN_POINT ( 'NONE',  ( 86.27418400483192329, 43.17587234054840195, -1.979591663834713966 ) ) ;
#77064 = CARTESIAN_POINT ( 'NONE',  ( -14.83262083840143575, 124.7156766241961208, 21.50000000000006750 ) ) ;
#77066 = ORIENTED_EDGE ( 'NONE', *, *, #540, .T. ) ;
#77067 = CARTESIAN_POINT ( 'NONE',  ( 150.7530568467738590, 269.5350414755053521, 15.60317050893315916 ) ) ;
#77068 = DIRECTION ( 'NONE',  ( 0.5000000000000014433, -0.8660254037844378194, 0.000000000000000000 ) ) ;
#77069 = CARTESIAN_POINT ( 'NONE',  ( 79.91723393423865218, 58.07319122800065259, 16.26806395467770727 ) ) ;
#77070 = CARTESIAN_POINT ( 'NONE',  ( 71.44486053167919692, 69.80518736647204037, -8.307854525019157776 ) ) ;
#77071 = ORIENTED_EDGE ( 'NONE', *, *, #90152, .T. ) ;
#77072 = CARTESIAN_POINT ( 'NONE',  ( 189.9462859318020946, 301.6503773875500087, -1.164147598593831656 ) ) ;
#77073 = EDGE_CURVE ( 'NONE', #38281, #97061, #6005, .T. ) ;
#77074 = CARTESIAN_POINT ( 'NONE',  ( 196.5806080813426888, 290.1593943507663766, -16.31912166233602690 ) ) ;
#77075 = ORIENTED_EDGE ( 'NONE', *, *, #37389, .T. ) ;
#77076 = AXIS2_PLACEMENT_3D ( 'NONE', #44099, #68905, #5618 ) ;
#77077 = CARTESIAN_POINT ( 'NONE',  ( 157.3988263959001870, 258.0242309610243865, 16.72376558639979294 ) ) ;
#77078 = EDGE_CURVE ( 'NONE', #31865, #98895, #66313, .T. ) ;
#77079 = CIRCLE ( 'NONE', #43081, 0.1418229129681591871 ) ;
#77080 = CARTESIAN_POINT ( 'NONE',  ( 158.6580134701507632, 265.3810918834140580, 16.98815342382654947 ) ) ;
#77081 = VERTEX_POINT ( 'NONE', #98226 ) ;
#77082 = DIRECTION ( 'NONE',  ( -0.5895128895116622525, -0.8077589696806904973, 0.000000000000000000 ) ) ;
#77083 = CARTESIAN_POINT ( 'NONE',  ( 78.17014198728131191, 47.55004527273559489, -13.86079054836211810 ) ) ;
#77084 = VERTEX_POINT ( 'NONE', #52590 ) ;
#77085 = CARTESIAN_POINT ( 'NONE',  ( -16.46315656107408287, 74.30252503275481502, 13.46087100379897450 ) ) ;
#77086 = FACE_BOUND ( 'NONE', #47440, .T. ) ;
#77087 = CARTESIAN_POINT ( 'NONE',  ( 162.1260167985288376, 266.6785162637209510, 17.71249957499354366 ) ) ;
#77089 = VECTOR ( 'NONE', #71386, 1000.000000000000114 ) ;
#77088 = CARTESIAN_POINT ( 'NONE',  ( 83.66769832939698404, 52.30133544591161865, 14.73017738415024169 ) ) ;
#77090 = ORIENTED_EDGE ( 'NONE', *, *, #13148, .F. ) ;
#77091 = VERTEX_POINT ( 'NONE', #83044 ) ;
#77092 =( BOUNDED_CURVE ( )  B_SPLINE_CURVE ( 2, ( #42328, #58042, #4341, #34246, #89023, #19574, #65143, #28133, #50434 ),
 .UNSPECIFIED., .F., .T. ) 
 B_SPLINE_CURVE_WITH_KNOTS ( ( 3, 2, 2, 2, 3 ),
 ( 0.1169354838709677491, 0.1182795698924731242, 0.1209677419354838745, 0.1236559139784946248, 0.1250000000000000000 ),
 .UNSPECIFIED. ) 
 CURVE ( )  GEOMETRIC_REPRESENTATION_ITEM ( )  RATIONAL_B_SPLINE_CURVE ( ( 0.9330127018922192983, 0.9330127018922196314, 1.000000000000000000, 0.8660254037844387076, 1.000000000000000000, 0.8660254037844387076, 1.000000000000000000, 0.9330127018922194093, 0.9330127018922194093 ) ) 
 REPRESENTATION_ITEM ( '' )  );
#77093 = LINE ( 'NONE', #62373, #67462 ) ;
#77094 = CARTESIAN_POINT ( 'NONE',  ( 77.57756690181206238, 204.0494855054051868, -2.679491924311248496 ) ) ;
#77095 = CARTESIAN_POINT ( 'NONE',  ( 147.7870527676176948, 274.6723112360602386, 9.257357958194809555 ) ) ;
#77096 = CARTESIAN_POINT ( 'NONE',  ( 148.9517569034208009, 272.6549844970639924, 12.50737104496728236 ) ) ;
#77097 = CARTESIAN_POINT ( 'NONE',  ( 173.0421597889786369, 276.4496783815933441, -15.69011261309027638 ) ) ;
#77098 = CARTESIAN_POINT ( 'NONE',  ( 147.3026092797766182, 275.5113919703970851, -0.02371565180376775453 ) ) ;
#77099 = CARTESIAN_POINT ( 'NONE',  ( 147.1034852426517148, 275.8562849197056153, -3.648177088342072327 ) ) ;
#77100 = DIRECTION ( 'NONE',  ( -0.5000000000000003331, 0.8660254037844383745, 0.000000000000000000 ) ) ;
#77101 = CARTESIAN_POINT ( 'NONE',  ( 71.69982436666802528, 70.81612773607918143, 5.925385826462316707 ) ) ;
#77102 = DIRECTION ( 'NONE',  ( -0.7440200784635719877, -0.6681572590663519273, 0.000000000000000000 ) ) ;
#77103 = CARTESIAN_POINT ( 'NONE',  ( 67.03549487444914234, 66.88278970582167915, 8.847049729461536671 ) ) ;
#77104 = CARTESIAN_POINT ( 'NONE',  ( 74.73315994561023956, 64.49924696742777996, -14.01681635444520957 ) ) ;
#77105 = CARTESIAN_POINT ( 'NONE',  ( 78.15103970674991274, 47.75416819384486899, 13.96761498558048231 ) ) ;
#77106 = EDGE_LOOP ( 'NONE', ( #13402, #44307, #33232, #61226 ) ) ;
#77107 = CARTESIAN_POINT ( 'NONE',  ( 149.7004146199789147, 271.3582712945064941, -12.74589670383119433 ) ) ;
#77108 = CARTESIAN_POINT ( 'NONE',  ( 19.31801425620940194, 115.5650415295850451, 20.00000000000000355 ) ) ;
#77109 = CARTESIAN_POINT ( 'NONE',  ( 87.71125355519491507, 45.00661457325054471, -6.624481356856373182 ) ) ;
#77110 = CARTESIAN_POINT ( 'NONE',  ( 79.08373359491760368, 46.13869499162948529, 12.70867304314121604 ) ) ;
#77111 = CARTESIAN_POINT ( 'NONE',  ( 180.6066648745947134, 283.7006809008031496, -16.18202752516933174 ) ) ;
#77112 = CARTESIAN_POINT ( 'NONE',  ( 82.35285118013293015, 53.50770157854819331, -15.77620284334257938 ) ) ;
#77113 = CARTESIAN_POINT ( 'NONE',  ( 168.7558045253416310, 286.1749812365729326, -7.730637050109386621 ) ) ;
#77114 = EDGE_LOOP ( 'NONE', ( #60847, #69726, #97671, #51945 ) ) ;
#77115 = CARTESIAN_POINT ( 'NONE',  ( 163.1369207721744772, 248.0855599626920593, -11.24692769914530110 ) ) ;
#77116 = B_SPLINE_CURVE_WITH_KNOTS ( 'NONE', 3,
 ( #5809, #34710, #35713, #59485, #66612, #80878, #26626, #44298, #74742, #82370, #96564, #51407, #98028, #90467 ),
 .UNSPECIFIED., .F., .F.,
 ( 4, 2, 2, 2, 2, 2, 4 ),
 ( 0.0002339632422484184916, 0.0009086598472604706872, 0.001246008149766496785, 0.001414682301019510972, 0.001499019376646056230, 0.001541187914459328859, 0.001583356452272601488 ),
 .UNSPECIFIED. ) ;
#77117 = CARTESIAN_POINT ( 'NONE',  ( 72.14394712234364704, 71.70061920742823247, 5.492383471420795082 ) ) ;
#77118 = CARTESIAN_POINT ( 'NONE',  ( 39.33606980327277824, 193.5177522451418781, -10.00000000000009592 ) ) ;
#77119 = CARTESIAN_POINT ( 'NONE',  ( 130.8370663736463655, 246.3458772461660544, 9.188101187500095079 ) ) ;
#77120 = CARTESIAN_POINT ( 'NONE',  ( 180.3598775736073776, 294.8113545327539669, -3.562513127318830186 ) ) ;
#77121 = CARTESIAN_POINT ( 'NONE',  ( 108.6384560342674064, 221.9824982072973967, 3.021315404115420679E-15 ) ) ;
#77122 = CARTESIAN_POINT ( 'NONE',  ( 157.3363371328520088, 258.1324655395517311, 18.24585617226787093 ) ) ;
#77123 = FACE_OUTER_BOUND ( 'NONE', #42687, .T. ) ;
#77124 = CARTESIAN_POINT ( 'NONE',  ( 54.03161192339643293, 195.8768266524159856, -9.188101187500091527 ) ) ;
#77125 = AXIS2_PLACEMENT_3D ( 'NONE', #97816, #5100, #59777 ) ;
#77126 = CARTESIAN_POINT ( 'NONE',  ( 178.7926337964088361, 291.8428451618758572, -5.965102354984807675 ) ) ;
#77128 = LINE ( 'NONE', #81918, #100146 ) ;
#77127 = AXIS2_PLACEMENT_3D ( 'NONE', #56761, #33991, #95823 ) ;
#77129 = VERTEX_POINT ( 'NONE', #13127 ) ;
#77130 = CARTESIAN_POINT ( 'NONE',  ( 70.37934122712871954, 61.23818324669216651, 14.28954007458889386 ) ) ;
#77131 = CARTESIAN_POINT ( 'NONE',  ( 87.63170318219837895, 44.36446170533411504, -4.079950490519347106 ) ) ;
#77132 = B_SPLINE_SURFACE_WITH_KNOTS ( 'NONE', 3, 1, ( 
 ( #5127, #97351 ),
 ( #27915, #12237 ),
 ( #73537, #42118 ),
 ( #3644, #96367 ),
 ( #4119, #35014 ),
 ( #43096, #74038 ),
 ( #65914, #82171 ),
 ( #74550, #35521 ),
 ( #96871, #58314 ),
 ( #4627, #58799 ),
 ( #12747, #36008 ),
 ( #53691, #67918 ),
 ( #30409, #59802 ),
 ( #60288, #28929 ),
 ( #6113, #76999 ),
 ( #83658, #92262 ),
 ( #98838, #5616 ),
 ( #51733, #60781 ),
 ( #7607, #84647 ),
 ( #22811, #61300 ),
 ( #37008, #69411 ),
 ( #22308, #38494 ),
 ( #91747, #29419 ),
 ( #45594, #91248 ),
 ( #83151, #21811 ),
 ( #90772, #76523 ),
 ( #15189, #46088 ),
 ( #52697, #22 ),
 ( #59289, #13241 ),
 ( #52201, #53211 ),
 ( #14710, #99331 ),
 ( #90268, #44593 ),
 ( #20841, #82675 ),
 ( #21322, #44095 ) ),
 .UNSPECIFIED., .T., .F., .F.,
 ( 4, 2, 2, 2, 2, 2, 2, 2, 2, 2, 2, 2, 2, 2, 2, 2, 4 ),
 ( 2, 2 ),
 ( 0.000000000000000000, 0.06250000000000000000, 0.1250000000000000000, 0.1875000000000000000, 0.2500000000000000000, 0.3125000000000000000, 0.3750000000000000000, 0.4375000000000000000, 0.5000000000000000000, 0.5625000000000000000, 0.6250000000000000000, 0.6875000000000000000, 0.7500000000000000000, 0.8125000000000000000, 0.8750000000000000000, 0.9375000000000000000, 1.000000000000000000 ),
 ( 0.000000000000000000, 1.000000000000000000 ),
 .UNSPECIFIED. ) ;
#77133 = DIRECTION ( 'NONE',  ( -1.000000000000000000, 0.000000000000000000, -0.000000000000000000 ) ) ;
#77134 = VECTOR ( 'NONE', #27034, 1000.000000000000000 ) ;
#77135 = FACE_OUTER_BOUND ( 'NONE', #53991, .T. ) ;
#77136 = DIRECTION ( 'NONE',  ( -0.5609510170580174204, -0.8278489937552475642, 0.000000000000000000 ) ) ;
#77137 = CARTESIAN_POINT ( 'NONE',  ( 206.9985020284622408, 270.1150727264914053, 3.388313042214953441 ) ) ;
#77138 = CARTESIAN_POINT ( 'NONE',  ( 16.02555268474166539, 173.3927522451417929, -10.00000000000009237 ) ) ;
#77139 = CARTESIAN_POINT ( 'NONE',  ( 101.6898988757523625, 229.5177522451418781, -10.00000000000009592 ) ) ;
#77140 = CARTESIAN_POINT ( 'NONE',  ( 41.50249547274756878, 124.4848494355456836, 10.00000000000000000 ) ) ;
#77141 = ORIENTED_EDGE ( 'NONE', *, *, #53901, .T. ) ;
#77142 = B_SPLINE_CURVE_WITH_KNOTS ( 'NONE', 3,
 ( #34162, #49851, #57945, #65054 ),
 .UNSPECIFIED., .F., .F.,
 ( 4, 4 ),
 ( 0.02967357326668309050, 0.03879524988894693383 ),
 .UNSPECIFIED. ) ;
#77143 = ADVANCED_FACE ( 'NONE', ( #81549 ), #90147, .T. ) ;
#77144 = CARTESIAN_POINT ( 'NONE',  ( 189.8314329296643450, 301.8493086226544619, -0.8085564604676659384 ) ) ;
#77145 = CARTESIAN_POINT ( 'NONE',  ( 153.9562949345533980, 264.3674845922398049, 16.52332238502633288 ) ) ;
#77146 = AXIS2_PLACEMENT_3D ( 'NONE', #100078, #83403, #83909 ) ;
#77147 = CARTESIAN_POINT ( 'NONE',  ( 28.53781555160951555, 187.2833772461660544, -9.188101187500095079 ) ) ;
#77148 = CARTESIAN_POINT ( 'NONE',  ( 18.69751666607634988, 11.76426979415088958, 3.090169943749476733 ) ) ;
#77149 = AXIS2_PLACEMENT_3D ( 'NONE', #65393, #73506, #4090 ) ;
#77150 = CARTESIAN_POINT ( 'NONE',  ( 192.1381319048448972, 272.2822842022381451, 14.66302914414172776 ) ) ;
#77151 = CARTESIAN_POINT ( 'NONE',  ( 32.93109025799825673, 196.4865022471903160, -10.00000000000009592 ) ) ;
#77152 = B_SPLINE_CURVE_WITH_KNOTS ( 'NONE', 3,
 ( #15820, #633, #1139, #48747 ),
 .UNSPECIFIED., .F., .F.,
 ( 4, 4 ),
 ( 0.000000000000000000, 0.1732562812666568475 ),
 .UNSPECIFIED. ) ;
#77153 = FACE_OUTER_BOUND ( 'NONE', #813, .T. ) ;
#77155 = CARTESIAN_POINT ( 'NONE',  ( 76.25066296318219372, 205.6423013555409796, -4.594050593750043987 ) ) ;
#77154 = CARTESIAN_POINT ( 'NONE',  ( 194.9277292273816329, 275.2606802342018568, -15.65310477115430032 ) ) ;
#77156 = CARTESIAN_POINT ( 'NONE',  ( 200.3765029811139584, 283.5847115241710981, 16.85207472104531590 ) ) ;
#77157 = CARTESIAN_POINT ( 'NONE',  ( 72.61990804881321537, 57.19017774089424222, 16.35758357749855207 ) ) ;
#77158 = EDGE_CURVE ( 'NONE', #43692, #15769, #12118, .T. ) ;
#77159 = CARTESIAN_POINT ( 'NONE',  ( -30.22909824404765899, 96.62485709217924068, 44.59310059583850716 ) ) ;
#77160 = CARTESIAN_POINT ( 'NONE',  ( 66.51309011095609947, 68.84183934625441736, -4.405043755099953273 ) ) ;
#77161 = ORIENTED_EDGE ( 'NONE', *, *, #8362, .T. ) ;
#77162 = AXIS2_PLACEMENT_3D ( 'NONE', #24365, #55237, #94795 ) ;
#77163 = EDGE_CURVE ( 'NONE', #79381, #25119, #35340, .T. ) ;
#77164 = CARTESIAN_POINT ( 'NONE',  ( 26.50806851326369440, 186.1115022471902591, 10.00000000000009592 ) ) ;
#77165 = CARTESIAN_POINT ( 'NONE',  ( 163.7587049410067266, 247.0085981909329576, -6.137518685179130351 ) ) ;
#77166 = CARTESIAN_POINT ( 'NONE',  ( -12.05712525078605069, 163.8458772461660544, 9.188101187500095079 ) ) ;
#77167 = CARTESIAN_POINT ( 'NONE',  ( 25.99623195869281744, 35.98502408145594700, -5.678558825948271327 ) ) ;
#77168 = CARTESIAN_POINT ( 'NONE',  ( 185.2932492178748873, 260.3554632076975963, 6.449134693235576421 ) ) ;
#77169 = CARTESIAN_POINT ( 'NONE',  ( 164.7297297678022403, 245.3267338555121455, 3.020078936458732599 ) ) ;
#77171 = FACE_OUTER_BOUND ( 'NONE', #33848, .T. ) ;
#77170 = CARTESIAN_POINT ( 'NONE',  ( 67.66477494612622934, 65.93994996590180335, 10.43000742999573838 ) ) ;
#77172 = CARTESIAN_POINT ( 'NONE',  ( 66.21400821115226165, 68.61137286571008076, 2.321765048532279163 ) ) ;
#77173 = VERTEX_POINT ( 'NONE', #14109 ) ;
#77174 = DIRECTION ( 'NONE',  ( 1.000000000000000000, 3.548748596569695807E-14, 0.000000000000000000 ) ) ;
#77175 = CARTESIAN_POINT ( 'NONE',  ( 177.8222571804544430, 286.5223583772871621, 13.77940225188420875 ) ) ;
#77176 = CARTESIAN_POINT ( 'NONE',  ( 156.0333632674501700, 279.4506186462613755, -5.256414494794261927 ) ) ;
#77177 = CARTESIAN_POINT ( 'NONE',  ( 13.03712377304622194, 16.03085787977761356, 9.188101187500006262 ) ) ;
#77178 = ORIENTED_EDGE ( 'NONE', *, *, #66634, .F. ) ;
#77179 = CARTESIAN_POINT ( 'NONE',  ( 206.7942001012778235, 272.4689340444584786, 9.528356049623848634 ) ) ;
#77180 = CARTESIAN_POINT ( 'NONE',  ( 75.58214075417596689, 65.23491603964200181, 14.35294216029142333 ) ) ;
#77181 = CARTESIAN_POINT ( 'NONE',  ( 204.9463377925012253, 275.6695254486514841, -14.15865086131798378 ) ) ;
#77182 = CARTESIAN_POINT ( 'NONE',  ( 148.7536333930846979, 273.6080040564672231, -8.868003689723101601 ) ) ;
#77183 = CARTESIAN_POINT ( 'NONE',  ( -97.59541525468981149, 48.06504152958505216, 36.50000000000000000 ) ) ;
#77184 = LINE ( 'NONE', #46262, #39578 ) ;
#77185 = CARTESIAN_POINT ( 'NONE',  ( 162.8480293090835005, 248.5859346546387769, -9.753154585358942086 ) ) ;
#77186 = CARTESIAN_POINT ( 'NONE',  ( 201.0732166862245549, 282.3779679885897167, -18.18766936363638820 ) ) ;
#77187 = ORIENTED_EDGE ( 'NONE', *, *, #28573, .T. ) ;
#77188 = ORIENTED_EDGE ( 'NONE', *, *, #56694, .T. ) ;
#77189 = EDGE_CURVE ( 'NONE', #20145, #8322, #29314, .T. ) ;
#77190 = CARTESIAN_POINT ( 'NONE',  ( 190.6023296602558901, 281.3493246229567717, 16.84671144084375172 ) ) ;
#77191 = CARTESIAN_POINT ( 'NONE',  ( 72.63381747954645107, 70.76794473758097581, 7.135479174949443504 ) ) ;
#77192 = ORIENTED_EDGE ( 'NONE', *, *, #77877, .F. ) ;
#77193 = CARTESIAN_POINT ( 'NONE',  ( 149.1903793729515257, 272.2416782560088677, 12.95958987445043675 ) ) ;
#77194 = CARTESIAN_POINT ( 'NONE',  ( 68.74550570596571220, 65.29344765021964747, 11.68071900121614526 ) ) ;
#77195 = CARTESIAN_POINT ( 'NONE',  ( 83.96921505230092464, 45.18285929837890080, -9.373418216583857543 ) ) ;
#77196 = EDGE_LOOP ( 'NONE', ( #59639, #57051, #35632, #73598 ) ) ;
#77197 = CARTESIAN_POINT ( 'NONE',  ( 191.2211340522693774, 299.4422756709672626, -8.405362570633277741 ) ) ;
#77198 = CARTESIAN_POINT ( 'NONE',  ( 79.52267089340274708, 59.39869781967021112, -16.20969956878131413 ) ) ;
#77199 = EDGE_CURVE ( 'NONE', #20907, #84697, #49815, .T. ) ;
#77200 = CARTESIAN_POINT ( 'NONE',  ( 8.162811221194553823, 28.21091486745858745, -1.111400068045478839E-16 ) ) ;
#77201 = DIRECTION ( 'NONE',  ( 0.8074371744834156761, 0.5899535653441194683, 0.000000000000000000 ) ) ;
#77202 = CIRCLE ( 'NONE', #90192, 1.449999999999994627 ) ;
#77203 = CARTESIAN_POINT ( 'NONE',  ( 69.68191272334148323, 62.54370116513975830, 13.40392498406904842 ) ) ;
#77204 = ORIENTED_EDGE ( 'NONE', *, *, #46654, .T. ) ;
#77205 = CARTESIAN_POINT ( 'NONE',  ( 97.73839765093606502, 236.4244531367911009, -4.594050593750046652 ) ) ;
#77206 = CARTESIAN_POINT ( 'NONE',  ( 155.7553667887436859, 260.8707865008068438, 18.13952515356204032 ) ) ;
#77207 = VECTOR ( 'NONE', #96688, 1000.000000000000000 ) ;
#77208 = CARTESIAN_POINT ( 'NONE',  ( 73.20181606317161993, 69.60992630376679813, -9.900803345273253342 ) ) ;
#77209 = CARTESIAN_POINT ( 'NONE',  ( 191.0170959869219303, 299.7956799668270946, 7.353346939903929069 ) ) ;
#77210 = LINE ( 'NONE', #23488, #47721 ) ;
#77211 = ORIENTED_EDGE ( 'NONE', *, *, #19298, .F. ) ;
#77212 = ADVANCED_FACE ( 'NONE', ( #44990 ), #21220, .T. ) ;
#77213 = VERTEX_POINT ( 'NONE', #52099 ) ;
#77214 = ORIENTED_EDGE ( 'NONE', *, *, #97028, .F. ) ;
#77215 = CARTESIAN_POINT ( 'NONE',  ( 73.39810145532288743, 61.39966270044930496, 14.96885843746143152 ) ) ;
#77216 = ORIENTED_EDGE ( 'NONE', *, *, #14840, .F. ) ;
#77217 = CARTESIAN_POINT ( 'NONE',  ( 160.0499875548515263, 257.7887348395778986, -17.19135428511508579 ) ) ;
#77218 = VERTEX_POINT ( 'NONE', #73920 ) ;
#77219 = CARTESIAN_POINT ( 'NONE',  ( 208.2777459429579210, 269.8993572713111462, 3.129643751043610589 ) ) ;
#77220 = AXIS2_PLACEMENT_3D ( 'NONE', #26796, #81050, #26304 ) ;
#77221 = CARTESIAN_POINT ( 'NONE',  ( 82.84292370591116139, 47.81104087607728559, 12.42676687899641230 ) ) ;
#77222 = CARTESIAN_POINT ( 'NONE',  ( 171.0295563763983751, 283.5921888939291193, 12.22847014256639042 ) ) ;
#77223 = CARTESIAN_POINT ( 'NONE',  ( 194.2900850603946310, 294.1266965989547657, -15.88613936555681505 ) ) ;
#77224 = CARTESIAN_POINT ( 'NONE',  ( 82.72605847261863232, 53.97080330652735825, -15.84526420522619894 ) ) ;
#77225 = PLANE ( 'NONE',  #70630 ) ;
#77226 = CARTESIAN_POINT ( 'NONE',  ( 11.72364552993787967, 24.95586893147754282, 7.433330006724141015 ) ) ;
#77227 = DIRECTION ( 'NONE',  ( -0.8660254037844387076, -0.4999999999999998890, -0.000000000000000000 ) ) ;
#77228 = CARTESIAN_POINT ( 'NONE',  ( 80.10302014060799536, 57.75140007922346541, 16.60262925785714216 ) ) ;
#77230 = VERTEX_POINT ( 'NONE', #13617 ) ;
#77229 = CARTESIAN_POINT ( 'NONE',  ( 200.2093391412865060, 269.7417714514684803, 10.46510648850140157 ) ) ;
#77231 = AXIS2_PLACEMENT_3D ( 'NONE', #28276, #13106, #35381 ) ;
#77232 = CARTESIAN_POINT ( 'NONE',  ( 170.6243390796742858, 258.8588259563213683, -13.92090666709099622 ) ) ;
#77233 = CARTESIAN_POINT ( 'NONE',  ( 206.8313602288537538, 272.4045708154811791, -9.607337080360906612 ) ) ;
#77234 = CARTESIAN_POINT ( 'NONE',  ( 77.30113122908805678, 49.12792392959498500, -15.30166374384701911 ) ) ;
#77235 = CARTESIAN_POINT ( 'NONE',  ( 80.61151161062586823, 46.19852708120087215, -12.13081066922774731 ) ) ;
#77236 = EDGE_CURVE ( 'NONE', #31865, #70938, #44490, .T. ) ;
#77237 = CARTESIAN_POINT ( 'NONE',  ( 171.9118178377493109, 254.7376308715724633, 11.11564670839499769 ) ) ;
#77238 = CARTESIAN_POINT ( 'NONE',  ( 157.9648847355622650, 281.0502099387495605, 1.885049730135211821 ) ) ;
#77239 = VERTEX_POINT ( 'NONE', #4505 ) ;
#77240 = CARTESIAN_POINT ( 'NONE',  ( 155.6699570996827617, 261.0187204217189674, -17.22644539015238863 ) ) ;
#77241 = AXIS2_PLACEMENT_3D ( 'NONE', #56859, #18892, #95924 ) ;
#77242 = DIRECTION ( 'NONE',  ( 0.1473778574936430164, 0.9890802632347809320, 0.000000000000000000 ) ) ;
#77244 = ADVANCED_FACE ( 'NONE', ( #97245 ), #27811, .T. ) ;
#77243 = LINE ( 'NONE', #69635, #79117 ) ;
#77245 = CARTESIAN_POINT ( 'NONE',  ( 10.82940026203503336, 170.3927522451418213, -10.00000000000009059 ) ) ;
#77246 = CARTESIAN_POINT ( 'NONE',  ( 93.16496130902324069, 224.5958772461660260, -9.188101187500095079 ) ) ;
#77247 = CARTESIAN_POINT ( 'NONE',  ( 192.8095291656202619, 267.1346876124251253, -11.12116723929773698 ) ) ;
#77248 = DIRECTION ( 'NONE',  ( -0.8393827800519415572, -0.5435407515102007592, 0.000000000000000000 ) ) ;
#77249 = CARTESIAN_POINT ( 'NONE',  ( 203.4661181658017597, 278.2333410484554861, -14.92553451795532204 ) ) ;
#77250 = CARTESIAN_POINT ( 'NONE',  ( 72.41389820116259557, 70.72247311216293042, 7.745007521649655224 ) ) ;
#77252 = CARTESIAN_POINT ( 'NONE',  ( 26.14792707536646432, 33.83478043621389020, -8.090169943749479842 ) ) ;
#77251 = CARTESIAN_POINT ( 'NONE',  ( 11.32556065139379875, 177.3458772461660544, 9.188101187500095079 ) ) ;
#77253 = CARTESIAN_POINT ( 'NONE',  ( 161.8948331661419218, 250.2369188037922356, 13.64419044796309777 ) ) ;
#77254 = EDGE_LOOP ( 'NONE', ( #97987, #3461, #18428, #12046 ) ) ;
#77255 = ORIENTED_EDGE ( 'NONE', *, *, #8799, .F. ) ;
#77256 = CARTESIAN_POINT ( 'NONE',  ( 161.3981413584396876, 253.0972142504356270, -15.11937522241654719 ) ) ;
#77257 = CARTESIAN_POINT ( 'NONE',  ( 198.2712628870943661, 265.0502820922010869, -3.032086182221595649 ) ) ;
#77258 = CARTESIAN_POINT ( 'NONE',  ( 83.11954624601993658, 46.44810582658406872, -11.20842123171843596 ) ) ;
#77259 = CARTESIAN_POINT ( 'NONE',  ( 205.2660270307054304, 275.1158074454486382, -13.97598661256119179 ) ) ;
#77260 = CARTESIAN_POINT ( 'NONE',  ( 80.74781574657598071, 57.21644485803223290, 16.56566952311892749 ) ) ;
#77261 = DIRECTION ( 'NONE',  ( -0.8450603975019854719, 0.5346708562973919721, 0.000000000000000000 ) ) ;
#77262 = CARTESIAN_POINT ( 'NONE',  ( 149.6449510338218829, 277.3920198197748164, 3.114130954607317925 ) ) ;
#77263 = CARTESIAN_POINT ( 'NONE',  ( 15.54743449484293372, 179.7833772461660544, -9.188101187500095079 ) ) ;
#77264 = CARTESIAN_POINT ( 'NONE',  ( 114.1117772151768577, 242.8149278399161233, -9.188101187500095079 ) ) ;
#77265 = CARTESIAN_POINT ( 'NONE',  ( 181.9627339888420465, 294.6573541485591932, -6.516454160791068873 ) ) ;
#77266 = CARTESIAN_POINT ( 'NONE',  ( 183.1055844247790958, 257.7654091154714706, -2.368402100318311110 ) ) ;
#77267 = ORIENTED_EDGE ( 'NONE', *, *, #83014, .F. ) ;
#77268 = CARTESIAN_POINT ( 'NONE',  ( 153.2819058590468160, 274.2512448977743134, -12.24885634829186287 ) ) ;
#77269 = DIRECTION ( 'NONE',  ( -0.5000000000000013323, 0.8660254037844380415, 0.000000000000000000 ) ) ;
#77270 = CARTESIAN_POINT ( 'NONE',  ( 151.7685526703961614, 270.8433852370800423, 14.21420454866266248 ) ) ;
#77271 = CARTESIAN_POINT ( 'NONE',  ( 157.3988263959001870, 258.0242309610243865, 16.72376558639979294 ) ) ;
#77272 = VECTOR ( 'NONE', #99861, 999.9999999999998863 ) ;
#77273 = CARTESIAN_POINT ( 'NONE',  ( 155.0197698005585494, 262.1448778582381465, 18.42918111182112284 ) ) ;
#77274 = CARTESIAN_POINT ( 'NONE',  ( 161.0974665087481981, 251.6179983666593216, -13.69252715295363210 ) ) ;
#77275 = CARTESIAN_POINT ( 'NONE',  ( 189.4308808934198680, 289.8491723414206831, 15.72891001903047048 ) ) ;
#77276 = CARTESIAN_POINT ( 'NONE',  ( 147.6264044922760377, 274.9505622111005323, -8.841872555777701592 ) ) ;
#77277 = CARTESIAN_POINT ( 'NONE',  ( 189.3717192525180337, 262.4809367720384898, 8.181044353032417504 ) ) ;
#77278 = CARTESIAN_POINT ( 'NONE',  ( 164.2214870300199152, 249.7080052763175217, -10.41861459481195595 ) ) ;
#77279 = DIRECTION ( 'NONE',  ( -0.8660254037844387076, -0.4999999999999998890, -0.000000000000000000 ) ) ;
#77280 = EDGE_CURVE ( 'NONE', #60835, #17038, #48631, .T. ) ;
#77281 = CARTESIAN_POINT ( 'NONE',  ( 69.15337702377902929, 69.07843188401378143, 6.265891433177522174 ) ) ;
#77282 = CARTESIAN_POINT ( 'NONE',  ( 147.6618183892331331, 274.8892235422768522, 8.990680574201936892 ) ) ;
#77283 = DIRECTION ( 'NONE',  ( 0.8080546441192343332, -0.5891075386695857619, 0.000000000000000000 ) ) ;
#77284 = VERTEX_POINT ( 'NONE', #37880 ) ;
#77285 = CARTESIAN_POINT ( 'NONE',  ( 152.3599525993681709, 267.1668075756145981, -15.39918555524012334 ) ) ;
#77286 = ADVANCED_FACE ( 'NONE', ( #84053 ), #31266, .F. ) ;
#77287 = CIRCLE ( 'NONE', #74050, 70.00000000000001421 ) ;
#77289 = ADVANCED_FACE ( 'NONE', ( #65198 ), #55576, .T. ) ;
#77288 = CARTESIAN_POINT ( 'NONE',  ( 185.1220358696202481, 269.6591034785776628, 15.69820767156324770 ) ) ;
#77290 = ADVANCED_FACE ( 'NONE', ( #73311 ), #80447, .T. ) ;
#77291 = CARTESIAN_POINT ( 'NONE',  ( 94.43719644265542001, 216.1423013555410080, -4.594050593750043987 ) ) ;
#77292 = CARTESIAN_POINT ( 'NONE',  ( 19.52749640002317122, 16.98920272979925628, 7.433330006724137462 ) ) ;
#77293 = CARTESIAN_POINT ( 'NONE',  ( 150.6571681785161445, 269.7011255207979730, 15.24894850018880454 ) ) ;
#77294 = CARTESIAN_POINT ( 'NONE',  ( 80.59739948449713154, 56.56319013636019832, -16.53599074302314165 ) ) ;
#77295 = VECTOR ( 'NONE', #82728, 1000.000000000000000 ) ;
#77297 = CARTESIAN_POINT ( 'NONE',  ( 195.2484836900998175, 279.0356495040737173, 16.29341914179182282 ) ) ;
#77296 = CARTESIAN_POINT ( 'NONE',  ( 145.1275483969982645, 243.0494855054051584, -2.679491924311248496 ) ) ;
#77298 = CARTESIAN_POINT ( 'NONE',  ( 176.6943099527350682, 256.7931168052207340, -11.17617521364210731 ) ) ;
#77299 = CARTESIAN_POINT ( 'NONE',  ( 74.14312167556930433, 66.30466486950707861, 1.224646799147354045E-15 ) ) ;
#77300 = CARTESIAN_POINT ( 'NONE',  ( -19.65312891409030271, 93.06504152958497400, 10.00000000000000888 ) ) ;
#77301 = CARTESIAN_POINT ( 'NONE',  ( 47.72569090598240393, 208.3615022471902876, 5.000000000000046185 ) ) ;
#77302 = DIRECTION ( 'NONE',  ( -1.000000000000000000, 0.000000000000000000, 0.000000000000000000 ) ) ;
#77303 = CARTESIAN_POINT ( 'NONE',  ( 28.46864935082047410, 149.7156766241961350, 37.50000000000000000 ) ) ;
#77304 = ORIENTED_EDGE ( 'NONE', *, *, #5915, .F. ) ;
#77305 = CARTESIAN_POINT ( 'NONE',  ( 192.4264036352439575, 266.3794008020136630, 11.60644757818683637 ) ) ;
#77306 = CARTESIAN_POINT ( 'NONE',  ( 33.66714878060290772, 21.29860640527294180, -2.839279412974138328 ) ) ;
#77307 = CARTESIAN_POINT ( 'NONE',  ( 69.85984440804038798, 64.57025534319816984, -12.75834560728216616 ) ) ;
#77308 = CARTESIAN_POINT ( 'NONE',  ( 82.10359218643519341, 52.07680853587788050, 15.36587509554532538 ) ) ;
#77309 = LINE ( 'NONE', #5912, #20213 ) ;
#77310 = CARTESIAN_POINT ( 'NONE',  ( 153.1548001820517868, 274.9824320604590184, 10.64421219061565793 ) ) ;
#77311 = CARTESIAN_POINT ( 'NONE',  ( 30.13368333964083590, 79.01311634467327849, 59.99999999999999289 ) ) ;
#77312 = CARTESIAN_POINT ( 'NONE',  ( 190.6688270659779221, 284.0946164064107506, -17.60360843008351495 ) ) ;
#77313 = CARTESIAN_POINT ( 'NONE',  ( 72.37415438388894984, 71.90064624941815907, -5.324036893254605829 ) ) ;
#77314 = CARTESIAN_POINT ( 'NONE',  ( 74.90236252610125689, 53.33673484778374529, -16.52890225279428549 ) ) ;
#77315 = CARTESIAN_POINT ( 'NONE',  ( 192.0331311261993790, 298.0358554833232461, 11.82583305898340953 ) ) ;
#77316 = VECTOR ( 'NONE', #88175, 1000.000000000000114 ) ;
#77317 = ORIENTED_EDGE ( 'NONE', *, *, #98920, .F. ) ;
#77318 = EDGE_CURVE ( 'NONE', #47320, #99135, #71609, .T. ) ;
#77319 = CARTESIAN_POINT ( 'NONE',  ( 73.63435323750927353, 69.71791780730768551, 10.06421556446032461 ) ) ;
#77320 = CARTESIAN_POINT ( 'NONE',  ( 34.33172647011804912, 40.79752408145593989, -5.678558825948271327 ) ) ;
#77321 = ORIENTED_EDGE ( 'NONE', *, *, #44572, .T. ) ;
#77322 = CARTESIAN_POINT ( 'NONE',  ( 165.1852812139168520, 248.1429326983447652, 7.096218362256309753 ) ) ;
#77323 = CARTESIAN_POINT ( 'NONE',  ( 85.04793144752866851, 49.76842598555752772, 13.42690168825988550 ) ) ;
#77324 = VERTEX_POINT ( 'NONE', #40874 ) ;
#77325 = CARTESIAN_POINT ( 'NONE',  ( 86.25376498619890242, 46.94328282020536136, -10.55339115541321604 ) ) ;
#77326 = CARTESIAN_POINT ( 'NONE',  ( 159.0577544183932446, 255.1508833399667253, 16.37810164263070334 ) ) ;
#77327 = CARTESIAN_POINT ( 'NONE',  ( 84.49275162666286576, 50.19829916693547744, 13.87667126673719231 ) ) ;
#77328 = CARTESIAN_POINT ( 'NONE',  ( 153.4436003264302144, 264.8748834687675071, -16.72600001480972765 ) ) ;
#77329 = DIRECTION ( 'NONE',  ( 0.000000000000000000, 0.000000000000000000, 1.000000000000000000 ) ) ;
#77330 = DIRECTION ( 'NONE',  ( -0.000000000000000000, -0.000000000000000000, -1.000000000000000000 ) ) ;
#77331 = CARTESIAN_POINT ( 'NONE',  ( 80.02357168100483875, 44.69250730557818940, 11.14898322769941608 ) ) ;
#77332 = CARTESIAN_POINT ( 'NONE',  ( 81.25101512611533394, 55.44295246005403754, -16.34115372143416778 ) ) ;
#77333 = B_SPLINE_CURVE_WITH_KNOTS ( 'NONE', 3,
 ( #27138, #26133, #58023, #56519 ),
 .UNSPECIFIED., .F., .F.,
 ( 4, 4 ),
 ( 0.008310172455301832045, 0.01464027962821165887 ),
 .UNSPECIFIED. ) ;
#77334 = ORIENTED_EDGE ( 'NONE', *, *, #54639, .T. ) ;
#77335 = DIRECTION ( 'NONE',  ( -0.8660254037844387076, -0.4999999999999998890, -0.000000000000000000 ) ) ;
#77336 = ORIENTED_EDGE ( 'NONE', *, *, #5156, .F. ) ;
#77337 = VERTEX_POINT ( 'NONE', #41384 ) ;
#77338 = CARTESIAN_POINT ( 'NONE',  ( 87.22262286821016630, 46.01322853962243897, -8.753954545221112937 ) ) ;
#77339 = ORIENTED_EDGE ( 'NONE', *, *, #52208, .F. ) ;
#77340 = FACE_OUTER_BOUND ( 'NONE', #56111, .T. ) ;
#77341 = CARTESIAN_POINT ( 'NONE',  ( 30.91633199877554716, 29.80066082961423746, 10.00000000000000533 ) ) ;
#77342 = CARTESIAN_POINT ( 'NONE',  ( 154.9032082715209810, 280.6326124547101699, -2.389722542998433230 ) ) ;
#77343 = CYLINDRICAL_SURFACE ( 'NONE', #78819, 70.00000000000002842 ) ;
#77344 = CARTESIAN_POINT ( 'NONE',  ( 82.33563566117209120, 40.89915267565207557, 1.012059201927479224 ) ) ;
#77345 = AXIS2_PLACEMENT_3D ( 'NONE', #88962, #66084, #51883 ) ;
#77347 = CARTESIAN_POINT ( 'NONE',  ( 167.6777283665894629, 249.2378510193953502, -5.459661846318103251 ) ) ;
#77346 = B_SPLINE_CURVE_WITH_KNOTS ( 'NONE', 3,
 ( #1557, #47128, #78051, #39509, #63338, #63835, #55705, #79080, #40523, #71458, #94773, #42516, #65819, #4034 ),
 .UNSPECIFIED., .F., .F.,
 ( 4, 2, 2, 2, 2, 2, 4 ),
 ( 0.001312137252800617574, 0.001526837886047112489, 0.001741538519293607404, 0.001956239152540102319, 0.002170939785786597017, 0.002600341052279644960, 0.003029742318772693337 ),
 .UNSPECIFIED. ) ;
#77348 = CARTESIAN_POINT ( 'NONE',  ( 54.65389413625798909, 192.3615022471901739, 5.000000000000051514 ) ) ;
#77349 = CARTESIAN_POINT ( 'NONE',  ( 183.5065578787086622, 284.7368108013639016, -15.01251262284198162 ) ) ;
#77350 = CARTESIAN_POINT ( 'NONE',  ( 112.6505328941731108, 235.8458772461660544, 9.188101187500095079 ) ) ;
#77351 = CARTESIAN_POINT ( 'NONE',  ( 183.5457472072443750, 260.5072762062756055, -9.285272734760553703 ) ) ;
#77352 = CARTESIAN_POINT ( 'NONE',  ( 36.41018743920069056, 41.99752408145594273, 5.678558825948277544 ) ) ;
#77353 = CARTESIAN_POINT ( 'NONE',  ( 177.3471610734995068, 288.7557762509717350, -9.520805881307069285 ) ) ;
#77355 = EDGE_CURVE ( 'NONE', #72111, #41570, #57909, .T. ) ;
#77354 = VECTOR ( 'NONE', #39603, 1000.000000000000000 ) ;
#77356 = ORIENTED_EDGE ( 'NONE', *, *, #28818, .F. ) ;
#77357 = AXIS2_PLACEMENT_3D ( 'NONE', #90971, #37701, #28618 ) ;
#77358 = VERTEX_POINT ( 'NONE', #26206 ) ;
#77359 = CARTESIAN_POINT ( 'NONE',  ( 73.89337880468768560, 68.29732366427398915, -11.63451623248603006 ) ) ;
#77360 = CARTESIAN_POINT ( 'NONE',  ( 75.83733595332329003, 62.71011828194265547, -15.04395063225968165 ) ) ;
#77361 = CARTESIAN_POINT ( 'NONE',  ( 164.4854433269806577, 246.2060377238486808, -1.879056492287135116 ) ) ;
#77362 = CARTESIAN_POINT ( 'NONE',  ( 157.2744851780909414, 258.2395962677452985, 18.17792129701959070 ) ) ;
#77363 = CARTESIAN_POINT ( 'NONE',  ( 73.34094528678892289, 66.77043691544750459, 12.11220508038992172 ) ) ;
#77364 = CARTESIAN_POINT ( 'NONE',  ( 152.7691010214056462, 266.0431505347400503, -16.40662330462167162 ) ) ;
#77365 = CARTESIAN_POINT ( 'NONE',  ( 177.1970037392277391, 288.7997655633063232, -9.298457205910423795 ) ) ;
#77366 = ORIENTED_EDGE ( 'NONE', *, *, #88200, .T. ) ;
#77367 = CARTESIAN_POINT ( 'NONE',  ( 50.18541494347880416, 88.31343213334855591, 177.5919119679930134 ) ) ;
#77368 = CARTESIAN_POINT ( 'NONE',  ( 175.4537718564577631, 254.8713487546767169, -7.339328112761260847 ) ) ;
#77369 = VECTOR ( 'NONE', #35914, 1000.000000000000000 ) ;
#77370 = ORIENTED_EDGE ( 'NONE', *, *, #50822, .F. ) ;
#77371 = CARTESIAN_POINT ( 'NONE',  ( 194.9636675848471441, 292.9600174435121289, -15.57898232594655319 ) ) ;
#77372 = LINE ( 'NONE', #60147, #18794 ) ;
#77373 = EDGE_LOOP ( 'NONE', ( #37849, #84106, #58859, #92120 ) ) ;
#77374 = MANIFOLD_SOLID_BREP ( 'Boss-Extrude13', #58778 ) ;
#77375 = CARTESIAN_POINT ( 'NONE',  ( 191.8392821121727536, 267.5768712655535637, -12.56012087630908169 ) ) ;
#77376 = AXIS2_PLACEMENT_3D ( 'NONE', #79773, #64024, #55397 ) ;
#77377 = CARTESIAN_POINT ( 'NONE',  ( 190.9710483804310854, 283.5610905854780981, -16.58407571954575488 ) ) ;
#77378 = CARTESIAN_POINT ( 'NONE',  ( 192.4246011695004768, 262.9676472730263868, 4.544249788418587954 ) ) ;
#77379 = CARTESIAN_POINT ( 'NONE',  ( -13.12676960854360786, 60.47780990635891385, -10.00000000000000000 ) ) ;
#77380 = CARTESIAN_POINT ( 'NONE',  ( 70.81620453278789284, 71.83147976216292818, -2.355153135381267582 ) ) ;
#77382 = CARTESIAN_POINT ( 'NONE',  ( 157.3376867920517554, 280.1474045426916177, 5.786264004936231942 ) ) ;
#77381 = CARTESIAN_POINT ( 'NONE',  ( 184.5344485499420273, 288.9945769638181901, -13.19104496679712213 ) ) ;
#77383 = CARTESIAN_POINT ( 'NONE',  ( 201.0468719883840265, 282.4235983437597497, -16.59631526626950659 ) ) ;
#77384 = VERTEX_POINT ( 'NONE', #56592 ) ;
#77385 = CARTESIAN_POINT ( 'NONE',  ( 190.9586609929293104, 299.8968923453624598, -4.970176667899034229 ) ) ;
#77387 = CARTESIAN_POINT ( 'NONE',  ( 168.3509053677366296, 264.6512997888990526, -17.59019591919307146 ) ) ;
#77386 = B_SPLINE_SURFACE_WITH_KNOTS ( 'NONE', 3, 1, ( 
 ( #88445, #80840 ),
 ( #58460, #27091 ),
 ( #87951, #42262 ),
 ( #96521, #26591 ),
 ( #11896, #50371 ),
 ( #33183, #72204 ),
 ( #27596, #35169 ),
 ( #3306, #80324 ),
 ( #89434, #33697 ),
 ( #95027, #19987 ),
 ( #56476, #34186 ),
 ( #17997, #96029 ),
 ( #57464, #73197 ),
 ( #50867, #48891 ),
 ( #64590, #64082 ),
 ( #42753, #57974 ),
 ( #88958, #18495 ),
 ( #10894, #79825 ),
 ( #10393, #4271 ),
 ( #41770, #19004 ),
 ( #41261, #66080 ),
 ( #3791, #97026 ),
 ( #2809, #95543 ),
 ( #49381, #26090 ),
 ( #6267, #98494 ),
 ( #43757, #82819 ),
 ( #45743, #60950 ),
 ( #53359, #58941 ),
 ( #12901, #90922 ),
 ( #75681, #5766 ),
 ( #20999, #97500 ),
 ( #36655, #75191 ),
 ( #66574, #67562 ),
 ( #29086, #21472 ) ),
 .UNSPECIFIED., .T., .F., .F.,
 ( 4, 2, 2, 2, 2, 2, 2, 2, 2, 2, 2, 2, 2, 2, 2, 2, 4 ),
 ( 2, 2 ),
 ( 0.000000000000000000, 0.06250000000000000000, 0.1250000000000000000, 0.1875000000000000000, 0.2500000000000000000, 0.3125000000000000000, 0.3750000000000000000, 0.4375000000000000000, 0.5000000000000000000, 0.5625000000000000000, 0.6250000000000000000, 0.6875000000000000000, 0.7500000000000000000, 0.8125000000000000000, 0.8750000000000000000, 0.9375000000000000000, 1.000000000000000000 ),
 ( 0.000000000000000000, 1.000000000000000000 ),
 .UNSPECIFIED. ) ;
#77388 = CARTESIAN_POINT ( 'NONE',  ( 187.0383423799210902, 262.1832919597250111, -8.674447465982201066 ) ) ;
#77389 = CARTESIAN_POINT ( 'NONE',  ( 182.6565686206717771, 276.0795042466008908, -16.45052173798808326 ) ) ;
#77390 = CARTESIAN_POINT ( 'NONE',  ( 87.83899792242847582, 44.00541668311378629, -1.848955303085625390 ) ) ;
#77391 = CARTESIAN_POINT ( 'NONE',  ( 192.8314823969449492, 271.7167918609114849, -14.83780806620786485 ) ) ;
#77392 = DIRECTION ( 'NONE',  ( -0.5000000000000019984, 0.8660254037844374864, 0.000000000000000000 ) ) ;
#77393 = CARTESIAN_POINT ( 'NONE',  ( 83.65644665907211674, 43.95837842834492903, 7.881347961145165115 ) ) ;
#77394 = CARTESIAN_POINT ( 'NONE',  ( 188.0775634319173832, 267.1413101313072502, 14.31780989748781252 ) ) ;
#77395 = CARTESIAN_POINT ( 'NONE',  ( 155.0929244053699847, 262.0181703658971628, 18.51426604808664678 ) ) ;
#77396 = CARTESIAN_POINT ( 'NONE',  ( 192.6881117187585062, 284.3071375317443881, -16.71636262633107606 ) ) ;
#77397 = CARTESIAN_POINT ( 'NONE',  ( 82.41797270617800564, 53.48512899883142779, -15.75897339677477582 ) ) ;
#77398 = CARTESIAN_POINT ( 'NONE',  ( 78.09096694622414248, 206.7048013555409796, 4.594050593750051981 ) ) ;
#77399 = CARTESIAN_POINT ( 'NONE',  ( 67.12731856515000572, 66.75179982629357767, 8.201365336552942864 ) ) ;
#77400 = CARTESIAN_POINT ( 'NONE',  ( 147.3236643320416022, 275.4749235501183193, -5.185334239426818037 ) ) ;
#77401 = CARTESIAN_POINT ( 'NONE',  ( 60.62040048720410823, 194.2592609112380160, 2.679491924311254714 ) ) ;
#77402 = CARTESIAN_POINT ( 'NONE',  ( 203.0498946958275326, 278.9542612457532869, -15.11479947333269003 ) ) ;
#77403 = B_SPLINE_CURVE_WITH_KNOTS ( 'NONE', 3,
 ( #9405, #76801, #16497, #77308, #54992, #38790, #69696, #85971, #301, #23582, #54474, #16000, #46899, #57997, #96542, #87485 ),
 .UNSPECIFIED., .F., .F.,
 ( 4, 1, 2, 2, 2, 1, 2, 2, 4 ),
 ( 0.000000000000000000, 0.1250000000000010547, 0.1875000000000025258, 0.2500000000000039968, 0.5000000000000062172, 0.6250000000000067724, 0.6875000000000056621, 0.7500000000000046629, 1.000000000000000000 ),
 .UNSPECIFIED. ) ;
#77404 = VECTOR ( 'NONE', #90779, 1000.000000000000114 ) ;
#77405 = CARTESIAN_POINT ( 'NONE',  ( 161.0974665087481981, 251.6179983666593216, -13.69252715295363210 ) ) ;
#77406 = CARTESIAN_POINT ( 'NONE',  ( 84.86723485156080926, 50.00129088274004374, -13.21731324173513400 ) ) ;
#77407 = DIRECTION ( 'NONE',  ( -0.8660254037844387076, -0.4999999999999998890, -0.000000000000000000 ) ) ;
#77409 = CARTESIAN_POINT ( 'NONE',  ( 76.07050809621944154, 51.21356314218704142, 16.11001018009165620 ) ) ;
#77408 = CARTESIAN_POINT ( 'NONE',  ( 73.66743201189373735, 69.33122701867863213, -9.963040539579864685 ) ) ;
#77410 = CARTESIAN_POINT ( 'NONE',  ( 168.9707749765159690, 251.9125659635931243, -8.781273530211780809 ) ) ;
#77411 = CARTESIAN_POINT ( 'NONE',  ( 161.3691267615756431, 251.8145564780636221, 13.54285799199859675 ) ) ;
#77412 = SHAPE_REPRESENTATION ( 'Circular Angle Protractor Plate', ( #68784 ), #70444 ) ;
#77413 = EDGE_CURVE ( 'NONE', #15552, #77091, #95658, .T. ) ;
#77414 = CARTESIAN_POINT ( 'NONE',  ( 157.5042325173297684, 257.8416622032797818, 16.70595240278738203 ) ) ;
#77415 = CARTESIAN_POINT ( 'NONE',  ( 71.76351473723396168, 71.84897031608997509, 2.971691788643022303 ) ) ;
#77416 = LINE ( 'NONE', #39873, #52972 ) ;
#77417 = ADVANCED_FACE ( 'NONE', ( #82454 ), #15900, .T. ) ;
#77418 = CARTESIAN_POINT ( 'NONE',  ( 33.73396797431614402, 190.2833772461660544, -9.188101187500095079 ) ) ;
#77419 = CIRCLE ( 'NONE', #27238, 0.5000000000000004441 ) ;
#77420 = EDGE_CURVE ( 'NONE', #55128, #69980, #8383, .T. ) ;
#77421 = CARTESIAN_POINT ( 'NONE',  ( 61.28457468009112574, 200.0643266524160424, 9.188101187500095079 ) ) ;
#77422 = CARTESIAN_POINT ( 'NONE',  ( 180.6161154953664152, 256.8960555319623609, 8.355174764559180289 ) ) ;
#77423 = CARTESIAN_POINT ( 'NONE',  ( 88.08725135673812190, 43.63233996731285202, 0.09640656973314606915 ) ) ;
#77424 = VECTOR ( 'NONE', #53824, 1000.000000000000114 ) ;
#77425 = CARTESIAN_POINT ( 'NONE',  ( 96.20275958967147290, 237.8967562850346837, -4.648177544792955347E-16 ) ) ;
#77426 = CARTESIAN_POINT ( 'NONE',  ( -13.83428154636143503, 169.4865022471903160, -10.00000000000009415 ) ) ;
#77427 = LINE ( 'NONE', #69803, #84649 ) ;
#77428 = AXIS2_PLACEMENT_3D ( 'NONE', #55396, #39193, #25012 ) ;
#77429 = CARTESIAN_POINT ( 'NONE',  ( 198.9154154329768573, 270.8075422652725024, -11.00997099090270481 ) ) ;
#77430 = CARTESIAN_POINT ( 'NONE',  ( 29.82838080365165112, 20.14754757982091249, -5.678558825948275768 ) ) ;
#77431 = CARTESIAN_POINT ( 'NONE',  ( 198.7136873185829984, 286.4647927352960437, -18.57144721070432070 ) ) ;
#77432 = CARTESIAN_POINT ( 'NONE',  ( 80.87570718637368827, 47.50421068166237859, -12.95331308923947056 ) ) ;
#77433 = CARTESIAN_POINT ( 'NONE',  ( 14.33134397731654630, 13.98920272979924917, 7.433330006724137462 ) ) ;
#77434 = CARTESIAN_POINT ( 'NONE',  ( 62.15025298811053744, 212.8149278399160949, -9.188101187500095079 ) ) ;
#77435 = CARTESIAN_POINT ( 'NONE',  ( 77.20655462988578677, 63.53086439471233859, 15.45977356242439349 ) ) ;
#77436 = CARTESIAN_POINT ( 'NONE',  ( 82.72330532876915754, 53.96112743574217774, -15.47339361700331928 ) ) ;
#77437 = AXIS2_PLACEMENT_3D ( 'NONE', #92323, #60853, #61366 ) ;
#77438 = CARTESIAN_POINT ( 'NONE',  ( 159.7953104873542145, 253.8733987550956783, 15.41928249285404107 ) ) ;
#77439 = CARTESIAN_POINT ( 'NONE',  ( 58.38862868653046689, 194.5177522451417929, 5.000000000000051514 ) ) ;
#77440 = CARTESIAN_POINT ( 'NONE',  ( 153.2550847801022087, 276.9870336669021640, 8.088704299435450551 ) ) ;
#77441 = CARTESIAN_POINT ( 'NONE',  ( 75.56006359584802112, 56.67736960126342183, -16.12308054916178079 ) ) ;
#77443 = CARTESIAN_POINT ( 'NONE',  ( 87.72955037964742075, 45.02833699891566255, -6.646681420800613971 ) ) ;
#77442 = CIRCLE ( 'NONE', #37002, 17.82106496071138935 ) ;
#77444 = CARTESIAN_POINT ( 'NONE',  ( 119.6057994200909036, 229.8615022471901739, 5.000000000000051514 ) ) ;
#77445 = CARTESIAN_POINT ( 'NONE',  ( 161.5431944097339851, 250.8459749958011287, 14.52339846942414603 ) ) ;
#77446 = CARTESIAN_POINT ( 'NONE',  ( 207.3062152119541679, 271.5820978585240368, 7.879821064966149535 ) ) ;
#77447 = EDGE_LOOP ( 'NONE', ( #96961, #7087, #99028, #24008 ) ) ;
#77448 = CARTESIAN_POINT ( 'NONE',  ( 77.36024730155139650, 49.51677810190187756, 14.91251237265224638 ) ) ;
#77449 = CARTESIAN_POINT ( 'NONE',  ( 82.88482919494256862, 53.69580434870785979, 15.74208873548984755 ) ) ;
#77450 = VERTEX_POINT ( 'NONE', #39250 ) ;
#77451 = CARTESIAN_POINT ( 'NONE',  ( 159.3451320108506764, 254.6531307488737355, -16.72997986213134425 ) ) ;
#77452 = CARTESIAN_POINT ( 'NONE',  ( 194.2091819726834103, 293.8763763881810291, 14.13354809719834826 ) ) ;
#77453 = CARTESIAN_POINT ( 'NONE',  ( 71.84509507049874344, 68.86203342550538764, -9.163320704559227536 ) ) ;
#77454 = ORIENTED_EDGE ( 'NONE', *, *, #19445, .F. ) ;
#77455 = CARTESIAN_POINT ( 'NONE',  ( 173.2985268944221104, 251.6510046717872910, -0.07099267305675936723 ) ) ;
#77456 = ORIENTED_EDGE ( 'NONE', *, *, #50746, .T. ) ;
#77457 = CARTESIAN_POINT ( 'NONE',  ( 79.56744450085628273, 46.24204545948038714, -13.19286817301344250 ) ) ;
#77458 = CARTESIAN_POINT ( 'NONE',  ( 147.9791529310278122, 274.3395839928920168, -7.789432462804474433 ) ) ;
#77459 = DIRECTION ( 'NONE',  ( 1.000000000000000000, 0.000000000000000000, 0.000000000000000000 ) ) ;
#77460 = AXIS2_PLACEMENT_3D ( 'NONE', #71941, #62816, #63323 ) ;
#77461 = ORIENTED_EDGE ( 'NONE', *, *, #32593, .F. ) ;
#77462 = PRODUCT_DEFINITION ( 'UNKNOWN', '', #99610, #39228 ) ;
#77463 = CARTESIAN_POINT ( 'NONE',  ( 23.19008890107776821, 36.49540643055188838, 3.479690158560446702E-15 ) ) ;
#77464 = CARTESIAN_POINT ( 'NONE',  ( 75.57971908217777468, 57.62099012794157460, 16.07717357865400842 ) ) ;
#77465 = FACE_OUTER_BOUND ( 'NONE', #72222, .T. ) ;
#77466 = LINE ( 'NONE', #37922, #71551 ) ;
#77467 = ORIENTED_EDGE ( 'NONE', *, *, #17895, .T. ) ;
#77468 = DIRECTION ( 'NONE',  ( 0.5000000000000014433, -0.8660254037844378194, 0.000000000000000000 ) ) ;
#77469 = CARTESIAN_POINT ( 'NONE',  ( 159.9647205790309101, 253.5799718689968927, -16.48298384325780219 ) ) ;
#77470 = VERTEX_POINT ( 'NONE', #15972 ) ;
#77471 = CARTESIAN_POINT ( 'NONE',  ( 174.7250473363198751, 286.2220955514192156, 10.55014635880517559 ) ) ;
#77472 = CARTESIAN_POINT ( 'NONE',  ( 67.75500653864465050, 65.62281390131039416, -10.81429207771451573 ) ) ;
#77473 = CARTESIAN_POINT ( 'NONE',  ( 207.6163508138795635, 271.0449272387537576, -1.385071889578343152 ) ) ;
#77474 = CARTESIAN_POINT ( 'NONE',  ( 163.9704062730716032, 246.6419207277664327, 7.317582738093436845 ) ) ;
#77475 = CARTESIAN_POINT ( 'NONE',  ( 185.4517836755765643, 292.6420132580468589, -10.71622804994104605 ) ) ;
#77476 = FACE_OUTER_BOUND ( 'NONE', #54650, .T. ) ;
#77477 = CARTESIAN_POINT ( 'NONE',  ( 144.1522069568320887, 254.0333772461660260, 9.188101187500095079 ) ) ;
#77478 = LINE ( 'NONE', #47552, #4830 ) ;
#77479 = CARTESIAN_POINT ( 'NONE',  ( 178.7522638060953852, 257.9681842698315108, 9.852045485592459073 ) ) ;
#77480 = CARTESIAN_POINT ( 'NONE',  ( 80.68904315757745849, 208.2048013555409796, 4.594050593750051981 ) ) ;
#77481 = ORIENTED_EDGE ( 'NONE', *, *, #14715, .T. ) ;
#77483 = CARTESIAN_POINT ( 'NONE',  ( 191.5281967176683509, 298.9104275333885994, 7.715154960566919407 ) ) ;
#77482 = B_SPLINE_CURVE_WITH_KNOTS ( 'NONE', 3,
 ( #776, #31662, #85431, #93520 ),
 .UNSPECIFIED., .F., .F.,
 ( 4, 4 ),
 ( 0.003345072186823920199, 0.01130424824522063658 ),
 .UNSPECIFIED. ) ;
#77484 = CARTESIAN_POINT ( 'NONE',  ( 185.7372650184451857, 257.4645284076796656, -2.264991511946413505E-12 ) ) ;
#77485 = EDGE_CURVE ( 'NONE', #28084, #99896, #7513, .T. ) ;
#77486 = ORIENTED_EDGE ( 'NONE', *, *, #10130, .T. ) ;
#77487 = CARTESIAN_POINT ( 'NONE',  ( -50.41871976035449165, 31.58591985673634639, -10.00000000000000000 ) ) ;
#77488 = EDGE_LOOP ( 'NONE', ( #40397, #38919, #23718, #68879 ) ) ;
#77489 = ORIENTED_EDGE ( 'NONE', *, *, #81793, .T. ) ;
#77490 = CARTESIAN_POINT ( 'NONE',  ( 66.43357910826331647, 67.89188047633619760, 6.623141227690268806 ) ) ;
#77491 = CARTESIAN_POINT ( 'NONE',  ( 197.9324133593710542, 286.8504239745568043, 16.93537766679494894 ) ) ;
#77492 = CARTESIAN_POINT ( 'NONE',  ( 83.76824508872513775, 42.19076294718777831, -5.428203380119669852 ) ) ;
#77493 = LINE ( 'NONE', #69867, #66071 ) ;
#77494 = CARTESIAN_POINT ( 'NONE',  ( 77.36600796148924530, 49.13692148722834929, -14.77749963168140113 ) ) ;
#77495 = CARTESIAN_POINT ( 'NONE',  ( 70.40095915148631889, 63.88372271459088836, 12.84393136659105572 ) ) ;
#77496 = CARTESIAN_POINT ( 'NONE',  ( 82.55649720842890815, 206.2202760586659167, -5.415160957724236172E-17 ) ) ;
#77497 = EDGE_LOOP ( 'NONE', ( #22986, #99911, #74629, #54041 ) ) ;
#77498 = EDGE_CURVE ( 'NONE', #86016, #43672, #84894, .T. ) ;
#77499 = EDGE_LOOP ( 'NONE', ( #58542, #38742, #11756, #18470 ) ) ;
#77500 = CARTESIAN_POINT ( 'NONE',  ( 15.68640692011977222, 32.55466486950700045, -1.111400068045478839E-16 ) ) ;
#77501 = CARTESIAN_POINT ( 'NONE',  ( 200.8466324750363299, 282.7704233545608190, -16.77580403217666927 ) ) ;
#77502 = EDGE_LOOP ( 'NONE', ( #23471, #33390, #79789, #45406 ) ) ;
#77503 = ADVANCED_FACE ( 'NONE', ( #41259 ), #79076, .F. ) ;
#77504 = CARTESIAN_POINT ( 'NONE',  ( 76.39943616605862076, 51.65488121685059042, -16.16297552989059128 ) ) ;
#77505 = CARTESIAN_POINT ( 'NONE',  ( 183.6917392022668309, 275.6525662950718356, 17.55237957418163930 ) ) ;
#77506 = CIRCLE ( 'NONE', #59449, 70.00000000000001421 ) ;
#77507 = CARTESIAN_POINT ( 'NONE',  ( 205.8030308266901898, 274.1856895869457844, 10.55961490432110317 ) ) ;
#77508 = CARTESIAN_POINT ( 'NONE',  ( 206.8711744556208885, 269.6661967102621702, -5.660351959544826712E-12 ) ) ;
#77509 = CARTESIAN_POINT ( 'NONE',  ( 207.1061707122464099, 270.1598718182783614, -2.616480830523119305 ) ) ;
#77510 = DIRECTION ( 'NONE',  ( 0.000000000000000000, 0.000000000000000000, 1.000000000000000000 ) ) ;
#77511 = AXIS2_PLACEMENT_3D ( 'NONE', #43353, #13964, #97592 ) ;
#77512 = ORIENTED_EDGE ( 'NONE', *, *, #86226, .F. ) ;
#77513 = CARTESIAN_POINT ( 'NONE',  ( 81.95226675463217703, 43.66151996434197713, -8.822569420014042763 ) ) ;
#77514 = CARTESIAN_POINT ( 'NONE',  ( 185.3548632422784976, 260.1969484205714025, 6.113967884209870363 ) ) ;
#77515 = CARTESIAN_POINT ( 'NONE',  ( 28.94742091202107304, 40.21091486745862653, 7.012934429366973338E-14 ) ) ;
#77516 = CARTESIAN_POINT ( 'NONE',  ( 200.6737073311291795, 283.0699384897140476, -17.61533935526990291 ) ) ;
#77517 = CARTESIAN_POINT ( 'NONE',  ( 72.44020731426283533, 70.76712560363094440, 7.696415609646560796 ) ) ;
#77518 = CARTESIAN_POINT ( 'NONE',  ( 69.47694127934478558, 67.41711995099386456, -9.198496735959366788 ) ) ;
#77519 = ORIENTED_EDGE ( 'NONE', *, *, #61638, .T. ) ;
#77520 = CARTESIAN_POINT ( 'NONE',  ( 185.1491161497484370, 292.9437783688060222, -11.97406807593424993 ) ) ;
#77521 = AXIS2_PLACEMENT_3D ( 'NONE', #3574, #41545, #4548 ) ;
#77522 = CARTESIAN_POINT ( 'NONE',  ( -15.31269525828471068, 104.2312461070085021, 43.89948692389422291 ) ) ;
#77523 = DIRECTION ( 'NONE',  ( 0.9681751565707763518, -0.2502735827033140681, 0.000000000000000000 ) ) ;
#77524 = CARTESIAN_POINT ( 'NONE',  ( 171.3649617487770911, 251.0102673366500596, 7.372720983288576946 ) ) ;
#77525 = CARTESIAN_POINT ( 'NONE',  ( 83.61973431552902980, 52.33906237753651425, 14.75805511933742054 ) ) ;
#77526 = CARTESIAN_POINT ( 'NONE',  ( -27.23710841895085721, 23.47708815495369450, 177.5919119679930134 ) ) ;
#77527 = ORIENTED_EDGE ( 'NONE', *, *, #46988, .F. ) ;
#77528 = CARTESIAN_POINT ( 'NONE',  ( 202.7041331321765938, 279.5531378413010657, 17.14708438049711248 ) ) ;
#77529 = CARTESIAN_POINT ( 'NONE',  ( 40.18174127881769664, 205.5530062829863027, -4.648177544792955347E-16 ) ) ;
#77531 = CARTESIAN_POINT ( 'NONE',  ( 74.06178371959768469, 55.22988461276135297, 16.12358979270296189 ) ) ;
#77530 = LINE ( 'NONE', #86175, #43487 ) ;
#77532 = CARTESIAN_POINT ( 'NONE',  ( 176.1242821188019718, 285.3583729749952909, -12.07621089340971920 ) ) ;
#77533 = EDGE_CURVE ( 'NONE', #59587, #20684, #66077, .T. ) ;
#77534 = CARTESIAN_POINT ( 'NONE',  ( 29.94731862920856358, 22.45404122711134676, -8.090169943749478065 ) ) ;
#77535 = B_SPLINE_CURVE_WITH_KNOTS ( 'NONE', 3,
 ( #23708, #54602, #85586, #16127 ),
 .UNSPECIFIED., .F., .F.,
 ( 4, 4 ),
 ( 0.01081206089262459064, 0.01921137274017016561 ),
 .UNSPECIFIED. ) ;
#77536 = CARTESIAN_POINT ( 'NONE',  ( 41.47569090598247499, 209.1868197944957899, 17.47570218321535762 ) ) ;
#77537 = DIRECTION ( 'NONE',  ( 1.000000000000000000, -3.152240373489283172E-13, 0.000000000000000000 ) ) ;
#77538 = CARTESIAN_POINT ( 'NONE',  ( 188.2526772805193502, 260.8404435756410180, 2.927908703176840266 ) ) ;
#77539 = CARTESIAN_POINT ( 'NONE',  ( 139.3620039403753879, 261.2677522451419350, -5.000000000000047962 ) ) ;
#77540 = CARTESIAN_POINT ( 'NONE',  ( 190.2505983465532324, 296.1737925351780518, -11.69656242540844282 ) ) ;
#77541 = EDGE_LOOP ( 'NONE', ( #75723, #18458, #56787, #13482 ) ) ;
#77542 = EDGE_CURVE ( 'NONE', #77961, #93808, #97024, .T. ) ;
#77543 = EDGE_CURVE ( 'NONE', #84457, #33337, #82330, .T. ) ;
#77544 = CARTESIAN_POINT ( 'NONE',  ( 178.5588389885454319, 256.8987037950940362, 8.463150697600209327 ) ) ;
#77545 = CARTESIAN_POINT ( 'NONE',  ( 72.82956929615316710, 70.88121797294115822, -7.877017184599600874 ) ) ;
#77546 = DIRECTION ( 'NONE',  ( 0.8660254037844380415, -0.5000000000000011102, 0.000000000000000000 ) ) ;
#77547 = CARTESIAN_POINT ( 'NONE',  ( 19.11978928545374501, 181.8458772461660544, 9.188101187500095079 ) ) ;
#77548 = CARTESIAN_POINT ( 'NONE',  ( 181.9657388339318231, 275.7813954516299191, -16.43665191748776877 ) ) ;
#77549 = CARTESIAN_POINT ( 'NONE',  ( 36.01802474176511026, 21.76426979415091978, 3.090169943749476733 ) ) ;
#77550 = CARTESIAN_POINT ( 'NONE',  ( 77.80683632129496630, 56.80414902711877545, 16.61016218681300316 ) ) ;
#77551 = CARTESIAN_POINT ( 'NONE',  ( 171.0406735725552210, 271.3140026262360607, -17.70316094230177129 ) ) ;
#77552 = CARTESIAN_POINT ( 'NONE',  ( 80.96958682834429055, 55.96437743930621878, 16.09281336319931199 ) ) ;
#77553 = B_SPLINE_CURVE_WITH_KNOTS ( 'NONE', 3,
 ( #43007, #90175, #20245, #75959 ),
 .UNSPECIFIED., .F., .F.,
 ( 4, 4 ),
 ( 0.03513230373696424325, 0.04390280448137185570 ),
 .UNSPECIFIED. ) ;
#77554 = CARTESIAN_POINT ( 'NONE',  ( 84.15650392679282277, 46.61449241044970648, 11.42639398603495948 ) ) ;
#77555 = CARTESIAN_POINT ( 'NONE',  ( 187.6663016716853747, 259.1672013800106242, -0.7921523300642274723 ) ) ;
#77556 = CARTESIAN_POINT ( 'NONE',  ( 72.84042761573121538, 202.8615022471901739, 5.000000000000051514 ) ) ;
#77557 = CARTESIAN_POINT ( 'NONE',  ( 37.86538501507694576, 37.56454794089044213, 10.00000000000000355 ) ) ;
#77558 = DIRECTION ( 'NONE',  ( -0.8660254037844387076, -0.4999999999999998890, -0.000000000000000000 ) ) ;
#77559 = CARTESIAN_POINT ( 'NONE',  ( 25.10051690851626560, 194.4869531367911293, 4.594050593750046652 ) ) ;
#77560 = CARTESIAN_POINT ( 'NONE',  ( 66.47763888060634940, 67.99612994687967671, 6.463816603905435443 ) ) ;
#77561 = CARTESIAN_POINT ( 'NONE',  ( 28.38430345058481663, 38.16126292948897003, -6.180339887498951690 ) ) ;
#77562 = CARTESIAN_POINT ( 'NONE',  ( 49.06003799288187395, 95.45573527953635562, 10.00000000000000000 ) ) ;
#77563 = CARTESIAN_POINT ( 'NONE',  ( 199.2299651681423143, 285.5705732690366858, -17.65328173313980642 ) ) ;
#77565 = PLANE ( 'NONE',  #74189 ) ;
#77564 = VECTOR ( 'NONE', #97509, 1000.000000000000000 ) ;
#77566 = CARTESIAN_POINT ( 'NONE',  ( 6.176825452568912134, 162.8262482093457777, 3.021315404115420679E-15 ) ) ;
#77567 = CARTESIAN_POINT ( 'NONE',  ( 162.2342503670216729, 281.0091534512037583, -10.48921805985605538 ) ) ;
#77568 = CARTESIAN_POINT ( 'NONE',  ( 163.8712475794395118, 282.0753919168961374, 10.04803168266247582 ) ) ;
#77569 = SHAPE_DEFINITION_REPRESENTATION ( #11989, #87244 ) ;
#77570 = CARTESIAN_POINT ( 'NONE',  ( 24.39888929631063519, 19.80170272979926693, 7.433330006724137462 ) ) ;
#77571 = CARTESIAN_POINT ( 'NONE',  ( 190.3144310910409445, 301.0127312671879167, -1.334877248546042949 ) ) ;
#77572 = CARTESIAN_POINT ( 'NONE',  ( 71.73982542038400823, 59.04037670598220444, 15.36454711367335513 ) ) ;
#77573 = CARTESIAN_POINT ( 'NONE',  ( 188.9238571764875871, 270.0808980012285474, -15.37208702597789234 ) ) ;
#77574 = ORIENTED_EDGE ( 'NONE', *, *, #11962, .T. ) ;
#77575 = AXIS2_PLACEMENT_3D ( 'NONE', #71580, #2176, #2678 ) ;
#77576 = CARTESIAN_POINT ( 'NONE',  ( 185.4211012460235395, 291.0283491078289444, 13.34097488155738631 ) ) ;
#77577 = CARTESIAN_POINT ( 'NONE',  ( 12.55777956335723644, 9.111106405272902720, -2.839279412974138328 ) ) ;
#77578 = CARTESIAN_POINT ( 'NONE',  ( 75.29803635635754233, 53.62586610745756843, -16.53393874230848581 ) ) ;
#77579 = CARTESIAN_POINT ( 'NONE',  ( -56.06787742410712383, 34.75406423768147590, 10.00000000000000000 ) ) ;
#77580 = CARTESIAN_POINT ( 'NONE',  ( 88.28488596560143264, 44.32818720243073329, 2.217326208295938628 ) ) ;
#77581 = VERTEX_POINT ( 'NONE', #27088 ) ;
#77582 = DIRECTION ( 'NONE',  ( -0.7691052716734824157, -0.08748735329025024432, -0.6331058711608398282 ) ) ;
#77583 = FACE_OUTER_BOUND ( 'NONE', #55998, .T. ) ;
#77585 = CARTESIAN_POINT ( 'NONE',  ( 77.05460391109571106, 63.75555097366715529, 14.97632912148298168 ) ) ;
#77584 = B_SPLINE_CURVE_WITH_KNOTS ( 'NONE', 3,
 ( #63670, #17063, #55549, #64174, #55057, #85526, #25164, #31748, #8475, #9482, #47464, #32764, #93605, #79918, #16568, #71290, #56047, #95633, #87039, #32266, #86533, #2391, #10480, #72299, #33799, #33271, #9987, #78389, #8970, #24665, #87553, #18086, #39840, #64683, #70771, #63169, #94113, #47954, #48982, #78897, #94609, #41357, #2906, #26181, #16069, #46971, #72810, #65169, #35767, #58555 ),
 .UNSPECIFIED., .F., .F.,
 ( 4, 2, 2, 2, 2, 2, 2, 2, 2, 2, 2, 2, 2, 2, 2, 2, 2, 2, 2, 2, 2, 2, 2, 2, 4 ),
 ( 0.002964269280204859160, 0.003162640838911195268, 0.003361012397617531809, 0.003460198176970720896, 0.003559383956323909984, 0.003658569735677099071, 0.003757755515030288158, 0.004154498632443132111, 0.004551241749855975197, 0.005344727984681663102, 0.006138214219507351008, 0.006931700454333038913, 0.007725186689158725084, 0.007824372468511853890, 0.007873965358188416558, 0.007923558247864980961, 0.007973151137541543629, 0.008022744027218108032, 0.008121929806571235103, 0.008320301365277530878, 0.008518672923983824918, 0.008717044482690120694, 0.008915416041396416469, 0.009113787600102712244, 0.009312159158809008019 ),
 .UNSPECIFIED. ) ;
#77586 = CARTESIAN_POINT ( 'NONE',  ( 173.8665542827094725, 250.6399523573830095, -0.9454928766311748722 ) ) ;
#77587 = ORIENTED_EDGE ( 'NONE', *, *, #55901, .T. ) ;
#77588 = AXIS2_PLACEMENT_3D ( 'NONE', #14079, #44965, #75904 ) ;
#77589 = EDGE_LOOP ( 'NONE', ( #48198, #24097, #91455, #35574, #73037, #51934, #32618, #98259, #86489, #6781, #30744, #66393, #20043, #47562, #17523, #76714, #24799, #51719, #86293, #86372, #46662, #8052, #47795, #96584, #94449, #66054, #53649, #11148, #24251, #67645, #17019, #36107, #75988, #26772, #43902, #26632, #82383, #52332, #63845, #27892, #7894, #35182, #56008, #96609, #58625, #71371, #43831, #95101, #20461, #61615 ) ) ;
#77591 = CARTESIAN_POINT ( 'NONE',  ( 87.61103589779790468, 43.76214543387700218, -0.04131823639585689711 ) ) ;
#77590 = CARTESIAN_POINT ( 'NONE',  ( 189.4681065570641749, 274.0997382612658271, -15.65967126434479617 ) ) ;
#77592 = VERTEX_POINT ( 'NONE', #89432 ) ;
#77593 = FACE_OUTER_BOUND ( 'NONE', #48659, .T. ) ;
#77594 = CARTESIAN_POINT ( 'NONE',  ( -27.42236680055714260, 166.5217562850347406, 1.224646799147364892E-15 ) ) ;
#77595 = CARTESIAN_POINT ( 'NONE',  ( -70.00000000000000000, 15.00000000000000000, 59.99999999999999289 ) ) ;
#77596 = CARTESIAN_POINT ( 'NONE',  ( 77.10733807873376122, 63.61886353868632682, 15.40965320646045100 ) ) ;
#77597 = CARTESIAN_POINT ( 'NONE',  ( 148.3997536239841679, 273.6110822229926498, 8.713694244701960301 ) ) ;
#77598 = CARTESIAN_POINT ( 'NONE',  ( 196.7491951525289835, 289.8673929779723721, -16.35352603081977207 ) ) ;
#77599 = VECTOR ( 'NONE', #77910, 1000.000000000000000 ) ;
#77600 = FACE_OUTER_BOUND ( 'NONE', #68342, .T. ) ;
#77601 = EDGE_CURVE ( 'NONE', #35992, #62993, #57044, .T. ) ;
#77602 = ORIENTED_EDGE ( 'NONE', *, *, #36924, .F. ) ;
#77603 = CARTESIAN_POINT ( 'NONE',  ( 195.7578697689113199, 291.5844189092309193, 17.18796537138345215 ) ) ;
#77604 = CARTESIAN_POINT ( 'NONE',  ( 208.3117541397001844, 269.8404533466799080, 2.895672523916592578 ) ) ;
#77605 = EDGE_LOOP ( 'NONE', ( #17561, #36074, #38937 ) ) ;
#77606 = CARTESIAN_POINT ( 'NONE',  ( 31.76492312988469280, 26.84335787977765264, 9.188101187500006262 ) ) ;
#77607 = CARTESIAN_POINT ( 'NONE',  ( 190.0550686570564949, 301.4619601804237732, 4.203010638620038542 ) ) ;
#77608 = CARTESIAN_POINT ( 'NONE',  ( 85.72375369157853697, 153.9044130683316212, 0.000000000000000000 ) ) ;
#77609 = ADVANCED_FACE ( 'NONE', ( #5764 ), #100030, .T. ) ;
#77610 = VERTEX_POINT ( 'NONE', #13866 ) ;
#77611 = DIRECTION ( 'NONE',  ( -1.000000000000000000, -1.156482317317871331E-15, 0.000000000000000000 ) ) ;
#77612 = CARTESIAN_POINT ( 'NONE',  ( 150.6571681785161445, 269.7011255207979730, 15.24894850018880454 ) ) ;
#77613 = DIRECTION ( 'NONE',  ( -0.8660254037844378194, -0.5000000000000014433, 0.000000000000000000 ) ) ;
#77614 = LINE ( 'NONE', #8198, #99736 ) ;
#77615 = VERTEX_POINT ( 'NONE', #77684 ) ;
#77616 = ORIENTED_EDGE ( 'NONE', *, *, #23058, .T. ) ;
#77617 = CARTESIAN_POINT ( 'NONE',  ( 190.8131867350074060, 299.6564803534650423, 5.431438511040964201 ) ) ;
#77618 = CARTESIAN_POINT ( 'NONE',  ( 5.783292089056025098, 27.85010085989871698, 177.5919119679930134 ) ) ;
#77619 = CARTESIAN_POINT ( 'NONE',  ( 190.6036479972031259, 300.5117928913073797, -0.6824572005520307405 ) ) ;
#77620 = ORIENTED_EDGE ( 'NONE', *, *, #43812, .T. ) ;
#77621 = CARTESIAN_POINT ( 'NONE',  ( 149.4539134692060145, 271.7852238117696402, 12.95627816374690688 ) ) ;
#77622 = CARTESIAN_POINT ( 'NONE',  ( 157.3604748455635729, 259.8466937948429063, -17.62934668591135079 ) ) ;
#77623 = EDGE_CURVE ( 'NONE', #47892, #89224, #52191, .T. ) ;
#77624 = DIRECTION ( 'NONE',  ( -0.8660254037844387076, -0.4999999999999998890, -0.000000000000000000 ) ) ;
#77625 = CARTESIAN_POINT ( 'NONE',  ( 192.4259603496955719, 297.3554553095298729, -12.40738485318142814 ) ) ;
#77626 = CARTESIAN_POINT ( 'NONE',  ( 160.0613924909338550, 255.6058025510563709, 16.19881800728115095 ) ) ;
#77627 = CARTESIAN_POINT ( 'NONE',  ( 69.03049085021430642, 65.53841201702186936, 10.92225791274772106 ) ) ;
#77628 = CARTESIAN_POINT ( 'NONE',  ( 102.5355703512972809, 241.5530062829863027, -4.648177544792955347E-16 ) ) ;
#77629 = CARTESIAN_POINT ( 'NONE',  ( 75.88013953913147702, 65.59923957098945380, 13.85558759313056143 ) ) ;
#77630 = CARTESIAN_POINT ( 'NONE',  ( 69.90077517449054767, 65.54052102004983738, -11.37488096913896030 ) ) ;
#77631 = CARTESIAN_POINT ( 'NONE',  ( 78.55989720566141443, 47.96478771419136677, 13.95455569139155827 ) ) ;
#77632 = CARTESIAN_POINT ( 'NONE',  ( 104.9102572999672276, 237.5024278399160949, 9.188101187500095079 ) ) ;
#77633 = VERTEX_POINT ( 'NONE', #7251 ) ;
#77634 = CARTESIAN_POINT ( 'NONE',  ( 191.4852287632733123, 298.9848502134979071, -9.870565261052552941 ) ) ;
#77635 = CARTESIAN_POINT ( 'NONE',  ( 70.22598590769381133, 65.16623735881336188, 11.86258439676588061 ) ) ;
#77636 = CARTESIAN_POINT ( 'NONE',  ( 87.79271458260285499, 45.16522989489592987, -6.842624051142037089 ) ) ;
#77637 = EDGE_CURVE ( 'NONE', #32407, #69987, #37746, .T. ) ;
#77638 = CARTESIAN_POINT ( 'NONE',  ( 203.3349860717029571, 278.4604684979374838, -16.59553970625579566 ) ) ;
#77639 = EDGE_CURVE ( 'NONE', #32226, #27140, #22320, .T. ) ;
#77640 = CARTESIAN_POINT ( 'NONE',  ( 183.2719456501309594, 284.6370414458698974, -14.99201719159501422 ) ) ;
#77641 = CARTESIAN_POINT ( 'NONE',  ( 83.55324616867257248, 51.62071861895685743, -14.85649312488210860 ) ) ;
#77642 = CARTESIAN_POINT ( 'NONE',  ( 168.8758384829626209, 284.8846904623786713, -7.958113118064016334 ) ) ;
#77643 = ORIENTED_EDGE ( 'NONE', *, *, #81244, .T. ) ;
#77644 = CARTESIAN_POINT ( 'NONE',  ( 80.32771389996757705, 57.94408260071152483, -16.24746918486167857 ) ) ;
#77645 = CARTESIAN_POINT ( 'NONE',  ( 72.07419404290544662, 71.65773480557935216, 5.498832909113074763 ) ) ;
#77646 = CARTESIAN_POINT ( 'NONE',  ( 74.60675634627781960, 67.01455260309188589, 12.52145295594442942 ) ) ;
#77647 = CARTESIAN_POINT ( 'NONE',  ( 135.2486435959970947, 239.7048013555409796, 4.594050593750051981 ) ) ;
#77648 = CARTESIAN_POINT ( 'NONE',  ( 190.9583202594226918, 294.9585867271870256, -12.20043999232385978 ) ) ;
#77649 = VECTOR ( 'NONE', #66262, 1000.000000000000000 ) ;
#77650 = FACE_OUTER_BOUND ( 'NONE', #46554, .T. ) ;
#77651 = CARTESIAN_POINT ( 'NONE',  ( 157.6335212189247557, 257.6177276032722716, 16.76495363836117036 ) ) ;
#77652 = DIRECTION ( 'NONE',  ( -0.3668518372888710521, -0.9302793824855948301, 0.000000000000000000 ) ) ;
#77653 = CARTESIAN_POINT ( 'NONE',  ( 52.89478003304684250, 201.3458772461660260, 9.188101187500095079 ) ) ;
#77654 = CARTESIAN_POINT ( 'NONE',  ( 85.61207876059154387, 48.93336676014416753, -12.63415981529851884 ) ) ;
#77655 = ORIENTED_EDGE ( 'NONE', *, *, #69283, .F. ) ;
#77656 = CARTESIAN_POINT ( 'NONE',  ( 71.10485482541737667, 63.64399173889170669, 13.27423776213106876 ) ) ;
#77657 = CARTESIAN_POINT ( 'NONE',  ( 87.66405103922522812, 44.36922529636178325, -4.037368063366974624 ) ) ;
#77658 = EDGE_CURVE ( 'NONE', #28879, #75738, #57876, .T. ) ;
#77659 = CARTESIAN_POINT ( 'NONE',  ( 73.23245250435016374, 60.46961760979917244, 15.70485221038128287 ) ) ;
#77660 = CARTESIAN_POINT ( 'NONE',  ( 147.4963928429778264, 275.1757489932608109, 4.929816573182678852 ) ) ;
#77661 = CARTESIAN_POINT ( 'NONE',  ( 151.3511865740561007, 278.6745403919405248, -1.693856907688049862 ) ) ;
#77662 = CARTESIAN_POINT ( 'NONE',  ( 154.9792334219179679, 262.2150889255981951, -17.21325849938693153 ) ) ;
#77663 = AXIS2_PLACEMENT_3D ( 'NONE', #13976, #29181, #69151 ) ;
#77664 = CARTESIAN_POINT ( 'NONE',  ( 178.5084147955354297, 261.1889675471575174, 12.22496176922636835 ) ) ;
#77665 = EDGE_CURVE ( 'NONE', #30031, #35626, #71576, .T. ) ;
#77666 = CARTESIAN_POINT ( 'NONE',  ( 113.3812418268422846, 236.2677522451418497, 10.00000000000009592 ) ) ;
#77667 = CARTESIAN_POINT ( 'NONE',  ( 169.3422351861262882, 267.3027105831644690, -17.79115954374443476 ) ) ;
#77668 = VERTEX_POINT ( 'NONE', #48258 ) ;
#77669 = EDGE_CURVE ( 'NONE', #29127, #82530, #8757, .T. ) ;
#77670 = CARTESIAN_POINT ( 'NONE',  ( 203.0535368433499457, 278.9479528611958585, 16.46202213522710167 ) ) ;
#77671 = CARTESIAN_POINT ( 'NONE',  ( 19.84093639355121397, 13.58380873178786530, 6.180339887498953466 ) ) ;
#77672 = VECTOR ( 'NONE', #74815, 1000.000000000000000 ) ;
#77673 = EDGE_CURVE ( 'NONE', #52913, #48736, #93902, .T. ) ;
#77674 = CARTESIAN_POINT ( 'NONE',  ( 36.16983797034238535, 185.5643266524159856, -9.188101187500093303 ) ) ;
#77675 = CARTESIAN_POINT ( 'NONE',  ( 21.01819855373923929, 11.94473085651391564, 1.475505719884397138E-15 ) ) ;
#77676 = DIRECTION ( 'NONE',  ( -0.8660254037844387076, -0.4999999999999998890, -0.000000000000000000 ) ) ;
#77677 = FACE_OUTER_BOUND ( 'NONE', #60274, .T. ) ;
#77678 = DIRECTION ( 'NONE',  ( -0.9762722099447411761, -0.2165469281463284212, 0.000000000000000000 ) ) ;
#77679 = EDGE_CURVE ( 'NONE', #62642, #54504, #62957, .T. ) ;
#77681 = CARTESIAN_POINT ( 'NONE',  ( 65.93911412966747321, 215.0024278399160949, 9.188101187500095079 ) ) ;
#77680 = CARTESIAN_POINT ( 'NONE',  ( 197.1856892100024652, 276.7320907554435507, -15.32951477734549961 ) ) ;
#77682 = EDGE_CURVE ( 'NONE', #69092, #13291, #82073, .T. ) ;
#77683 = CARTESIAN_POINT ( 'NONE',  ( 200.1103929410127762, 284.0456276340304953, 17.67835211026828901 ) ) ;
#77684 = CARTESIAN_POINT ( 'NONE',  ( 32.18695666311190706, 46.02670049433633181, -10.00000000000000000 ) ) ;
#77685 = CARTESIAN_POINT ( 'NONE',  ( 69.60656329481270177, 65.89280548041654129, 11.57311433810471435 ) ) ;
#77686 = CARTESIAN_POINT ( 'NONE',  ( 66.52392041415761526, 68.84470833993178474, -4.415679280538202356 ) ) ;
#77687 = ORIENTED_EDGE ( 'NONE', *, *, #69475, .F. ) ;
#77688 = CARTESIAN_POINT ( 'NONE',  ( 25.28119919123577475, 178.7365022471902023, -10.00000000000009059 ) ) ;
#77689 = CARTESIAN_POINT ( 'NONE',  ( 162.6937333994314656, 248.8531830095558632, 10.02305144031113926 ) ) ;
#77690 = CARTESIAN_POINT ( 'NONE',  ( 152.7045549149684405, 246.7202760586659736, -5.415160957724236172E-17 ) ) ;
#77691 = CARTESIAN_POINT ( 'NONE',  ( 24.61059131263772670, 35.18502408145592852, 5.678558825948277544 ) ) ;
#77692 = CARTESIAN_POINT ( 'NONE',  ( 164.0807478505496988, 260.5315732147755625, -16.15795033331652775 ) ) ;
#77693 = CARTESIAN_POINT ( 'NONE',  ( 188.3128329290244665, 261.7237649635724779, 6.448241612589410643 ) ) ;
#77694 = CARTESIAN_POINT ( 'NONE',  ( 164.3939401533646958, 245.9083385283718712, 2.844462461176849200 ) ) ;
#77695 = CARTESIAN_POINT ( 'NONE',  ( 71.47018505618770234, 71.90846791982409059, 3.715355237622318896 ) ) ;
#77696 = CARTESIAN_POINT ( 'NONE',  ( 66.04017617576342047, 68.56661300442509344, 1.988326559363849055 ) ) ;
#77697 = ORIENTED_EDGE ( 'NONE', *, *, #60859, .F. ) ;
#77698 = CARTESIAN_POINT ( 'NONE',  ( 7.127696690345725727, 16.06628583063839244, -9.188101187500006262 ) ) ;
#77699 = CARTESIAN_POINT ( 'NONE',  ( 178.7584752446753669, 285.6265442481744685, 13.03273535059368093 ) ) ;
#77700 = CARTESIAN_POINT ( 'NONE',  ( 196.6848264441626100, 289.2939774968210713, 16.62394592573511432 ) ) ;
#77701 = CARTESIAN_POINT ( 'NONE',  ( 15.46199490364264406, 17.43085787977761925, -9.188101187500008038 ) ) ;
#77702 = ORIENTED_EDGE ( 'NONE', *, *, #49251, .F. ) ;
#77703 = FACE_OUTER_BOUND ( 'NONE', #44806, .T. ) ;
#77704 = CARTESIAN_POINT ( 'NONE',  ( 24.35067441160642687, 40.23626134430271861, -10.00000000000000000 ) ) ;
#77705 = CARTESIAN_POINT ( 'NONE',  ( 71.74013172673453198, 72.14163783910345273, 0.6028694846914187666 ) ) ;
#77706 = CARTESIAN_POINT ( 'NONE',  ( 192.5712965840290849, 297.1037255674836501, 11.03742858512898906 ) ) ;
#77707 = CARTESIAN_POINT ( 'NONE',  ( 164.9779129355220562, 244.8968679994381148, -1.771286574179712803 ) ) ;
#77708 = CARTESIAN_POINT ( 'NONE',  ( -22.42236680055709641, 157.8615022471902591, 0.000000000000000000 ) ) ;
#77709 = CARTESIAN_POINT ( 'NONE',  ( 87.86298961015023679, 44.89260222163543546, 6.207647304897663254 ) ) ;
#77710 = CARTESIAN_POINT ( 'NONE',  ( 201.0844796915553161, 282.3584598911111812, -16.59562674965125950 ) ) ;
#77711 = VERTEX_POINT ( 'NONE', #44503 ) ;
#77712 =( BOUNDED_CURVE ( )  B_SPLINE_CURVE ( 2, ( #1761, #71165, #85389, #77762, #47819, #25550, #55415, #79297, #39216 ),
 .UNSPECIFIED., .F., .T. ) 
 B_SPLINE_CURVE_WITH_KNOTS ( ( 3, 2, 2, 2, 3 ),
 ( 0.8911290322580645018, 0.8924731182795698770, 0.8951612903225806273, 0.8978494623655913776, 0.8991935483870967527 ),
 .UNSPECIFIED. ) 
 CURVE ( )  GEOMETRIC_REPRESENTATION_ITEM ( )  RATIONAL_B_SPLINE_CURVE ( ( 0.9330127018922194093, 0.9330127018922194093, 1.000000000000000000, 0.8660254037844387076, 1.000000000000000000, 0.8660254037844387076, 1.000000000000000000, 0.9330127018922194093, 0.9330127018922194093 ) ) 
 REPRESENTATION_ITEM ( '' )  );
#77713 = ORIENTED_EDGE ( 'NONE', *, *, #64009, .F. ) ;
#77714 = CARTESIAN_POINT ( 'NONE',  ( 198.6444633007815810, 284.5846922512318997, -17.80363864581810418 ) ) ;
#77715 = CARTESIAN_POINT ( 'NONE',  ( 164.2173609823407219, 248.5881690971583851, 10.00396525085479915 ) ) ;
#77716 = VERTEX_POINT ( 'NONE', #66815 ) ;
#77717 = CARTESIAN_POINT ( 'NONE',  ( 69.62991599110473828, 67.28754920473278389, 10.19854214946012938 ) ) ;
#77718 = CARTESIAN_POINT ( 'NONE',  ( 155.4152395589816251, 261.8557187948458704, -16.98081665858997624 ) ) ;
#77719 = EDGE_LOOP ( 'NONE', ( #79090, #48315, #84850, #32391 ) ) ;
#77720 = CARTESIAN_POINT ( 'NONE',  ( 191.0724301404414689, 299.6998384015373063, -9.342134220577969828 ) ) ;
#77721 = CARTESIAN_POINT ( 'NONE',  ( 79.45404352011763649, 59.64539556637617324, -16.18188341986842005 ) ) ;
#77722 = CARTESIAN_POINT ( 'NONE',  ( 84.99999999999998579, 14.99999999999999467, -59.99999999999999289 ) ) ;
#77723 = CARTESIAN_POINT ( 'NONE',  ( 69.41727946307592845, 62.73729316916369925, 13.77678217037445840 ) ) ;
#77724 = ORIENTED_EDGE ( 'NONE', *, *, #21108, .T. ) ;
#77725 = CARTESIAN_POINT ( 'NONE',  ( 200.5438717407500917, 283.2948203288816558, 18.39667691545567152 ) ) ;
#77726 = CARTESIAN_POINT ( 'NONE',  ( 127.3796741259112792, 255.8967562850346553, -4.648177544792955347E-16 ) ) ;
#77727 = CARTESIAN_POINT ( 'NONE',  ( 191.4941427383744781, 298.9694107557253346, 8.584406880462095657 ) ) ;
#77728 = LINE ( 'NONE', #95471, #50982 ) ;
#77729 = VERTEX_POINT ( 'NONE', #68307 ) ;
#77730 = ORIENTED_EDGE ( 'NONE', *, *, #85069, .T. ) ;
#77731 = B_SPLINE_CURVE_WITH_KNOTS ( 'NONE', 3,
 ( #22114, #91546, #52505, #92548, #83454, #53007, #83958, #14522, #45404, #76334, #6427, #44404, #6908, #30715, #14020, #82960, #37304, #7401, #44899, #98137, #76807, #13534, #52021, #28722, #30212, #68204, #22614, #37796, #75336, #68701, #15489, #99630, #61094, #92065, #99131, #23095, #29715, #84454, #14995, #38293, #69203, #100129, #61597, #53985, #36309, #74846 ),
 .UNSPECIFIED., .F., .F.,
 ( 4, 2, 2, 2, 2, 2, 2, 2, 2, 2, 2, 2, 2, 2, 2, 2, 2, 2, 2, 2, 2, 2, 4 ),
 ( 0.002307665126650576288, 0.002732801707347156522, 0.002945369997695357518, 0.003051654142869509190, 0.003157938288043660863, 0.003264222433217812535, 0.003370506578391964207, 0.003583074868740191658, 0.004008211449436645257, 0.004858484610829631387, 0.005708757772222617516, 0.006559030933615603645, 0.006984167514312139211, 0.007409304095008673041, 0.007515588240182871985, 0.007568730312769972324, 0.007621872385357072663, 0.007675014457944171267, 0.007728156530531271606, 0.007834440675705392487, 0.008259577256402054687, 0.008684713837098716888, 0.009109850417795377353 ),
 .UNSPECIFIED. ) ;
#77732 = VERTEX_POINT ( 'NONE', #29325 ) ;
#77733 = CARTESIAN_POINT ( 'NONE',  ( 72.89193669360001593, 59.22924534911017957, 15.51103768891951695 ) ) ;
#77734 = ORIENTED_EDGE ( 'NONE', *, *, #83156, .F. ) ;
#77735 = CARTESIAN_POINT ( 'NONE',  ( 71.40725718522095633, 71.90619859764527178, 1.119957492137431343 ) ) ;
#77736 = CIRCLE ( 'NONE', #46984, 17.82106496071138935 ) ;
#77737 = ORIENTED_EDGE ( 'NONE', *, *, #98923, .F. ) ;
#77738 = CARTESIAN_POINT ( 'NONE',  ( 164.1146561143383167, 246.3920726737087534, -7.362905700427413436 ) ) ;
#77739 = CARTESIAN_POINT ( 'NONE',  ( 81.50752084980894097, 44.54043232651186912, 10.17210088699022918 ) ) ;
#77740 = CARTESIAN_POINT ( 'NONE',  ( 168.0039864032107459, 281.1839448478028771, 11.64247976579110144 ) ) ;
#77741 = CARTESIAN_POINT ( 'NONE',  ( 148.1974503712686158, 273.9614817352322120, -7.884397846570731616 ) ) ;
#77743 = EDGE_CURVE ( 'NONE', #14532, #46006, #33699, .T. ) ;
#77742 = B_SPLINE_CURVE_WITH_KNOTS ( 'NONE', 3,
 ( #85668, #86665, #17198, #78525, #55187, #9109, #46086, #48100, #1012, #7605, #16206, #23293, #38991, #39983, #93238, #76997, #62796, #32406, #79041, #20, #69407, #47098, #70918, #70400, #87182, #1526, #23797, #71422, #24797, #38492, #63304, #78020, #54180, #31890, #2013, #32898, #94739, #94245, #86170, #30905, #85148, #69896, #8610, #25301 ),
 .UNSPECIFIED., .F., .F.,
 ( 4, 2, 2, 2, 2, 2, 2, 2, 2, 2, 2, 2, 2, 2, 2, 2, 2, 2, 2, 2, 2, 4 ),
 ( 0.003093253362364405644, 0.003290131544961049769, 0.003487009727557693894, 0.003585448818856016174, 0.003683887910154338453, 0.003880766092751096203, 0.004274522457944560094, 0.004668278823138022685, 0.005455791553525046744, 0.006243304283912070804, 0.007030817014299093996, 0.007818329744686117189, 0.007916768835984536179, 0.008015207927282951700, 0.008064427472932161195, 0.008113647018581370690, 0.008212086109879786211, 0.008408964292476488883, 0.008605842475073191555, 0.008802720657669894228, 0.008999598840266596900, 0.009393355205460038673 ),
 .UNSPECIFIED. ) ;
#77744 = CARTESIAN_POINT ( 'NONE',  ( 174.8312020576883299, 289.9788226860209193, 6.252573175169373165 ) ) ;
#77745 = FACE_OUTER_BOUND ( 'NONE', #51055, .T. ) ;
#77746 = CARTESIAN_POINT ( 'NONE',  ( 81.73998748822677385, 54.58416966175224161, -16.14354867815247729 ) ) ;
#77747 = CARTESIAN_POINT ( 'NONE',  ( 18.76490627030545610, 13.76004757982088655, 5.678558825948272215 ) ) ;
#77748 = CARTESIAN_POINT ( 'NONE',  ( 199.9740574423823887, 278.2632206211216612, -15.47992833812561564 ) ) ;
#77749 = CARTESIAN_POINT ( 'NONE',  ( 80.01979875032591849, 57.54866692369599690, 16.59896302490740538 ) ) ;
#77751 = ORIENTED_EDGE ( 'NONE', *, *, #80993, .F. ) ;
#77750 = CARTESIAN_POINT ( 'NONE',  ( 198.0858447170796524, 287.5522480202560018, 18.44384186289807559 ) ) ;
#77752 = CARTESIAN_POINT ( 'NONE',  ( -22.42236680055709641, 157.8615022471902591, 0.000000000000000000 ) ) ;
#77753 = CARTESIAN_POINT ( 'NONE',  ( 206.5237403681858552, 272.9373840435757188, -10.81420335655575116 ) ) ;
#77754 = ADVANCED_FACE ( 'NONE', ( #75949 ), #84675, .F. ) ;
#77755 = FACE_OUTER_BOUND ( 'NONE', #83338, .T. ) ;
#77756 = CARTESIAN_POINT ( 'NONE',  ( 153.2819058590468160, 274.2512448977743134, -12.24885634829186287 ) ) ;
#77757 = ADVANCED_FACE ( 'NONE', ( #38400 ), #70821, .T. ) ;
#77758 = LINE ( 'NONE', #8341, #17617 ) ;
#77759 = CARTESIAN_POINT ( 'NONE',  ( 71.41016749218992743, 59.45273978182970609, 15.69346469599747174 ) ) ;
#77760 = VERTEX_POINT ( 'NONE', #85048 ) ;
#77761 = CARTESIAN_POINT ( 'NONE',  ( 155.3559454620313147, 261.5626045322989626, -17.00790974192431548 ) ) ;
#77762 = CARTESIAN_POINT ( 'NONE',  ( 128.4645176094212502, 251.6427522451419350, 10.00000000000009415 ) ) ;
#77763 = DIRECTION ( 'NONE',  ( -0.000000000000000000, 0.000000000000000000, -1.000000000000000000 ) ) ;
#77764 = CARTESIAN_POINT ( 'NONE',  ( 6.354935675815381657, 181.1427522451419350, 10.00000000000009237 ) ) ;
#77765 = CARTESIAN_POINT ( 'NONE',  ( 98.87557663705065636, 218.7048013555409796, 4.594050593750051981 ) ) ;
#77766 = CARTESIAN_POINT ( 'NONE',  ( 82.42089004567290544, 40.96640717916999108, -1.235892450584623381 ) ) ;
#77767 = CARTESIAN_POINT ( 'NONE',  ( 7.599693759758307188, 26.16126292948893806, -6.180339887498951690 ) ) ;
#77768 = CARTESIAN_POINT ( 'NONE',  ( 207.5492168967516875, 271.1612065941299079, 2.279797467183042325 ) ) ;
#77769 = CARTESIAN_POINT ( 'NONE',  ( 8.890927067706668296, 164.3932355074535394, -2.679491924311248496 ) ) ;
#77771 = CARTESIAN_POINT ( 'NONE',  ( 75.84828732440915644, 65.60728826867935481, 13.84218333541264556 ) ) ;
#77770 = CARTESIAN_POINT ( 'NONE',  ( 12.62459875707045143, 178.0958772461660544, -9.188101187500095079 ) ) ;
#77772 = CARTESIAN_POINT ( 'NONE',  ( 186.8123841630082040, 258.3999256946553942, 3.104652050626591553 ) ) ;
#77773 = EDGE_LOOP ( 'NONE', ( #62141, #96061, #22024, #4930 ) ) ;
#77775 = ORIENTED_EDGE ( 'NONE', *, *, #88112, .T. ) ;
#77774 = PRODUCT_DEFINITION_CONTEXT ( 'detailed design', #40519, 'design' ) ;
#77776 = DIRECTION ( 'NONE',  ( 0.8660254037844384856, 0.5000000000000002220, 0.000000000000000000 ) ) ;
#77777 = CARTESIAN_POINT ( 'NONE',  ( 189.0259968054108128, 261.1256047311666180, -6.165518503103954551 ) ) ;
#77778 = LINE ( 'NONE', #54429, #64772 ) ;
#77779 = CARTESIAN_POINT ( 'NONE',  ( 160.2571224103306236, 275.9534525238444758, -14.07895364344611977 ) ) ;
#77780 = DIRECTION ( 'NONE',  ( -0.000000000000000000, -0.000000000000000000, -1.000000000000000000 ) ) ;
#77781 = CARTESIAN_POINT ( 'NONE',  ( 178.7215982705234012, 283.0458118805923391, -16.00884060594773217 ) ) ;
#77782 = EDGE_CURVE ( 'NONE', #48220, #96813, #85572, .T. ) ;
#77783 = CARTESIAN_POINT ( 'NONE',  ( 34.27488675591641965, 202.8464784336661637, 1.353441290958777525E-15 ) ) ;
#77784 = CARTESIAN_POINT ( 'NONE',  ( 121.2293367285889616, 249.9869531367911293, 4.594050593750046652 ) ) ;
#77785 = CARTESIAN_POINT ( 'NONE',  ( 198.3441781175109497, 276.9090831475363075, 15.17843888428162735 ) ) ;
#77786 = EDGE_LOOP ( 'NONE', ( #95165, #55374, #31982, #65380 ) ) ;
#77787 = CARTESIAN_POINT ( 'NONE',  ( 150.2864214986432501, 271.8288624510125828, -11.67904241962729728 ) ) ;
#77788 = EDGE_CURVE ( 'NONE', #10368, #2343, #81894, .T. ) ;
#77789 = EDGE_CURVE ( 'NONE', #35626, #90703, #68223, .T. ) ;
#77790 = CARTESIAN_POINT ( 'NONE',  ( 181.6873167589662330, 259.7205209471545118, -11.14285176367228836 ) ) ;
#77791 = CARTESIAN_POINT ( 'NONE',  ( 168.4945589903323366, 288.0950524468156004, -4.184919968760112852 ) ) ;
#77792 = CARTESIAN_POINT ( 'NONE',  ( 80.50903874866318688, 57.12766137858866244, -16.22900141427163945 ) ) ;
#77793 = LINE ( 'NONE', #78788, #1459 ) ;
#77794 = CARTESIAN_POINT ( 'NONE',  ( 207.7666684749232786, 270.7845694125510931, -6.630926507062123498 ) ) ;
#77795 = CARTESIAN_POINT ( 'NONE',  ( 147.8819534105757043, 274.5079385007862811, -9.338341377131436971 ) ) ;
#77796 = CARTESIAN_POINT ( 'NONE',  ( 148.1974503712686158, 273.9614817352322120, -7.884397846570731616 ) ) ;
#77797 = EDGE_CURVE ( 'NONE', #78204, #166, #64725, .T. ) ;
#77798 = EDGE_CURVE ( 'NONE', #27243, #76018, #40888, .T. ) ;
#77799 = CARTESIAN_POINT ( 'NONE',  ( 189.3330452661960237, 262.4894502133154788, 8.166639359185952074 ) ) ;
#77800 = CARTESIAN_POINT ( 'NONE',  ( 165.0066022244254498, 249.8389599805948080, -10.62953420576023511 ) ) ;
#77801 = CARTESIAN_POINT ( 'NONE',  ( 68.45082498735337140, 68.05190841428618853, 7.383510520589708470 ) ) ;
#77802 = CARTESIAN_POINT ( 'NONE',  ( 190.5893431400089923, 300.5365696307625853, -0.3099240395267599535 ) ) ;
#77803 = CARTESIAN_POINT ( 'NONE',  ( 181.0854462269685428, 266.2271372736428816, -14.79605532646364097 ) ) ;
#77804 = VERTEX_POINT ( 'NONE', #9534 ) ;
#77805 = CARTESIAN_POINT ( 'NONE',  ( 153.0234837362991698, 266.8886651207910177, -16.12888749788869447 ) ) ;
#77806 = CIRCLE ( 'NONE', #30854, 70.00000000000001421 ) ;
#77807 = DIRECTION ( 'NONE',  ( -0.8916269620120497175, 0.4527707594502572430, 0.000000000000000000 ) ) ;
#77808 = CARTESIAN_POINT ( 'NONE',  ( 102.3121810886138832, 236.0024278399160949, 9.188101187500095079 ) ) ;
#77809 = CARTESIAN_POINT ( 'NONE',  ( 14.38185574516869458, 23.70171378149918695, -9.188101187500004485 ) ) ;
#77810 = CARTESIAN_POINT ( 'NONE',  ( 191.3375250863502970, 299.2406804863936145, 8.828791580707859410 ) ) ;
#77811 = DIRECTION ( 'NONE',  ( -0.8614378286617615510, 0.5078630399532039208, 0.000000000000000000 ) ) ;
#77813 = CARTESIAN_POINT ( 'NONE',  ( 86.53906990778989439, 43.21878081143324835, -0.5596625769422287622 ) ) ;
#77812 = CARTESIAN_POINT ( 'NONE',  ( 66.19292216254950745, 68.59989815790002865, 2.318610380053390596 ) ) ;
#77814 = LINE ( 'NONE', #1803, #30308 ) ;
#77815 = CARTESIAN_POINT ( 'NONE',  ( 198.4522155198218059, 286.9176751754968109, -17.57438352224490075 ) ) ;
#77816 = CARTESIAN_POINT ( 'NONE',  ( 144.7927049134883077, 247.7365022471901739, -10.00000000000009237 ) ) ;
#77817 = CARTESIAN_POINT ( 'NONE',  ( 45.41683807177152943, 29.14754757982093736, -5.678558825948275768 ) ) ;
#77818 = CARTESIAN_POINT ( 'NONE',  ( 40.15112871924374360, 31.38052372038644577, 10.00000000000000533 ) ) ;
#77819 = CARTESIAN_POINT ( 'NONE',  ( 81.50691414224651510, 55.96606086945440950, -16.03680236514553314 ) ) ;
#77820 = VERTEX_POINT ( 'NONE', #32810 ) ;
#77821 = CARTESIAN_POINT ( 'NONE',  ( 192.8818986906848636, 267.2098981360021526, 11.18199646913336842 ) ) ;
#77822 = LINE ( 'NONE', #32193, #50689 ) ;
#77823 = CARTESIAN_POINT ( 'NONE',  ( 196.5239536785732923, 267.5882975073278089, 9.598076446533468697 ) ) ;
#77824 = CARTESIAN_POINT ( 'NONE',  ( 187.0605947865943222, 282.7524552142733114, -17.49343033980654027 ) ) ;
#77825 = CARTESIAN_POINT ( 'NONE',  ( 75.14966582671556239, 65.99894161753822175, 13.81944563728900377 ) ) ;
#77826 = DIRECTION ( 'NONE',  ( 1.000000000000000000, 0.000000000000000000, 0.000000000000000000 ) ) ;
#77827 = CARTESIAN_POINT ( 'NONE',  ( 169.8745519614330419, 281.1702744907113356, -14.29939960421313039 ) ) ;
#77828 = B_SPLINE_CURVE_WITH_KNOTS ( 'NONE', 3,
 ( #73075, #89786, #88823, #43123 ),
 .UNSPECIFIED., .F., .F.,
 ( 4, 4 ),
 ( 0.01763317218926846799, 0.02658475294366728983 ),
 .UNSPECIFIED. ) ;
#77829 = EDGE_LOOP ( 'NONE', ( #26566, #46329, #88029, #27570, #81600, #43039, #82618, #93692, #75504, #84502, #9951, #87512, #79571, #98182, #73237, #96094, #16345, #47203, #85480, #56129 ) ) ;
#77830 = CARTESIAN_POINT ( 'NONE',  ( 73.20446552614963309, 69.86374744967437778, 9.599577609524185817 ) ) ;
#77831 = CARTESIAN_POINT ( 'NONE',  ( 36.06377727768691699, 41.79752408145595410, -5.678558825948271327 ) ) ;
#77832 = ORIENTED_EDGE ( 'NONE', *, *, #74704, .T. ) ;
#77833 = CARTESIAN_POINT ( 'NONE',  ( 164.6836044745662377, 247.6625381034837403, 7.171422519083344049 ) ) ;
#77834 = EDGE_CURVE ( 'NONE', #6810, #57758, #72845, .T. ) ;
#77835 = DIRECTION ( 'NONE',  ( -0.8660254037844387076, -0.4999999999999998890, -0.000000000000000000 ) ) ;
#77836 = CARTESIAN_POINT ( 'NONE',  ( 157.2674082780516471, 258.2518538181732879, 18.34755329151241554 ) ) ;
#77837 = EDGE_LOOP ( 'NONE', ( #67969, #5681, #4962, #15017 ) ) ;
#77838 = CARTESIAN_POINT ( 'NONE',  ( 86.46583077919046900, 47.10391736892673009, -10.05241405704699353 ) ) ;
#77839 = DIRECTION ( 'NONE',  ( -0.9879428538673719062, -0.1548189829846212673, 0.000000000000000000 ) ) ;
#77840 = CARTESIAN_POINT ( 'NONE',  ( 193.1926327199271327, 296.0275398115294934, -12.21752165518055833 ) ) ;
#77841 = CARTESIAN_POINT ( 'NONE',  ( 85.42383634753986144, 44.41940826771883621, -7.937727123839215082 ) ) ;
#77842 = FACE_OUTER_BOUND ( 'NONE', #96828, .T. ) ;
#77843 = DIRECTION ( 'NONE',  ( -0.8660254037844377084, -0.5000000000000014433, -0.000000000000000000 ) ) ;
#77844 = ORIENTED_EDGE ( 'NONE', *, *, #30650, .T. ) ;
#77845 = CARTESIAN_POINT ( 'NONE',  ( 162.7020145476934090, 284.0983276010327359, 6.051621772638641872 ) ) ;
#77846 = ORIENTED_EDGE ( 'NONE', *, *, #53213, .T. ) ;
#77847 = CARTESIAN_POINT ( 'NONE',  ( 81.18434463996317163, 55.62183548715842107, 16.37412944077603782 ) ) ;
#77848 = EDGE_LOOP ( 'NONE', ( #19552, #83580, #62558 ) ) ;
#77849 = CARTESIAN_POINT ( 'NONE',  ( 172.6226713180010961, 270.9341145373659856, 16.43373278848542540 ) ) ;
#77850 = CARTESIAN_POINT ( 'NONE',  ( 78.31144745436395738, 49.34677990821563753, 14.65856222115218443 ) ) ;
#77851 = VERTEX_POINT ( 'NONE', #2435 ) ;
#77852 = CARTESIAN_POINT ( 'NONE',  ( 164.5259176133158689, 246.1953198488120051, 1.882264443804981813 ) ) ;
#77853 = CARTESIAN_POINT ( 'NONE',  ( 34.02846334099481140, 24.81029122506296503, 8.090169943749479842 ) ) ;
#77854 = CARTESIAN_POINT ( 'NONE',  ( 147.6272645182038161, 274.9490726024977789, -5.838234932324007254 ) ) ;
#77855 = CARTESIAN_POINT ( 'NONE',  ( 190.0259678364800493, 301.5123642802043946, 4.004183174499006626 ) ) ;
#77856 = CARTESIAN_POINT ( 'NONE',  ( 75.51323141522172477, 65.35427051582675517, 13.87231131232226744 ) ) ;
#77857 = CARTESIAN_POINT ( 'NONE',  ( 170.4391975808936479, 250.6982047760319858, -5.514033325473483238 ) ) ;
#77858 = CYLINDRICAL_SURFACE ( 'NONE', #84177, 10.00000000000010658 ) ;
#77859 = B_SPLINE_CURVE_WITH_KNOTS ( 'NONE', 3,
 ( #99534, #51931, #60496, #53408, #30116, #43816, #60998, #5334, #21050, #82872, #36215, #36711, #67618, #29136, #60004, #21531, #75740, #37213, #30621, #76715, #68114, #91969, #91453, #99039, #52912, #22515, #14905, #83864, #82384, #12953, #7309, #14429, #45309, #38191, #20543, #100034, #74754, #89964, #23000, #85882, #78229, #47793, #38702, #24508, #40697, #46810 ),
 .UNSPECIFIED., .F., .F.,
 ( 4, 1, 2, 2, 1, 2, 2, 1, 1, 2, 2, 1, 1, 2, 2, 1, 1, 2, 2, 1, 1, 1, 2, 2, 1, 1, 1, 2, 2, 4 ),
 ( 0.000000000000000000, 0.06250000000000975608, 0.09375000000001376677, 0.1250000000000177913, 0.1875000000000250910, 0.2187500000000290601, 0.2500000000000330291, 0.3125000000000403011, 0.3437500000000449085, 0.3593750000000467959, 0.3750000000000486278, 0.4375000000000480727, 0.4687500000000481282, 0.4843750000000476286, 0.5000000000000470735, 0.5625000000000482947, 0.5937500000000489608, 0.6093750000000479616, 0.6250000000000469624, 0.6875000000000460743, 0.7187500000000449640, 0.7343750000000438538, 0.7421875000000432987, 0.7500000000000426326, 0.8125000000000284217, 0.8437500000000207612, 0.8593750000000167644, 0.8671875000000155431, 0.8750000000000143219, 1.000000000000000000 ),
 .UNSPECIFIED. ) ;
#77860 = ADVANCED_FACE ( 'NONE', ( #56092 ), #87085, .T. ) ;
#77861 = CARTESIAN_POINT ( 'NONE',  ( -50.24117156905492720, 92.72553494444620981, 36.50000000000000000 ) ) ;
#77862 = CARTESIAN_POINT ( 'NONE',  ( 124.1796696299359724, 236.3768266524159856, -9.188101187500091527 ) ) ;
#77863 = CARTESIAN_POINT ( 'NONE',  ( 186.6174597086819631, 262.7463543296344142, -9.059254040013616560 ) ) ;
#77864 = CARTESIAN_POINT ( 'NONE',  ( 42.15722797529793553, 32.84335787977767041, 9.188101187500006262 ) ) ;
#77865 = CARTESIAN_POINT ( 'NONE',  ( 177.4671251619221550, 288.9374044400234425, -9.330515757822047007 ) ) ;
#77866 = ORIENTED_EDGE ( 'NONE', *, *, #21264, .T. ) ;
#77867 = ORIENTED_EDGE ( 'NONE', *, *, #41272, .T. ) ;
#77868 = CARTESIAN_POINT ( 'NONE',  ( 200.1964548776884101, 273.9920713698066379, 13.59980230080865837 ) ) ;
#77869 = CARTESIAN_POINT ( 'NONE',  ( 81.74119788692269140, 59.14441083166271085, 0.000000000000000000 ) ) ;
#77870 = CARTESIAN_POINT ( 'NONE',  ( 174.2452046127573908, 290.2058683568998845, -4.780677047540736524 ) ) ;
#77871 = CARTESIAN_POINT ( 'NONE',  ( 196.0034224882197975, 291.1591091234520263, 17.53794140922627776 ) ) ;
#77872 = CARTESIAN_POINT ( 'NONE',  ( 72.55405144367838943, 63.78809379931346513, 13.69945044486563468 ) ) ;
#77873 = EDGE_CURVE ( 'NONE', #99249, #48842, #23114, .T. ) ;
#77874 = CARTESIAN_POINT ( 'NONE',  ( 66.66373457531125268, 68.30566046464788599, 4.557399502277720060 ) ) ;
#77875 = CARTESIAN_POINT ( 'NONE',  ( 77.99681166185179393, 50.47661464015640576, 15.62787934327010397 ) ) ;
#77876 = CARTESIAN_POINT ( 'NONE',  ( -50.41871976035449165, 31.58591985673634639, 10.00000000000000000 ) ) ;
#77877 = EDGE_CURVE ( 'NONE', #56899, #37919, #96654, .T. ) ;
#77878 = AXIS2_PLACEMENT_3D ( 'NONE', #31956, #16764, #47655 ) ;
#77879 = CARTESIAN_POINT ( 'NONE',  ( 174.0182248954802731, 253.4737597407804515, -7.581100471685894071 ) ) ;
#77880 = ORIENTED_EDGE ( 'NONE', *, *, #77063, .F. ) ;
#77881 = CARTESIAN_POINT ( 'NONE',  ( 194.9455394410084921, 292.9914163096879065, -15.01116663483170655 ) ) ;
#77882 = CARTESIAN_POINT ( 'NONE',  ( 65.74496443904322973, 69.08459607026262006, -0.1437899284560469337 ) ) ;
#77883 = VERTEX_POINT ( 'NONE', #79462 ) ;
#77884 = DIRECTION ( 'NONE',  ( -0.8660254037844377084, -0.5000000000000014433, -0.000000000000000000 ) ) ;
#77885 = CARTESIAN_POINT ( 'NONE',  ( 160.2241445597728102, 279.1506239025324589, 10.70181301040688204 ) ) ;
#77886 = CARTESIAN_POINT ( 'NONE',  ( 192.4441357708844578, 262.6530372631752925, 4.622430316263682393 ) ) ;
#77887 = CARTESIAN_POINT ( 'NONE',  ( 190.5477107455830321, 300.6086790531491033, 3.126266616601216963 ) ) ;
#77888 = CARTESIAN_POINT ( 'NONE',  ( 204.7130176219587554, 272.9107139802454753, -10.75958745166956909 ) ) ;
#77890 = CARTESIAN_POINT ( 'NONE',  ( 160.8497281054386576, 281.5906459864224871, 5.647281140516729359 ) ) ;
#77889 = CARTESIAN_POINT ( 'NONE',  ( 153.4696322588327178, 270.0294559819171809, 15.09029231870687937 ) ) ;
#77891 = CARTESIAN_POINT ( 'NONE',  ( 152.9273493951901628, 265.7690563111299298, -17.70273273795505631 ) ) ;
#77892 = ORIENTED_EDGE ( 'NONE', *, *, #47272, .T. ) ;
#77893 = CARTESIAN_POINT ( 'NONE',  ( 190.6218339396177441, 300.4802939150614520, -4.178005820806754755 ) ) ;
#77894 = LINE ( 'NONE', #61665, #51336 ) ;
#77895 = CARTESIAN_POINT ( 'NONE',  ( 187.2956951681344151, 261.7326779137165431, -8.891522745801257344 ) ) ;
#77896 = DIRECTION ( 'NONE',  ( -1.000000000000000000, 0.000000000000000000, 0.000000000000000000 ) ) ;
#77897 = CARTESIAN_POINT ( 'NONE',  ( 193.3429555150086685, 288.0943436124296113, -17.13583794773776248 ) ) ;
#77898 = CARTESIAN_POINT ( 'NONE',  ( 167.7444804051520748, 288.1361480929475078, -1.744605501772117595 ) ) ;
#77899 = B_SPLINE_CURVE_WITH_KNOTS ( 'NONE', 3,
 ( #97127, #89535, #90527, #20096, #21098, #36759, #62032, #78271, #14944, #45834 ),
 .UNSPECIFIED., .F., .F.,
 ( 4, 2, 2, 2, 4 ),
 ( 0.000000000000000000, 0.0002622400424272595238, 0.0005244800848545190476, 0.0007867201272817785172, 0.001048960169709038095 ),
 .UNSPECIFIED. ) ;
#77900 = CARTESIAN_POINT ( 'NONE',  ( 204.3548082856772794, 276.0577276202552071, 13.12054476288156302 ) ) ;
#77901 = CARTESIAN_POINT ( 'NONE',  ( 155.5770330754656072, 261.1796695529068302, 18.26969263326161297 ) ) ;
#77902 = DIRECTION ( 'NONE',  ( 0.9213551052231946370, -0.3887219701523905724, 0.000000000000000000 ) ) ;
#77903 = EDGE_CURVE ( 'NONE', #14650, #5695, #20834, .T. ) ;
#77904 = CARTESIAN_POINT ( 'NONE',  ( -5.399381411310669066, 161.5643266524160140, -9.188101187500093303 ) ) ;
#77905 = CARTESIAN_POINT ( 'NONE',  ( 88.13101510164371177, 227.8149278399160949, -9.188101187500095079 ) ) ;
#77906 = CARTESIAN_POINT ( 'NONE',  ( 147.0314375879888757, 275.9810751181479986, -5.168577011192616588 ) ) ;
#77907 = CARTESIAN_POINT ( 'NONE',  ( 208.2124092825819162, 270.0125236866795149, -2.339659020816897694 ) ) ;
#77908 = CARTESIAN_POINT ( 'NONE',  ( 155.5066938333533528, 261.3015006940112244, -18.40036130547566273 ) ) ;
#77909 = CARTESIAN_POINT ( 'NONE',  ( 78.27615213422006946, 56.24099877768735922, 16.18748323720173943 ) ) ;
#77910 = DIRECTION ( 'NONE',  ( 1.716797197045744035E-15, -2.973579971575064630E-15, 1.000000000000000000 ) ) ;
#77912 = CARTESIAN_POINT ( 'NONE',  ( 75.99893621847269287, 51.39177364591706265, 15.66710071473398358 ) ) ;
#77911 = CARTESIAN_POINT ( 'NONE',  ( 73.61134034488466682, 69.26824756038205066, -9.998744155463656469 ) ) ;
#77913 = CARTESIAN_POINT ( 'NONE',  ( 207.5088755035018551, 271.2310799368871699, 6.444438407027963223 ) ) ;
#77914 = CARTESIAN_POINT ( 'NONE',  ( 73.76584831522595209, 68.38082682530665579, 11.49424229391075514 ) ) ;
#77915 = DIRECTION ( 'NONE',  ( 0.4999999999999998890, -0.8660254037844385966, 0.000000000000000000 ) ) ;
#77916 = CARTESIAN_POINT ( 'NONE',  ( 157.7365441389748923, 257.4392866714015895, 18.13124212464487073 ) ) ;
#77917 = CYLINDRICAL_SURFACE ( 'NONE', #59198, 17.82106496071139645 ) ;
#77918 = CARTESIAN_POINT ( 'NONE',  ( 38.38920161542251464, 180.7202760586659451, -5.415160957724236172E-17 ) ) ;
#77919 = CARTESIAN_POINT ( 'NONE',  ( 69.59257202794182717, 220.1744531367911293, 4.594050593750047540 ) ) ;
#77920 = CARTESIAN_POINT ( 'NONE',  ( 52.35966550219796289, 188.3352228055615001, 4.537668576076727307E-14 ) ) ;
#77921 = CARTESIAN_POINT ( 'NONE',  ( 88.01740701321664062, 43.99393894108155934, 0.5439121987275350456 ) ) ;
#77922 = CARTESIAN_POINT ( 'NONE',  ( 10.80369284495069238, 14.43677371833799583, -10.00000000000000355 ) ) ;
#77923 = CARTESIAN_POINT ( 'NONE',  ( -9.864998445682726214, 165.1115022471902591, 10.00000000000009592 ) ) ;
#77925 = DIRECTION ( 'NONE',  ( -0.8660254037844387076, -0.4999999999999998890, -0.000000000000000000 ) ) ;
#77924 = LINE ( 'NONE', #44123, #6404 ) ;
#77926 = ADVANCED_FACE ( 'NONE', ( #71837 ), #57599, .F. ) ;
#77927 = DIRECTION ( 'NONE',  ( -0.000000000000000000, 0.000000000000000000, 1.000000000000000000 ) ) ;
#77928 = CARTESIAN_POINT ( 'NONE',  ( 27.58635055662477598, 24.43085787977765122, -9.188101187500008038 ) ) ;
#77929 = CARTESIAN_POINT ( 'NONE',  ( 198.7357616895271804, 286.4265588032756114, -17.04018524297827497 ) ) ;
#77930 = CARTESIAN_POINT ( 'NONE',  ( 80.23656086893576855, 47.63841505922916753, -13.26053850169819803 ) ) ;
#77931 = CARTESIAN_POINT ( 'NONE',  ( 10.40777469057294091, 26.98502408145591502, -5.678558825948271327 ) ) ;
#77932 = CARTESIAN_POINT ( 'NONE',  ( 54.35602435405059651, 208.3149278399161233, -9.188101187500095079 ) ) ;
#77933 = CARTESIAN_POINT ( 'NONE',  ( 77.14069742968855792, 63.65222853049024110, 15.02831949864487271 ) ) ;
#77934 = CARTESIAN_POINT ( 'NONE',  ( 18.52134341065868384, 22.64441083166259716, 0.000000000000000000 ) ) ;
#77935 = CARTESIAN_POINT ( 'NONE',  ( 159.9628729326222754, 253.5831720864507588, 15.75051413866357386 ) ) ;
#77936 = CARTESIAN_POINT ( 'NONE',  ( 74.12249027442281601, 67.16814668724251192, 12.15174938425090012 ) ) ;
#77937 = CARTESIAN_POINT ( 'NONE',  ( 201.3854624970792599, 281.8371423797387934, 17.49239072403049988 ) ) ;
#77938 = VECTOR ( 'NONE', #99857, 999.9999999999998863 ) ;
#77939 = CARTESIAN_POINT ( 'NONE',  ( 74.89708722414906106, 56.88665470694825643, -16.07962807653123605 ) ) ;
#77940 = CARTESIAN_POINT ( 'NONE',  ( 87.68902078672120126, 44.98529012857299136, -6.607530655827392074 ) ) ;
#77941 = CARTESIAN_POINT ( 'NONE',  ( 111.0177141658951854, 228.2365022471901739, -10.00000000000009059 ) ) ;
#77942 = CARTESIAN_POINT ( 'NONE',  ( 161.5056331467593225, 250.9110330116698435, 14.52719814064025528 ) ) ;
#77943 = CARTESIAN_POINT ( 'NONE',  ( 164.7243055739305078, 245.3361288348881999, -1.445094907380085170 ) ) ;
#77944 = VERTEX_POINT ( 'NONE', #27224 ) ;
#77945 = CARTESIAN_POINT ( 'NONE',  ( 77.37658274812778814, 49.21614173473252407, 15.31778251827114623 ) ) ;
#77946 = CARTESIAN_POINT ( 'NONE',  ( 184.7502022281630047, 271.1445130452900685, 16.43725824281414560 ) ) ;
#77947 = ORIENTED_EDGE ( 'NONE', *, *, #9427, .F. ) ;
#77948 = CARTESIAN_POINT ( 'NONE',  ( 206.0946696452135427, 273.6805563358039421, -10.19627505985792837 ) ) ;
#77949 = CARTESIAN_POINT ( 'NONE',  ( 194.1728500316723967, 293.9464425811553383, 14.07605957608015501 ) ) ;
#77950 = CARTESIAN_POINT ( 'NONE',  ( 69.95819854987405506, 68.88853697437434676, -7.495272743277247685 ) ) ;
#77951 = ORIENTED_EDGE ( 'NONE', *, *, #9867, .T. ) ;
#77952 = CARTESIAN_POINT ( 'NONE',  ( 173.5253749324791954, 251.2404134093094683, 0.4681658163635857850 ) ) ;
#77953 = ORIENTED_EDGE ( 'NONE', *, *, #13954, .T. ) ;
#77954 = CARTESIAN_POINT ( 'NONE',  ( 65.92723761088207368, 68.94945291059251247, -2.624861928015910895 ) ) ;
#77955 = CARTESIAN_POINT ( 'NONE',  ( 194.3541845315608612, 294.0156730581561533, -14.67567721756631016 ) ) ;
#77956 = PLANE ( 'NONE',  #69281 ) ;
#77957 = ORIENTED_EDGE ( 'NONE', *, *, #84044, .F. ) ;
#77958 = CARTESIAN_POINT ( 'NONE',  ( 23.41017057962146097, 28.91421378149919619, 9.188101187500008038 ) ) ;
#77959 = CARTESIAN_POINT ( 'NONE',  ( 22.44857442947618154, 193.7677522451419350, -5.000000000000047962 ) ) ;
#77960 = CARTESIAN_POINT ( 'NONE',  ( 75.07321287302792712, 66.36857194797330806, -13.14009733065324070 ) ) ;
#77961 = VERTEX_POINT ( 'NONE', #56611 ) ;
#77962 = CARTESIAN_POINT ( 'NONE',  ( 141.2767884429413243, 240.8262482093457777, 3.021315404115420679E-15 ) ) ;
#77963 = FACE_OUTER_BOUND ( 'NONE', #43681, .T. ) ;
#77964 = EDGE_LOOP ( 'NONE', ( #61966, #85669, #62348, #31238 ) ) ;
#77965 = CARTESIAN_POINT ( 'NONE',  ( 172.4923911848786702, 285.1025841718646916, 10.57918879521990618 ) ) ;
#77967 = CARTESIAN_POINT ( 'NONE',  ( 67.98680250238912492, 65.22133151511555127, -10.62698878092350085 ) ) ;
#77966 = CARTESIAN_POINT ( 'NONE',  ( 163.2715301498190854, 283.7935623289845921, -2.937509578771470675 ) ) ;
#77968 = CARTESIAN_POINT ( 'NONE',  ( 208.2912792141756029, 269.8759169579697641, -2.198672330625011995 ) ) ;
#77969 = CARTESIAN_POINT ( 'NONE',  ( 155.0898745997320134, 262.0234527842152374, 17.05457557403769542 ) ) ;
#77970 = CARTESIAN_POINT ( 'NONE',  ( 185.4923030054532092, 292.6699065248636202, -10.71444798707586621 ) ) ;
#77971 = CARTESIAN_POINT ( 'NONE',  ( 205.3708847852691406, 274.9341884869767227, -13.70973585089674174 ) ) ;
#77972 = CARTESIAN_POINT ( 'NONE',  ( 147.5084024922618084, 243.7202760586659167, -5.415160957724236172E-17 ) ) ;
#77973 = CARTESIAN_POINT ( 'NONE',  ( 206.4627041557072573, 270.6281706969085121, 2.566430978744102198 ) ) ;
#77974 = CARTESIAN_POINT ( 'NONE',  ( 182.6873171513263969, 259.2587024686063160, 9.588166490408216447 ) ) ;
#77975 = CARTESIAN_POINT ( 'NONE',  ( 85.53293889029040997, 226.3149278399160949, -9.188101187500095079 ) ) ;
#77977 = ORIENTED_EDGE ( 'NONE', *, *, #52200, .T. ) ;
#77976 = B_SPLINE_CURVE_WITH_KNOTS ( 'NONE', 3,
 ( #8147, #93272, #40020, #79589, #545, #69928, #31428, #62830, #63342, #17755, #93786, #54723, #92774, #24346, #48656, #8643, #56227, #40527, #23328, #86699, #86201, #10153, #85704, #41019, #71462, #16240, #32935, #24835, #16740, #47629, #47131, #55709 ),
 .UNSPECIFIED., .F., .F.,
 ( 4, 2, 2, 2, 2, 2, 2, 2, 2, 2, 2, 2, 2, 2, 2, 4 ),
 ( 0.0005803556464477676669, 0.001213002923345877972, 0.001845650200243988386, 0.003110944754040269496, 0.003743592030938444962, 0.004059915669387570425, 0.004138996578999795846, 0.004178537033805908990, 0.004218077488612021267, 0.004257617943418134411, 0.004297158398224247555, 0.004376239307836427006, 0.004692562946285125727, 0.005008886584733824449, 0.005325210223182522302, 0.005641533861631220156 ),
 .UNSPECIFIED. ) ;
#77978 = CARTESIAN_POINT ( 'NONE',  ( 150.7254409736883645, 269.5828735707850683, 14.54962197351449049 ) ) ;
#77979 = CARTESIAN_POINT ( 'NONE',  ( 162.0670251645566680, 279.3129746912387645, 12.26946893937585337 ) ) ;
#77980 = CARTESIAN_POINT ( 'NONE',  ( 77.84440724905273612, 61.40677674231441330, -16.14086307328630809 ) ) ;
#77981 = ORIENTED_EDGE ( 'NONE', *, *, #76496, .F. ) ;
#77982 = CARTESIAN_POINT ( 'NONE',  ( 157.4297042318662534, 257.9707489803037674, -17.23334323327960149 ) ) ;
#77983 = ORIENTED_EDGE ( 'NONE', *, *, #17613, .T. ) ;
#77984 = ORIENTED_EDGE ( 'NONE', *, *, #17117, .F. ) ;
#77985 = CARTESIAN_POINT ( 'NONE',  ( 80.02753730852559499, 44.42912664858859273, -10.91029207558068670 ) ) ;
#77986 = DIRECTION ( 'NONE',  ( -0.6363689690731114679, -0.7713848165480218233, 0.000000000000000000 ) ) ;
#77988 = B_SPLINE_SURFACE_WITH_KNOTS ( 'NONE', 3, 1, ( 
 ( #45082, #28386 ),
 ( #98314, #76020 ),
 ( #66887, #35983 ),
 ( #6597, #99306 ),
 ( #44073, #5592 ),
 ( #5104, #36482 ),
 ( #74524, #60267 ),
 ( #59266, #6091 ),
 ( #97819, #20815 ),
 ( #13214, #67386 ),
 ( #68872, #83128 ),
 ( #52673, #29886 ),
 ( #83633, #28903 ),
 ( #59780, #75506 ),
 ( #90747, #7078 ),
 ( #53186, #61272 ),
 ( #15166, #60760 ),
 ( #21303, #52179 ),
 ( #91722, #22286 ),
 ( #13699, #37965 ),
 ( #44571, #84142 ),
 ( #14690, #45571 ),
 ( #30386, #22790 ),
 ( #8096, #10981 ),
 ( #2890, #69876 ),
 ( #46567, #7581 ),
 ( #77504, #38971 ),
 ( #18577, #85641 ),
 ( #88524, #16188 ),
 ( #489, #33786 ),
 ( #72798, #49455 ) ),
 .UNSPECIFIED., .F., .F., .F.,
 ( 4, 3, 3, 3, 3, 3, 3, 3, 3, 3, 4 ),
 ( 2, 2 ),
 ( 0.000000000000000000, 0.1122669598086537268, 0.2243161639709344568, 0.3396355846218790386, 0.4553962076584738838, 0.5677860799921967683, 0.6749047109689209067, 0.7773884377078009722, 0.8775581155833749314, 0.9782364162377522598, 1.000000000000000000 ),
 ( 0.000000000000000000, 1.000000000000000000 ),
 .UNSPECIFIED. ) ;
#77987 = LINE ( 'NONE', #9079, #85450 ) ;
#77989 = CARTESIAN_POINT ( 'NONE',  ( 40.34888600819125060, 126.6204015641749834, -10.00000000000000000 ) ) ;
#77990 = CARTESIAN_POINT ( 'NONE',  ( 48.42933654300934876, 208.7677522451419350, -5.000000000000047962 ) ) ;
#77991 = EDGE_CURVE ( 'NONE', #79111, #34466, #17017, .T. ) ;
#77992 = CARTESIAN_POINT ( 'NONE',  ( -21.31413092498266693, 24.33771760303832465, -10.00000000000000000 ) ) ;
#77993 = CARTESIAN_POINT ( 'NONE',  ( 81.52757139778736928, 224.0024278399160949, 9.188101187500095079 ) ) ;
#77994 = ORIENTED_EDGE ( 'NONE', *, *, #56591, .F. ) ;
#77995 = EDGE_CURVE ( 'NONE', #51013, #2862, #97155, .T. ) ;
#77996 = ORIENTED_EDGE ( 'NONE', *, *, #27655, .T. ) ;
#77997 = EDGE_CURVE ( 'NONE', #49393, #71997, #75827, .T. ) ;
#77998 = ORIENTED_EDGE ( 'NONE', *, *, #36213, .F. ) ;
#77999 = CARTESIAN_POINT ( 'NONE',  ( 24.22498904768565353, 14.39040679176983062, 1.333680081654574804E-15 ) ) ;
#78000 = ADVANCED_FACE ( 'NONE', ( #29216 ), #86368, .F. ) ;
#78001 = CARTESIAN_POINT ( 'NONE',  ( 75.92541454099094267, 65.74968322642241958, -14.18997729123868901 ) ) ;
#78002 = CARTESIAN_POINT ( 'NONE',  ( 200.5407427438653656, 272.3366537803537994, -12.86405620053299614 ) ) ;
#78003 = CARTESIAN_POINT ( 'NONE',  ( 207.4163210057841127, 270.9512484179036278, -1.435526549205535130 ) ) ;
#78004 = CARTESIAN_POINT ( 'NONE',  ( 87.66889377758084834, 44.69705958948441094, 5.015779035299128275 ) ) ;
#78005 = ORIENTED_EDGE ( 'NONE', *, *, #93241, .T. ) ;
#78006 = CARTESIAN_POINT ( 'NONE',  ( 189.0134143059085261, 294.9326290385585025, 11.47382056046370735 ) ) ;
#78007 = DIRECTION ( 'NONE',  ( -0.8660254037844387076, -0.4999999999999998890, -0.000000000000000000 ) ) ;
#78008 = CARTESIAN_POINT ( 'NONE',  ( 207.1181895030469491, 269.9077679394811753, 1.745611964362854929 ) ) ;
#78009 = CARTESIAN_POINT ( 'NONE',  ( 153.4542976351440302, 264.8563551865710224, -17.11782692037292009 ) ) ;
#78010 = SHAPE_REPRESENTATION ( 'Middle Movable Base', ( #68784 ), #81782 ) ;
#78011 = CARTESIAN_POINT ( 'NONE',  ( 204.2143397907769611, 276.5280330293650195, 13.36303585211030054 ) ) ;
#78012 = CARTESIAN_POINT ( 'NONE',  ( -110.0000000000000142, -8.000000000000000000, -9.212605237762117483 ) ) ;
#78013 = ORIENTED_EDGE ( 'NONE', *, *, #44813, .T. ) ;
#78014 = CARTESIAN_POINT ( 'NONE',  ( 196.1671714888020972, 264.5940953169613294, 5.402994724792868020 ) ) ;
#78015 = B_SPLINE_CURVE_WITH_KNOTS ( 'NONE', 3,
 ( #60332, #74592, #81708, #51249 ),
 .UNSPECIFIED., .F., .F.,
 ( 4, 4 ),
 ( 0.04823799508478943121, 0.04887066958154930724 ),
 .UNSPECIFIED. ) ;
#78016 = CARTESIAN_POINT ( 'NONE',  ( 153.6323727466833873, 269.3172676078306154, -15.66543061290010641 ) ) ;
#78017 = FACE_OUTER_BOUND ( 'NONE', #11568, .T. ) ;
#78018 = CARTESIAN_POINT ( 'NONE',  ( 187.9080819789693919, 266.1900786697327703, -11.89483730255598282 ) ) ;
#78019 = CYLINDRICAL_SURFACE ( 'NONE', #36965, 17.82106496071139645 ) ;
#78020 = CARTESIAN_POINT ( 'NONE',  ( 153.2977412669953310, 270.3394998157883720, 13.96444872914787716 ) ) ;
#78021 = EDGE_LOOP ( 'NONE', ( #95736, #26744, #20404, #88043, #51397 ) ) ;
#78022 = CARTESIAN_POINT ( 'NONE',  ( -22.42236680055709641, 157.8615022471902591, 0.000000000000000000 ) ) ;
#78023 = CARTESIAN_POINT ( 'NONE',  ( 202.3894997978090373, 280.0980987621804275, 16.95659012541789323 ) ) ;
#78024 = CARTESIAN_POINT ( 'NONE',  ( 164.8670003495851404, 245.0889742334797177, -1.557028074864921674 ) ) ;
#78026 = CARTESIAN_POINT ( 'NONE',  ( 73.59812156768246894, 55.56520137471197529, 16.10559722777662373 ) ) ;
#78025 = CARTESIAN_POINT ( 'NONE',  ( 163.1218343930725894, 256.2508100442478849, -16.13596270478102923 ) ) ;
#78027 = CARTESIAN_POINT ( 'NONE',  ( 199.1469736795485801, 281.8990786193456870, -16.60023204625315785 ) ) ;
#78028 = CARTESIAN_POINT ( 'NONE',  ( 25.64360150771698343, 30.50829794293882102, -10.00000000000000355 ) ) ;
#78029 = CARTESIAN_POINT ( 'NONE',  ( 163.4339502362531675, 283.8181923016741166, -3.128993586085420553 ) ) ;
#78030 = CARTESIAN_POINT ( 'NONE',  ( -19.65312891409030271, 93.06504152958497400, 10.00000000000000888 ) ) ;
#78031 = CARTESIAN_POINT ( 'NONE',  ( 188.6135346955672389, 260.1468269458595159, 3.785692842197046826 ) ) ;
#78032 = CARTESIAN_POINT ( 'NONE',  ( 183.8301289239822722, 272.2411597453489662, -17.34995410509954183 ) ) ;
#78033 = CARTESIAN_POINT ( 'NONE',  ( 0.9064528339360315989, 162.1423013555410080, -4.594050593750043987 ) ) ;
#78034 = CARTESIAN_POINT ( 'NONE',  ( 153.3073463970432044, 273.0798447238802282, -13.25289232200638345 ) ) ;
#78035 = VERTEX_POINT ( 'NONE', #85966 ) ;
#78036 = EDGE_CURVE ( 'NONE', #20756, #14203, #92252, .T. ) ;
#78037 = B_SPLINE_CURVE_WITH_KNOTS ( 'NONE', 3,
 ( #37535, #60329, #5166, #6658, #66947, #97876, #75074, #28450, #5654, #36543, #67450, #98378, #28966, #21362, #75565, #38024, #53246, #21851 ),
 .UNSPECIFIED., .F., .F.,
 ( 4, 2, 2, 2, 2, 2, 2, 2, 4 ),
 ( 7.473417450352270646E-17, 0.0003311343341728208351, 0.0006622686683455668603, 0.0009934030025183129397, 0.001324537336691059127, 0.001655671670863805315, 0.001986806005036550853, 0.002317940339209297040, 0.002649074673382043228 ),
 .UNSPECIFIED. ) ;
#78038 = CARTESIAN_POINT ( 'NONE',  ( 160.1656321119008624, 253.6529854836419133, -14.85229712523751466 ) ) ;
#78039 = PLANE ( 'NONE',  #56394 ) ;
#78040 = FACE_OUTER_BOUND ( 'NONE', #26592, .T. ) ;
#78041 = CARTESIAN_POINT ( 'NONE',  ( 12.78680497239753322, 184.3149278399160949, -9.188101187500095079 ) ) ;
#78042 = EDGE_CURVE ( 'NONE', #4283, #8200, #7389, .T. ) ;
#78043 = AXIS2_PLACEMENT_3D ( 'NONE', #19570, #64649, #50430 ) ;
#78044 = CARTESIAN_POINT ( 'NONE',  ( 29.16343140518078414, 25.03677371833803278, 10.00000000000000533 ) ) ;
#78045 = CARTESIAN_POINT ( 'NONE',  ( 29.01663622185449753, 35.49103043416550918, -8.090169943749479842 ) ) ;
#78046 = CARTESIAN_POINT ( 'NONE',  ( 130.7684581937436405, 234.7592609112379876, 2.679491924311254714 ) ) ;
#78047 = CARTESIAN_POINT ( 'NONE',  ( 173.6365052420643167, 272.7251026486088676, -16.35588217120040255 ) ) ;
#78048 = CARTESIAN_POINT ( 'NONE',  ( 13.51768745649715697, 168.6115022471901739, -5.000000000000041744 ) ) ;
#78049 = CARTESIAN_POINT ( 'NONE',  ( 189.9884492570354269, 298.3977273640915655, -7.992435462398296053 ) ) ;
#78050 = CARTESIAN_POINT ( 'NONE',  ( 190.7539468448011064, 261.9718772365148425, -0.8656167993522486670 ) ) ;
#78051 = CARTESIAN_POINT ( 'NONE',  ( 193.0242241521888502, 295.9312083549096428, -12.21184685123513347 ) ) ;
#78052 = CARTESIAN_POINT ( 'NONE',  ( 69.44849478424214340, 204.2365022471902023, -10.00000000000009059 ) ) ;
#78053 = CARTESIAN_POINT ( 'NONE',  ( 164.4654423005978288, 246.2001330526308323, 1.735427645011155873 ) ) ;
#78054 = CARTESIAN_POINT ( 'NONE',  ( -19.65312891409030271, 93.06504152958497400, 20.00000000000000355 ) ) ;
#78055 = CARTESIAN_POINT ( 'NONE',  ( 23.17910981781079727, 190.3149278399161233, -9.188101187500095079 ) ) ;
#78056 = CARTESIAN_POINT ( 'NONE',  ( 171.2743479101317234, 254.4242377521371736, -11.94796457435898951 ) ) ;
#78057 = ADVANCED_FACE ( 'NONE', ( #46894 ), #69190, .T. ) ;
#78058 = CARTESIAN_POINT ( 'NONE',  ( 135.1942566882107997, 238.8615022471902023, 5.000000000000051514 ) ) ;
#78059 = CARTESIAN_POINT ( 'NONE',  ( 203.0856642093833671, 269.8431269742375775, -6.121545823302062317 ) ) ;
#78060 = CARTESIAN_POINT ( 'NONE',  ( 177.9925615710933755, 254.8251403409008731, -7.350624415798725053 ) ) ;
#78061 = CARTESIAN_POINT ( 'NONE',  ( 74.14312167556930433, 66.30466486950707861, 1.224646799147354045E-15 ) ) ;
#78063 = FACE_OUTER_BOUND ( 'NONE', #3325, .T. ) ;
#78062 = VECTOR ( 'NONE', #68018, 1000.000000000000000 ) ;
#78064 = CARTESIAN_POINT ( 'NONE',  ( 159.8982138663949399, 278.4101122861870863, -10.05609574519431071 ) ) ;
#78065 = DIRECTION ( 'NONE',  ( 0.000000000000000000, 0.000000000000000000, 1.000000000000000000 ) ) ;
#78066 = CARTESIAN_POINT ( 'NONE',  ( 24.68213521633936836, 16.11110640527292759, -2.839279412974138328 ) ) ;
#78067 = CARTESIAN_POINT ( 'NONE',  ( 163.1008115941903895, 248.1481028935802442, 11.25332017433677834 ) ) ;
#78068 = CARTESIAN_POINT ( 'NONE',  ( 102.4837554958880759, 236.6427522451419350, 10.00000000000009415 ) ) ;
#78069 = CARTESIAN_POINT ( 'NONE',  ( 186.4223700097188043, 267.8240592505130167, -15.11424446612579864 ) ) ;
#78070 = ORIENTED_EDGE ( 'NONE', *, *, #1667, .T. ) ;
#78071 = CARTESIAN_POINT ( 'NONE',  ( 43.29939952211008602, 27.12755873383629890, -6.180339887498949025 ) ) ;
#78072 = CARTESIAN_POINT ( 'NONE',  ( 12.38457448260035143, 9.011106405272903075, 2.839279412974134775 ) ) ;
#78073 = DIRECTION ( 'NONE',  ( 0.8660254037844475894, 0.4999999999999846789, -0.000000000000000000 ) ) ;
#78074 = CARTESIAN_POINT ( 'NONE',  ( 71.95199650962558735, 72.63932214931871556, -0.9219114722910072279 ) ) ;
#78075 = CARTESIAN_POINT ( 'NONE',  ( 43.01983786573178037, 33.03677371833806120, 10.00000000000000533 ) ) ;
#78076 = ORIENTED_EDGE ( 'NONE', *, *, #34026, .F. ) ;
#78077 = CARTESIAN_POINT ( 'NONE',  ( 30.47735161394240322, 181.7365022471901739, -10.00000000000009237 ) ) ;
#78078 = CARTESIAN_POINT ( 'NONE',  ( 72.24303396261568366, 71.49679634179437926, -5.037392375358459518 ) ) ;
#78079 = CARTESIAN_POINT ( 'NONE',  ( 150.8757650385446993, 269.3225046528533539, 14.31332712971473953 ) ) ;
#78080 = CARTESIAN_POINT ( 'NONE',  ( 83.43773055803072225, 41.05266667205868458, 1.786701415307724750 ) ) ;
#78081 = ORIENTED_EDGE ( 'NONE', *, *, #211, .F. ) ;
#78082 = ORIENTED_EDGE ( 'NONE', *, *, #21384, .T. ) ;
#78084 = CARTESIAN_POINT ( 'NONE',  ( 84.90289089734821459, 42.76399680830722616, -3.660411970491889377 ) ) ;
#78083 = CARTESIAN_POINT ( 'NONE',  ( 186.9159192308579236, 272.5337820971376459, -15.87923880755278461 ) ) ;
#78085 = ORIENTED_EDGE ( 'NONE', *, *, #84199, .F. ) ;
#78086 = CARTESIAN_POINT ( 'NONE',  ( 153.2906404175950854, 265.1398178023911782, -17.60231834963988007 ) ) ;
#78087 = CARTESIAN_POINT ( 'NONE',  ( 189.7740653892032014, 260.9666063005456635, -5.939916383645439169 ) ) ;
#78088 = CARTESIAN_POINT ( 'NONE',  ( 80.03143596134809457, 57.61873189500683878, 16.60059503390609592 ) ) ;
#78089 = CARTESIAN_POINT ( 'NONE',  ( 77.27782791576461818, 63.42193016440150899, 15.51014190020122641 ) ) ;
#78090 = CARTESIAN_POINT ( 'NONE',  ( 147.9710862514405960, 274.3535558917855042, 7.785500222159708272 ) ) ;
#78091 = DIRECTION ( 'NONE',  ( 0.9458118053197297481, -0.3247153044096220409, 0.000000000000000000 ) ) ;
#78092 = VERTEX_POINT ( 'NONE', #70691 ) ;
#78093 = CARTESIAN_POINT ( 'NONE',  ( 195.7291534503633272, 291.6341570319625021, 16.44925029361851543 ) ) ;
#78094 = CARTESIAN_POINT ( 'NONE',  ( 162.1614388314975486, 266.6158802597933004, 17.60528378688847795 ) ) ;
#78095 = ORIENTED_EDGE ( 'NONE', *, *, #31857, .F. ) ;
#78096 = CARTESIAN_POINT ( 'NONE',  ( 23.93942162470478863, 34.79752408145593989, -5.678558825948271327 ) ) ;
#78097 = EDGE_CURVE ( 'NONE', #97401, #44408, #45016, .T. ) ;
#78098 = CARTESIAN_POINT ( 'NONE',  ( 159.2111180226792726, 254.8852497853115722, 16.01057445397460910 ) ) ;
#78099 = CYLINDRICAL_SURFACE ( 'NONE', #56291, 16.60714546451156792 ) ;
#78100 = CARTESIAN_POINT ( 'NONE',  ( 56.08842225738447240, 197.0643266524160140, 9.188101187500095079 ) ) ;
#78101 = EDGE_LOOP ( 'NONE', ( #3439, #3004, #81967, #4478 ) ) ;
#78102 = CARTESIAN_POINT ( 'NONE',  ( -15.49391466533604067, 73.38841914279046819, 13.64384121658392246 ) ) ;
#78103 = CARTESIAN_POINT ( 'NONE',  ( 24.67798091686682938, 37.18080186712595037, 3.090169943749475401 ) ) ;
#78104 = CARTESIAN_POINT ( 'NONE',  ( 180.8890834033174713, 294.3766012452771861, 6.559837412958372305 ) ) ;
#78106 = B_SPLINE_CURVE_WITH_KNOTS ( 'NONE', 3,
 ( #11302, #10283, #18386, #73096, #49281, #95439, #58837, #96410, #26485, #42160 ),
 .UNSPECIFIED., .F., .F.,
 ( 4, 2, 2, 2, 4 ),
 ( 0.000000000000000000, 0.0002622400424272597406, 0.0005244800848545194813, 0.0007867201272817791677, 0.001048960169709038963 ),
 .UNSPECIFIED. ) ;
#78105 = CARTESIAN_POINT ( 'NONE',  ( 173.7338896087951809, 271.5854767220461667, 16.43201141598054349 ) ) ;
#78107 = ORIENTED_EDGE ( 'NONE', *, *, #93311, .T. ) ;
#78108 = ORIENTED_EDGE ( 'NONE', *, *, #36509, .T. ) ;
#78109 = CARTESIAN_POINT ( 'NONE',  ( 190.2020559385390470, 299.9191148095094377, 5.071379031179562347 ) ) ;
#78110 = CARTESIAN_POINT ( 'NONE',  ( 68.76057960370418698, 222.0530062829863027, -4.648177544792955347E-16 ) ) ;
#78111 = CARTESIAN_POINT ( 'NONE',  ( 190.5726849661229210, 300.5654224342945326, -0.2192718484028965964 ) ) ;
#78112 = VERTEX_POINT ( 'NONE', #54468 ) ;
#78113 = CARTESIAN_POINT ( 'NONE',  ( 174.5508403973756515, 260.3590064504865040, -14.93617697178709314 ) ) ;
#78114 = DIRECTION ( 'NONE',  ( -0.000000000000000000, -0.000000000000000000, -1.000000000000000000 ) ) ;
#78115 = CARTESIAN_POINT ( 'NONE',  ( 207.8996209429610360, 270.5542889829179103, -5.987818313449536411 ) ) ;
#78116 = EDGE_CURVE ( 'NONE', #54626, #43956, #32189, .T. ) ;
#78117 = CARTESIAN_POINT ( 'NONE',  ( 147.4271219180435253, 275.2957297547342819, -3.800519706258907782 ) ) ;
#78118 = CARTESIAN_POINT ( 'NONE',  ( 190.0607312434325138, 301.4521522931182176, 3.538147641957853473 ) ) ;
#78119 = AXIS2_PLACEMENT_3D ( 'NONE', #64091, #41781, #9909 ) ;
#78120 = CARTESIAN_POINT ( 'NONE',  ( 69.45390216962655927, 66.50352562030866466, 10.22003932022287032 ) ) ;
#78121 = CONICAL_SURFACE ( 'NONE', #21421, 2.749999999999999112, 0.7853981633974469467 ) ;
#78122 = CARTESIAN_POINT ( 'NONE',  ( 88.45958475239287111, 43.85926912372239883, -0.5941283661710258235 ) ) ;
#78123 = LINE ( 'NONE', #39580, #36377 ) ;
#78124 = CARTESIAN_POINT ( 'NONE',  ( 70.37752084497869021, 65.47563201637457553, -11.66932464330069230 ) ) ;
#78125 = CARTESIAN_POINT ( 'NONE',  ( 77.94338102238666011, 47.97603164893081384, 14.13821563815946725 ) ) ;
#78126 = CARTESIAN_POINT ( 'NONE',  ( 121.5276403787286483, 228.7202760586659736, -5.415160957724236172E-17 ) ) ;
#78127 = ORIENTED_EDGE ( 'NONE', *, *, #84369, .T. ) ;
#78128 = CARTESIAN_POINT ( 'NONE',  ( 147.2592533090473239, 275.5864867145116932, -0.3770461397900867762 ) ) ;
#78129 = CARTESIAN_POINT ( 'NONE',  ( 78.92023586790456591, 59.45316570216661489, -16.52216786098997403 ) ) ;
#78130 = CARTESIAN_POINT ( 'NONE',  ( -0.01211276271276956473, 139.0458036431182620, 21.50000000000006750 ) ) ;
#78131 = VECTOR ( 'NONE', #62674, 1000.000000000000000 ) ;
#78132 = CARTESIAN_POINT ( 'NONE',  ( 155.0304386007204016, 262.1263989543018056, -17.12961552904782181 ) ) ;
#78133 = CARTESIAN_POINT ( 'NONE',  ( 163.7064929935861244, 247.0990319366274548, 6.401263337036986023 ) ) ;
#78134 = CARTESIAN_POINT ( 'NONE',  ( 83.86143710801805184, 52.01156594317939152, -14.55893269640292154 ) ) ;
#78135 = CARTESIAN_POINT ( 'NONE',  ( 69.31152416607949363, 65.05164803522899319, -11.50429494836084565 ) ) ;
#78136 = ORIENTED_EDGE ( 'NONE', *, *, #1251, .F. ) ;
#78137 = FACE_OUTER_BOUND ( 'NONE', #60344, .T. ) ;
#78138 = CARTESIAN_POINT ( 'NONE',  ( 71.94643353573425770, 71.53214566342799685, 5.625104812542582877 ) ) ;
#78139 = CARTESIAN_POINT ( 'NONE',  ( 206.3929371469040746, 272.7357536028613936, 8.215407031707147922 ) ) ;
#78140 = CARTESIAN_POINT ( 'NONE',  ( 128.2389901622930495, 244.8458772461660544, 9.188101187500095079 ) ) ;
#78141 = CARTESIAN_POINT ( 'NONE',  ( 198.8570476668614049, 286.2164853282868080, -17.01721544293231858 ) ) ;
#78142 = VECTOR ( 'NONE', #17649, 1000.000000000000000 ) ;
#78143 = CARTESIAN_POINT ( 'NONE',  ( 186.9854375150685257, 297.4581504985191032, 4.686305160240775258 ) ) ;
#78144 = CARTESIAN_POINT ( 'NONE',  ( 187.4766440450278537, 281.3944037113421359, -17.42068772228976314 ) ) ;
#78145 = CARTESIAN_POINT ( 'NONE',  ( -169.5327448629461742, 46.94652375874896677, -30.52142883766498116 ) ) ;
#78146 = CARTESIAN_POINT ( 'NONE',  ( 39.14627965220388006, 205.6589784336661637, -6.496448406907675876E-16 ) ) ;
#78147 = CARTESIAN_POINT ( 'NONE',  ( 85.65277752055500571, 48.41186657597218357, -12.21575983946770450 ) ) ;
#78148 = ORIENTED_EDGE ( 'NONE', *, *, #35203, .T. ) ;
#78149 = CARTESIAN_POINT ( 'NONE',  ( 71.98134248244618050, 66.42195643918441306, 11.72108357238321652 ) ) ;
#78150 = CARTESIAN_POINT ( 'NONE',  ( -17.33262083840143930, 129.0458036431182904, 21.50000000000006750 ) ) ;
#78151 = CYLINDRICAL_SURFACE ( 'NONE', #36863, 70.00000000000002842 ) ;
#78152 = CARTESIAN_POINT ( 'NONE',  ( 175.0900761532694219, 261.2389906071587689, 14.88021766879188412 ) ) ;
#78153 = CARTESIAN_POINT ( 'NONE',  ( 84.79042978850567636, 219.7608392184588411, -2.428612866367529932E-12 ) ) ;
#78154 = B_SPLINE_CURVE_WITH_KNOTS ( 'NONE', 3,
 ( #38844, #39825, #77875, #63153, #23636, #9972, #16056, #70756, #55533, #25672, #86518, #62636, #86025, #17049, #1369, #33257 ),
 .UNSPECIFIED., .F., .F.,
 ( 4, 1, 2, 2, 2, 1, 2, 2, 4 ),
 ( 0.000000000000000000, 0.1250000000000033307, 0.1875000000000040523, 0.2500000000000047740, 0.5000000000000016653, 0.6250000000000000000, 0.6875000000000001110, 0.7500000000000002220, 1.000000000000000000 ),
 .UNSPECIFIED. ) ;
#78155 = LINE ( 'NONE', #1150, #90016 ) ;
#78156 = CARTESIAN_POINT ( 'NONE',  ( 118.0722127640079577, 245.6427522451419065, 10.00000000000009237 ) ) ;
#78157 = CARTESIAN_POINT ( 'NONE',  ( 194.4648444083005359, 293.3692358227498289, -14.53531652569186150 ) ) ;
#78158 = ORIENTED_EDGE ( 'NONE', *, *, #3619, .T. ) ;
#78159 = B_SPLINE_CURVE_WITH_KNOTS ( 'NONE', 3,
 ( #77520, #1007, #31884, #62790 ),
 .UNSPECIFIED., .F., .F.,
 ( 4, 4 ),
 ( 0.006723087913367474522, 0.01173915425796831676 ),
 .UNSPECIFIED. ) ;
#78160 = CARTESIAN_POINT ( 'NONE',  ( 202.5245888501533216, 279.8641176599742266, 15.60152447840272494 ) ) ;
#78161 = CARTESIAN_POINT ( 'NONE',  ( 87.87676930530868447, 44.78862430170916298, 4.932775619378069187 ) ) ;
#78162 = EDGE_CURVE ( 'NONE', #81006, #68960, #78608, .T. ) ;
#78163 = CARTESIAN_POINT ( 'NONE',  ( 24.36989474801440636, 191.0024278399160949, 9.188101187500095079 ) ) ;
#78164 = CARTESIAN_POINT ( 'NONE',  ( 12.92385338608513301, 23.16454794089040092, -10.00000000000000355 ) ) ;
#78165 = CARTESIAN_POINT ( 'NONE',  ( 83.51796290786062116, 48.89396064590803093, -13.43348588850899183 ) ) ;
#78166 = DIRECTION ( 'NONE',  ( -0.6855440362341554961, 0.7280311630581363103, 0.000000000000000000 ) ) ;
#78167 = CARTESIAN_POINT ( 'NONE',  ( 66.49317117068670768, 67.78108392186146602, -6.905541408637477119 ) ) ;
#78169 = CARTESIAN_POINT ( 'NONE',  ( 59.87693630317638593, 211.5024278399160949, -9.188101187500093303 ) ) ;
#78168 = DIRECTION ( 'NONE',  ( 0.6793907169778423683, 0.000000000000000000, 0.7337767056021424761 ) ) ;
#78170 = EDGE_CURVE ( 'NONE', #60148, #57418, #37785, .T. ) ;
#78171 = CARTESIAN_POINT ( 'NONE',  ( 126.6061714340151241, 237.2365022471902023, -10.00000000000009237 ) ) ;
#78172 = DIRECTION ( 'NONE',  ( 0.000000000000000000, -0.000000000000000000, 1.000000000000000000 ) ) ;
#78173 = DIRECTION ( 'NONE',  ( -0.8769651246872975925, 0.4805540241036304616, 0.000000000000000000 ) ) ;
#78174 = CARTESIAN_POINT ( 'NONE',  ( 161.7988821920622513, 251.5333527145129437, -12.97904280059305293 ) ) ;
#78175 = ORIENTED_EDGE ( 'NONE', *, *, #15891, .T. ) ;
#78176 = CARTESIAN_POINT ( 'NONE',  ( 30.47735161394240322, 181.7365022471901739, -10.00000000000009059 ) ) ;
#78177 = DIRECTION ( 'NONE',  ( -0.8660254037844359321, -0.5000000000000051070, -0.000000000000000000 ) ) ;
#78178 = CARTESIAN_POINT ( 'NONE',  ( 202.3139361598622372, 280.2289788223093865, 15.93832709035092421 ) ) ;
#78179 = CARTESIAN_POINT ( 'NONE',  ( 151.5948730924283723, 249.1423013555410080, -4.594050593750043987 ) ) ;
#78180 = CARTESIAN_POINT ( 'NONE',  ( 28.84929788977513709, 34.84336893147758474, -7.433330006724137462 ) ) ;
#78183 = ADVANCED_FACE ( 'NONE', ( #84932 ), #30197, .T. ) ;
#78182 = CARTESIAN_POINT ( 'NONE',  ( 170.5221306371715286, 263.5122761618970344, 15.79513009679484803 ) ) ;
#78181 = CARTESIAN_POINT ( 'NONE',  ( 166.9114198365767550, 262.1412704778039142, -16.32394542780318858 ) ) ;
#78184 = CARTESIAN_POINT ( 'NONE',  ( 185.4455296801821476, 260.4024382772719264, 6.342364096776786475 ) ) ;
#78185 = CARTESIAN_POINT ( 'NONE',  ( 206.2520115784021471, 273.4080321133600933, 11.69992874350409018 ) ) ;
#78186 = CARTESIAN_POINT ( 'NONE',  ( 186.4709408934271266, 258.2127684368444989, -2.486660817739086315 ) ) ;
#78187 = CARTESIAN_POINT ( 'NONE',  ( 65.93175743083646978, 68.97510768830362338, 2.497091622996998161 ) ) ;
#78188 = ORIENTED_EDGE ( 'NONE', *, *, #81421, .T. ) ;
#78189 = CARTESIAN_POINT ( 'NONE',  ( 56.22356517706928969, 213.2677522451419350, -5.000000000000047962 ) ) ;
#78190 = CARTESIAN_POINT ( 'NONE',  ( 178.3565173979539509, 285.6070500341613183, 12.91966154977564329 ) ) ;
#78191 = CARTESIAN_POINT ( 'NONE',  ( -59.87889494062799400, 37.30571521936384016, 10.00000000000000000 ) ) ;
#78192 = CARTESIAN_POINT ( 'NONE',  ( 13.72994409607376731, 16.43085787977761569, -9.188101187500008038 ) ) ;
#78193 = CARTESIAN_POINT ( 'NONE',  ( -27.23710841895085011, 23.47708815495369450, -10.00000000000000000 ) ) ;
#78194 = B_SPLINE_CURVE_WITH_KNOTS ( 'NONE', 3,
 ( #47867, #71207, #7381, #76788, #32683, #63583, #94525, #53480, #84431, #100111, #14976, #30695, #19013, #27099, #64088, #72211 ),
 .UNSPECIFIED., .F., .F.,
 ( 4, 1, 2, 2, 2, 1, 2, 2, 4 ),
 ( 0.000000000000000000, 0.1249999999999962808, 0.1874999999999963363, 0.2499999999999963918, 0.4999999999999973355, 0.6249999999999973355, 0.6874999999999972244, 0.7499999999999970024, 1.000000000000000000 ),
 .UNSPECIFIED. ) ;
#78195 = CARTESIAN_POINT ( 'NONE',  ( 69.47336484112540234, 62.61584900673512522, 13.29333455021356158 ) ) ;
#78196 = AXIS2_PLACEMENT_3D ( 'NONE', #9787, #78177, #25981 ) ;
#78197 = EDGE_CURVE ( 'NONE', #35992, #35860, #90827, .T. ) ;
#78198 = CARTESIAN_POINT ( 'NONE',  ( 152.6992418905140028, 266.1641500988167763, 17.27767170937316621 ) ) ;
#78199 = CARTESIAN_POINT ( 'NONE',  ( 81.06766895168330223, 227.6115022471903160, -5.000000000000047962 ) ) ;
#78200 = DIRECTION ( 'NONE',  ( -0.8660254037844378194, -0.5000000000000014433, -0.000000000000000000 ) ) ;
#78201 = CARTESIAN_POINT ( 'NONE',  ( 208.2912792141756029, 269.8759169579697641, -2.198672330625011995 ) ) ;
#78202 = CARTESIAN_POINT ( 'NONE',  ( 154.8556227199321427, 262.4291889417971788, 17.77326384500479861 ) ) ;
#78203 = ORIENTED_EDGE ( 'NONE', *, *, #78563, .T. ) ;
#78204 = VERTEX_POINT ( 'NONE', #34204 ) ;
#78205 = CARTESIAN_POINT ( 'NONE',  ( 155.8645391177437887, 277.2735152180572982, -10.45080344275615758 ) ) ;
#78206 = VECTOR ( 'NONE', #9401, 1000.000000000000114 ) ;
#78207 = CARTESIAN_POINT ( 'NONE',  ( 72.89440483270105631, 70.83506548046183582, 7.273745411891205492 ) ) ;
#78208 = ORIENTED_EDGE ( 'NONE', *, *, #22608, .T. ) ;
#78209 = PLANE ( 'NONE',  #20823 ) ;
#78210 = CARTESIAN_POINT ( 'NONE',  ( -26.40302582819689547, -15.24379406933011616, -3.684716733547464345E-15 ) ) ;
#78211 = VERTEX_POINT ( 'NONE', #3808 ) ;
#78212 = CARTESIAN_POINT ( 'NONE',  ( 146.5689048584090699, 276.7822053059436485, -0.4306668706573002492 ) ) ;
#78213 = DIRECTION ( 'NONE',  ( -0.000000000000000000, -0.000000000000000000, -1.000000000000000000 ) ) ;
#78214 = VECTOR ( 'NONE', #47247, 1000.000000000000000 ) ;
#78215 = CARTESIAN_POINT ( 'NONE',  ( 17.34117332728243355, 10.41603393254323962, -1.583844403245362020 ) ) ;
#78216 = CARTESIAN_POINT ( 'NONE',  ( 81.17880017041383667, 48.14434756715330366, -13.80270438712140013 ) ) ;
#78217 = CARTESIAN_POINT ( 'NONE',  ( 69.64850847652870414, 62.66264390746926694, 13.89643941053915022 ) ) ;
#78218 = VERTEX_POINT ( 'NONE', #56982 ) ;
#78219 = CARTESIAN_POINT ( 'NONE',  ( 155.6211605266461220, 261.1032385654538075, 17.14571743626555644 ) ) ;
#78220 = CARTESIAN_POINT ( 'NONE',  ( 167.6711793886181852, 254.0238391605262223, -13.38728416657071563 ) ) ;
#78221 = CARTESIAN_POINT ( 'NONE',  ( 190.7851751463332164, 300.1973786460605425, 8.237717828100052486 ) ) ;
#78222 = DIRECTION ( 'NONE',  ( 1.000000000000000000, -7.930164461608259651E-15, 0.000000000000000000 ) ) ;
#78223 = B_SPLINE_SURFACE_WITH_KNOTS ( 'NONE', 3, 1, ( 
 ( #34589, #65488 ),
 ( #9297, #59869 ),
 ( #4183, #82736 ),
 ( #90835, #35084 ),
 ( #75102, #43676 ),
 ( #57885, #28996 ),
 ( #65988, #11812 ),
 ( #59357, #89353 ),
 ( #58377, #58858 ),
 ( #13307, #28476 ),
 ( #96941, #88864 ),
 ( #20910, #98402 ),
 ( #44166, #89827 ),
 ( #19429, #27979 ),
 ( #5680, #50285 ),
 ( #51797, #36569 ),
 ( #12814, #20403 ),
 ( #81238, #43164 ),
 ( #97411, #74618 ),
 ( #4699, #42669 ),
 ( #90333, #73602 ),
 ( #97901, #67476 ),
 ( #27507, #51272 ),
 ( #19906, #50778 ),
 ( #5191, #36073 ),
 ( #81728, #66974 ),
 ( #82238, #12305 ),
 ( #74105, #35589 ),
 ( #66484, #26325 ),
 ( #79563, #10121 ),
 ( #18226, #80560 ),
 ( #42491, #10625 ),
 ( #58206, #57198 ),
 ( #17726, #34896 ) ),
 .UNSPECIFIED., .T., .F., .F.,
 ( 4, 2, 2, 2, 2, 2, 2, 2, 2, 2, 2, 2, 2, 2, 2, 2, 4 ),
 ( 2, 2 ),
 ( 0.000000000000000000, 0.06250000000000000000, 0.1250000000000000000, 0.1875000000000000000, 0.2500000000000000000, 0.3125000000000000000, 0.3750000000000000000, 0.4375000000000000000, 0.5000000000000000000, 0.5625000000000000000, 0.6250000000000000000, 0.6875000000000000000, 0.7500000000000000000, 0.8125000000000000000, 0.8750000000000000000, 0.9375000000000000000, 1.000000000000000000 ),
 ( 0.000000000000000000, 1.000000000000000000 ),
 .UNSPECIFIED. ) ;
#78224 = ORIENTED_EDGE ( 'NONE', *, *, #3840, .T. ) ;
#78225 = EDGE_CURVE ( 'NONE', #66499, #28990, #72220, .T. ) ;
#78226 = EDGE_CURVE ( 'NONE', #79518, #87939, #3769, .T. ) ;
#78227 = ORIENTED_EDGE ( 'NONE', *, *, #6967, .F. ) ;
#78228 = ORIENTED_EDGE ( 'NONE', *, *, #7772, .T. ) ;
#78229 = CARTESIAN_POINT ( 'NONE',  ( 80.22712853404131295, 46.14526667274431304, 12.26665755571171701 ) ) ;
#78230 = VERTEX_POINT ( 'NONE', #44767 ) ;
#78231 = CARTESIAN_POINT ( 'NONE',  ( 177.5865089022509551, 268.7852845103913069, 17.37969943402860906 ) ) ;
#78232 = ORIENTED_EDGE ( 'NONE', *, *, #6359, .F. ) ;
#78233 = EDGE_CURVE ( 'NONE', #20199, #30467, #60609, .T. ) ;
#78234 = CARTESIAN_POINT ( 'NONE',  ( 208.3132655666949233, 269.8378354783333180, 2.688523655043302707 ) ) ;
#78235 = CARTESIAN_POINT ( 'NONE',  ( -13.76211276271272865, 162.8615022471902307, 0.000000000000000000 ) ) ;
#78236 = CARTESIAN_POINT ( 'NONE',  ( 171.0393489256058217, 283.3835579739524064, 12.04226256192440836 ) ) ;
#78237 = CARTESIAN_POINT ( 'NONE',  ( 194.9819925439454664, 292.9282776833073285, -15.33279721168237586 ) ) ;
#78238 = EDGE_CURVE ( 'NONE', #34378, #46023, #96538, .T. ) ;
#78239 = CARTESIAN_POINT ( 'NONE',  ( 197.7402002575066433, 288.1509217855910379, -17.43364815852810423 ) ) ;
#78240 = CARTESIAN_POINT ( 'NONE',  ( 166.7979224981183108, 247.0939422667762813, 1.921831505315402477 ) ) ;
#78241 = CARTESIAN_POINT ( 'NONE',  ( 19.86428432551159418, 29.65586893147756342, -7.433330006724137462 ) ) ;
#78242 = CARTESIAN_POINT ( 'NONE',  ( 195.6914848190668863, 279.7035040353765680, -17.46620344769279853 ) ) ;
#78243 = CARTESIAN_POINT ( 'NONE',  ( 164.5648480107187197, 245.6123174360222094, 3.015887571020871238 ) ) ;
#78245 = ORIENTED_EDGE ( 'NONE', *, *, #39078, .T. ) ;
#78244 = FACE_OUTER_BOUND ( 'NONE', #67563, .T. ) ;
#78246 = ADVANCED_FACE ( 'NONE', ( #29103 ), #36672, .T. ) ;
#78247 = CARTESIAN_POINT ( 'NONE',  ( 190.8086039075475071, 300.1567988412789987, 5.217942970589348306 ) ) ;
#78248 = CARTESIAN_POINT ( 'NONE',  ( 152.7043854946215049, 268.1552411151685078, 15.94764448997051964 ) ) ;
#78249 = ADVANCED_FACE ( 'NONE', ( #83323 ), #28088, .F. ) ;
#78250 = CARTESIAN_POINT ( 'NONE',  ( 206.4640281786353171, 273.0408085897082060, -10.81921452789957883 ) ) ;
#78251 = CYLINDRICAL_SURFACE ( 'NONE', #65120, 17.82106496071139645 ) ;
#78252 = CARTESIAN_POINT ( 'NONE',  ( 84.30423139501758101, 45.69133797766890837, -9.735438995952875985 ) ) ;
#78253 = CARTESIAN_POINT ( 'NONE',  ( 161.6707029936031574, 250.6251236501384483, 14.45053103226186231 ) ) ;
#78254 = CARTESIAN_POINT ( 'NONE',  ( 104.1130136275158975, 242.4637435831425023, 2.679491924311251605 ) ) ;
#78255 = ORIENTED_EDGE ( 'NONE', *, *, #41738, .T. ) ;
#78256 = CARTESIAN_POINT ( 'NONE',  ( 193.9668281760451976, 294.6865939465442921, -14.27585970476158472 ) ) ;
#78257 = DIRECTION ( 'NONE',  ( -0.6444573283589029034, 0.7646402761589956576, 0.000000000000000000 ) ) ;
#78258 = DIRECTION ( 'NONE',  ( 0.9008877160804890094, 0.4340522123146939859, 0.000000000000000000 ) ) ;
#78259 = CARTESIAN_POINT ( 'NONE',  ( 18.55146011244625370, 181.5177522451418497, -10.00000000000009592 ) ) ;
#78260 = CARTESIAN_POINT ( 'NONE',  ( 84.85626976964255164, 228.9869531367911293, 4.594050593750046652 ) ) ;
#78261 = DIRECTION ( 'NONE',  ( -0.9778746070300391446, 0.2091919045418505763, 0.000000000000000000 ) ) ;
#78262 = CARTESIAN_POINT ( 'NONE',  ( 171.6481351228935353, 251.7782516689747183, -8.436504614365913923 ) ) ;
#78263 = CARTESIAN_POINT ( 'NONE',  ( 166.9835885616171254, 278.1161903108272213, -13.50565314437992726 ) ) ;
#78265 = DIRECTION ( 'NONE',  ( -0.8660254037844387076, -0.5000000000000000000, 0.000000000000000000 ) ) ;
#78264 = CARTESIAN_POINT ( 'NONE',  ( 16.79251956066557128, 174.3768266524160140, 9.188101187500098632 ) ) ;
#78266 = CLOSED_SHELL ( 'NONE', ( #35507, #52696, #46138, #48784 ) ) ;
#78267 = CARTESIAN_POINT ( 'NONE',  ( 200.5621507313343557, 283.2631601884785368, 16.81037192529623425 ) ) ;
#78268 = ORIENTED_EDGE ( 'NONE', *, *, #26705, .T. ) ;
#78269 = ORIENTED_EDGE ( 'NONE', *, *, #48245, .T. ) ;
#78270 = CARTESIAN_POINT ( 'NONE',  ( 201.3911183001464451, 266.9640362439821502, -3.754059931952923534 ) ) ;
#78271 = CARTESIAN_POINT ( 'NONE',  ( 67.28774071949871427, 67.22545272451772291, -8.569909696590800152 ) ) ;
#78272 = CIRCLE ( 'NONE', #55599, 49.99999999999999289 ) ;
#78273 = CARTESIAN_POINT ( 'NONE',  ( 42.54989241151534429, 183.8262482093457493, 3.021315404115420679E-15 ) ) ;
#78274 = CARTESIAN_POINT ( 'NONE',  ( 92.83118068642198750, 217.7365022471901739, -10.00000000000009237 ) ) ;
#78275 = CARTESIAN_POINT ( 'NONE',  ( 74.36956061611711277, 67.95497152727877221, -11.68736594047405930 ) ) ;
#78276 = CARTESIAN_POINT ( 'NONE',  ( 32.70573635520464251, 183.5643266524160140, 9.188101187500095079 ) ) ;
#78277 = CARTESIAN_POINT ( 'NONE',  ( 94.68952686182812783, 232.1427522451419065, 10.00000000000009415 ) ) ;
#78278 = ORIENTED_EDGE ( 'NONE', *, *, #37953, .F. ) ;
#78279 = CARTESIAN_POINT ( 'NONE',  ( 151.4434765650916859, 272.4879699064614442, -11.67392547022929783 ) ) ;
#78280 = AXIS2_PLACEMENT_3D ( 'NONE', #58725, #90699, #89700 ) ;
#78281 = PLANE ( 'NONE',  #59836 ) ;
#78282 = EDGE_CURVE ( 'NONE', #28585, #37573, #49687, .T. ) ;
#78283 = CARTESIAN_POINT ( 'NONE',  ( 166.6782394145706974, 287.1526701389618665, -3.786997032746254988 ) ) ;
#78284 = CARTESIAN_POINT ( 'NONE',  ( 157.2744851780909414, 258.2395962677452985, 18.17792129701959070 ) ) ;
#78285 = CARTESIAN_POINT ( 'NONE',  ( 68.68909986772983700, 64.16576715822536414, -12.55144644528872533 ) ) ;
#78286 = CARTESIAN_POINT ( 'NONE',  ( 68.53065452504849020, 198.8262482093457777, 3.021315404115420679E-15 ) ) ;
#78287 = CARTESIAN_POINT ( 'NONE',  ( -34.06669189922481422, 36.18719137533145158, 59.99999999999999289 ) ) ;
#78288 = CARTESIAN_POINT ( 'NONE',  ( 194.3442947553755005, 294.0328026529847421, -15.97648891113594871 ) ) ;
#78289 = ADVANCED_FACE ( 'NONE', ( #54350, #99999, #15356 ), #92908, .T. ) ;
#78290 = CARTESIAN_POINT ( 'NONE',  ( 192.4162201953099895, 265.1061942910134235, 7.764509510832549033 ) ) ;
#78291 = CARTESIAN_POINT ( 'NONE',  ( 171.4174712912980567, 280.1694600568308147, 15.32434928890935133 ) ) ;
#78292 = CYLINDRICAL_SURFACE ( 'NONE', #598, 17.82106496071139645 ) ;
#78293 = CARTESIAN_POINT ( 'NONE',  ( 146.6363376198206652, 276.6654083370839885, -0.5879280619134327202 ) ) ;
#78294 = CARTESIAN_POINT ( 'NONE',  ( 147.9710862514405960, 274.3535558917855042, 7.785500222159708272 ) ) ;
#78295 = CARTESIAN_POINT ( 'NONE',  ( 180.9086552280229512, 266.9847810424545855, -14.76064602474076537 ) ) ;
#78296 = ORIENTED_EDGE ( 'NONE', *, *, #11455, .F. ) ;
#78297 = CARTESIAN_POINT ( 'NONE',  ( 74.35158511417792226, 58.53122306914246309, 16.30383169004117150 ) ) ;
#78298 =( BOUNDED_CURVE ( )  B_SPLINE_CURVE ( 2, ( #69071, #1698, #15867, #32581, #69573, #39648, #45759 ),
 .UNSPECIFIED., .F., .T. ) 
 B_SPLINE_CURVE_WITH_KNOTS ( ( 3, 2, 2, 3 ),
 ( 0.9798387096774193727, 0.9811827956989247479, 0.9838709677419354982, 0.9855363728105643872 ),
 .UNSPECIFIED. ) 
 CURVE ( )  GEOMETRIC_REPRESENTATION_ITEM ( )  RATIONAL_B_SPLINE_CURVE ( ( 0.9330127018922194093, 0.9330127018922194093, 1.000000000000000000, 0.8660254037844387076, 1.000000000000000000, 0.9169986265629754829, 0.9368410486966849415 ) ) 
 REPRESENTATION_ITEM ( '' )  );
#78299 = CARTESIAN_POINT ( 'NONE',  ( 207.5215400641004351, 271.2091442744748520, 2.886080616848571534 ) ) ;
#78300 = CARTESIAN_POINT ( 'NONE',  ( 181.1695799106581148, 268.1689120071131924, 16.08932648799075338 ) ) ;
#78301 = CARTESIAN_POINT ( 'NONE',  ( 100.7694865641816051, 238.1744531367911293, 4.594050593750047540 ) ) ;
#78302 = CARTESIAN_POINT ( 'NONE',  ( 19.08966579672462061, 13.94754757982089188, 5.678558825948272215 ) ) ;
#78304 = ADVANCED_FACE ( 'NONE', ( #85850 ), #30080, .F. ) ;
#78303 = CARTESIAN_POINT ( 'NONE',  ( 151.4361976351029000, 268.3518069213970421, 15.15218985681980612 ) ) ;
#78305 = LINE ( 'NONE', #30697, #62977 ) ;
#78307 = CARTESIAN_POINT ( 'NONE',  ( 195.1777878793919854, 279.1127009034667594, 16.30558289032921948 ) ) ;
#78306 = CARTESIAN_POINT ( 'NONE',  ( 157.5042325173297684, 257.8416622032797818, 16.70595240278738203 ) ) ;
#78308 = CARTESIAN_POINT ( 'NONE',  ( 150.6248456996347045, 269.7571096964470598, -15.31580666236335908 ) ) ;
#78309 = CARTESIAN_POINT ( 'NONE',  ( -89.11465314115665137, 93.37593066204027537, -37.49999999999999289 ) ) ;
#78310 = CARTESIAN_POINT ( 'NONE',  ( 149.9417705975453430, 271.6836028715711677, -11.65547513120671219 ) ) ;
#78311 = CARTESIAN_POINT ( 'NONE',  ( 105.2496719664350451, 243.1199935810941213, 2.679491924311251605 ) ) ;
#78312 = CARTESIAN_POINT ( 'NONE',  ( 146.7943851877206214, 276.3916619194686746, -4.608908220452185844 ) ) ;
#78313 = CARTESIAN_POINT ( 'NONE',  ( 45.66470909604093720, 114.5311720768849995, 10.00000000000000000 ) ) ;
#78314 = ORIENTED_EDGE ( 'NONE', *, *, #73449, .T. ) ;
#78315 = CARTESIAN_POINT ( 'NONE',  ( 190.5690073685513255, 266.3856132956990450, 10.80116815030898003 ) ) ;
#78316 = DIRECTION ( 'NONE',  ( -0.8660254037844384856, -0.5000000000000002220, -3.252519625699449945E-16 ) ) ;
#78317 = CARTESIAN_POINT ( 'NONE',  ( 196.6843777741297856, 267.5020668084886211, 9.700680000278353532 ) ) ;
#78319 = ORIENTED_EDGE ( 'NONE', *, *, #3505, .F. ) ;
#78318 = EDGE_CURVE ( 'NONE', #31824, #69871, #8283, .T. ) ;
#78320 = EDGE_CURVE ( 'NONE', #91318, #78857, #22482, .T. ) ;
#78321 = CARTESIAN_POINT ( 'NONE',  ( 85.19931647622364324, 44.72206782681810466, 8.604955222596291975 ) ) ;
#78322 = CARTESIAN_POINT ( 'NONE',  ( 179.8937413821747100, 262.8266594973790689, -12.81885310938439382 ) ) ;
#78323 = CARTESIAN_POINT ( 'NONE',  ( 186.7554075434758545, 282.3000898601083577, 17.53539547572453827 ) ) ;
#78324 = CARTESIAN_POINT ( 'NONE',  ( 74.92485320761846879, 53.17783355571813075, -16.51377003329815096 ) ) ;
#78325 = CARTESIAN_POINT ( 'NONE',  ( 192.0712386031329686, 297.9698513971258649, 12.12276320360788873 ) ) ;
#78326 = ORIENTED_EDGE ( 'NONE', *, *, #57873, .F. ) ;
#78327 = B_SPLINE_CURVE_WITH_KNOTS ( 'NONE', 3,
 ( #1791, #31162, #62552, #93515 ),
 .UNSPECIFIED., .F., .F.,
 ( 4, 4 ),
 ( 0.04501900553147333839, 0.04887120950165264877 ),
 .UNSPECIFIED. ) ;
#78328 = DIRECTION ( 'NONE',  ( -0.6758705274779434058, -0.2489746672676118044, 0.6936934806855752367 ) ) ;
#78329 = CARTESIAN_POINT ( 'NONE',  ( 40.64525884627276042, 24.26216523072497466, -2.296566073217252530E-15 ) ) ;
#78330 = ORIENTED_EDGE ( 'NONE', *, *, #16335, .F. ) ;
#78331 = CARTESIAN_POINT ( 'NONE',  ( 78.43012671350176390, 61.37287260322700888, 16.21548333613125337 ) ) ;
#78332 = DIRECTION ( 'NONE',  ( 0.4999999999999998890, -0.8660254037844385966, 0.000000000000000000 ) ) ;
#78333 = LINE ( 'NONE', #57003, #30569 ) ;
#78334 = VERTEX_POINT ( 'NONE', #31065 ) ;
#78335 = CARTESIAN_POINT ( 'NONE',  ( 86.17560058389634037, 46.94341623220315540, -10.60084123426474179 ) ) ;
#78336 = DIRECTION ( 'NONE',  ( 0.4999999999999998890, -0.8660254037844385966, 0.000000000000000000 ) ) ;
#78337 = CARTESIAN_POINT ( 'NONE',  ( 150.8555837531579868, 276.0290483310748755, -8.437460036063264113 ) ) ;
#78338 = CARTESIAN_POINT ( 'NONE',  ( 87.56148871955852542, 44.50103375289268826, -5.753754189115007023 ) ) ;
#78339 = CARTESIAN_POINT ( 'NONE',  ( 37.70440764347101492, 39.95586893147758900, 7.433330006724141015 ) ) ;
#78340 = CARTESIAN_POINT ( 'NONE',  ( 80.38494540807658950, 44.35137226082142803, 11.33962482632668944 ) ) ;
#78341 = CARTESIAN_POINT ( 'NONE',  ( 84.83590989842353736, 50.19589791021755332, -13.76099895038702847 ) ) ;
#78342 = CARTESIAN_POINT ( 'NONE',  ( 203.5080190724872011, 278.1607665491929993, -15.47044080916498743 ) ) ;
#78343 = ORIENTED_EDGE ( 'NONE', *, *, #53512, .F. ) ;
#78344 = ORIENTED_EDGE ( 'NONE', *, *, #79534, .T. ) ;
#78345 = CARTESIAN_POINT ( 'NONE',  ( 162.6525385610000569, 249.3719130927429717, 10.67620540106957350 ) ) ;
#78346 = EDGE_LOOP ( 'NONE', ( #20288, #15479, #79268, #67613 ) ) ;
#78347 = CARTESIAN_POINT ( 'NONE',  ( 77.30283862971377573, 49.68973779529829216, -15.49743936997366411 ) ) ;
#78348 = VECTOR ( 'NONE', #15075, 1000.000000000000114 ) ;
#78349 = ORIENTED_EDGE ( 'NONE', *, *, #68874, .T. ) ;
#78350 = CARTESIAN_POINT ( 'NONE',  ( 86.92574391271591594, 45.77938117786232652, -8.666101563913320760 ) ) ;
#78351 = CARTESIAN_POINT ( 'NONE',  ( 164.8075539017095252, 280.4672370525465226, 12.63796469268613265 ) ) ;
#78352 = EDGE_LOOP ( 'NONE', ( #55266, #82078, #3504, #90110 ) ) ;
#78353 = EDGE_CURVE ( 'NONE', #27025, #95233, #61470, .T. ) ;
#78354 = CARTESIAN_POINT ( 'NONE',  ( 165.4979031618668444, 275.0437756392552160, -16.09671154009961569 ) ) ;
#78355 = CARTESIAN_POINT ( 'NONE',  ( 165.0260329286864760, 244.8135217264176049, -2.114260670082726890 ) ) ;
#78356 = CARTESIAN_POINT ( 'NONE',  ( 147.1659813806172110, 275.7480384334725159, -6.355065261369051477 ) ) ;
#78357 = CARTESIAN_POINT ( 'NONE',  ( 196.0450415453838673, 284.4196233059693100, -17.59408283607186263 ) ) ;
#78358 = CARTESIAN_POINT ( 'NONE',  ( 78.95260674202536677, 46.19732041717283977, 12.80077979390832610 ) ) ;
#78359 = CARTESIAN_POINT ( 'NONE',  ( -110.0000000000000000, 15.00000000000000000, 59.99999999999999289 ) ) ;
#78360 = LINE ( 'NONE', #72779, #74406 ) ;
#78361 = AXIS2_PLACEMENT_3D ( 'NONE', #48132, #79075, #47624 ) ;
#78362 = CARTESIAN_POINT ( 'NONE',  ( 154.0080725480042645, 280.0853259021857298, 2.227893399009504449 ) ) ;
#78363 = EDGE_CURVE ( 'NONE', #43169, #346, #27972, .T. ) ;
#78364 = CARTESIAN_POINT ( 'NONE',  ( 117.5758788303146076, 244.8149278399160664, 9.188101187500093303 ) ) ;
#78365 = CARTESIAN_POINT ( 'NONE',  ( 70.62955678144575700, 60.80479719377109404, -15.06269029760223077 ) ) ;
#78366 = ORIENTED_EDGE ( 'NONE', *, *, #16550, .F. ) ;
#78367 = EDGE_CURVE ( 'NONE', #32340, #25515, #60967, .T. ) ;
#78369 = ORIENTED_EDGE ( 'NONE', *, *, #35527, .T. ) ;
#78368 = CARTESIAN_POINT ( 'NONE',  ( 85.74702290878657607, 48.70847181056628727, -12.40582123554878358 ) ) ;
#78370 = CARTESIAN_POINT ( 'NONE',  ( 200.3293654959697392, 273.7156512906800572, 13.98704503334941229 ) ) ;
#78371 = CARTESIAN_POINT ( 'NONE',  ( 177.9052972741453971, 254.1236105787376687, 1.345436856673193127 ) ) ;
#78372 = DIRECTION ( 'NONE',  ( -0.8143688203140632131, 0.5803476755362092510, 0.000000000000000000 ) ) ;
#78373 = CARTESIAN_POINT ( 'NONE',  ( 190.1523655968549917, 300.2662179550520705, 3.189538939137619877 ) ) ;
#78374 = FACE_OUTER_BOUND ( 'NONE', #22639, .T. ) ;
#78375 = CARTESIAN_POINT ( 'NONE',  ( 81.19662769710231487, 43.13455380257515515, 9.541327768654262798 ) ) ;
#78376 = CARTESIAN_POINT ( 'NONE',  ( 173.6157233020167610, 287.1844615712983568, -9.596145886780515610 ) ) ;
#78377 = CARTESIAN_POINT ( 'NONE',  ( 26.41003172443570790, 38.18080186712595037, 3.090169943749475401 ) ) ;
#78378 = DIRECTION ( 'NONE',  ( -0.8660254037844384856, -0.5000000000000004441, 0.000000000000000000 ) ) ;
#78379 = ORIENTED_EDGE ( 'NONE', *, *, #26480, .F. ) ;
#78380 = CARTESIAN_POINT ( 'NONE',  ( 148.3625667886952044, 273.6754917110858401, -8.960758510948144462 ) ) ;
#78381 = CARTESIAN_POINT ( 'NONE',  ( 150.1137873495230224, 271.7467049757541986, 11.69504156493408686 ) ) ;
#78382 = EDGE_LOOP ( 'NONE', ( #2274, #21026, #83142, #96707 ) ) ;
#78383 = CARTESIAN_POINT ( 'NONE',  ( 191.1909278266552974, 267.6859549916610490, -12.12569103935590675 ) ) ;
#78384 = CARTESIAN_POINT ( 'NONE',  ( 190.6715059189721728, 283.1265308623420083, -16.56656797196155750 ) ) ;
#78385 = CARTESIAN_POINT ( 'NONE',  ( 191.7031701327977657, 298.6073646884106552, -10.95670423068276200 ) ) ;
#78386 = CARTESIAN_POINT ( 'NONE',  ( 149.3833831332874240, 271.9073859370555510, 11.40518020539810173 ) ) ;
#78387 = CARTESIAN_POINT ( 'NONE',  ( 163.1002605973966126, 283.8590136238245236, 7.096359992437378139 ) ) ;
#78389 = CARTESIAN_POINT ( 'NONE',  ( 151.5633707495463227, 275.0466943824089299, -8.634966370009285797 ) ) ;
#78388 = CARTESIAN_POINT ( 'NONE',  ( 161.5427656070157241, 281.5317803557720708, -6.609083002670620210 ) ) ;
#78390 = CARTESIAN_POINT ( 'NONE',  ( 17.38248943320504836, 35.13769309531819829, -10.00000000000000000 ) ) ;
#78391 = ORIENTED_EDGE ( 'NONE', *, *, #20877, .T. ) ;
#78392 = CARTESIAN_POINT ( 'NONE',  ( 190.9441801652054096, 299.9219738747156043, -4.765040093794296716 ) ) ;
#78393 = CARTESIAN_POINT ( 'NONE',  ( 187.1508084581589344, 263.0214344965982036, -9.031509870500761039 ) ) ;
#78394 = CARTESIAN_POINT ( 'NONE',  ( 190.1014290098027004, 274.4466737287558544, -15.67214041744576924 ) ) ;
#78395 = DIRECTION ( 'NONE',  ( 0.000000000000000000, -0.000000000000000000, 1.000000000000000000 ) ) ;
#78396 = B_SPLINE_CURVE_WITH_KNOTS ( 'NONE', 3,
 ( #49067, #73371, #10570, #3958, #34841, #87639, #72385, #25779, #33359, #10068 ),
 .UNSPECIFIED., .F., .F.,
 ( 4, 2, 2, 2, 4 ),
 ( 0.000000000000000000, 0.0002622400424272591985, 0.0005244800848545183971, 0.0007867201272817776498, 0.001048960169709036794 ),
 .UNSPECIFIED. ) ;
#78397 = CARTESIAN_POINT ( 'NONE',  ( 195.8285188278500470, 273.2427770020486832, 15.26130794574777383 ) ) ;
#78398 = CARTESIAN_POINT ( 'NONE',  ( 153.3100492430090753, 265.1062007306585997, 16.32434963471121492 ) ) ;
#78399 = CARTESIAN_POINT ( 'NONE',  ( 73.78595477147815984, 68.43622263357737268, 11.45456581244436123 ) ) ;
#78400 = CARTESIAN_POINT ( 'NONE',  ( -4.668846022976054222, 158.1115022471902023, -5.000000000000041744 ) ) ;
#78401 = CARTESIAN_POINT ( 'NONE',  ( -22.42236680055709641, 157.8615022471902591, 0.000000000000000000 ) ) ;
#78402 = CARTESIAN_POINT ( 'NONE',  ( 3.071516343397128423, 163.3923013555410080, 4.594050593750050204 ) ) ;
#78403 = CARTESIAN_POINT ( 'NONE',  ( 86.94057726720511425, 214.8768266524160140, 9.188101187500098632 ) ) ;
#78404 = CARTESIAN_POINT ( 'NONE',  ( 203.4357368910538355, 278.2859629599173559, -16.45855118664066197 ) ) ;
#78405 = CARTESIAN_POINT ( 'NONE',  ( 146.8868584395697781, 276.2314935489248455, -3.891417269505058396 ) ) ;
#78406 = CARTESIAN_POINT ( 'NONE',  ( 182.8360444305251349, 294.4420450557742583, -8.068983014621899486 ) ) ;
#78407 = EDGE_CURVE ( 'NONE', #65018, #36928, #30304, .T. ) ;
#78408 = CARTESIAN_POINT ( 'NONE',  ( 155.3250150347760723, 261.6161776038049425, -18.57420904020362684 ) ) ;
#78409 = LINE ( 'NONE', #55568, #78131 ) ;
#78410 = CARTESIAN_POINT ( 'NONE',  ( 84.65037625111526154, 50.51595192201220641, -13.58046508661252894 ) ) ;
#78411 = CARTESIAN_POINT ( 'NONE',  ( 78.12758897056819762, 61.89708633492155343, 15.71247334545933505 ) ) ;
#78413 = CARTESIAN_POINT ( 'NONE',  ( -20.78386844332395711, 95.22353984434415963, 45.19937630303414977 ) ) ;
#78412 = DIRECTION ( 'NONE',  ( -0.5000000000000014433, 0.8660254037844379305, 0.000000000000000000 ) ) ;
#78414 = CARTESIAN_POINT ( 'NONE',  ( 180.9657615313112728, 291.1000814692523022, 9.328123854075322186 ) ) ;
#78415 = CARTESIAN_POINT ( 'NONE',  ( -17.23454462704816947, 134.8759306620403038, 8.444826468009708598E-14 ) ) ;
#78416 = CARTESIAN_POINT ( 'NONE',  ( 204.8040236202276674, 275.9160208256662941, -13.14144539090630204 ) ) ;
#78417 = CARTESIAN_POINT ( 'NONE',  ( 157.2744851780909414, 258.2395962677452985, 18.17792129701959070 ) ) ;
#78418 = CARTESIAN_POINT ( 'NONE',  ( -15.10528209597770299, 24.46087392797018722, -10.00000000000000000 ) ) ;
#78419 = CIRCLE ( 'NONE', #33137, 70.00000000000001421 ) ;
#78420 = CARTESIAN_POINT ( 'NONE',  ( 161.8839333999304415, 250.2557977526613229, -13.90128376743482441 ) ) ;
#78421 = CARTESIAN_POINT ( 'NONE',  ( 41.52819660837609916, 194.7833772461660544, -9.188101187500095079 ) ) ;
#78422 = B_SPLINE_CURVE_WITH_KNOTS ( 'NONE', 3,
 ( #42844, #88537, #65662, #12995 ),
 .UNSPECIFIED., .F., .F.,
 ( 4, 4 ),
 ( 0.003497155503932982204, 0.007366944115509544908 ),
 .UNSPECIFIED. ) ;
#78423 = CARTESIAN_POINT ( 'NONE',  ( 67.67116493723634107, 216.0024278399160664, -9.188101187500093303 ) ) ;
#78424 = CARTESIAN_POINT ( 'NONE',  ( 3.854092266844447501, 28.45370138451378850, -10.00000000000000000 ) ) ;
#78427 = EDGE_CURVE ( 'NONE', #1591, #13682, #18390, .T. ) ;
#78426 = CARTESIAN_POINT ( 'NONE',  ( 88.14558033319170249, 43.66656252067526367, 0.1579512601322911325 ) ) ;
#78425 = VECTOR ( 'NONE', #50755, 1000.000000000000114 ) ;
#78428 = CARTESIAN_POINT ( 'NONE',  ( 9.265696904164599346, 17.30066082961419838, -10.00000000000000533 ) ) ;
#78430 = DIRECTION ( 'NONE',  ( -0.000000000000000000, -0.000000000000000000, -1.000000000000000000 ) ) ;
#78429 = DIRECTION ( 'NONE',  ( 0.000000000000000000, 0.5247752241695049502, 0.8512408378936280329 ) ) ;
#78431 = CARTESIAN_POINT ( 'NONE',  ( 196.4451169242987305, 269.0860587627796576, -10.53632002257244338 ) ) ;
#78432 = CARTESIAN_POINT ( 'NONE',  ( 33.29248241878940462, 22.14754757982091604, -5.678558825948275768 ) ) ;
#78433 = CARTESIAN_POINT ( 'NONE',  ( 198.7501991201633018, 286.4015524398827779, -18.58948563601804693 ) ) ;
#78434 = CARTESIAN_POINT ( 'NONE',  ( 196.5806080813426888, 290.1593943507663766, -16.31912166233602690 ) ) ;
#78435 = CARTESIAN_POINT ( 'NONE',  ( 14.92192532440567199, 20.56628583063839955, 9.188101187500006262 ) ) ;
#78436 = CARTESIAN_POINT ( 'NONE',  ( 73.32782722540972031, 203.9548013555409796, -4.594050593750042211 ) ) ;
#78437 = CARTESIAN_POINT ( 'NONE',  ( 76.92045831404706746, 63.69682018499118925, 15.34400990693822564 ) ) ;
#78438 = CARTESIAN_POINT ( 'NONE',  ( 203.2732885619977026, 278.5673317194472247, -16.64305493556850024 ) ) ;
#78439 = CARTESIAN_POINT ( 'NONE',  ( 160.0072461633487535, 253.5063153963366744, 16.23938890643736244 ) ) ;
#78440 = CARTESIAN_POINT ( 'NONE',  ( 48.09199531666208571, 210.1199935810940929, 2.679491924311303119 ) ) ;
#78441 = CARTESIAN_POINT ( 'NONE',  ( 154.0754981180030825, 263.7804043885726060, 17.67325968003652292 ) ) ;
#78442 = EDGE_CURVE ( 'NONE', #99135, #68704, #37648, .T. ) ;
#78443 = EDGE_CURVE ( 'NONE', #70599, #90346, #12628, .T. ) ;
#78444 = CARTESIAN_POINT ( 'NONE',  ( 78.54737301421290852, 55.66250919272829378, -16.12479227928217540 ) ) ;
#78445 = CARTESIAN_POINT ( 'NONE',  ( 100.6254093204818645, 242.2365022471903444, 2.944929066748280225E-16 ) ) ;
#78446 = CARTESIAN_POINT ( 'NONE',  ( 200.7897860911934913, 282.8688841796032420, 18.17522996445731920 ) ) ;
#78447 = CARTESIAN_POINT ( 'NONE',  ( 206.9676408587583296, 272.1685258403992975, 7.544050792475608169 ) ) ;
#78448 = ORIENTED_EDGE ( 'NONE', *, *, #24112, .F. ) ;
#78449 = CARTESIAN_POINT ( 'NONE',  ( 77.47838539169265459, 49.59694670388121551, 14.91689290702275983 ) ) ;
#78450 = CARTESIAN_POINT ( 'NONE',  ( 187.9837572234687002, 273.3093249989548212, 15.64228832037970562 ) ) ;
#78451 = ORIENTED_EDGE ( 'NONE', *, *, #57248, .T. ) ;
#78452 = CARTESIAN_POINT ( 'NONE',  ( 159.2713554375903300, 254.7809155221686410, -15.70062444474382168 ) ) ;
#78453 = CARTESIAN_POINT ( 'NONE',  ( 193.6538297768585153, 294.3106073703939387, 13.99927879369582406 ) ) ;
#78454 = CARTESIAN_POINT ( 'NONE',  ( 167.4734756851294151, 275.5778401279644640, 16.39827101669492393 ) ) ;
#78455 = ORIENTED_EDGE ( 'NONE', *, *, #42236, .F. ) ;
#78456 = CARTESIAN_POINT ( 'NONE',  ( 177.2715209000007235, 253.2106104779961981, -0.2627270112733235963 ) ) ;
#78457 = VERTEX_POINT ( 'NONE', #3693 ) ;
#78458 = CARTESIAN_POINT ( 'NONE',  ( 72.46567298678348834, 71.74231227323613780, 5.836615459846345999 ) ) ;
#78459 = CARTESIAN_POINT ( 'NONE',  ( 194.9455394410084921, 292.9914163096879065, -15.01116663483170655 ) ) ;
#78460 = CARTESIAN_POINT ( 'NONE',  ( 148.5451600033913735, 273.7521268005480124, 8.257041405901727416 ) ) ;
#78461 = ORIENTED_EDGE ( 'NONE', *, *, #37929, .F. ) ;
#78462 = CARTESIAN_POINT ( 'NONE',  ( 25.06043674821822265, 32.65586893147757053, -7.433330006724137462 ) ) ;
#78463 = CARTESIAN_POINT ( 'NONE',  ( 79.99303828038561903, 44.39269627614997660, 11.58267821196168157 ) ) ;
#78464 = CARTESIAN_POINT ( 'NONE',  ( 30.69616969366791537, 176.9824982072973967, 3.021315404115420679E-15 ) ) ;
#78465 = CARTESIAN_POINT ( 'NONE',  ( 75.32876355654416045, 66.66275840934527253, -13.04208647660080089 ) ) ;
#78466 = CARTESIAN_POINT ( 'NONE',  ( 78.41488460546182182, 49.53322450150187706, -14.69929798244788266 ) ) ;
#78467 = ORIENTED_EDGE ( 'NONE', *, *, #37924, .F. ) ;
#78468 = CYLINDRICAL_SURFACE ( 'NONE', #9328, 70.00000000000002842 ) ;
#78469 = CARTESIAN_POINT ( 'NONE',  ( -22.42236680055709641, 157.8615022471902591, 0.000000000000000000 ) ) ;
#78470 = EDGE_LOOP ( 'NONE', ( #64070, #59763, #37340, #7439 ) ) ;
#78471 = CARTESIAN_POINT ( 'NONE',  ( 174.2976836722478424, 286.0237415149990738, 10.49720334598133498 ) ) ;
#78472 = EDGE_CURVE ( 'NONE', #77592, #35956, #97392, .T. ) ;
#78473 = CARTESIAN_POINT ( 'NONE',  ( 68.26378387136982440, 65.68578065247751852, -10.31175839017903328 ) ) ;
#78474 = CARTESIAN_POINT ( 'NONE',  ( 208.1612901671020381, 270.1010645919285480, -2.401583477149568768 ) ) ;
#78475 = CARTESIAN_POINT ( 'NONE',  ( 194.4263876777154394, 293.8906135405502482, 15.23185943445137802 ) ) ;
#78476 = CARTESIAN_POINT ( 'NONE',  ( 19.62422909362874535, 11.73415679381821342, 1.333680081654574804E-15 ) ) ;
#78477 = CARTESIAN_POINT ( 'NONE',  ( 204.8878784573704195, 275.7707799872745795, -14.13380496213581594 ) ) ;
#78478 = CARTESIAN_POINT ( 'NONE',  ( 148.9967968810750563, 247.6423013555410080, -4.594050593750043987 ) ) ;
#78479 = CARTESIAN_POINT ( 'NONE',  ( 70.20948996332299430, 63.06637520435538846, -13.85461378616484041 ) ) ;
#78480 = CARTESIAN_POINT ( 'NONE',  ( 172.4171479096595476, 249.8244119910172572, -1.292277060833630919 ) ) ;
#78481 = CARTESIAN_POINT ( 'NONE',  ( 81.82518085639701155, 227.2369531367911293, -4.594050593750048428 ) ) ;
#78482 = VERTEX_POINT ( 'NONE', #59851 ) ;
#78483 = CARTESIAN_POINT ( 'NONE',  ( 191.2056514706806070, 299.4690922889112699, 7.290007621276087590 ) ) ;
#78484 = LINE ( 'NONE', #24270, #67401 ) ;
#78485 = FACE_OUTER_BOUND ( 'NONE', #18809, .T. ) ;
#78486 = ORIENTED_EDGE ( 'NONE', *, *, #81005, .F. ) ;
#78487 = CARTESIAN_POINT ( 'NONE',  ( 195.3218463993883631, 292.3396335385324392, -16.35123038532568174 ) ) ;
#78488 = EDGE_LOOP ( 'NONE', ( #38819, #61299, #55537, #93725 ) ) ;
#78489 = EDGE_LOOP ( 'NONE', ( #28511, #76245, #38421, #65586, #21521, #71983, #76323, #53538 ) ) ;
#78490 = CARTESIAN_POINT ( 'NONE',  ( 80.11111641639102743, 44.89713496294027095, -11.28635903916993932 ) ) ;
#78491 = EDGE_CURVE ( 'NONE', #64537, #16291, #89570, .T. ) ;
#78492 = FACE_OUTER_BOUND ( 'NONE', #64576, .T. ) ;
#78493 = CARTESIAN_POINT ( 'NONE',  ( 191.3413020738616410, 299.2341385521244774, -8.295023558158421295 ) ) ;
#78494 = CARTESIAN_POINT ( 'NONE',  ( 81.37739665788856769, 55.81704345181816507, 16.38624498997419110 ) ) ;
#78495 = CARTESIAN_POINT ( 'NONE',  ( 83.00813062480057170, 47.72000278234192194, -12.31777161607909044 ) ) ;
#78496 = CARTESIAN_POINT ( 'NONE',  ( 162.5082079047825800, 249.1745225923870919, 11.52567592363465465 ) ) ;
#78497 = CARTESIAN_POINT ( 'NONE',  ( 80.49933977867583224, 217.2833772461660544, -9.188101187500095079 ) ) ;
#78498 = VERTEX_POINT ( 'NONE', #66955 ) ;
#78499 = CIRCLE ( 'NONE', #7310, 0.1418229129680793899 ) ;
#78500 = VERTEX_POINT ( 'NONE', #90316 ) ;
#78501 = B_SPLINE_SURFACE_WITH_KNOTS ( 'NONE', 3, 1, ( 
 ( #84075, #37900 ),
 ( #97263, #94160 ),
 ( #70827, #92657 ),
 ( #61211, #93661 ),
 ( #8526, #85579 ),
 ( #23208, #31802 ),
 ( #54098, #38908 ),
 ( #86579, #39395 ),
 ( #1437, #32317 ),
 ( #16616, #23701 ),
 ( #69812, #93150 ),
 ( #54596, #24713 ),
 ( #63218, #85054 ),
 ( #92177, #24225 ),
 ( #70312, #16122 ),
 ( #15602, #62703 ),
 ( #46501, #422 ),
 ( #8035, #45994 ),
 ( #31311, #77438 ),
 ( #62200, #38406 ),
 ( #47020, #15103 ),
 ( #55596, #77935 ),
 ( #925, #55105 ),
 ( #47512, #69320 ),
 ( #86092, #78439 ),
 ( #9020, #39893 ),
 ( #17112, #48010 ),
 ( #78953, #61705 ),
 ( #9542, #68808 ),
 ( #99737, #30323 ),
 ( #22727, #53606 ),
 ( #84565, #76912 ),
 ( #7509, #100241 ),
 ( #30825, #10530 ) ),
 .UNSPECIFIED., .T., .F., .F.,
 ( 4, 2, 2, 2, 2, 2, 2, 2, 2, 2, 2, 2, 2, 2, 2, 2, 4 ),
 ( 2, 2 ),
 ( 0.000000000000000000, 0.06250000000000000000, 0.1250000000000000000, 0.1875000000000000000, 0.2500000000000000000, 0.3125000000000000000, 0.3750000000000000000, 0.4375000000000000000, 0.5000000000000000000, 0.5625000000000000000, 0.6250000000000000000, 0.6875000000000000000, 0.7500000000000000000, 0.8125000000000000000, 0.8750000000000000000, 0.9375000000000000000, 1.000000000000000000 ),
 ( 0.000000000000000000, 1.000000000000000000 ),
 .UNSPECIFIED. ) ;
#78502 = CARTESIAN_POINT ( 'NONE',  ( 200.9599690715405984, 282.5741186110587364, -18.15734256570992855 ) ) ;
#78503 = ORIENTED_EDGE ( 'NONE', *, *, #64828, .F. ) ;
#78504 = AXIS2_PLACEMENT_3D ( 'NONE', #91787, #58838, #75568 ) ;
#78505 = CARTESIAN_POINT ( 'NONE',  ( 76.08373593127036827, 64.71300453985560353, -14.35646715271085405 ) ) ;
#78506 = CARTESIAN_POINT ( 'NONE',  ( 161.8559746524236118, 283.8847177754445283, 0.5186945926108780247 ) ) ;
#78507 = LINE ( 'NONE', #86155, #29938 ) ;
#78508 = CARTESIAN_POINT ( 'NONE',  ( 87.80215979260032100, 44.26138434534234278, 4.729176973005307261 ) ) ;
#78509 = ORIENTED_EDGE ( 'NONE', *, *, #34398, .F. ) ;
#78510 = CARTESIAN_POINT ( 'NONE',  ( 189.8312826409137131, 295.2143506670603301, 11.32827604750477413 ) ) ;
#78511 = CARTESIAN_POINT ( 'NONE',  ( 40.95666657127031840, 28.81029122506297924, 8.090169943749479842 ) ) ;
#78512 = CARTESIAN_POINT ( 'NONE',  ( 159.3995226465659982, 254.5589234043588078, -16.81133486613867234 ) ) ;
#78513 = CARTESIAN_POINT ( 'NONE',  ( 155.5995420464182644, 262.6346450740109617, -17.48312782858739567 ) ) ;
#78514 = CARTESIAN_POINT ( 'NONE',  ( 174.6073334282909570, 283.8159819771393018, 13.70195899965856690 ) ) ;
#78515 = CARTESIAN_POINT ( 'NONE',  ( 198.9874128674464373, 285.2371454184261097, -17.19338160671415139 ) ) ;
#78516 = EDGE_CURVE ( 'NONE', #5086, #14650, #51777, .T. ) ;
#78517 = DIRECTION ( 'NONE',  ( -0.2649596321165964552, 0.4589235447807054058, -0.8480480961564325071 ) ) ;
#78518 = ORIENTED_EDGE ( 'NONE', *, *, #15300, .F. ) ;
#78519 = PLANE ( 'NONE',  #4099 ) ;
#78520 = CARTESIAN_POINT ( 'NONE',  ( 200.1102648775588193, 284.0458494464393198, 17.54251420653697835 ) ) ;
#78521 = CARTESIAN_POINT ( 'NONE',  ( 19.31801425620940194, 115.5650415295850451, -45.00000000000001421 ) ) ;
#78522 = CARTESIAN_POINT ( 'NONE',  ( 188.0892524428953152, 265.9230919214824667, -13.13131459770854725 ) ) ;
#78523 = CARTESIAN_POINT ( 'NONE',  ( 84.07138645536940658, 51.57118087273711637, 14.70185406139691153 ) ) ;
#78524 = EDGE_CURVE ( 'NONE', #59341, #25263, #58461, .T. ) ;
#78525 = CARTESIAN_POINT ( 'NONE',  ( 156.7822077518624440, 272.7230075932969839, 14.67370109713490933 ) ) ;
#78526 = ORIENTED_EDGE ( 'NONE', *, *, #86296, .T. ) ;
#78527 = CARTESIAN_POINT ( 'NONE',  ( -17.43550054826663498, 104.2312461070085021, 44.57229221387615326 ) ) ;
#78528 = VECTOR ( 'NONE', #90996, 1000.000000000000000 ) ;
#78529 = CARTESIAN_POINT ( 'NONE',  ( 164.9404048476745004, 244.9618339132846074, -2.801285734921658666 ) ) ;
#78531 = CARTESIAN_POINT ( 'NONE',  ( 73.66928586354876529, 55.48613233660923072, 16.58448172204914783 ) ) ;
#78530 = CARTESIAN_POINT ( 'NONE',  ( 177.8817410463586555, 265.0886103430123057, -15.04724780127894412 ) ) ;
#78532 = CARTESIAN_POINT ( 'NONE',  ( 199.5551099226704821, 281.1097900043435516, -17.04800700720547368 ) ) ;
#78533 = CARTESIAN_POINT ( 'NONE',  ( 23.53456118939196529, 35.36126292948896577, 6.180339887498949913 ) ) ;
#78534 = CARTESIAN_POINT ( 'NONE',  ( 172.3227493250666953, 275.1189843839183027, 16.65430444194719684 ) ) ;
#78535 = CARTESIAN_POINT ( 'NONE',  ( -22.42236680055709641, 157.8615022471902591, 0.000000000000000000 ) ) ;
#78536 = CARTESIAN_POINT ( 'NONE',  ( 133.5985852126658529, 236.3932355074535963, -2.679491924311248496 ) ) ;
#78537 = CARTESIAN_POINT ( 'NONE',  ( -65.00000000000000000, 18.66025403784439973, -54.99999999999999289 ) ) ;
#78538 = CARTESIAN_POINT ( 'NONE',  ( 207.8844858873204657, 270.5805036682629066, -6.251308616122969397 ) ) ;
#78539 = CARTESIAN_POINT ( 'NONE',  ( -2.476892769303202790, 175.5024278399161233, -9.188101187500093303 ) ) ;
#78540 = CARTESIAN_POINT ( 'NONE',  ( 82.24012673451345279, 47.97130509467530857, 12.79208699616589229 ) ) ;
#78541 = EDGE_LOOP ( 'NONE', ( #79243, #63501, #40700, #92247 ) ) ;
#78542 = CARTESIAN_POINT ( 'NONE',  ( 178.8600085713521537, 256.7301307640913706, 8.633611849901967616 ) ) ;
#78543 = FACE_OUTER_BOUND ( 'NONE', #34122, .T. ) ;
#78544 = CARTESIAN_POINT ( 'NONE',  ( 81.59255471807858839, 41.71843698051294780, 5.901189277464562011 ) ) ;
#78545 = CARTESIAN_POINT ( 'NONE',  ( 19.39059577201889084, 175.8768266524160140, 9.188101187500096856 ) ) ;
#78546 = CARTESIAN_POINT ( 'NONE',  ( 169.7005567072155259, 288.7155782076579271, 4.430715832634252394 ) ) ;
#78547 = CARTESIAN_POINT ( 'NONE',  ( 37.16144446923997435, 23.58380873178789727, 6.180339887498953466 ) ) ;
#78548 = CARTESIAN_POINT ( 'NONE',  ( 122.1317068477954422, 247.9865022471903444, 10.00000000000009415 ) ) ;
#78549 = CARTESIAN_POINT ( 'NONE',  ( 99.25420243115651431, 238.1115022471902876, -5.000000000000047962 ) ) ;
#78550 = CARTESIAN_POINT ( 'NONE',  ( 80.98395585398840524, 56.01611329191965893, 16.09912269941438723 ) ) ;
#78551 = CYLINDRICAL_SURFACE ( 'NONE', #78361, 17.82106496071139645 ) ;
#78552 = CARTESIAN_POINT ( 'NONE',  ( 85.04793144752866851, 49.76842598555752772, 13.42690168825988550 ) ) ;
#78553 = CARTESIAN_POINT ( 'NONE',  ( 187.5308134497532819, 259.4978860586243741, -0.7759764616068984822 ) ) ;
#78554 = EDGE_CURVE ( 'NONE', #95622, #3742, #23340, .T. ) ;
#78555 = EDGE_CURVE ( 'NONE', #65763, #63007, #77442, .T. ) ;
#78556 = DIRECTION ( 'NONE',  ( -0.000000000000000000, 0.000000000000000000, -1.000000000000000000 ) ) ;
#78557 = CARTESIAN_POINT ( 'NONE',  ( 68.07728789491675059, 210.1115022471902591, 10.00000000000009592 ) ) ;
#78558 = CARTESIAN_POINT ( 'NONE',  ( 164.5259176133158689, 246.1953198488120051, 1.882264443804981813 ) ) ;
#78559 = CARTESIAN_POINT ( 'NONE',  ( 30.62489312496363425, 46.16797101519271962, 10.00000000000000000 ) ) ;
#78560 = ADVANCED_FACE ( 'NONE', ( #66 ), #60316, .F. ) ;
#78561 = CARTESIAN_POINT ( 'NONE',  ( 24.04513522159523475, 190.8149278399161233, 9.188101187500093303 ) ) ;
#78562 = CARTESIAN_POINT ( 'NONE',  ( 198.1300353965528984, 287.4757075181870505, 18.48278456664528946 ) ) ;
#78563 = EDGE_CURVE ( 'NONE', #43174, #6804, #40170, .T. ) ;
#78564 = CARTESIAN_POINT ( 'NONE',  ( 203.1536195656275652, 269.7275029030552105, -6.026020274049146863 ) ) ;
#78565 = CARTESIAN_POINT ( 'NONE',  ( 151.3999564459286375, 268.4145785023736153, -15.40574304386609050 ) ) ;
#78566 = AXIS2_PLACEMENT_3D ( 'NONE', #80460, #25729, #94651 ) ;
#78567 = CARTESIAN_POINT ( 'NONE',  ( 67.01770718203071908, 66.86662898352919626, -8.855153707138468278 ) ) ;
#78568 = ORIENTED_EDGE ( 'NONE', *, *, #44182, .F. ) ;
#78569 = CARTESIAN_POINT ( 'NONE',  ( 17.89217828605986327, 10.73415679381820986, 1.333680081654574804E-15 ) ) ;
#78570 = CARTESIAN_POINT ( 'NONE',  ( 202.8096126329844253, 278.9917248286524796, -15.16107960898829532 ) ) ;
#78571 = CARTESIAN_POINT ( 'NONE',  ( 205.6622124036295247, 269.3173564635357593, -1.337127560418800654 ) ) ;
#78572 = CARTESIAN_POINT ( 'NONE',  ( 27.97303175072023151, 18.01110640527293327, 2.839279412974134775 ) ) ;
#78573 = CARTESIAN_POINT ( 'NONE',  ( 202.3894997978090373, 280.0980987621804275, 16.95659012541789323 ) ) ;
#78574 = CARTESIAN_POINT ( 'NONE',  ( 149.3801359649374092, 271.9130101976182914, -11.41245530317637424 ) ) ;
#78575 = CARTESIAN_POINT ( 'NONE',  ( 188.7310474590576632, 269.8941210489508080, -14.07782309740324500 ) ) ;
#78576 = EDGE_LOOP ( 'NONE', ( #5480, #60651, #96722, #51016 ) ) ;
#78577 = B_SPLINE_CURVE_WITH_KNOTS ( 'NONE', 3,
 ( #83992, #43935, #36843, #61626 ),
 .UNSPECIFIED., .F., .F.,
 ( 4, 4 ),
 ( 0.006037860917506979175, 0.01410894879655490500 ),
 .UNSPECIFIED. ) ;
#78578 = CARTESIAN_POINT ( 'NONE',  ( 16.39654754030849659, 10.26216523072493203, -2.296566073217252530E-15 ) ) ;
#78579 = LINE ( 'NONE', #33465, #42934 ) ;
#78580 = CARTESIAN_POINT ( 'NONE',  ( 75.74547564527691179, 59.01063491041397668, -15.93052030936962460 ) ) ;
#78581 = CARTESIAN_POINT ( 'NONE',  ( 38.70287833452073301, 99.18198963270081947, 59.99999999999999289 ) ) ;
#78582 = ORIENTED_EDGE ( 'NONE', *, *, #27275, .T. ) ;
#78583 = CARTESIAN_POINT ( 'NONE',  ( 23.34060026799419063, 195.8297689869269504, -2.679491924311252493 ) ) ;
#78584 = CARTESIAN_POINT ( 'NONE',  ( 72.34691042023506213, 71.90931229659582868, -5.260778230539377098 ) ) ;
#78585 = B_SPLINE_CURVE_WITH_KNOTS ( 'NONE', 3,
 ( #64114, #24114, #18034, #41805, #95580, #55987, #79370, #2845, #40796, #47895 ),
 .UNSPECIFIED., .F., .F.,
 ( 4, 2, 2, 2, 4 ),
 ( 0.000000000000000000, 0.0004220628552397187377, 0.0008441257104794374754, 0.001266188565719156105, 0.001688251420958874951 ),
 .UNSPECIFIED. ) ;
#78586 = CARTESIAN_POINT ( 'NONE',  ( 85.13065436355927318, 49.01193835628323114, 12.45131667738069225 ) ) ;
#78587 = CARTESIAN_POINT ( 'NONE',  ( 178.1343968340341348, 256.5670189455112222, -7.272430892715192385 ) ) ;
#78588 = ORIENTED_EDGE ( 'NONE', *, *, #21677, .F. ) ;
#78589 = ORIENTED_EDGE ( 'NONE', *, *, #3104, .T. ) ;
#78591 = CARTESIAN_POINT ( 'NONE',  ( 82.36190372195099485, 42.31745646093239088, -6.261288449950242807 ) ) ;
#78590 = LINE ( 'NONE', #95334, #34188 ) ;
#78592 = ORIENTED_EDGE ( 'NONE', *, *, #87623, .T. ) ;
#78593 = CARTESIAN_POINT ( 'NONE',  ( 66.14792423582534298, 68.51351281792520354, -2.683414512432761079 ) ) ;
#78594 = CARTESIAN_POINT ( 'NONE',  ( 71.67184923690800247, 72.06465046553262255, -3.547063142499712551 ) ) ;
#78595 = CARTESIAN_POINT ( 'NONE',  ( 72.95830788359974406, 56.77128196665827176, -15.96545419981961267 ) ) ;
#78596 = CARTESIAN_POINT ( 'NONE',  ( 47.92671612011951510, 80.40884667711614497, -10.00000000000000000 ) ) ;
#78597 = CARTESIAN_POINT ( 'NONE',  ( 148.2159754900428936, 273.9293952882992471, 9.267836332806297150 ) ) ;
#78598 = CARTESIAN_POINT ( 'NONE',  ( 184.0730272687639513, 288.7302421887371793, -13.16879209019809061 ) ) ;
#78599 = ORIENTED_EDGE ( 'NONE', *, *, #49987, .T. ) ;
#78600 = CARTESIAN_POINT ( 'NONE',  ( 157.2464636617698375, 258.2881309577184652, 18.14284729738657731 ) ) ;
#78601 = LINE ( 'NONE', #9187, #57489 ) ;
#78602 = ORIENTED_EDGE ( 'NONE', *, *, #28954, .T. ) ;
#78603 = CARTESIAN_POINT ( 'NONE',  ( 28.52453836335597614, 34.65586893147758474, -7.433330006724137462 ) ) ;
#78604 = CARTESIAN_POINT ( 'NONE',  ( 197.9552487813401456, 287.7784468162186613, 17.26493623863614602 ) ) ;
#78605 = CARTESIAN_POINT ( 'NONE',  ( 78.26988008674611308, 47.94124790171424877, -14.02519726671745737 ) ) ;
#78606 = CARTESIAN_POINT ( 'NONE',  ( 53.57110205792969282, 210.9244531367911577, -4.594050593750046652 ) ) ;
#78607 = CARTESIAN_POINT ( 'NONE',  ( 74.32474745866193189, 68.52230083288840490, 11.15590001247776364 ) ) ;
#78608 =( BOUNDED_CURVE ( )  B_SPLINE_CURVE ( 2, ( #789, #23082, #53974, #52995, #83946, #45391, #76321, #6896, #31182 ),
 .UNSPECIFIED., .F., .T. ) 
 B_SPLINE_CURVE_WITH_KNOTS ( ( 3, 2, 2, 2, 3 ),
 ( 0.8669354838709677491, 0.8682795698924731242, 0.8709677419354838745, 0.8736559139784946248, 0.8750000000000000000 ),
 .UNSPECIFIED. ) 
 CURVE ( )  GEOMETRIC_REPRESENTATION_ITEM ( )  RATIONAL_B_SPLINE_CURVE ( ( 0.9330127018922194093, 0.9330127018922194093, 1.000000000000000000, 0.8660254037844387076, 1.000000000000000000, 0.8660254037844387076, 1.000000000000000000, 0.9330127018922194093, 0.9330127018922194093 ) ) 
 REPRESENTATION_ITEM ( '' )  );
#78609 = DIRECTION ( 'NONE',  ( 0.000000000000000000, -0.000000000000000000, -1.000000000000000000 ) ) ;
#78610 = DIRECTION ( 'NONE',  ( -0.7646402761590023189, -0.6444573283588951318, 0.000000000000000000 ) ) ;
#78611 = VECTOR ( 'NONE', #477, 1000.000000000000000 ) ;
#78612 = CARTESIAN_POINT ( 'NONE',  ( 176.1305938586311299, 272.9992343613586741, 17.56359532786331457 ) ) ;
#78613 = ORIENTED_EDGE ( 'NONE', *, *, #85122, .T. ) ;
#78614 = LINE ( 'NONE', #69983, #25381 ) ;
#78615 = DIRECTION ( 'NONE',  ( 0.000000000000000000, -0.000000000000000000, 1.000000000000000000 ) ) ;
#78616 = CARTESIAN_POINT ( 'NONE',  ( 189.8533352240220893, 301.8113727360248504, -0.2033756396389863053 ) ) ;
#78617 = ORIENTED_EDGE ( 'NONE', *, *, #13960, .T. ) ;
#78618 = CARTESIAN_POINT ( 'NONE',  ( 171.7561557084762001, 259.2930754640176474, -13.77066962676198969 ) ) ;
#78619 = CARTESIAN_POINT ( 'NONE',  ( 170.6581720520257761, 275.3793360666527974, -16.53181577443977446 ) ) ;
#78620 = CARTESIAN_POINT ( 'NONE',  ( 207.7836085030675690, 270.7552284231231852, -5.468305433308493058 ) ) ;
#78621 = CARTESIAN_POINT ( 'NONE',  ( 192.8301672656986341, 296.6553483942417415, -13.40355799340913556 ) ) ;
#78622 = CARTESIAN_POINT ( 'NONE',  ( 190.7705347155322499, 300.2227366160529414, 3.504769718465625239 ) ) ;
#78623 = ADVANCED_FACE ( 'NONE', ( #28752 ), #69270, .T. ) ;
#78624 = CARTESIAN_POINT ( 'NONE',  ( 177.1099337379980625, 269.6391827967807444, 16.17709596969117669 ) ) ;
#78625 = CARTESIAN_POINT ( 'NONE',  ( 164.5648480107187197, 245.6123174360222094, 3.015887571020871238 ) ) ;
#78626 = CARTESIAN_POINT ( 'NONE',  ( 11.60290295393121696, 189.0530062829863027, -4.648177544792955347E-16 ) ) ;
#78627 = CARTESIAN_POINT ( 'NONE',  ( 71.54698464547352899, 65.28335351056534819, -12.36203232579594236 ) ) ;
#78628 = CARTESIAN_POINT ( 'NONE',  ( 163.7323023463233937, 247.0543288263758086, -6.244751637846886361 ) ) ;
#78629 = CARTESIAN_POINT ( 'NONE',  ( 113.2460989071574460, 230.0643266524160140, 9.188101187500095079 ) ) ;
#78630 = ORIENTED_EDGE ( 'NONE', *, *, #84131, .F. ) ;
#78631 = AXIS2_PLACEMENT_3D ( 'NONE', #99454, #59416, #82794 ) ;
#78632 = CIRCLE ( 'NONE', #34917, 3.299999999999978950 ) ;
#78633 = CARTESIAN_POINT ( 'NONE',  ( 147.2180753513904961, 275.6578090293250511, 0.4909717733184589261 ) ) ;
#78634 = DIRECTION ( 'NONE',  ( 1.000000000000000000, 0.000000000000000000, 0.000000000000000000 ) ) ;
#78635 = CARTESIAN_POINT ( 'NONE',  ( 26.18314342202568668, 41.82794442100486521, -10.00000000000000000 ) ) ;
#78636 = AXIS2_PLACEMENT_3D ( 'NONE', #32, #30917, #61804 ) ;
#78637 = CARTESIAN_POINT ( 'NONE',  ( 192.5672132233574700, 296.7161803602032819, 11.26440590052197521 ) ) ;
#78638 = CARTESIAN_POINT ( 'NONE',  ( 83.79506744998815293, 51.52028683484932259, -14.36816095265300319 ) ) ;
#78639 = CARTESIAN_POINT ( 'NONE',  ( -19.65312891409030271, 93.06504152958497400, 59.99999999999999289 ) ) ;
#78640 = ORIENTED_EDGE ( 'NONE', *, *, #30157, .F. ) ;
#78641 = CARTESIAN_POINT ( 'NONE',  ( 163.4178923001155681, 247.5989030008181260, -10.38047187240561442 ) ) ;
#78642 = CARTESIAN_POINT ( 'NONE',  ( 154.5673665054800949, 273.4584833364699534, -13.30136609530668501 ) ) ;
#78643 = CARTESIAN_POINT ( 'NONE',  ( 185.6000254797699256, 261.4070812443545151, 10.17022056266204011 ) ) ;
#78644 = CARTESIAN_POINT ( 'NONE',  ( 74.58922631747107346, 66.95469429158355013, 12.55546573254312470 ) ) ;
#78645 = CARTESIAN_POINT ( 'NONE',  ( 139.3894143317826888, 239.0327760586659736, 1.948934522072302763E-15 ) ) ;
#78646 = CARTESIAN_POINT ( 'NONE',  ( 198.7501991201633018, 286.4015524398827779, -18.58948563601804693 ) ) ;
#78647 = CARTESIAN_POINT ( 'NONE',  ( 185.9018016517766796, 296.7470552638663435, 4.635871442932423925 ) ) ;
#78648 = CARTESIAN_POINT ( 'NONE',  ( 157.8360072705708603, 257.2670114739976839, 17.12122855844125269 ) ) ;
#78649 = DIRECTION ( 'NONE',  ( -0.8660254037844387076, -0.4999999999999998890, -0.000000000000000000 ) ) ;
#78650 = CARTESIAN_POINT ( 'NONE',  ( 58.36173894231861681, 198.3768266524159856, 9.188101187500098632 ) ) ;
#78651 = CARTESIAN_POINT ( 'NONE',  ( 85.39636071719610300, 48.32640963909398124, -12.26545443191637297 ) ) ;
#78652 = EDGE_LOOP ( 'NONE', ( #91882, #61313, #435, #66758 ) ) ;
#78653 = CARTESIAN_POINT ( 'NONE',  ( 72.13197559556067517, 66.88302471189031451, 11.41260966439740798 ) ) ;
#78654 = DIRECTION ( 'NONE',  ( -0.8606332181800099290, 0.5092253565614338617, 0.000000000000000000 ) ) ;
#78655 = CARTESIAN_POINT ( 'NONE',  ( 67.66566145506487828, 69.67521865087169886, -0.2583700242925219270 ) ) ;
#78656 = CARTESIAN_POINT ( 'NONE',  ( 171.1954379026365132, 259.7559371881407060, 15.23461156733691979 ) ) ;
#78657 = DIRECTION ( 'NONE',  ( 0.8660254037844323793, 0.5000000000000108802, 1.093569679255778877E-14 ) ) ;
#78658 = CARTESIAN_POINT ( 'NONE',  ( 155.6048174803203210, 261.1315455520403361, -17.38645169541727498 ) ) ;
#78659 = CARTESIAN_POINT ( 'NONE',  ( 179.7248642212219920, 261.8487014404206548, 12.23902209130197782 ) ) ;
#78660 = CARTESIAN_POINT ( 'NONE',  ( 118.5773942495488882, 249.2677522451419065, -5.000000000000047962 ) ) ;
#78661 = LINE ( 'NONE', #62938, #28906 ) ;
#78662 = ORIENTED_EDGE ( 'NONE', *, *, #47231, .T. ) ;
#78663 = CARTESIAN_POINT ( 'NONE',  ( 163.4216610345155800, 247.5923753613567442, 10.58669027323842826 ) ) ;
#78664 = CARTESIAN_POINT ( 'NONE',  ( 87.96858562469613219, 44.79953861350612954, 4.806926248663378587 ) ) ;
#78665 = AXIS2_PLACEMENT_3D ( 'NONE', #97065, #75229, #59490 ) ;
#78666 = CARTESIAN_POINT ( 'NONE',  ( 18.30771692152332975, 187.5024278399160949, -9.188101187500093303 ) ) ;
#78667 = CARTESIAN_POINT ( 'NONE',  ( 19.84093639355121397, 13.58380873178786707, 6.180339887498953466 ) ) ;
#78669 = VECTOR ( 'NONE', #54289, 1000.000000000000114 ) ;
#78668 = CARTESIAN_POINT ( 'NONE',  ( 188.7259824843985427, 290.5464306864724335, -14.95866673843798189 ) ) ;
#78670 = CARTESIAN_POINT ( 'NONE',  ( 72.02976470237955198, 59.30830629416841759, -15.33705471575644808 ) ) ;
#78671 = PLANE ( 'NONE',  #75039 ) ;
#78673 = CARTESIAN_POINT ( 'NONE',  ( 55.71838369152838766, 209.6427522451419350, 10.00000000000009237 ) ) ;
#78672 = CARTESIAN_POINT ( 'NONE',  ( 12.69602586335324190, 7.734156793818200981, -2.889640176918245968E-15 ) ) ;
#78674 = CARTESIAN_POINT ( 'NONE',  ( 173.5202059484193171, 289.2069962268759582, 8.056742666160944921 ) ) ;
#78675 = DIRECTION ( 'NONE',  ( -0.8660254037844379305, -0.5000000000000016653, -3.252519625699479034E-16 ) ) ;
#78676 = CARTESIAN_POINT ( 'NONE',  ( 157.1458804504438831, 258.4623461901232417, -17.08829597948888335 ) ) ;
#78677 = CARTESIAN_POINT ( 'NONE',  ( 162.2432041231853646, 251.8243937157151322, -12.96429670712563009 ) ) ;
#78678 = ORIENTED_EDGE ( 'NONE', *, *, #40432, .T. ) ;
#78679 = AXIS2_PLACEMENT_3D ( 'NONE', #88388, #81755, #52299 ) ;
#78680 = CARTESIAN_POINT ( 'NONE',  ( 161.4388948769270087, 267.8778111258301919, 16.93954275417836541 ) ) ;
#78681 = CARTESIAN_POINT ( 'NONE',  ( 17.48697055717573789, 194.2365022471903728, 2.944929066748280225E-16 ) ) ;
#78682 = DIRECTION ( 'NONE',  ( 0.4999999999999995559, -0.8660254037844389297, 0.000000000000000000 ) ) ;
#78683 = CARTESIAN_POINT ( 'NONE',  ( 202.3425522658138505, 280.1794142728863903, 15.86053073629060961 ) ) ;
#78684 = CARTESIAN_POINT ( 'NONE',  ( -4.262896616726100874, 168.3458772461660544, 9.188101187500095079 ) ) ;
#78685 = CARTESIAN_POINT ( 'NONE',  ( 24.26418115112394247, 34.98502408145593279, -5.678558825948271327 ) ) ;
#78687 = CARTESIAN_POINT ( 'NONE',  ( 170.8865616681041786, 262.8912071418242817, 16.88624067591380040 ) ) ;
#78686 = CARTESIAN_POINT ( 'NONE',  ( 164.0691337515192174, 260.5160139313006766, -16.15666796438198460 ) ) ;
#78688 = EDGE_CURVE ( 'NONE', #71267, #57136, #73921, .T. ) ;
#78689 = CARTESIAN_POINT ( 'NONE',  ( 48.77433535142597520, 99.76555324011610537, -10.00000000000000000 ) ) ;
#78690 = CARTESIAN_POINT ( 'NONE',  ( 204.1633547645365638, 275.3510256380408237, 13.36249479004741580 ) ) ;
#78691 = CARTESIAN_POINT ( 'NONE',  ( 183.2640056662122277, 257.8466347788053099, -2.285499766636972296 ) ) ;
#78692 = CARTESIAN_POINT ( 'NONE',  ( 65.81576594865798313, 68.96196425835729826, 2.168796872202445769 ) ) ;
#78693 = VERTEX_POINT ( 'NONE', #62116 ) ;
#78694 = CARTESIAN_POINT ( 'NONE',  ( 137.7201641159153098, 256.9865022471903444, 10.00000000000009415 ) ) ;
#78695 =( NAMED_UNIT ( * ) PLANE_ANGLE_UNIT ( ) SI_UNIT ( $, .RADIAN. ) );
#78696 = CARTESIAN_POINT ( 'NONE',  ( 178.4611519391757497, 285.4942648953933144, 12.99929199147914716 ) ) ;
#78697 = CARTESIAN_POINT ( 'NONE',  ( 155.8136364298667331, 279.2791936157335044, -5.243594246769619716 ) ) ;
#78698 = CARTESIAN_POINT ( 'NONE',  ( 8.146472837920740062, 20.10171378149916777, 9.188101187500008038 ) ) ;
#78699 = CARTESIAN_POINT ( 'NONE',  ( 160.6683587774825526, 252.3612347591322020, 15.32470308806421855 ) ) ;
#78700 = AXIS2_PLACEMENT_3D ( 'NONE', #27808, #58683, #43982 ) ;
#78701 = VECTOR ( 'NONE', #53457, 1000.000000000000114 ) ;
#78702 = CARTESIAN_POINT ( 'NONE',  ( 152.6945189806187955, 266.1723304187151484, 16.62409282110771613 ) ) ;
#78703 = CARTESIAN_POINT ( 'NONE',  ( 191.8986733338516331, 296.2687432111309249, 12.49828825629462337 ) ) ;
#78704 = VECTOR ( 'NONE', #71605, 1000.000000000000000 ) ;
#78705 = CARTESIAN_POINT ( 'NONE',  ( 157.5215017335775940, 258.4853116787141971, -16.92298772477023761 ) ) ;
#78706 = CARTESIAN_POINT ( 'NONE',  ( 87.89611104468033886, 44.97730679797473385, 6.346758332113883405 ) ) ;
#78707 = CARTESIAN_POINT ( 'NONE',  ( -61.39381520214497101, 38.43978098112751951, -10.00000000000000000 ) ) ;
#78708 = EDGE_LOOP ( 'NONE', ( #99122, #9606, #8723, #20958 ) ) ;
#78709 = VERTEX_POINT ( 'NONE', #7953 ) ;
#78710 = DIRECTION ( 'NONE',  ( -0.9981280818701456781, -0.06115825522547174015, 0.000000000000000000 ) ) ;
#78711 = CARTESIAN_POINT ( 'NONE',  ( 85.97987434235641047, 47.62252706626447463, 10.87664434560344340 ) ) ;
#78712 = ORIENTED_EDGE ( 'NONE', *, *, #20158, .T. ) ;
#78713 = CARTESIAN_POINT ( 'NONE',  ( 8.953011887168695893, 182.6427522451419350, 10.00000000000009415 ) ) ;
#78714 = CARTESIAN_POINT ( 'NONE',  ( 73.75461245277466560, 71.97758258259658248, 0.000000000000000000 ) ) ;
#78715 = ORIENTED_EDGE ( 'NONE', *, *, #88434, .F. ) ;
#78716 = CARTESIAN_POINT ( 'NONE',  ( 68.90560621877192204, 63.79076715805910425, -12.30144644517788421 ) ) ;
#78717 = FACE_OUTER_BOUND ( 'NONE', #90730, .T. ) ;
#78718 = CARTESIAN_POINT ( 'NONE',  ( 12.17791779510973171, 30.52903772873356658, -1.583844403245363575 ) ) ;
#78719 = VERTEX_POINT ( 'NONE', #63136 ) ;
#78720 = CARTESIAN_POINT ( 'NONE',  ( 203.4846675955504907, 278.2012124936790087, 16.44718627781510634 ) ) ;
#78721 = LINE ( 'NONE', #29247, #22324 ) ;
#78722 = CARTESIAN_POINT ( 'NONE',  ( 190.8443993347725325, 300.0947993426467519, 8.522468760355437212 ) ) ;
#78723 = CARTESIAN_POINT ( 'NONE',  ( 38.08795742478228163, 27.15404122711136381, 8.090169943749479842 ) ) ;
#78724 = ORIENTED_EDGE ( 'NONE', *, *, #86126, .T. ) ;
#78725 = LINE ( 'NONE', #80254, #29336 ) ;
#78726 = ORIENTED_EDGE ( 'NONE', *, *, #88894, .F. ) ;
#78727 = ORIENTED_EDGE ( 'NONE', *, *, #76587, .T. ) ;
#78728 = CARTESIAN_POINT ( 'NONE',  ( 73.68192328755300480, 62.65634618987721183, 14.56402732850078152 ) ) ;
#78729 = ORIENTED_EDGE ( 'NONE', *, *, #93807, .F. ) ;
#78730 = CARTESIAN_POINT ( 'NONE',  ( 45.80758703142363686, 72.03864405183792030, 10.00000000000000000 ) ) ;
#78731 = EDGE_LOOP ( 'NONE', ( #12549, #35490, #33369, #89001 ) ) ;
#78732 = CARTESIAN_POINT ( 'NONE',  ( 81.96249893094650929, 45.51685736730845377, 10.90602769004302530 ) ) ;
#78733 = CARTESIAN_POINT ( 'NONE',  ( 71.28049052964838950, 69.11027213759044230, 8.374494312738244517 ) ) ;
#78734 = CARTESIAN_POINT ( 'NONE',  ( 148.2670916631250861, 273.8408594794321971, -7.980554973576580835 ) ) ;
#78735 = B_SPLINE_CURVE_WITH_KNOTS ( 'NONE', 3,
 ( #73892, #36365, #28778, #44964 ),
 .UNSPECIFIED., .F., .F.,
 ( 4, 4 ),
 ( 0.01084982095175494182, 0.01228877948971598445 ),
 .UNSPECIFIED. ) ;
#78736 = CARTESIAN_POINT ( 'NONE',  ( -76.38857681351474582, 54.22815603855766398, -10.00000000000000000 ) ) ;
#78737 = CARTESIAN_POINT ( 'NONE',  ( 159.1305972428150710, 255.0247158671010084, -16.79903268104793312 ) ) ;
#78738 = ORIENTED_EDGE ( 'NONE', *, *, #70332, .T. ) ;
#78739 = CARTESIAN_POINT ( 'NONE',  ( 167.0389919848387592, 247.0514236948299072, 1.939505287189084326 ) ) ;
#78740 = B_SPLINE_CURVE_WITH_KNOTS ( 'NONE', 3,
 ( #86445, #46880, #9385, #54974, #38262, #69175, #53962, #85951, #84919, #55459, #47374, #78297, #15463, #46360, #8881, #39749 ),
 .UNSPECIFIED., .F., .F.,
 ( 4, 1, 2, 2, 2, 1, 2, 2, 4 ),
 ( 0.000000000000000000, 0.1250000000000003053, 0.1875000000000004441, 0.2500000000000006106, 0.4999999999999976130, 0.6249999999999962252, 0.6874999999999963363, 0.7499999999999964473, 1.000000000000000000 ),
 .UNSPECIFIED. ) ;
#78741 = CARTESIAN_POINT ( 'NONE',  ( 23.25741983583088413, 25.37878583063841376, 9.188101187500006262 ) ) ;
#78743 = EDGE_CURVE ( 'NONE', #65907, #96690, #94081, .T. ) ;
#78742 = VECTOR ( 'NONE', #12328, 1000.000000000000000 ) ;
#78744 = DIRECTION ( 'NONE',  ( 0.1378186779084994706, -0.2387089523694924387, -0.9612616959383186721 ) ) ;
#78746 = VERTEX_POINT ( 'NONE', #78862 ) ;
#78745 = CARTESIAN_POINT ( 'NONE',  ( 159.2077906806335932, 254.8910129107889588, 16.14624949541834553 ) ) ;
#78747 = VECTOR ( 'NONE', #92592, 1000.000000000000114 ) ;
#78748 = CARTESIAN_POINT ( 'NONE',  ( 190.6257723682618064, 300.4734723565479158, 5.229856753389036328 ) ) ;
#78749 = DIRECTION ( 'NONE',  ( -0.2471055264905585858, 0.9689885751534038638, 0.000000000000000000 ) ) ;
#78750 = CARTESIAN_POINT ( 'NONE',  ( 159.9770824720811220, 253.5585604421560788, -16.42166711341322483 ) ) ;
#78751 = CARTESIAN_POINT ( 'NONE',  ( 161.1252381510204259, 272.2179608743590506, -16.27752944574491778 ) ) ;
#78752 = EDGE_CURVE ( 'NONE', #73362, #24288, #92090, .T. ) ;
#78753 = CARTESIAN_POINT ( 'NONE',  ( 161.8016137473484548, 250.3983795733946636, 14.25000412375400316 ) ) ;
#78754 = CARTESIAN_POINT ( 'NONE',  ( 190.8174609004742592, 261.9199525876146595, -0.4327646785539380758 ) ) ;
#78755 = VERTEX_POINT ( 'NONE', #77856 ) ;
#78756 = CARTESIAN_POINT ( 'NONE',  ( 187.5197201530054656, 260.4900132203839576, 7.667313317775144021 ) ) ;
#78757 = CARTESIAN_POINT ( 'NONE',  ( 75.00762831775021766, 66.90256318391983825, -13.19391308334217605 ) ) ;
#78759 = ADVANCED_FACE ( 'NONE', ( #40319 ), #24829, .F. ) ;
#78758 = CARTESIAN_POINT ( 'NONE',  ( 164.8251969117060298, 245.1613799118173063, -1.508678420156898348 ) ) ;
#78760 = CARTESIAN_POINT ( 'NONE',  ( 7.293129863248505984, 185.0177522451419065, 5.000000000000046185 ) ) ;
#78761 = CARTESIAN_POINT ( 'NONE',  ( 92.62404252742300059, 212.0327760586659451, 1.948934522072302763E-15 ) ) ;
#78762 = CARTESIAN_POINT ( 'NONE',  ( 82.34414259798680291, 40.36743405348067881, -1.213300603182490001 ) ) ;
#78763 = PLANE ( 'NONE',  #32526 ) ;
#78764 = CARTESIAN_POINT ( 'NONE',  ( 168.2168545625571596, 279.0239035984992597, -13.38986689698590737 ) ) ;
#78766 = CARTESIAN_POINT ( 'NONE',  ( 75.88363445057348144, 65.49265179502715739, 14.31053417012051554 ) ) ;
#78765 = CARTESIAN_POINT ( 'NONE',  ( 8.998290926605619688, 169.8768266524160140, 9.188101187500098632 ) ) ;
#78767 = CARTESIAN_POINT ( 'NONE',  ( 161.1611771195837548, 251.5076483517112536, 14.17749514252127163 ) ) ;
#78768 = VECTOR ( 'NONE', #9758, 1000.000000000000114 ) ;
#78769 = ORIENTED_EDGE ( 'NONE', *, *, #12930, .T. ) ;
#78770 = AXIS2_PLACEMENT_3D ( 'NONE', #2741, #72136, #94958 ) ;
#78772 = ORIENTED_EDGE ( 'NONE', *, *, #89022, .T. ) ;
#78771 = PRODUCT_DEFINITION_CONTEXT ( 'detailed design', #50890, 'design' ) ;
#78773 = CARTESIAN_POINT ( 'NONE',  ( 188.4359633627616404, 260.4672849544427322, -6.269197070210934974 ) ) ;
#78774 = CARTESIAN_POINT ( 'NONE',  ( 81.50940192328098988, 59.54589321767952725, 0.1873032967079516220 ) ) ;
#78775 = AXIS2_PLACEMENT_3D ( 'NONE', #11608, #58664, #28781 ) ;
#78776 = CARTESIAN_POINT ( 'NONE',  ( 84.12407613425114050, 43.74822318919484587, 7.135943603182840711 ) ) ;
#78777 = CARTESIAN_POINT ( 'NONE',  ( 38.19941146435361645, 192.8615022471902591, -10.00000000000009592 ) ) ;
#78778 = CARTESIAN_POINT ( 'NONE',  ( 82.30424563670493399, 42.66182458811155698, 6.991864634221377273 ) ) ;
#78779 = CARTESIAN_POINT ( 'NONE',  ( 48.95103868752454446, 97.61288834769685252, 10.00000000000000000 ) ) ;
#78780 = CARTESIAN_POINT ( 'NONE',  ( 36.16983797034238535, 185.5643266524159856, -9.188101187500093303 ) ) ;
#78781 = CARTESIAN_POINT ( 'NONE',  ( 76.50299338235490154, 221.6427522451419065, 10.00000000000009237 ) ) ;
#78782 = CARTESIAN_POINT ( 'NONE',  ( 196.1813314310145415, 275.5097970061073056, 15.45116200187350586 ) ) ;
#78783 = ORIENTED_EDGE ( 'NONE', *, *, #51113, .T. ) ;
#78784 = CARTESIAN_POINT ( 'NONE',  ( 153.5359445101103404, 274.1292087801049888, -12.02885945652445976 ) ) ;
#78785 = CARTESIAN_POINT ( 'NONE',  ( 175.1707756323828846, 281.3988818488836046, -14.22492014867428090 ) ) ;
#78786 = CARTESIAN_POINT ( 'NONE',  ( -11.73236572436687730, 164.0333772461660544, 9.188101187500095079 ) ) ;
#78787 = CARTESIAN_POINT ( 'NONE',  ( 66.50871531961365690, 67.78145361369897159, -6.921353532618302218 ) ) ;
#78788 = CARTESIAN_POINT ( 'NONE',  ( 49.09245556086620610, 93.56363653685789927, 10.00000000000000000 ) ) ;
#78789 = CARTESIAN_POINT ( 'NONE',  ( 151.1126408083691501, 268.9122237844355254, -15.82705194100464396 ) ) ;
#78790 = CARTESIAN_POINT ( 'NONE',  ( 187.5768131394391958, 283.2038405381267125, 16.23894686413832034 ) ) ;
#78791 = CARTESIAN_POINT ( 'NONE',  ( 194.4666154385731431, 293.8209370148700827, -14.56896502715340702 ) ) ;
#78792 = ADVANCED_FACE ( 'NONE', ( #18055 ), #71762, .F. ) ;
#78793 = EDGE_CURVE ( 'NONE', #48146, #70901, #25653, .T. ) ;
#78794 = CARTESIAN_POINT ( 'NONE',  ( 189.7252522328423368, 262.4931234074404642, 8.270058708727324515 ) ) ;
#78795 = CARTESIAN_POINT ( 'NONE',  ( 163.9587364689194260, 246.6621334214722481, 5.816126667419880825 ) ) ;
#78796 = CARTESIAN_POINT ( 'NONE',  ( 148.0389988358468827, 274.2359278451201590, 7.783622668412842671 ) ) ;
#78797 = ORIENTED_EDGE ( 'NONE', *, *, #74352, .F. ) ;
#78798 = CARTESIAN_POINT ( 'NONE',  ( 156.0916382163451601, 277.5285333452508212, -10.52960063827285886 ) ) ;
#78799 = CARTESIAN_POINT ( 'NONE',  ( 208.2764314485352770, 269.9016340424377063, 2.433736665191914117 ) ) ;
#78800 = CARTESIAN_POINT ( 'NONE',  ( 181.2716795336521329, 267.9920306002611028, 16.35033316730358877 ) ) ;
#78801 = CARTESIAN_POINT ( 'NONE',  ( 106.9945647975297760, 223.3923013555410080, 4.594050593750050204 ) ) ;
#78802 = CARTESIAN_POINT ( 'NONE',  ( 9.796739006517501736, 23.84336893147754566, -7.433330006724137462 ) ) ;
#78803 = CARTESIAN_POINT ( 'NONE',  ( 191.0900422946452011, 299.6693332556258724, 8.872191398975367349 ) ) ;
#78804 = EDGE_CURVE ( 'NONE', #91470, #38315, #69054, .T. ) ;
#78805 = CARTESIAN_POINT ( 'NONE',  ( -41.62359735524142934, 26.60228115600143184, -10.00000000000000000 ) ) ;
#78807 = CARTESIAN_POINT ( 'NONE',  ( 166.5418805794664934, 264.7512503615053561, 17.71810435351582669 ) ) ;
#78806 = CARTESIAN_POINT ( 'NONE',  ( 195.6974783896144174, 291.6890198465123945, 16.70600479393688431 ) ) ;
#78808 = FACE_OUTER_BOUND ( 'NONE', #11099, .T. ) ;
#78809 = EDGE_CURVE ( 'NONE', #48939, #29494, #46691, .T. ) ;
#78810 = CARTESIAN_POINT ( 'NONE',  ( 29.85841906089621389, 18.20801979619929867, -3.090169943749474069 ) ) ;
#78811 = CARTESIAN_POINT ( 'NONE',  ( 196.8104339078508076, 289.7613243423628546, -16.40335862274955403 ) ) ;
#78812 = AXIS2_PLACEMENT_3D ( 'NONE', #22658, #44942, #84004 ) ;
#78813 = DIRECTION ( 'NONE',  ( -0.9414334852479556703, -0.3371987438498062484, 0.000000000000000000 ) ) ;
#78814 = CARTESIAN_POINT ( 'NONE',  ( 173.2147484828852839, 289.7388750556115724, -1.099818896463917284 ) ) ;
#78815 = CARTESIAN_POINT ( 'NONE',  ( 67.41069134358542669, 70.04696837240071261, -4.305487806446024446E-08 ) ) ;
#78816 = ORIENTED_EDGE ( 'NONE', *, *, #73080, .T. ) ;
#78817 = DIRECTION ( 'NONE',  ( -0.8143688203140567738, 0.5803476755362181327, 0.000000000000000000 ) ) ;
#78818 = CARTESIAN_POINT ( 'NONE',  ( 25.95703985525452850, 15.39040679176983240, 1.333680081654574804E-15 ) ) ;
#78819 = AXIS2_PLACEMENT_3D ( 'NONE', #15518, #17535, #71257 ) ;
#78820 = CARTESIAN_POINT ( 'NONE',  ( 186.5128128464827455, 296.3652354721813822, -8.829210103799347564 ) ) ;
#78821 = EDGE_CURVE ( 'NONE', #51318, #95480, #54264, .T. ) ;
#78822 = VERTEX_POINT ( 'NONE', #23377 ) ;
#78823 = CARTESIAN_POINT ( 'NONE',  ( 72.13210804887378913, 72.31988279945024090, 1.151498749227306995 ) ) ;
#78824 = B_SPLINE_SURFACE_WITH_KNOTS ( 'NONE', 3, 1, ( 
 ( #52100, #44491 ),
 ( #82565, #98737 ),
 ( #29315, #85034 ),
 ( #99716, #8999 ),
 ( #403, #94139 ),
 ( #6997, #47985 ),
 ( #70808, #54573 ),
 ( #8505, #15580 ),
 ( #30305, #85557 ),
 ( #92639, #32296 ),
 ( #61687, #22711 ),
 ( #46483, #84545 ),
 ( #63199, #45975 ),
 ( #23681, #77414 ),
 ( #8017, #37881 ),
 ( #16099, #902 ),
 ( #86071, #62178 ),
 ( #23188, #38386 ),
 ( #53589, #68791 ),
 ( #15087, #100222 ),
 ( #54081, #55085 ),
 ( #39375, #61190 ),
 ( #24694, #69298 ),
 ( #70291, #17092 ),
 ( #39870, #30807 ),
 ( #47002, #38891 ),
 ( #31781, #77916 ),
 ( #55577, #86559 ),
 ( #62683, #92158 ),
 ( #69793, #76892 ),
 ( #31292, #93132 ),
 ( #93636, #24204 ),
 ( #16596, #7492 ),
 ( #47492, #78417 ) ),
 .UNSPECIFIED., .T., .F., .F.,
 ( 4, 2, 2, 2, 2, 2, 2, 2, 2, 2, 2, 2, 2, 2, 2, 2, 4 ),
 ( 2, 2 ),
 ( 0.000000000000000000, 0.06250000000000000000, 0.1250000000000000000, 0.1875000000000000000, 0.2500000000000000000, 0.3125000000000000000, 0.3750000000000000000, 0.4375000000000000000, 0.5000000000000000000, 0.5625000000000000000, 0.6250000000000000000, 0.6875000000000000000, 0.7500000000000000000, 0.8125000000000000000, 0.8750000000000000000, 0.9375000000000000000, 1.000000000000000000 ),
 ( 0.000000000000000000, 1.000000000000000000 ),
 .UNSPECIFIED. ) ;
#78825 = CARTESIAN_POINT ( 'NONE',  ( 78.91779975210128839, 49.13212207373893392, 14.41565681662890341 ) ) ;
#78826 = CARTESIAN_POINT ( 'NONE',  ( 182.7235263772020346, 258.7439045234889932, -9.311915605583727995 ) ) ;
#78827 = CARTESIAN_POINT ( 'NONE',  ( 189.2759868517105986, 283.1334299989923124, 17.63300985876514915 ) ) ;
#78828 = CARTESIAN_POINT ( 'NONE',  ( 153.4242699508872647, 264.9083646613370320, 16.62000820703435267 ) ) ;
#78829 = CIRCLE ( 'NONE', #86976, 0.1418229129680828593 ) ;
#78830 = EDGE_LOOP ( 'NONE', ( #25690, #81454, #14082, #30018 ) ) ;
#78831 = CARTESIAN_POINT ( 'NONE',  ( 161.6059911608744812, 269.3330164776378410, -17.24104619120290494 ) ) ;
#78832 = CARTESIAN_POINT ( 'NONE',  ( 39.89592612264573290, 25.96004757982093025, -5.678558825948276656 ) ) ;
#78833 = CARTESIAN_POINT ( 'NONE',  ( 177.2074197889685365, 274.7965786531511867, -16.93324248537096111 ) ) ;
#78834 = ORIENTED_EDGE ( 'NONE', *, *, #43523, .F. ) ;
#78835 = CARTESIAN_POINT ( 'NONE',  ( 167.7018358744333000, 280.9558910960651019, 11.69324581573506805 ) ) ;
#78836 = LINE ( 'NONE', #24113, #49951 ) ;
#78837 = CARTESIAN_POINT ( 'NONE',  ( -28.78056054657192320, 23.66266410781089391, 10.00000000000000000 ) ) ;
#78838 = ORIENTED_EDGE ( 'NONE', *, *, #78804, .F. ) ;
#78839 = CARTESIAN_POINT ( 'NONE',  ( 86.44990779080247023, 47.08395378219080385, -10.04107686951885192 ) ) ;
#78840 = FACE_OUTER_BOUND ( 'NONE', #73461, .T. ) ;
#78841 = CARTESIAN_POINT ( 'NONE',  ( 66.61587002248261058, 209.2677522451418497, 10.00000000000009592 ) ) ;
#78842 = CARTESIAN_POINT ( 'NONE',  ( 17.74977768659132593, 33.18080186712593616, 3.090169943749475401 ) ) ;
#78843 = CARTESIAN_POINT ( 'NONE',  ( -19.65312891409030271, 93.06504152958497400, 60.00000000000000000 ) ) ;
#78844 = CARTESIAN_POINT ( 'NONE',  ( 85.82777105212227298, 44.89325558436473784, -8.300099996375795541 ) ) ;
#78845 = CIRCLE ( 'NONE', #73994, 17.82106496071138935 ) ;
#78846 = CARTESIAN_POINT ( 'NONE',  ( 80.16024689640217105, 44.74056149942663296, 11.12043925283496115 ) ) ;
#78847 = CARTESIAN_POINT ( 'NONE',  ( 84.86414386349152039, 49.99136666923657657, -13.21250203946878621 ) ) ;
#78848 = CARTESIAN_POINT ( 'NONE',  ( 155.6281496932864457, 261.0911329737299980, -18.07904265579665548 ) ) ;
#78849 = ORIENTED_EDGE ( 'NONE', *, *, #39203, .T. ) ;
#78850 = ORIENTED_EDGE ( 'NONE', *, *, #16354, .T. ) ;
#78851 = CARTESIAN_POINT ( 'NONE',  ( 178.9732493734400407, 260.1133086608659823, 12.29518698491872186 ) ) ;
#78852 = EDGE_LOOP ( 'NONE', ( #10533, #19300, #35729, #51705 ) ) ;
#78853 = CARTESIAN_POINT ( 'NONE',  ( 77.15726504878196579, 49.33124488487003845, -15.40379270228043573 ) ) ;
#78854 = VERTEX_POINT ( 'NONE', #61872 ) ;
#78855 = CARTESIAN_POINT ( 'NONE',  ( 30.65561236560288805, 105.1146769143126960, 59.99999999999999289 ) ) ;
#78856 = FACE_OUTER_BOUND ( 'NONE', #29973, .T. ) ;
#78857 = VERTEX_POINT ( 'NONE', #69488 ) ;
#78858 = AXIS2_PLACEMENT_3D ( 'NONE', #91921, #22477, #45754 ) ;
#78859 = CARTESIAN_POINT ( 'NONE',  ( 165.0803978706131545, 244.7193588848498678, -1.793249961207334486 ) ) ;
#78860 = CARTESIAN_POINT ( 'NONE',  ( 71.54202820451581601, 72.24755327463289234, 2.386327895633298279 ) ) ;
#78861 = CARTESIAN_POINT ( 'NONE',  ( 196.4404618256887147, 284.6410079857341771, -17.31378922566917211 ) ) ;
#78862 = CARTESIAN_POINT ( 'NONE',  ( 80.44297273216874089, 44.73620253192707708, -11.65665792466250039 ) ) ;
#78863 = CARTESIAN_POINT ( 'NONE',  ( 167.9449114283013955, 248.6326271889187751, -4.934543203145975276 ) ) ;
#78864 = DIRECTION ( 'NONE',  ( 1.000000000000000000, 0.000000000000000000, 0.000000000000000000 ) ) ;
#78865 = CARTESIAN_POINT ( 'NONE',  ( 153.8909117540673037, 279.9112642337403258, 2.216438095792761409 ) ) ;
#78866 = B_SPLINE_CURVE_WITH_KNOTS ( 'NONE', 3,
 ( #2933, #33822, #50983, #4911 ),
 .UNSPECIFIED., .F., .F.,
 ( 4, 4 ),
 ( 0.008486201099387760682, 0.01670945231454646837 ),
 .UNSPECIFIED. ) ;
#78867 = CARTESIAN_POINT ( 'NONE',  ( 124.8563387505838165, 233.7048013555409796, 4.594050593750051981 ) ) ;
#78869 = CARTESIAN_POINT ( 'NONE',  ( 183.4730159057174319, 260.4080488702623484, -9.317792726801004122 ) ) ;
#78868 = B_SPLINE_CURVE_WITH_KNOTS ( 'NONE', 3,
 ( #22800, #53679, #6608, #20828 ),
 .UNSPECIFIED., .F., .F.,
 ( 4, 4 ),
 ( 0.01467339918438643684, 0.02339405670009707047 ),
 .UNSPECIFIED. ) ;
#78870 = CARTESIAN_POINT ( 'NONE',  ( 40.74993669414823927, 32.03085787977766330, 9.188101187500006262 ) ) ;
#78871 = VERTEX_POINT ( 'NONE', #98423 ) ;
#78872 = ADVANCED_FACE ( 'NONE', ( #37092 ), #59888, .F. ) ;
#78874 = EDGE_LOOP ( 'NONE', ( #81119, #8316, #72121, #86877 ) ) ;
#78873 = CARTESIAN_POINT ( 'NONE',  ( 85.46624767806203238, 43.53765940098641352, -6.277485798516380555 ) ) ;
#78875 = CARTESIAN_POINT ( 'NONE',  ( 203.4267045473674500, 276.1086550667716324, 13.32450178018177844 ) ) ;
#78876 = DIRECTION ( 'NONE',  ( 0.4999999999999998890, -0.8660254037844385966, 0.000000000000000000 ) ) ;
#78877 = EDGE_CURVE ( 'NONE', #26239, #39540, #62886, .T. ) ;
#78878 = CARTESIAN_POINT ( 'NONE',  ( 173.8731466349179016, 289.7565554419105069, -4.721349978305271478 ) ) ;
#78879 = CARTESIAN_POINT ( 'NONE',  ( 147.3488861203839235, 275.4312381312514049, 3.942095418248577676 ) ) ;
#78880 = DIRECTION ( 'NONE',  ( -0.000000000000000000, -0.000000000000000000, -1.000000000000000000 ) ) ;
#78881 = FACE_OUTER_BOUND ( 'NONE', #90179, .T. ) ;
#78882 = CARTESIAN_POINT ( 'NONE',  ( 173.8535554309253257, 287.2246996319072423, -9.538136335621828721 ) ) ;
#78883 = CARTESIAN_POINT ( 'NONE',  ( 194.9515580553570260, 292.9809917638447132, 16.65666034366562798 ) ) ;
#78884 = CARTESIAN_POINT ( 'NONE',  ( 177.1268731193232497, 255.9947964353676468, -7.287581347330274184 ) ) ;
#78885 = ORIENTED_EDGE ( 'NONE', *, *, #16316, .F. ) ;
#78886 = CARTESIAN_POINT ( 'NONE',  ( 147.6095889327917803, 274.9796876144846465, -8.460961150142429332 ) ) ;
#78887 = CARTESIAN_POINT ( 'NONE',  ( 65.75369581714585365, 69.08918575267863105, -0.1828176307183302651 ) ) ;
#78888 = ORIENTED_EDGE ( 'NONE', *, *, #75850, .T. ) ;
#78890 = EDGE_CURVE ( 'NONE', #15755, #66560, #60419, .T. ) ;
#78889 = CARTESIAN_POINT ( 'NONE',  ( -40.42249077443060656, 27.53003111760058275, -10.00000000000000000 ) ) ;
#78891 = CARTESIAN_POINT ( 'NONE',  ( 191.0209356936215386, 283.3490554861720625, -16.57420257736403713 ) ) ;
#78892 = CARTESIAN_POINT ( 'NONE',  ( 152.2897644507763459, 266.8733858289956515, -15.49661418983042083 ) ) ;
#78893 = CARTESIAN_POINT ( 'NONE',  ( 148.9266665119372703, 272.6984423298952152, 12.06339424062075061 ) ) ;
#78894 = CIRCLE ( 'NONE', #35185, 70.00000000000001421 ) ;
#78895 = CARTESIAN_POINT ( 'NONE',  ( 202.7599932440484451, 279.4563852894229967, 15.58249343055423353 ) ) ;
#78897 = CARTESIAN_POINT ( 'NONE',  ( 151.5138970483880030, 274.8970949040892719, -9.081682327913926045 ) ) ;
#78896 = CARTESIAN_POINT ( 'NONE',  ( 153.4014598655621739, 270.1403366047916847, 14.11843096852130941 ) ) ;
#78898 = CARTESIAN_POINT ( 'NONE',  ( 153.0790963368640689, 265.5062228982576471, -17.74594954892339160 ) ) ;
#78899 = ORIENTED_EDGE ( 'NONE', *, *, #14534, .T. ) ;
#78900 = CARTESIAN_POINT ( 'NONE',  ( 205.1662051911351057, 272.1315205505885046, -9.477979197527140798 ) ) ;
#78901 = CARTESIAN_POINT ( 'NONE',  ( 187.4088158364907315, 261.5390839597025092, -9.233908393253857483 ) ) ;
#78902 = CARTESIAN_POINT ( 'NONE',  ( 193.4438847740023846, 276.1245385600062718, -16.33226197978559213 ) ) ;
#78903 = CARTESIAN_POINT ( 'NONE',  ( 58.68017357788676946, 217.3877816888190750, 5.188172501216618598E-14 ) ) ;
#78904 = ADVANCED_FACE ( 'NONE', ( #7183 ), #91331, .T. ) ;
#78905 = CARTESIAN_POINT ( 'NONE',  ( 188.0737869051473012, 299.5124861214166572, -3.734995909225475863 ) ) ;
#78906 = ADVANCED_FACE ( 'NONE', ( #102 ), #91833, .F. ) ;
#78907 = CARTESIAN_POINT ( 'NONE',  ( 85.02612526452620045, 46.67130807634502077, 10.38696136103375878 ) ) ;
#78908 = CARTESIAN_POINT ( 'NONE',  ( -27.42236680055714260, 166.5217562850347406, 1.224646799147364892E-15 ) ) ;
#78909 = CIRCLE ( 'NONE', #22251, 17.82106496071138224 ) ;
#78910 =( BOUNDED_CURVE ( )  B_SPLINE_CURVE ( 2, ( #37388, #75932, #84539, #75418, #60176, #28806, #29801, #91141, #21217 ),
 .UNSPECIFIED., .F., .T. ) 
 B_SPLINE_CURVE_WITH_KNOTS ( ( 3, 2, 2, 2, 3 ),
 ( 0.8024193548387096309, 0.8037634408602150060, 0.8064516129032257563, 0.8091397849462365066, 0.8104838709677418818 ),
 .UNSPECIFIED. ) 
 CURVE ( )  GEOMETRIC_REPRESENTATION_ITEM ( )  RATIONAL_B_SPLINE_CURVE ( ( 0.9330127018922194093, 0.9330127018922194093, 1.000000000000000000, 0.8660254037844387076, 1.000000000000000000, 0.8660254037844387076, 1.000000000000000000, 0.9330127018922194093, 0.9330127018922194093 ) ) 
 REPRESENTATION_ITEM ( '' )  );
#78911 = CARTESIAN_POINT ( 'NONE',  ( 74.39841895140679640, 68.21392270468032848, 11.45628786500076579 ) ) ;
#78912 = CARTESIAN_POINT ( 'NONE',  ( 166.2786170299253854, 246.9376851968044377, -4.638038840367427085 ) ) ;
#78913 = CARTESIAN_POINT ( 'NONE',  ( -5.237175195983594378, 167.7833772461660828, -9.188101187500095079 ) ) ;
#78914 = CARTESIAN_POINT ( 'NONE',  ( 83.31357524521028779, 231.1589784336661637, -6.496448406907675876E-16 ) ) ;
#78915 = CARTESIAN_POINT ( 'NONE',  ( 70.00074031614300907, 71.54231853062985635, 1.101452585462014300 ) ) ;
#78916 = CARTESIAN_POINT ( 'NONE',  ( 182.2373335159190901, 280.9600371166583841, -17.30031729693378040 ) ) ;
#78917 = CARTESIAN_POINT ( 'NONE',  ( -19.65312891409030271, 93.06504152958497400, 177.5919119679930134 ) ) ;
#78918 = CARTESIAN_POINT ( 'NONE',  ( 202.9490938173916561, 279.1288534886517709, -16.56031645010252973 ) ) ;
#78919 = CIRCLE ( 'NONE', #35214, 17.82106496071138224 ) ;
#78920 = CARTESIAN_POINT ( 'NONE',  ( 78.09662876767376360, 55.14805409318260843, 16.10810231782577873 ) ) ;
#78921 = CYLINDRICAL_SURFACE ( 'NONE', #4475, 17.82106496071139645 ) ;
#78922 = AXIS2_PLACEMENT_3D ( 'NONE', #76363, #53530, #13072 ) ;
#78923 = CARTESIAN_POINT ( 'NONE',  ( 165.8866640751390094, 265.8956478032751534, 17.81115609982314751 ) ) ;
#78925 = CARTESIAN_POINT ( 'NONE',  ( 162.6541320028305506, 248.9217746405196294, -10.16950121496441817 ) ) ;
#78924 = CARTESIAN_POINT ( 'NONE',  ( 190.0047355206681914, 300.4812981626290593, -1.397688852404484372 ) ) ;
#78926 = CARTESIAN_POINT ( 'NONE',  ( 178.2461545249785502, 289.9108068321567657, 9.551079046322911381 ) ) ;
#78927 = EDGE_CURVE ( 'NONE', #94071, #58717, #90854, .T. ) ;
#78928 = PLANE ( 'NONE',  #65319 ) ;
#78929 = CARTESIAN_POINT ( 'NONE',  ( 80.74974841587442143, 43.27611110060701805, 10.01619596027649806 ) ) ;
#78930 = CARTESIAN_POINT ( 'NONE',  ( 80.38505107983586129, 54.19253253477483412, -15.81918041010719023 ) ) ;
#78931 = CARTESIAN_POINT ( 'NONE',  ( 27.81076257310190769, 39.55466486950702176, 7.012934429366973338E-14 ) ) ;
#78932 = ADVANCED_FACE ( 'NONE', ( #75609 ), #29497, .T. ) ;
#78933 = CARTESIAN_POINT ( 'NONE',  ( 42.04265951369687571, 185.8923013555410080, 4.594050593750050204 ) ) ;
#78934 = CIRCLE ( 'NONE', #35232, 70.00000000000001421 ) ;
#78935 = CARTESIAN_POINT ( 'NONE',  ( 77.05176924353446566, 63.79896054814203410, -15.33469885150045542 ) ) ;
#78936 = CARTESIAN_POINT ( 'NONE',  ( 66.56148311469628709, 218.4244531367911293, -4.594050593750046652 ) ) ;
#78937 = CARTESIAN_POINT ( 'NONE',  ( 164.2137379661740795, 246.9428399464227937, -5.807035987355257944 ) ) ;
#78938 = CARTESIAN_POINT ( 'NONE',  ( 88.48828274770076519, 43.87397573844135934, -0.5490789642627272871 ) ) ;
#78939 = EDGE_CURVE ( 'NONE', #72976, #59430, #99908, .T. ) ;
#78940 = CARTESIAN_POINT ( 'NONE',  ( 166.6394175675808356, 259.6070987380002180, 15.76739866228208165 ) ) ;
#78942 = DIRECTION ( 'NONE',  ( -0.000000000000000000, 1.000000000000000000, -0.000000000000000000 ) ) ;
#78941 = CYLINDRICAL_SURFACE ( 'NONE', #82464, 17.82106496071139645 ) ;
#78943 = CARTESIAN_POINT ( 'NONE',  ( 175.3932935011599170, 269.2958584618301643, -17.65833184418574930 ) ) ;
#78944 = EDGE_CURVE ( 'NONE', #16883, #57886, #95502, .T. ) ;
#78945 = CARTESIAN_POINT ( 'NONE',  ( 31.05045217176252237, 26.43085787977764767, -9.188101187500008038 ) ) ;
#78946 = CARTESIAN_POINT ( 'NONE',  ( 198.4344074287054696, 286.9485196940960918, -17.83642855442570152 ) ) ;
#78947 = CARTESIAN_POINT ( 'NONE',  ( 196.7491951525289835, 289.8673929779723721, -16.35352603081977207 ) ) ;
#78948 = VERTEX_POINT ( 'NONE', #30986 ) ;
#78949 = CARTESIAN_POINT ( 'NONE',  ( 13.12254358208367400, 30.68290643055187061, 3.479690158560446702E-15 ) ) ;
#78950 = CARTESIAN_POINT ( 'NONE',  ( 63.63864737692379236, 216.7369531367911293, -4.594050593750048428 ) ) ;
#78951 = DIRECTION ( 'NONE',  ( -0.8452030915256549815, -0.5344452582589497291, 0.000000000000000000 ) ) ;
#78952 = CARTESIAN_POINT ( 'NONE',  ( 155.4810912439522212, 261.3458456796594760, -18.44218279064527266 ) ) ;
#78953 = CARTESIAN_POINT ( 'NONE',  ( 198.6012358295098750, 286.6595644277572887, 18.21911298807435386 ) ) ;
#78954 = CARTESIAN_POINT ( 'NONE',  ( -19.65312891409030271, 93.06504152958497400, 10.00000000000000888 ) ) ;
#78955 = CARTESIAN_POINT ( 'NONE',  ( 201.8747764691672728, 280.9896257192293660, 16.31383242165743042 ) ) ;
#78956 = EDGE_CURVE ( 'NONE', #74106, #87650, #46686, .T. ) ;
#78957 = FACE_OUTER_BOUND ( 'NONE', #13435, .T. ) ;
#78958 = CARTESIAN_POINT ( 'NONE',  ( 87.47063030522556915, 45.04046199688875163, -6.105227862096588964 ) ) ;
#78959 = CARTESIAN_POINT ( 'NONE',  ( 123.9359264390130591, 242.3615022471902591, -10.00000000000009592 ) ) ;
#78960 = CARTESIAN_POINT ( 'NONE',  ( -13.11024591527734628, 27.99999999999999645, 32.50000000000000000 ) ) ;
#78961 = CARTESIAN_POINT ( 'NONE',  ( 207.6900289502458179, 270.9173129631602706, 7.178327969100043227 ) ) ;
#78962 = EDGE_LOOP ( 'NONE', ( #83233, #85307, #50500, #48927 ) ) ;
#78963 = CARTESIAN_POINT ( 'NONE',  ( 77.55626133878480744, 49.73613333205595666, 14.95107568548285215 ) ) ;
#78964 = AXIS2_PLACEMENT_3D ( 'NONE', #78054, #71957, #94280 ) ;
#78965 = CARTESIAN_POINT ( 'NONE',  ( 188.1911093852794465, 273.3801814407030406, 15.63271712328260676 ) ) ;
#78966 = VERTEX_POINT ( 'NONE', #61382 ) ;
#78967 = CARTESIAN_POINT ( 'NONE',  ( 206.1408608592916494, 273.6005508061571732, -10.42739367433323494 ) ) ;
#78968 = CARTESIAN_POINT ( 'NONE',  ( 153.3999530563582425, 279.9403317724381282, -0.6565603302638768346 ) ) ;
#78969 = CARTESIAN_POINT ( 'NONE',  ( 71.29390400445934972, 68.89192637807246911, -8.686554677171336891 ) ) ;
#78970 = ORIENTED_EDGE ( 'NONE', *, *, #86343, .F. ) ;
#78971 = FACE_OUTER_BOUND ( 'NONE', #18042, .T. ) ;
#78972 = VERTEX_POINT ( 'NONE', #92336 ) ;
#78973 = CARTESIAN_POINT ( 'NONE',  ( 65.83400234654939709, 68.92279781603272681, -2.474918377774905753 ) ) ;
#78974 = CARTESIAN_POINT ( 'NONE',  ( 40.29776668260214478, 205.6199935810941213, 2.679491924311251605 ) ) ;
#78975 = CARTESIAN_POINT ( 'NONE',  ( 148.7030012686772977, 273.8011336086232177, 8.646799806445988779 ) ) ;
#78976 = CIRCLE ( 'NONE', #14220, 0.1418229129684228651 ) ;
#78977 = VERTEX_POINT ( 'NONE', #22884 ) ;
#78978 = AXIS2_PLACEMENT_3D ( 'NONE', #28598, #19544, #50405 ) ;
#78979 = CARTESIAN_POINT ( 'NONE',  ( 25.14222138719033595, 29.91421378149919619, 9.188101187500008038 ) ) ;
#78980 = CARTESIAN_POINT ( 'NONE',  ( 74.93795995569031732, 66.37748476621555938, -13.08215655857838655 ) ) ;
#78981 = CARTESIAN_POINT ( 'NONE',  ( 80.44963597398161426, 49.01439875558640580, -13.96582802915731492 ) ) ;
#78982 = ORIENTED_EDGE ( 'NONE', *, *, #59685, .F. ) ;
#78983 = DIRECTION ( 'NONE',  ( 0.000000000000000000, 0.000000000000000000, -1.000000000000000000 ) ) ;
#78984 = CARTESIAN_POINT ( 'NONE',  ( 206.6703863510205679, 272.6833857505801006, -10.72500664779635393 ) ) ;
#78985 = ORIENTED_EDGE ( 'NONE', *, *, #41701, .F. ) ;
#78986 = ORIENTED_EDGE ( 'NONE', *, *, #75842, .F. ) ;
#78987 = CARTESIAN_POINT ( 'NONE',  ( 186.2526055351975174, 298.2835612753726764, 1.053363499427862449 ) ) ;
#78988 = AXIS2_PLACEMENT_3D ( 'NONE', #2930, #80955, #64707 ) ;
#78990 = CARTESIAN_POINT ( 'NONE',  ( 194.2223991963907963, 294.2439319543634610, -14.97294938100067441 ) ) ;
#78989 = CARTESIAN_POINT ( 'NONE',  ( 67.65051319695646725, 65.91095239435391306, 10.45228776382301383 ) ) ;
#78991 = DIRECTION ( 'NONE',  ( 0.000000000000000000, 0.000000000000000000, 1.000000000000000000 ) ) ;
#78992 = CARTESIAN_POINT ( 'NONE',  ( 185.4350764609872897, 292.4497694977334845, -11.01741108579075856 ) ) ;
#78993 = CARTESIAN_POINT ( 'NONE',  ( 204.6713671561005299, 276.1457885614869951, -12.94307097876490431 ) ) ;
#78994 = CARTESIAN_POINT ( 'NONE',  ( 145.9657079678295020, 245.8923013555409511, 4.594050593750050204 ) ) ;
#78995 = CARTESIAN_POINT ( 'NONE',  ( 46.50192534792603283, 74.36443251879779837, -10.00000000000000000 ) ) ;
#78996 = VECTOR ( 'NONE', #1229, 1000.000000000000114 ) ;
#78997 = CARTESIAN_POINT ( 'NONE',  ( 149.8050492866161392, 271.5723974896224604, -11.69608657949948061 ) ) ;
#78998 = CARTESIAN_POINT ( 'NONE',  ( 85.37073267496330686, 220.0958772461660544, -9.188101187500095079 ) ) ;
#78999 = ORIENTED_EDGE ( 'NONE', *, *, #53625, .T. ) ;
#79000 = CARTESIAN_POINT ( 'NONE',  ( 150.7226148805041817, 269.5877685077668957, 15.52819754351937576 ) ) ;
#79001 = DIRECTION ( 'NONE',  ( 0.02225111142181396273, 0.9997524133706774396, 0.000000000000000000 ) ) ;
#79002 = ORIENTED_EDGE ( 'NONE', *, *, #35552, .T. ) ;
#79003 = CARTESIAN_POINT ( 'NONE',  ( 195.3220404309544449, 292.3392974660017103, -16.60012830897328229 ) ) ;
#79004 = ORIENTED_EDGE ( 'NONE', *, *, #67209, .F. ) ;
#79005 = ORIENTED_EDGE ( 'NONE', *, *, #5707, .F. ) ;
#79006 = CARTESIAN_POINT ( 'NONE',  ( 80.31904029099077036, 44.94024336421264820, -11.21917720938367324 ) ) ;
#79007 = FACE_OUTER_BOUND ( 'NONE', #53654, .T. ) ;
#79008 = CARTESIAN_POINT ( 'NONE',  ( 146.5865263025993954, 276.7516840693029962, 0.4918294119671828835 ) ) ;
#79009 = CARTESIAN_POINT ( 'NONE',  ( 164.1514498073476034, 249.9675132558865016, 10.20859178390983324 ) ) ;
#79010 = CARTESIAN_POINT ( 'NONE',  ( 83.79842386373591978, 47.52858511108933470, -11.83496612566354855 ) ) ;
#79011 = CARTESIAN_POINT ( 'NONE',  ( 162.5705829494080490, 249.0664858459717550, 10.39261705965051341 ) ) ;
#79012 = CARTESIAN_POINT ( 'NONE',  ( 83.61187889534991768, 209.8923013555409796, 4.594050593750050204 ) ) ;
#79013 = ORIENTED_EDGE ( 'NONE', *, *, #24549, .T. ) ;
#79014 = VERTEX_POINT ( 'NONE', #80139 ) ;
#79015 = CARTESIAN_POINT ( 'NONE',  ( 161.2503778443652607, 251.3531481643174743, -13.44633621139661095 ) ) ;
#79016 = ORIENTED_EDGE ( 'NONE', *, *, #53442, .F. ) ;
#79018 = ADVANCED_FACE ( 'NONE', ( #54781 ), #56278, .T. ) ;
#79017 = B_SPLINE_CURVE_WITH_KNOTS ( 'NONE', 3,
 ( #52946, #46321, #85393, #91484, #30145, #7338, #37246, #53921, #30654, #36745, #67653, #13959, #84884, #77247, #7853, #44839, #45341, #75276, #61538, #45823, #76272, #61030, #52446, #44345, #98584, #38735, #69639, #6846, #247, #31128, #62021, #37731, #60035, #22550, #53435, #5860, #29167, #23527, #54417, #84386, #14932, #92481, #54938, #71675, #55419, #64047, #85915, #93484 ),
 .UNSPECIFIED., .F., .F.,
 ( 4, 2, 2, 2, 2, 2, 2, 2, 2, 2, 2, 2, 2, 2, 2, 2, 2, 2, 2, 2, 2, 2, 2, 4 ),
 ( 0.001794995322932195925, 0.002245303848294032383, 0.002695612373655869275, 0.002808189504996264421, 0.002920766636336659568, 0.003033343767677054714, 0.003145920899017449427, 0.003371075161698240154, 0.003596229424379030447, 0.004046537949740726392, 0.004496846475102421470, 0.005397463525825844585, 0.006298080576549267701, 0.006748389101911021759, 0.007198697627272777552, 0.007311274758613178770, 0.007367563324283427084, 0.007423851889953675398, 0.007536429021294069677, 0.007649006152634463956, 0.008099314677995971684, 0.008549623203357479412, 0.008774777466038235010, 0.008999931728718987139 ),
 .UNSPECIFIED. ) ;
#79019 = CARTESIAN_POINT ( 'NONE',  ( 76.21739704791244208, 64.80718227787073715, -14.34818600867717464 ) ) ;
#79020 = CARTESIAN_POINT ( 'NONE',  ( 164.9191543487298190, 285.0012716261463197, 0.5041077705605265802 ) ) ;
#79021 = CARTESIAN_POINT ( 'NONE',  ( 104.4503548538631890, 231.1115022471902307, 10.00000000000009592 ) ) ;
#79022 = DIRECTION ( 'NONE',  ( -0.6303371332823575202, -0.7763215174174804556, 0.000000000000000000 ) ) ;
#79023 = EDGE_LOOP ( 'NONE', ( #98907, #27050, #19163, #27633 ) ) ;
#79024 = CARTESIAN_POINT ( 'NONE',  ( 191.7321250286022121, 296.2108873932954225, 11.25078612220933927 ) ) ;
#79025 = CARTESIAN_POINT ( 'NONE',  ( 80.73870607681467959, 45.87205857520788044, 11.81702607854560050 ) ) ;
#79026 = CARTESIAN_POINT ( 'NONE',  ( 206.1615484827472358, 273.5647187912443314, -9.556459874778100883 ) ) ;
#79027 = CARTESIAN_POINT ( 'NONE',  ( 148.0706186424908140, 275.6441064196449702, -5.227547594756374316 ) ) ;
#79029 = EDGE_CURVE ( 'NONE', #43553, #98181, #89038, .T. ) ;
#79028 = CARTESIAN_POINT ( 'NONE',  ( 175.0425229888917045, 283.7493962866749939, 13.34536946309205341 ) ) ;
#79030 = DIRECTION ( 'NONE',  ( 0.4999999999999992784, -0.8660254037844390407, 0.000000000000000000 ) ) ;
#79031 = ADVANCED_FACE ( 'NONE', ( #25390 ), #47183, .T. ) ;
#79032 = CARTESIAN_POINT ( 'NONE',  ( 195.4920518568790158, 279.6224761531880176, -17.31986585614815866 ) ) ;
#79033 = ORIENTED_EDGE ( 'NONE', *, *, #41012, .F. ) ;
#79034 = CYLINDRICAL_SURFACE ( 'NONE', #2528, 70.00000000000002842 ) ;
#79035 = CARTESIAN_POINT ( 'NONE',  ( 161.8016137473484548, 250.3983795733946636, 14.25000412375400316 ) ) ;
#79036 = DIRECTION ( 'NONE',  ( -0.5000000000000016653, 0.8660254037844375974, 0.000000000000000000 ) ) ;
#79037 = AXIS2_PLACEMENT_3D ( 'NONE', #41880, #19614, #11997 ) ;
#79038 = CARTESIAN_POINT ( 'NONE',  ( 187.9510599096114163, 266.1630128281000793, -12.95057174692511204 ) ) ;
#79039 = CARTESIAN_POINT ( 'NONE',  ( 77.88662807442577218, 62.02336507127854759, 15.65480789639172876 ) ) ;
#79040 = CARTESIAN_POINT ( 'NONE',  ( 177.5604642151115513, 291.0442495137150445, -6.142901185704334743 ) ) ;
#79041 = CARTESIAN_POINT ( 'NONE',  ( 155.1439221426048505, 271.2780826592891685, 14.03075285333380862 ) ) ;
#79042 = VERTEX_POINT ( 'NONE', #87276 ) ;
#79043 = AXIS2_PLACEMENT_3D ( 'NONE', #3082, #74473, #87725 ) ;
#79044 = CIRCLE ( 'NONE', #17545, 70.00000000000001421 ) ;
#79045 = AXIS2_PLACEMENT_3D ( 'NONE', #16307, #24411, #86267 ) ;
#79046 = CARTESIAN_POINT ( 'NONE',  ( 72.63029380029557558, 64.40628814066955954, -13.38103629891480217 ) ) ;
#79048 = CARTESIAN_POINT ( 'NONE',  ( 73.94500316957324060, 55.09575893527664192, 16.60253717196292200 ) ) ;
#79047 = CARTESIAN_POINT ( 'NONE',  ( 180.7542070542261854, 266.7828525480385338, -16.22133153096915947 ) ) ;
#79049 = CARTESIAN_POINT ( 'NONE',  ( 199.4856116213349537, 281.2262712591287936, -16.83883655570358684 ) ) ;
#79050 = CARTESIAN_POINT ( 'NONE',  ( 28.39959312520600676, 35.13478043621390157, 8.090169943749478065 ) ) ;
#79051 = CARTESIAN_POINT ( 'NONE',  ( 99.82359446507273049, 216.8932355074535394, -2.679491924311248496 ) ) ;
#79052 = CARTESIAN_POINT ( 'NONE',  ( 168.8894219329319242, 272.9552995970117308, 15.96619431876584017 ) ) ;
#79053 = CARTESIAN_POINT ( 'NONE',  ( 180.4080136573045365, 272.9691542711491365, 17.06805577271178365 ) ) ;
#79054 = DIRECTION ( 'NONE',  ( 0.000000000000000000, 0.000000000000000000, 1.000000000000000000 ) ) ;
#79055 = B_SPLINE_CURVE_WITH_KNOTS ( 'NONE', 3,
 ( #11706, #27398, #96833, #34975, #89255, #74002 ),
 .UNSPECIFIED., .F., .F.,
 ( 4, 2, 4 ),
 ( 0.02234597899312508462, 0.02694808822545060809, 0.03155019745777613155 ),
 .UNSPECIFIED. ) ;
#79056 = CARTESIAN_POINT ( 'NONE',  ( 205.9449877905329345, 273.5527750745989692, -9.681680776101762476 ) ) ;
#79057 = CARTESIAN_POINT ( 'NONE',  ( 207.8575108622103755, 270.6272257822888037, -6.381720258959569847 ) ) ;
#79058 = VECTOR ( 'NONE', #8779, 1000.000000000000114 ) ;
#79059 = EDGE_CURVE ( 'NONE', #24573, #94007, #49206, .T. ) ;
#79060 = CARTESIAN_POINT ( 'NONE',  ( -1.340060878953613477, 170.0333772461660828, 9.188101187500095079 ) ) ;
#79061 = CARTESIAN_POINT ( 'NONE',  ( 82.93874205646059750, 50.87638965249802681, 14.26819964912884231 ) ) ;
#79062 = VERTEX_POINT ( 'NONE', #32986 ) ;
#79063 = CARTESIAN_POINT ( 'NONE',  ( 178.7466306158354712, 256.8873838365522602, 8.522590757080182655 ) ) ;
#79064 = EDGE_CURVE ( 'NONE', #74614, #77581, #88324, .T. ) ;
#79065 = CARTESIAN_POINT ( 'NONE',  ( 34.63914548426571116, 22.12755873383627758, -6.180339887498949025 ) ) ;
#79066 = CARTESIAN_POINT ( 'NONE',  ( 82.32963097709573219, 41.38348250535303663, 5.483832747226924376 ) ) ;
#79068 = CARTESIAN_POINT ( 'NONE',  ( 11.67712314985746858, 186.7369531367911293, -4.594050593750048428 ) ) ;
#79067 = B_SPLINE_CURVE_WITH_KNOTS ( 'NONE', 3,
 ( #43480, #59160, #36380, #83032 ),
 .UNSPECIFIED., .F., .F.,
 ( 4, 4 ),
 ( 0.009153972151010242309, 0.01742534041516074009 ),
 .UNSPECIFIED. ) ;
#79069 = CARTESIAN_POINT ( 'NONE',  ( 81.50343375784891009, 59.55623038343588149, -0.1545084971874786939 ) ) ;
#79070 = CARTESIAN_POINT ( 'NONE',  ( 35.05240415091495976, 28.43677371833803846, -10.00000000000000355 ) ) ;
#79071 = CARTESIAN_POINT ( 'NONE',  ( 178.7121136867105804, 291.7201401133655168, 6.070087115661351618 ) ) ;
#79072 = CARTESIAN_POINT ( 'NONE',  ( 105.8215617431885534, 225.2365022471902023, -10.00000000000009237 ) ) ;
#79073 = CARTESIAN_POINT ( 'NONE',  ( 148.9742902571590264, 272.6159555835243964, 12.12504745624938529 ) ) ;
#79074 = CARTESIAN_POINT ( 'NONE',  ( 152.7122812589697958, 277.9324518551267147, 6.933031942251369983 ) ) ;
#79075 = DIRECTION ( 'NONE',  ( -0.8660254037844387076, -0.4999999999999998890, -0.000000000000000000 ) ) ;
#79076 = B_SPLINE_SURFACE_WITH_KNOTS ( 'NONE', 3, 1, ( 
 ( #95541, #40259 ),
 ( #95025, #72202 ),
 ( #88442, #17477 ),
 ( #86439, #19002 ),
 ( #32674, #80322 ),
 ( #47856, #2807 ),
 ( #33695, #10390 ),
 ( #71199, #55454 ),
 ( #8874, #72715 ),
 ( #48386, #57462 ),
 ( #70671, #16966 ),
 ( #10892, #79823 ),
 ( #48889, #1286 ),
 ( #32170, #41768 ),
 ( #64080, #87949 ),
 ( #63574, #3304 ),
 ( #79330, #63074 ),
 ( #94017, #78795 ),
 ( #94518, #64588 ),
 ( #1792, #71706 ),
 ( #26088, #87463 ),
 ( #9898, #56963 ),
 ( #18493, #34184 ),
 ( #2299, #65077 ),
 ( #33181, #25587 ),
 ( #96027, #56474 ),
 ( #49877, #98492 ),
 ( #74201, #35167 ),
 ( #36157, #3789 ),
 ( #65572, #4269 ),
 ( #89910, #51361 ),
 ( #11407, #34670 ),
 ( #74699, #12899 ),
 ( #96519, #59442 ) ),
 .UNSPECIFIED., .T., .F., .F.,
 ( 4, 2, 2, 2, 2, 2, 2, 2, 2, 2, 2, 2, 2, 2, 2, 2, 4 ),
 ( 2, 2 ),
 ( 0.000000000000000000, 0.06250000000000000000, 0.1250000000000000000, 0.1875000000000000000, 0.2500000000000000000, 0.3125000000000000000, 0.3750000000000000000, 0.4375000000000000000, 0.5000000000000000000, 0.5625000000000000000, 0.6250000000000000000, 0.6875000000000000000, 0.7500000000000000000, 0.8125000000000000000, 0.8750000000000000000, 0.9375000000000000000, 1.000000000000000000 ),
 ( 0.000000000000000000, 1.000000000000000000 ),
 .UNSPECIFIED. ) ;
#79077 = EDGE_CURVE ( 'NONE', #52870, #54113, #8694, .T. ) ;
#79078 = CARTESIAN_POINT ( 'NONE',  ( 190.1127736092558962, 298.7324422743296850, -8.109491230568453446 ) ) ;
#79079 = CARTESIAN_POINT ( 'NONE',  ( 83.82185059330514321, 51.95230014857059331, 14.93193377595571825 ) ) ;
#79080 = CARTESIAN_POINT ( 'NONE',  ( 193.0124118986755093, 295.6209498147566137, -12.68620708360851701 ) ) ;
#79081 = CARTESIAN_POINT ( 'NONE',  ( 68.51030059680894624, 220.3615022471903160, 5.000000000000046185 ) ) ;
#79082 = CARTESIAN_POINT ( 'NONE',  ( 203.7690284654797210, 275.7086850192775955, -13.99192714286714612 ) ) ;
#79083 = CARTESIAN_POINT ( 'NONE',  ( 164.4706844205170171, 281.1311524026570510, 11.86625682173560925 ) ) ;
#79084 = CARTESIAN_POINT ( 'NONE',  ( 92.93017357788669131, 158.0650415295850735, 36.50000000000000000 ) ) ;
#79085 = CARTESIAN_POINT ( 'NONE',  ( 30.64892602121659593, 182.3768266524159856, -9.188101187500091527 ) ) ;
#79086 = CARTESIAN_POINT ( 'NONE',  ( 197.9952413503812352, 287.7091776547143809, 17.17611241386010690 ) ) ;
#79087 = CARTESIAN_POINT ( 'NONE',  ( 64.90981964964726103, 219.8297689869269504, -2.679491924311252493 ) ) ;
#79088 = CYLINDRICAL_SURFACE ( 'NONE', #36855, 70.00000000000002842 ) ;
#79089 = CARTESIAN_POINT ( 'NONE',  ( 67.13884004924136661, 66.79719628306519041, -9.043772424411733013 ) ) ;
#79090 = ORIENTED_EDGE ( 'NONE', *, *, #23090, .F. ) ;
#79091 = FACE_OUTER_BOUND ( 'NONE', #59984, .T. ) ;
#79092 = CARTESIAN_POINT ( 'NONE',  ( 69.12672858200174630, 64.33651235087042153, -11.97836756590942997 ) ) ;
#79093 = DIRECTION ( 'NONE',  ( -0.000000000000000000, -0.000000000000000000, -1.000000000000000000 ) ) ;
#79094 = CARTESIAN_POINT ( 'NONE',  ( 23.56475526289127842, 35.64646525600391413, -2.839279412974133887 ) ) ;
#79095 = CARTESIAN_POINT ( 'NONE',  ( 202.4323889586180201, 280.0238125565655878, 15.69595176008160919 ) ) ;
#79096 = CARTESIAN_POINT ( 'NONE',  ( 196.5114383562724072, 290.2791998289336561, -17.87308875047256862 ) ) ;
#79097 = CARTESIAN_POINT ( 'NONE',  ( 185.5448903953628985, 267.7045173717977491, -14.56276892697053071 ) ) ;
#79098 = ORIENTED_EDGE ( 'NONE', *, *, #84522, .F. ) ;
#79099 = CARTESIAN_POINT ( 'NONE',  ( 6.007877864960585512, 21.65586893147753855, -7.433330006724137462 ) ) ;
#79100 = CARTESIAN_POINT ( 'NONE',  ( 189.7094295309238419, 300.0606247079692253, 5.078421157105148076 ) ) ;
#79101 = CARTESIAN_POINT ( 'NONE',  ( 77.22652224754085637, 58.45676704727122797, -16.12585536898887284 ) ) ;
#79102 = DIRECTION ( 'NONE',  ( -0.009162850352621045372, 0.9999580202055561307, 0.000000000000000000 ) ) ;
#79103 = ORIENTED_EDGE ( 'NONE', *, *, #85291, .T. ) ;
#79104 = CARTESIAN_POINT ( 'NONE',  ( 31.70422093597037616, 179.1115022471902023, -5.000000000000041744 ) ) ;
#79105 = CARTESIAN_POINT ( 'NONE',  ( 72.48187990437281769, 71.22453042848766813, -6.074313086633869929 ) ) ;
#79106 = DIRECTION ( 'NONE',  ( 0.5000000000000014433, -0.8660254037844378194, 0.000000000000000000 ) ) ;
#79107 = CARTESIAN_POINT ( 'NONE',  ( 35.43817338645654758, 49.87999306568067226, 177.5919119679930134 ) ) ;
#79108 = CARTESIAN_POINT ( 'NONE',  ( 149.2511585606875428, 272.1364056148075292, 11.40684181024752242 ) ) ;
#79109 = ADVANCED_FACE ( 'NONE', ( #62883 ), #44126, .F. ) ;
#79110 = ORIENTED_EDGE ( 'NONE', *, *, #15583, .T. ) ;
#79111 = VERTEX_POINT ( 'NONE', #74514 ) ;
#79112 = B_SPLINE_CURVE_WITH_KNOTS ( 'NONE', 3,
 ( #4406, #28705, #97153, #74833, #81944, #82948, #73812, #51500, #82469, #28199, #27719, #58587 ),
 .UNSPECIFIED., .F., .F.,
 ( 4, 2, 2, 2, 2, 4 ),
 ( 7.844548453170152250E-15, 0.0004651973059127275886, 0.0009303946118176106492, 0.001395591917722493547, 0.001628190570674949416, 0.001860789223627405285 ),
 .UNSPECIFIED. ) ;
#79114 = CARTESIAN_POINT ( 'NONE',  ( 82.48583416037470784, 42.33184412569765698, -6.146425681634053895 ) ) ;
#79113 = CARTESIAN_POINT ( 'NONE',  ( 161.8926315922002743, 250.2407320417157166, -13.77020595223768495 ) ) ;
#79115 = ORIENTED_EDGE ( 'NONE', *, *, #65948, .T. ) ;
#79116 = CARTESIAN_POINT ( 'NONE',  ( 38.46077748372667315, 37.90829794293884447, 10.00000000000000355 ) ) ;
#79117 = VECTOR ( 'NONE', #54414, 1000.000000000000114 ) ;
#79118 = DIRECTION ( 'NONE',  ( 0.000000000000000000, 1.000000000000000000, 0.000000000000000000 ) ) ;
#79119 = CARTESIAN_POINT ( 'NONE',  ( 72.70720764797087554, 57.09321477475226914, -15.89700010401374364 ) ) ;
#79120 = CARTESIAN_POINT ( 'NONE',  ( 110.0000000000000142, 10.00000000000004086, 59.99999999999999289 ) ) ;
#79121 = ADVANCED_FACE ( 'NONE', ( #73502 ), #28377, .F. ) ;
#79122 = CARTESIAN_POINT ( 'NONE',  ( 204.9184781223158609, 275.7177798128946620, -12.59106622113254126 ) ) ;
#79123 = CARTESIAN_POINT ( 'NONE',  ( 108.9159718882352479, 227.5643266524159856, -9.188101187500093303 ) ) ;
#79124 = VECTOR ( 'NONE', #62290, 1000.000000000000000 ) ;
#79125 = VECTOR ( 'NONE', #46063, 999.9999999999998863 ) ;
#79126 = CARTESIAN_POINT ( 'NONE',  ( 184.1487307564388516, 288.9301599317471982, -13.09092302844920575 ) ) ;
#79127 = ORIENTED_EDGE ( 'NONE', *, *, #62646, .F. ) ;
#79128 = AXIS2_PLACEMENT_3D ( 'NONE', #77595, #76583, #16769 ) ;
#79129 = CARTESIAN_POINT ( 'NONE',  ( 161.8762453271136224, 267.0714273172965818, 16.50803258978729460 ) ) ;
#79130 = ORIENTED_EDGE ( 'NONE', *, *, #24972, .T. ) ;
#79131 = CARTESIAN_POINT ( 'NONE',  ( 34.90123498099573851, 22.01110640527294393, 2.839279412974134775 ) ) ;
#79132 = DIRECTION ( 'NONE',  ( 0.4999999999999998890, -0.8660254037844385966, 0.000000000000000000 ) ) ;
#79133 = CARTESIAN_POINT ( 'NONE',  ( 78.30023004233427741, 47.96220519360661427, -14.02684811912188323 ) ) ;
#79134 = CARTESIAN_POINT ( 'NONE',  ( 58.06412948370898164, 195.1423013555410080, -4.594050593750043987 ) ) ;
#79135 = ORIENTED_EDGE ( 'NONE', *, *, #44335, .F. ) ;
#79136 = CARTESIAN_POINT ( 'NONE',  ( 73.81469611240122219, 68.48838210847161179, 11.42215486908103728 ) ) ;
#79137 = CARTESIAN_POINT ( 'NONE',  ( 191.4044787581200069, 299.1247133251352466, 7.435199718141230818 ) ) ;
#79138 = CARTESIAN_POINT ( 'NONE',  ( 197.9812996484125449, 287.7333253908681741, 17.50297787674340455 ) ) ;
#79139 = CARTESIAN_POINT ( 'NONE',  ( 172.9576090935003094, 271.2785582124699886, 16.43141609699088335 ) ) ;
#79140 = ORIENTED_EDGE ( 'NONE', *, *, #13796, .T. ) ;
#79141 = AXIS2_PLACEMENT_3D ( 'NONE', #79120, #16272, #23361 ) ;
#79142 = CARTESIAN_POINT ( 'NONE',  ( 74.14148900092213523, 58.70489250135918979, -15.78255431708223888 ) ) ;
#79143 = CARTESIAN_POINT ( 'NONE',  ( 177.7824965871422762, 288.9732240448931293, 11.16390339965338541 ) ) ;
#79144 = LINE ( 'NONE', #72013, #57737 ) ;
#79145 = VERTEX_POINT ( 'NONE', #19326 ) ;
#79146 = CARTESIAN_POINT ( 'NONE',  ( -110.0000000000000284, 0.000000000000000000, 9.212605237762149457 ) ) ;
#79147 = CARTESIAN_POINT ( 'NONE',  ( 71.27247878601987452, 69.85383392380222745, -7.214268055942345548 ) ) ;
#79148 = CARTESIAN_POINT ( 'NONE',  ( 207.2707369601997982, 271.6435479931266173, -5.381413637561199614 ) ) ;
#79149 = CARTESIAN_POINT ( 'NONE',  ( 147.2089949622447875, 275.6735367246781720, -3.633014386235353221 ) ) ;
#79150 = EDGE_CURVE ( 'NONE', #57256, #74347, #26403, .T. ) ;
#79151 = CARTESIAN_POINT ( 'NONE',  ( 149.7128599965862463, 271.3367152699035501, 12.33532264622322394 ) ) ;
#79152 = CARTESIAN_POINT ( 'NONE',  ( 180.8104799410488681, 271.3708678522607443, 16.68610488619162524 ) ) ;
#79153 = VECTOR ( 'NONE', #33947, 1000.000000000000227 ) ;
#79154 = CARTESIAN_POINT ( 'NONE',  ( 205.8918578537579833, 274.0318366629789466, 11.52627491423194250 ) ) ;
#79155 = CARTESIAN_POINT ( 'NONE',  ( 67.31665553791867751, 66.91278932699420068, 9.026460761065990823 ) ) ;
#79156 = CARTESIAN_POINT ( 'NONE',  ( 75.09035324708760584, 64.38728148916531779, -14.18083448766436128 ) ) ;
#79157 = CARTESIAN_POINT ( 'NONE',  ( -19.65312891409030271, 93.06504152958497400, 10.00000000000000888 ) ) ;
#79158 = CARTESIAN_POINT ( 'NONE',  ( 108.5637151982415389, 242.6744531367911293, 4.594050593750047540 ) ) ;
#79159 = ORIENTED_EDGE ( 'NONE', *, *, #39427, .F. ) ;
#79160 = CARTESIAN_POINT ( 'NONE',  ( 148.9665168016069288, 272.6294196034908737, -12.32906446557564806 ) ) ;
#79161 = LINE ( 'NONE', #48216, #49750 ) ;
#79162 = DIRECTION ( 'NONE',  ( 0.5011331959107180323, 0.8653701635463924013, 0.000000000000000000 ) ) ;
#79163 = EDGE_CURVE ( 'NONE', #90523, #72718, #65881, .T. ) ;
#79164 = CARTESIAN_POINT ( 'NONE',  ( 183.2770270516915900, 284.7653891124718939, -14.95557695974454937 ) ) ;
#79165 = EDGE_CURVE ( 'NONE', #99984, #49104, #20628, .T. ) ;
#79166 = CARTESIAN_POINT ( 'NONE',  ( 83.75130605492059033, 51.70531176359354220, -14.84358514963803977 ) ) ;
#79167 = PLANE ( 'NONE',  #14659 ) ;
#79168 = ORIENTED_EDGE ( 'NONE', *, *, #44925, .F. ) ;
#79169 = CARTESIAN_POINT ( 'NONE',  ( 80.38256674825400694, 58.04436476229781761, -16.60504034864360179 ) ) ;
#79170 = CARTESIAN_POINT ( 'NONE',  ( 158.3104460577808368, 274.8641074767056693, -12.54398958924856267 ) ) ;
#79171 = CARTESIAN_POINT ( 'NONE',  ( -110.0000000000000000, 0.000000000000000000, -59.99999999999999289 ) ) ;
#79172 = CARTESIAN_POINT ( 'NONE',  ( 78.30955769916531040, 61.43963167811126169, 15.82323565659766373 ) ) ;
#79173 = CARTESIAN_POINT ( 'NONE',  ( 131.9738982639959488, 240.8768266524159856, -9.188101187500093303 ) ) ;
#79174 = CARTESIAN_POINT ( 'NONE',  ( 191.1041001801271761, 295.0267033716904734, -12.18635420512492473 ) ) ;
#79175 = CARTESIAN_POINT ( 'NONE',  ( 185.9833676731276171, 296.7909978881492066, 4.657551602822923797 ) ) ;
#79176 = CARTESIAN_POINT ( 'NONE',  ( 81.74119788692269140, 59.14441083166271085, 0.000000000000000000 ) ) ;
#79177 = CARTESIAN_POINT ( 'NONE',  ( 45.37135788555205096, 190.8768266524159856, 9.188101187500098632 ) ) ;
#79178 = CARTESIAN_POINT ( 'NONE',  ( 85.57719226846251104, 48.31999287754577210, -11.71062333427767044 ) ) ;
#79179 = CARTESIAN_POINT ( 'NONE',  ( 205.3704330671644414, 274.9349708856848338, -13.01557521325596944 ) ) ;
#79180 = LINE ( 'NONE', #8737, #78768 ) ;
#79181 = FILL_AREA_STYLE ('',( #56323 ) ) ;
#79182 = CARTESIAN_POINT ( 'NONE',  ( 174.3107956278732900, 262.1115639708946219, 14.35749921995197909 ) ) ;
#79183 = CARTESIAN_POINT ( 'NONE',  ( 41.50249547274756878, 124.4848494355456836, -10.00000000000000000 ) ) ;
#79185 = CARTESIAN_POINT ( 'NONE',  ( 178.9474598655808109, 291.8225860576774267, -6.155819841034777973 ) ) ;
#79184 = B_SPLINE_CURVE_WITH_KNOTS ( 'NONE', 3,
 ( #74523, #79472, #87094, #11544, #42402, #88588, #33325, #19647, #3445, #96661, #73338, #2445, #25742, #4417, #27231, #80978, #19150, #3923, #34324, #10036, #26725, #56622, #65708, #57609, #58115, #66225, #73827, #35312, #34806, #87605, #65221 ),
 .UNSPECIFIED., .F., .F.,
 ( 4, 3, 3, 3, 3, 3, 3, 3, 3, 3, 4 ),
 ( 0.000000000000000000, 0.1333490885032306283, 0.3007194338854234927, 0.4699862290244963270, 0.5844252810809187348, 0.6686540514502645749, 0.7354980260655307189, 0.8028463152565288308, 0.8633854507756889562, 0.9437142632666959408, 1.000000000000000000 ),
 .UNSPECIFIED. ) ;
#79186 = CARTESIAN_POINT ( 'NONE',  ( 203.4682009197399566, 278.2297336128146412, -15.36039508894693206 ) ) ;
#79187 = CARTESIAN_POINT ( 'NONE',  ( 157.0611216476779077, 270.7214317481134458, -14.74200130514388007 ) ) ;
#79188 = ADVANCED_FACE ( 'NONE', ( #57778 ), #47468, .F. ) ;
#79189 = CARTESIAN_POINT ( 'NONE',  ( 123.7735466722555771, 232.2677522451417929, -5.000000000000041744 ) ) ;
#79190 = VECTOR ( 'NONE', #12682, 1000.000000000000000 ) ;
#79191 = CARTESIAN_POINT ( 'NONE',  ( 75.58055549604159751, 53.46810915028748212, -16.02836618447256001 ) ) ;
#79192 = VERTEX_POINT ( 'NONE', #6591 ) ;
#79193 = EDGE_CURVE ( 'NONE', #98946, #53182, #37464, .T. ) ;
#79194 = AXIS2_PLACEMENT_3D ( 'NONE', #40182, #76708, #84845 ) ;
#79195 = CARTESIAN_POINT ( 'NONE',  ( 163.2919429874875448, 247.8170536094679903, 9.876785378511263147 ) ) ;
#79196 = CARTESIAN_POINT ( 'NONE',  ( 87.53662896702414287, 44.58992679936064008, 4.926115213305346074 ) ) ;
#79197 = CARTESIAN_POINT ( 'NONE',  ( 26.96797095936772237, 192.5024278399160949, 9.188101187500095079 ) ) ;
#79198 = AXIS2_PLACEMENT_3D ( 'NONE', #12837, #87015, #2367 ) ;
#79199 = CARTESIAN_POINT ( 'NONE',  ( 11.78502771447809394, 29.73705186507753240, -3.090169943749475845 ) ) ;
#79200 = CARTESIAN_POINT ( 'NONE',  ( 44.44706364856357084, 64.93738052781135650, 10.00000000000000000 ) ) ;
#79201 = CARTESIAN_POINT ( 'NONE',  ( 190.2510882691990730, 301.1224442529128851, -5.480893437181090455 ) ) ;
#79202 = CARTESIAN_POINT ( 'NONE',  ( 72.00170078070283353, 72.01756085178577393, 2.840212697767991568 ) ) ;
#79204 = CARTESIAN_POINT ( 'NONE',  ( 56.22356517706928969, 213.2677522451419350, -5.000000000000047962 ) ) ;
#79203 = CARTESIAN_POINT ( 'NONE',  ( 84.06604358195920668, 51.46910565605918464, 14.65639964578790533 ) ) ;
#79205 = CARTESIAN_POINT ( 'NONE',  ( 174.5414916011210664, 289.0348056237772312, 7.720355924734928266 ) ) ;
#79206 = CARTESIAN_POINT ( 'NONE',  ( 184.5160214038196500, 257.1200641698031859, 1.403992015128312287 ) ) ;
#79207 = CARTESIAN_POINT ( 'NONE',  ( 6.292850856353352285, 162.8932355074535678, -2.679491924311248496 ) ) ;
#79208 = LINE ( 'NONE', #33058, #95411 ) ;
#79209 = ORIENTED_EDGE ( 'NONE', *, *, #66448, .F. ) ;
#79210 =( BOUNDED_CURVE ( )  B_SPLINE_CURVE ( 2, ( #17589, #76881, #86058, #7477, #8492, #47969, #23175, #93115, #31766 ),
 .UNSPECIFIED., .F., .T. ) 
 B_SPLINE_CURVE_WITH_KNOTS ( ( 3, 2, 2, 2, 3 ),
 ( 0.2782258064516128782, 0.2795698924731182533, 0.2822580645161290591, 0.2849462365591398094, 0.2862903225806451846 ),
 .UNSPECIFIED. ) 
 CURVE ( )  GEOMETRIC_REPRESENTATION_ITEM ( )  RATIONAL_B_SPLINE_CURVE ( ( 0.9330127018922194093, 0.9330127018922194093, 1.000000000000000000, 0.8660254037844387076, 1.000000000000000000, 0.8660254037844387076, 1.000000000000000000, 0.9330127018922194093, 0.9330127018922194093 ) ) 
 REPRESENTATION_ITEM ( '' )  );
#79211 = CARTESIAN_POINT ( 'NONE',  ( 161.8434637317903935, 267.2159794866400944, 16.48508094337421070 ) ) ;
#79212 = CARTESIAN_POINT ( 'NONE',  ( 31.70422093597037616, 179.1115022471902023, -5.000000000000041744 ) ) ;
#79213 = DIRECTION ( 'NONE',  ( 0.2503889871761765251, 0.9681453171404014180, 0.000000000000000000 ) ) ;
#79214 = CARTESIAN_POINT ( 'NONE',  ( 208.3135187673106543, 269.8373969220020285, 2.829653198597726682 ) ) ;
#79215 = CARTESIAN_POINT ( 'NONE',  ( -3.992090130160959482, 162.3768266524160140, 9.188101187500098632 ) ) ;
#79216 = CARTESIAN_POINT ( 'NONE',  ( 39.01788588657935719, 31.03085787977765975, 9.188101187500006262 ) ) ;
#79218 = LINE ( 'NONE', #48783, #35465 ) ;
#79217 = CARTESIAN_POINT ( 'NONE',  ( -57.88150100324660485, 35.92665207732901678, -10.00000000000000000 ) ) ;
#79219 = CARTESIAN_POINT ( 'NONE',  ( 192.8325075361489382, 296.6512949269187516, 11.74553025762331515 ) ) ;
#79220 = CARTESIAN_POINT ( 'NONE',  ( 35.77386594998528579, 21.44966523072496756, -2.296566073217252530E-15 ) ) ;
#79221 = CARTESIAN_POINT ( 'NONE',  ( 205.7576124508049418, 274.2643565215761328, 10.88614016733041545 ) ) ;
#79222 = B_SPLINE_CURVE_WITH_KNOTS ( 'NONE', 3,
 ( #69389, #6, #9092, #30890 ),
 .UNSPECIFIED., .F., .F.,
 ( 4, 4 ),
 ( 0.01340827837672923378, 0.01979442427779384839 ),
 .UNSPECIFIED. ) ;
#79223 = CARTESIAN_POINT ( 'NONE',  ( 183.1953467321624203, 257.8017632849582697, -2.260499853111983537 ) ) ;
#79224 = DIRECTION ( 'NONE',  ( 0.8660254037844379305, 0.5000000000000011102, 0.000000000000000000 ) ) ;
#79225 = VERTEX_POINT ( 'NONE', #71896 ) ;
#79226 = CARTESIAN_POINT ( 'NONE',  ( 196.4501996009505831, 290.3852684645433442, -17.82325615854289680 ) ) ;
#79227 = PLANE ( 'NONE',  #69752 ) ;
#79228 = ADVANCED_FACE ( 'NONE', ( #55648 ), #24770, .T. ) ;
#79229 = CARTESIAN_POINT ( 'NONE',  ( 15.64721481668148328, 11.96004757982088940, -5.678558825948276656 ) ) ;
#79230 = CARTESIAN_POINT ( 'NONE',  ( 168.5795673232786669, 288.2161938891477462, 0.5292475961296263520 ) ) ;
#79231 = CARTESIAN_POINT ( 'NONE',  ( 21.16812676580726915, 15.14754757982089650, -5.678558825948275768 ) ) ;
#79232 = VECTOR ( 'NONE', #58, 1000.000000000000000 ) ;
#79233 = CARTESIAN_POINT ( 'NONE',  ( 160.6659065328018130, 252.3654821715117862, 15.57355298855281411 ) ) ;
#79234 = CARTESIAN_POINT ( 'NONE',  ( 45.80758703142364396, 72.03864405183792030, -10.00000000000000000 ) ) ;
#79235 = CARTESIAN_POINT ( 'NONE',  ( 206.8317058779879574, 272.4039721336197317, -10.41591514895975834 ) ) ;
#79236 = ORIENTED_EDGE ( 'NONE', *, *, #35525, .F. ) ;
#79238 = CARTESIAN_POINT ( 'NONE',  ( 24.32480936679734640, 35.81751292744058190, -6.180339887498951690 ) ) ;
#79237 =( BOUNDED_CURVE ( )  B_SPLINE_CURVE ( 2, ( #32712, #49415, #24611, #9420, #94552, #25107, #17515, #95066, #71741 ),
 .UNSPECIFIED., .F., .T. ) 
 B_SPLINE_CURVE_WITH_KNOTS ( ( 3, 2, 2, 2, 3 ),
 ( 0.1814516129032258118, 0.1827956989247311870, 0.1854838709677419373, 0.1881720430107526876, 0.1895161290322580627 ),
 .UNSPECIFIED. ) 
 CURVE ( )  GEOMETRIC_REPRESENTATION_ITEM ( )  RATIONAL_B_SPLINE_CURVE ( ( 0.9330127018922194093, 0.9330127018922194093, 1.000000000000000000, 0.8660254037844387076, 1.000000000000000000, 0.8660254037844387076, 1.000000000000000000, 0.9330127018922194093, 0.9330127018922194093 ) ) 
 REPRESENTATION_ITEM ( '' )  );
#79239 = CARTESIAN_POINT ( 'NONE',  ( 164.9404048476745004, 244.9618339132846074, -2.801285734921658666 ) ) ;
#79240 = CARTESIAN_POINT ( 'NONE',  ( 148.2404373810095706, 275.8870260502966403, -5.709515531134017330 ) ) ;
#79241 = CARTESIAN_POINT ( 'NONE',  ( 207.5959034698703078, 271.0803430774575418, -1.830000129038042544 ) ) ;
#79242 = CARTESIAN_POINT ( 'NONE',  ( 193.7901930790854976, 294.9925349088783264, 14.24765323155741115 ) ) ;
#79243 = ORIENTED_EDGE ( 'NONE', *, *, #12347, .T. ) ;
#79244 = ORIENTED_EDGE ( 'NONE', *, *, #74099, .F. ) ;
#79245 = CARTESIAN_POINT ( 'NONE',  ( 155.8886909462579524, 276.9667409604651880, -10.24749302008156171 ) ) ;
#79246 = CARTESIAN_POINT ( 'NONE',  ( 86.05378759701316937, 47.66281079019294964, 10.87423542265411136 ) ) ;
#79247 = ORIENTED_EDGE ( 'NONE', *, *, #63629, .F. ) ;
#79248 = CARTESIAN_POINT ( 'NONE',  ( 76.92291097195925431, 53.37782505870914918, 15.93814142932378353 ) ) ;
#79249 = CARTESIAN_POINT ( 'NONE',  ( 188.6351333907390710, 297.8094963952060539, 7.741002703549384023 ) ) ;
#79250 = ORIENTED_EDGE ( 'NONE', *, *, #43789, .T. ) ;
#79251 = CARTESIAN_POINT ( 'NONE',  ( 34.95497629653712579, 28.38052372038643156, 10.00000000000000533 ) ) ;
#79252 = CYLINDRICAL_SURFACE ( 'NONE', #96179, 60.00000000000002132 ) ;
#79253 = CARTESIAN_POINT ( 'NONE',  ( 10.49025449741314375, 29.55466486950698624, -1.111400068045478839E-16 ) ) ;
#79254 = ORIENTED_EDGE ( 'NONE', *, *, #10174, .F. ) ;
#79255 = CARTESIAN_POINT ( 'NONE',  ( 173.7393789614961861, 267.2768702419098759, 16.72977566464747312 ) ) ;
#79256 = CARTESIAN_POINT ( 'NONE',  ( 74.86688500840476479, 62.61836409510868151, -15.31937621055942067 ) ) ;
#79257 = CARTESIAN_POINT ( 'NONE',  ( 128.2660534579352145, 254.8615022471902876, 5.000000000000046185 ) ) ;
#79258 = CARTESIAN_POINT ( 'NONE',  ( 191.3375250863502970, 299.2406804863936145, 8.828791580707859410 ) ) ;
#79259 = CARTESIAN_POINT ( 'NONE',  ( 151.4285566098263018, 275.0047588379541708, -8.595722058304710700 ) ) ;
#79260 = VERTEX_POINT ( 'NONE', #39449 ) ;
#79261 = CARTESIAN_POINT ( 'NONE',  ( 173.6868681682090312, 257.1546749658006661, -11.76848105503814601 ) ) ;
#79262 = ORIENTED_EDGE ( 'NONE', *, *, #81189, .F. ) ;
#79263 = ORIENTED_EDGE ( 'NONE', *, *, #74236, .F. ) ;
#79264 = CARTESIAN_POINT ( 'NONE',  ( -19.65312891409030271, 93.06504152958497400, 10.00000000000000888 ) ) ;
#79266 = ORIENTED_EDGE ( 'NONE', *, *, #31776, .T. ) ;
#79265 = B_SPLINE_CURVE_WITH_KNOTS ( 'NONE', 3,
 ( #38587, #7695, #85764, #62889, #61386, #71018, #22888, #106, #23884, #94335, #77617, #30991, #16791, #78109, #39566, #47679 ),
 .UNSPECIFIED., .F., .F.,
 ( 4, 2, 2, 2, 2, 2, 2, 4 ),
 ( 2.809234570782672869E-17, 0.0003787177898467172050, 0.0007574355796934063292, 0.001136153369540095562, 0.001514871159386784686, 0.001893588949233473593, 0.002272306739080162934, 0.003029742318773669552 ),
 .UNSPECIFIED. ) ;
#79267 = DIRECTION ( 'NONE',  ( 0.4999999999999992784, -0.8660254037844390407, 0.000000000000000000 ) ) ;
#79268 = ORIENTED_EDGE ( 'NONE', *, *, #65026, .T. ) ;
#79269 = CARTESIAN_POINT ( 'NONE',  ( 83.37517334370022581, 49.65420094554470865, 13.45943336448511296 ) ) ;
#79270 = CARTESIAN_POINT ( 'NONE',  ( 168.4007742750857517, 272.6532539270589268, 15.98367080703011567 ) ) ;
#79271 = DIRECTION ( 'NONE',  ( -0.000000000000000000, -0.000000000000000000, -1.000000000000000000 ) ) ;
#79272 = CARTESIAN_POINT ( 'NONE',  ( 70.41189838529163580, 67.31627706263940070, 9.946319558533476268 ) ) ;
#79273 = CARTESIAN_POINT ( 'NONE',  ( 152.7618747630824885, 266.0556667813044101, 16.41480086888796919 ) ) ;
#79275 = CARTESIAN_POINT ( 'NONE',  ( 82.35285118013293015, 53.50770157854819331, -15.77620284334259360 ) ) ;
#79274 = VECTOR ( 'NONE', #71764, 1000.000000000000000 ) ;
#79276 = DIRECTION ( 'NONE',  ( 0.5000000000000048850, -0.8660254037844358210, 0.000000000000000000 ) ) ;
#79277 = VERTEX_POINT ( 'NONE', #1492 ) ;
#79278 = DIRECTION ( 'NONE',  ( -0.2649596321165964552, 0.4589235447807054058, -0.8480480961564325071 ) ) ;
#79279 = CARTESIAN_POINT ( 'NONE',  ( 24.83671989960918935, 22.84335787977763488, 9.188101187500006262 ) ) ;
#79280 = CARTESIAN_POINT ( 'NONE',  ( -50.66096862766640641, 31.69950886434491721, -10.00000000000000000 ) ) ;
#79281 = VECTOR ( 'NONE', #54947, 1000.000000000000114 ) ;
#79283 = VERTEX_POINT ( 'NONE', #93207 ) ;
#79282 = CARTESIAN_POINT ( 'NONE',  ( 159.2111180226792726, 254.8852497853115722, 16.01057445397460910 ) ) ;
#79284 = EDGE_LOOP ( 'NONE', ( #31687, #64125, #34007, #20504 ) ) ;
#79285 = CARTESIAN_POINT ( 'NONE',  ( 191.1214701901826345, 299.6148985437802708, 6.122719862588978046 ) ) ;
#79286 = CARTESIAN_POINT ( 'NONE',  ( 168.2186807742798464, 257.0030785273878564, -14.53950667589619350 ) ) ;
#79287 = CARTESIAN_POINT ( 'NONE',  ( 206.3423291502491566, 273.2515974901050413, -10.76717883871977577 ) ) ;
#79288 = DIRECTION ( 'NONE',  ( -0.09274582908234035861, -0.9956898167541080591, 0.000000000000000000 ) ) ;
#79289 = EDGE_CURVE ( 'NONE', #58918, #90569, #75003, .T. ) ;
#79290 = CARTESIAN_POINT ( 'NONE',  ( 200.6097954076514895, 283.1806371883870383, 16.82611162221071766 ) ) ;
#79291 = EDGE_CURVE ( 'NONE', #56261, #75967, #22951, .T. ) ;
#79292 = CARTESIAN_POINT ( 'NONE',  ( 71.55257436342132848, 59.07939963282102269, 15.82466129307116098 ) ) ;
#79293 = VECTOR ( 'NONE', #84525, 1000.000000000000000 ) ;
#79294 = VERTEX_POINT ( 'NONE', #58651 ) ;
#79295 = DIRECTION ( 'NONE',  ( -0.8660254037844387076, -0.4999999999999998890, -0.000000000000000000 ) ) ;
#79296 = CARTESIAN_POINT ( 'NONE',  ( 11.39908531360040911, 14.78052372038638573, -10.00000000000000355 ) ) ;
#79297 = CARTESIAN_POINT ( 'NONE',  ( 137.1012689553694486, 238.4155109091895781, 2.679491924311254714 ) ) ;
#79298 = EDGE_CURVE ( 'NONE', #82006, #749, #33323, .T. ) ;
#79299 = CARTESIAN_POINT ( 'NONE',  ( 207.2383675728608239, 271.6996134166075763, 7.873592648726489784 ) ) ;
#79300 = EDGE_CURVE ( 'NONE', #65492, #37083, #12588, .T. ) ;
#79301 = CARTESIAN_POINT ( 'NONE',  ( 15.88121511744419756, 186.6427522451419350, -10.00000000000009415 ) ) ;
#79302 = CARTESIAN_POINT ( 'NONE',  ( 93.67942421434402434, 215.7048013555409796, 4.594050593750051981 ) ) ;
#79303 = CARTESIAN_POINT ( 'NONE',  ( 188.8544700204132880, 297.4231428397746413, 9.261439979758030461 ) ) ;
#79304 = LINE ( 'NONE', #88414, #34057 ) ;
#79305 = CARTESIAN_POINT ( 'NONE',  ( 162.9968728533147271, 248.3281300736514652, 11.73082768548638910 ) ) ;
#79307 = CARTESIAN_POINT ( 'NONE',  ( 74.15479259499207387, 55.62765001666249276, -16.59030973340311022 ) ) ;
#79306 = CARTESIAN_POINT ( 'NONE',  ( 4.668163907683432257, 167.3768266524159856, -9.188101187500091527 ) ) ;
#79308 = VECTOR ( 'NONE', #89099, 1000.000000000000000 ) ;
#79309 = CARTESIAN_POINT ( 'NONE',  ( 161.5875797534026219, 250.7690973254556468, 12.95526170413129030 ) ) ;
#79310 = ORIENTED_EDGE ( 'NONE', *, *, #64163, .F. ) ;
#79311 = ORIENTED_EDGE ( 'NONE', *, *, #7138, .T. ) ;
#79312 = CARTESIAN_POINT ( 'NONE',  ( 200.9036115388549320, 267.7944843482957822, -2.996125407750229730 ) ) ;
#79313 = VECTOR ( 'NONE', #24810, 1000.000000000000000 ) ;
#79314 = CARTESIAN_POINT ( 'NONE',  ( 81.06156068051836883, 46.84227557089664629, -12.44431404537389696 ) ) ;
#79315 = CARTESIAN_POINT ( 'NONE',  ( 23.64814127513158937, 118.0650415295850451, 60.00000000000000000 ) ) ;
#79316 = CARTESIAN_POINT ( 'NONE',  ( 207.8575108622103755, 270.6272257822888037, -6.381720258959569847 ) ) ;
#79317 = DIRECTION ( 'NONE',  ( 1.000000000000000000, 0.000000000000000000, 0.000000000000000000 ) ) ;
#79318 = CARTESIAN_POINT ( 'NONE',  ( 74.38843302549192060, 67.97504088991867377, -11.67932444824502802 ) ) ;
#79319 = CARTESIAN_POINT ( 'NONE',  ( 33.73396797431614402, 190.2833772461660544, -9.188101187500095079 ) ) ;
#79320 = CARTESIAN_POINT ( 'NONE',  ( 82.20432729060250665, 218.2677522451418497, 10.00000000000009592 ) ) ;
#79321 = ORIENTED_EDGE ( 'NONE', *, *, #8925, .T. ) ;
#79322 = CARTESIAN_POINT ( 'NONE',  ( 84.73412771832131796, 49.86158731552951195, 13.15459715302734978 ) ) ;
#79323 = CARTESIAN_POINT ( 'NONE',  ( 175.1863726193077184, 281.4530106220159951, -14.19852717654378260 ) ) ;
#79324 = CARTESIAN_POINT ( 'NONE',  ( 36.87552185948406702, 26.45404122711136097, -8.090169943749478065 ) ) ;
#79325 = PLANE ( 'NONE',  #62901 ) ;
#79326 = CARTESIAN_POINT ( 'NONE',  ( 161.1232569692349443, 251.5733279787459367, -14.02750397520710557 ) ) ;
#79327 = CARTESIAN_POINT ( 'NONE',  ( 186.1036463308693953, 283.4423093435331111, 16.91945572683130905 ) ) ;
#79328 = CARTESIAN_POINT ( 'NONE',  ( 194.9220242159064185, 293.0321458743159724, -14.92681063007793263 ) ) ;
#79329 = CARTESIAN_POINT ( 'NONE',  ( 71.21424051265081800, 68.22285992147928368, -10.17931454856913120 ) ) ;
#79330 = CARTESIAN_POINT ( 'NONE',  ( 204.2799274532736433, 276.8237820148827950, 13.55359442435934803 ) ) ;
#79331 = CARTESIAN_POINT ( 'NONE',  ( 191.6723191112861855, 298.6608002251342100, -9.737039817265848995 ) ) ;
#79332 = CARTESIAN_POINT ( 'NONE',  ( 190.3049670482083684, 301.0291234702190764, 0.2225066852051815758 ) ) ;
#79333 = CARTESIAN_POINT ( 'NONE',  ( 135.6272693901029243, 259.1115022471903444, -5.000000000000047962 ) ) ;
#79334 = CARTESIAN_POINT ( 'NONE',  ( 114.7887934315897382, 227.8923013555410080, 4.594050593750050204 ) ) ;
#79335 = CARTESIAN_POINT ( 'NONE',  ( 22.99159801516092472, 18.98920272979926693, 7.433330006724137462 ) ) ;
#79336 = CARTESIAN_POINT ( 'NONE',  ( 74.68831750804957892, 67.03523027571368686, 12.97943796060243216 ) ) ;
#79337 = CIRCLE ( 'NONE', #95551, 70.00000000000001421 ) ;
#79338 = CARTESIAN_POINT ( 'NONE',  ( 72.91440843804703320, 59.27959524831282323, -15.98284220614978501 ) ) ;
#79339 = B_SPLINE_CURVE_WITH_KNOTS ( 'NONE', 3,
 ( #27954, #29947, #58835, #89801 ),
 .UNSPECIFIED., .F., .F.,
 ( 4, 4 ),
 ( 0.004601785012094098890, 0.01014120948868826866 ),
 .UNSPECIFIED. ) ;
#79341 = CARTESIAN_POINT ( 'NONE',  ( 192.6361035247282985, 294.0892689374524593, 14.43747539422717630 ) ) ;
#79340 = DIRECTION ( 'NONE',  ( -0.009162850352631533510, 0.9999580202055560196, 0.000000000000000000 ) ) ;
#79342 =( REPRESENTATION_RELATIONSHIP ('NONE','NONE', #67038, #77412 ) REPRESENTATION_RELATIONSHIP_WITH_TRANSFORMATION ( #53251 )SHAPE_REPRESENTATION_RELATIONSHIP( ) );
#79343 = CARTESIAN_POINT ( 'NONE',  ( 150.7303054078841456, 269.5744481236075671, -15.29931087522330735 ) ) ;
#79344 = DIRECTION ( 'NONE',  ( -0.8660254037844387076, -0.4999999999999998890, -0.000000000000000000 ) ) ;
#79345 = CARTESIAN_POINT ( 'NONE',  ( 149.0203866098534888, 272.5361143586139860, -12.73049804737905255 ) ) ;
#79346 = EDGE_CURVE ( 'NONE', #94303, #66081, #49492, .T. ) ;
#79347 = CARTESIAN_POINT ( 'NONE',  ( 46.16617079539854274, 27.44966523072498177, -2.296566073217252530E-15 ) ) ;
#79348 = CARTESIAN_POINT ( 'NONE',  ( 173.1762443375220926, 289.7177692896065651, -1.166275841582373296 ) ) ;
#79349 = FACE_OUTER_BOUND ( 'NONE', #66576, .T. ) ;
#79350 = ORIENTED_EDGE ( 'NONE', *, *, #94138, .T. ) ;
#79351 = CARTESIAN_POINT ( 'NONE',  ( 69.57147599204645871, 65.95357847136563123, -11.50044640693676001 ) ) ;
#79352 = CARTESIAN_POINT ( 'NONE',  ( 176.8552821818880147, 279.2679361169009553, 15.50986861091530145 ) ) ;
#79353 = DIRECTION ( 'NONE',  ( 0.000000000000000000, 0.000000000000000000, 1.000000000000000000 ) ) ;
#79354 = B_SPLINE_CURVE_WITH_KNOTS ( 'NONE', 3,
 ( #87300, #71538, #1641, #63419, #1125, #17313, #54809, #70006, #621, #78637 ),
 .UNSPECIFIED., .F., .F.,
 ( 4, 2, 2, 2, 4 ),
 ( 0.000000000000000000, 0.0003983244503580934048, 0.0007966489007161868096, 0.001194973351074280106, 0.001593297801432373619 ),
 .UNSPECIFIED. ) ;
#79355 = ORIENTED_EDGE ( 'NONE', *, *, #46022, .T. ) ;
#79356 = CARTESIAN_POINT ( 'NONE',  ( 85.69613440654960357, 45.85434288225457777, 9.691492161565614438 ) ) ;
#79357 = CARTESIAN_POINT ( 'NONE',  ( 83.90135245898494532, 51.67424826075555444, -14.40821023666590150 ) ) ;
#79358 = CARTESIAN_POINT ( 'NONE',  ( 170.5993847053230468, 287.8722104901659691, 7.679145147933459370 ) ) ;
#79359 = AXIS2_PLACEMENT_3D ( 'NONE', #51725, #82668, #81655 ) ;
#79360 = CARTESIAN_POINT ( 'NONE',  ( 182.1439385020048860, 290.0253507885926183, 13.01467259685074573 ) ) ;
#79361 = VERTEX_POINT ( 'NONE', #18187 ) ;
#79362 = CARTESIAN_POINT ( 'NONE',  ( 200.3804403721752578, 281.5778917628034606, 17.30444700233937994 ) ) ;
#79363 = B_SPLINE_SURFACE_WITH_KNOTS ( 'NONE', 3, 1, ( 
 ( #26499, #60845 ),
 ( #90830, #29968 ),
 ( #6676, #99388 ),
 ( #20398, #21381 ),
 ( #45649, #89822 ),
 ( #76103, #97896 ),
 ( #53265, #36068 ),
 ( #91308, #6172 ),
 ( #84220, #37553 ),
 ( #98398, #27974 ),
 ( #90328, #12808 ),
 ( #68462, #36564 ),
 ( #83208, #4692 ),
 ( #60348, #82730 ),
 ( #59864, #75096 ),
 ( #59352, #21869 ),
 ( #37069, #13302 ),
 ( #5675, #28471 ),
 ( #67471, #28989 ),
 ( #44161, #43670 ),
 ( #91807, #22368 ),
 ( #52269, #14768 ),
 ( #58852, #52754 ),
 ( #20903, #51792 ),
 ( #35584, #66479 ),
 ( #67973, #83715 ),
 ( #66967, #14273 ),
 ( #13773, #97405 ),
 ( #44652, #75586 ),
 ( #51268, #98894 ),
 ( #5187, #82233 ),
 ( #74613, #29476 ),
 ( #45164, #47155 ),
 ( #92314, #70461 ) ),
 .UNSPECIFIED., .T., .F., .F.,
 ( 4, 2, 2, 2, 2, 2, 2, 2, 2, 2, 2, 2, 2, 2, 2, 2, 4 ),
 ( 2, 2 ),
 ( 0.000000000000000000, 0.06250000000000000000, 0.1250000000000000000, 0.1875000000000000000, 0.2500000000000000000, 0.3125000000000000000, 0.3750000000000000000, 0.4375000000000000000, 0.5000000000000000000, 0.5625000000000000000, 0.6250000000000000000, 0.6875000000000000000, 0.7500000000000000000, 0.8125000000000000000, 0.8750000000000000000, 0.9375000000000000000, 1.000000000000000000 ),
 ( 0.000000000000000000, 1.000000000000000000 ),
 .UNSPECIFIED. ) ;
#79364 = CARTESIAN_POINT ( 'NONE',  ( 35.53452623260358223, 35.91421378149921395, 9.188101187500008038 ) ) ;
#79365 = CARTESIAN_POINT ( 'NONE',  ( 174.0778791619732715, 272.0937389636918056, -17.24785809618570909 ) ) ;
#79366 = ORIENTED_EDGE ( 'NONE', *, *, #54268, .T. ) ;
#79367 = CARTESIAN_POINT ( 'NONE',  ( 77.87494449001893315, 61.77424058857110367, 16.06449337301375735 ) ) ;
#79368 = ADVANCED_FACE ( 'NONE', ( #66764 ), #537, .F. ) ;
#79369 = CARTESIAN_POINT ( 'NONE',  ( 39.77289032284285497, 58.49985355908045648, 10.00000000000000000 ) ) ;
#79370 = CARTESIAN_POINT ( 'NONE',  ( 164.5515570353740031, 246.1500442291780644, -1.332946268338321083 ) ) ;
#79371 = ORIENTED_EDGE ( 'NONE', *, *, #89569, .F. ) ;
#79372 = CARTESIAN_POINT ( 'NONE',  ( 86.19539083654223077, 46.94244887560866886, -10.58787169974292297 ) ) ;
#79373 = CARTESIAN_POINT ( 'NONE',  ( 188.4650206215856088, 293.1607027833161396, 12.53756631082011630 ) ) ;
#79374 = CARTESIAN_POINT ( 'NONE',  ( 27.36453209247643770, 17.92755873383626408, 6.180339887498953466 ) ) ;
#79375 = CARTESIAN_POINT ( 'NONE',  ( 83.64242591893872714, 50.13093507612888544, -13.68615876095049266 ) ) ;
#79376 = CARTESIAN_POINT ( 'NONE',  ( 84.81815374307583966, 49.91023469830950177, -13.17998982162479571 ) ) ;
#79377 = CARTESIAN_POINT ( 'NONE',  ( 154.9528145190857344, 262.2608478075840708, -17.26679351315302213 ) ) ;
#79378 = ORIENTED_EDGE ( 'NONE', *, *, #39754, .T. ) ;
#79379 = EDGE_LOOP ( 'NONE', ( #80797, #12966, #1449, #92328 ) ) ;
#79380 = CARTESIAN_POINT ( 'NONE',  ( 176.1816596051692727, 259.6738327371759283, 12.35962930718384989 ) ) ;
#79381 = VERTEX_POINT ( 'NONE', #91591 ) ;
#79382 = CARTESIAN_POINT ( 'NONE',  ( 77.15327844083580544, 49.48234140023242134, -15.45668963368342119 ) ) ;
#79383 = ORIENTED_EDGE ( 'NONE', *, *, #7343, .T. ) ;
#79384 = CARTESIAN_POINT ( 'NONE',  ( 88.37114838251338256, 44.19826770168089780, 0.1617965445409229042 ) ) ;
#79385 = CARTESIAN_POINT ( 'NONE',  ( 79.42409360036769783, 54.45300451108273876, 15.94632819799358892 ) ) ;
#79386 = ORIENTED_EDGE ( 'NONE', *, *, #61515, .T. ) ;
#79387 = CARTESIAN_POINT ( 'NONE',  ( 164.3284847670581144, 246.0217105830841433, -2.055838629128057704 ) ) ;
#79388 = CARTESIAN_POINT ( 'NONE',  ( 189.9967389050536610, 301.5629902744856281, 3.223574158822913205 ) ) ;
#79389 = CARTESIAN_POINT ( 'NONE',  ( -13.11024591527734451, 6.000000000000000000, -20.00000000000000000 ) ) ;
#79390 = CARTESIAN_POINT ( 'NONE',  ( 146.7943851877206214, 276.3916619194686746, -4.608908220452185844 ) ) ;
#79391 = CARTESIAN_POINT ( 'NONE',  ( 153.2513309553138470, 265.2079037882803618, -16.24091495603130397 ) ) ;
#79392 = CARTESIAN_POINT ( 'NONE',  ( 23.08833070876649529, 13.73415679381821874, 1.333680081654574804E-15 ) ) ;
#79393 = CARTESIAN_POINT ( 'NONE',  ( 203.3946109532447224, 276.3571951737117729, -14.55139583984842133 ) ) ;
#79394 = CARTESIAN_POINT ( 'NONE',  ( 126.7777458412893026, 237.8768266524160140, -9.188101187500091527 ) ) ;
#79395 = CARTESIAN_POINT ( 'NONE',  ( 70.59038599826907046, 60.90612631591859127, -14.48346838026379579 ) ) ;
#79396 = CARTESIAN_POINT ( 'NONE',  ( 45.61829935282815995, 28.19860640527296525, 2.839279412974134775 ) ) ;
#79397 = ORIENTED_EDGE ( 'NONE', *, *, #74862, .F. ) ;
#79399 = VERTEX_POINT ( 'NONE', #99674 ) ;
#79398 = CARTESIAN_POINT ( 'NONE',  ( 85.49318370521093868, 48.99722645306706426, -12.73116331006621316 ) ) ;
#79400 = CARTESIAN_POINT ( 'NONE',  ( 203.5684408170273514, 276.3809927624695320, 13.51646973350518444 ) ) ;
#79401 = CARTESIAN_POINT ( 'NONE',  ( 180.7033225138871444, 256.2122485056048617, 1.289357501824909935 ) ) ;
#79402 = CARTESIAN_POINT ( 'NONE',  ( 171.2412005135090851, 287.8500574525499474, -4.635942788142338067 ) ) ;
#79403 = CARTESIAN_POINT ( 'NONE',  ( 147.4632325565963527, 275.2331842940668594, 3.329760414512866085 ) ) ;
#79404 = CARTESIAN_POINT ( 'NONE',  ( 73.40795240808809297, 67.02439710917190041, 11.95168579066343995 ) ) ;
#79405 = CARTESIAN_POINT ( 'NONE',  ( 76.45572749640669485, 51.64231386250387601, -16.15369532800221108 ) ) ;
#79406 = CARTESIAN_POINT ( 'NONE',  ( 176.8458400405337443, 288.5831395991251611, -9.313839573048495524 ) ) ;
#79407 = CARTESIAN_POINT ( 'NONE',  ( 192.6700440564185044, 292.3860465289164381, -14.35732980996189845 ) ) ;
#79408 = DIRECTION ( 'NONE',  ( 1.000000000000000000, 0.000000000000000000, -1.082076799516502204E-16 ) ) ;
#79409 = EDGE_LOOP ( 'NONE', ( #56364, #24619, #84622, #1216 ) ) ;
#79410 = CARTESIAN_POINT ( 'NONE',  ( 147.8308140999695866, 274.5965143850199865, -7.866624397492971710 ) ) ;
#79411 = CARTESIAN_POINT ( 'NONE',  ( -42.18579364100346396, 26.51648975995176372, 10.00000000000000000 ) ) ;
#79412 = VERTEX_POINT ( 'NONE', #59136 ) ;
#79413 = EDGE_CURVE ( 'NONE', #83448, #29993, #37465, .T. ) ;
#79414 = CARTESIAN_POINT ( 'NONE',  ( 163.4882229232755151, 278.1335026457492745, 13.64712021366251804 ) ) ;
#79415 = EDGE_CURVE ( 'NONE', #79774, #91452, #5510, .T. ) ;
#79416 = CARTESIAN_POINT ( 'NONE',  ( 159.4766020264466420, 278.1878426662964330, 10.34255018954605276 ) ) ;
#79417 = CARTESIAN_POINT ( 'NONE',  ( 191.4370491047775715, 299.0682998299044471, -9.862002456538565554 ) ) ;
#79418 = CARTESIAN_POINT ( 'NONE',  ( 148.9228818358559749, 272.7049975811580680, 12.13823097167056275 ) ) ;
#79419 = CARTESIAN_POINT ( 'NONE',  ( 162.6774150396764469, 248.8814472377480911, 10.88033986792731689 ) ) ;
#79421 = CARTESIAN_POINT ( 'NONE',  ( 160.8923266782674659, 281.5875368026315755, 5.746848696840308968 ) ) ;
#79420 = CARTESIAN_POINT ( 'NONE',  ( 153.4150141106643161, 270.1174769024833040, 14.14566187613772641 ) ) ;
#79422 = CARTESIAN_POINT ( 'NONE',  ( 199.9222995550700261, 267.4785754008608478, 6.216224682353979070 ) ) ;
#79423 = ORIENTED_EDGE ( 'NONE', *, *, #77669, .T. ) ;
#79424 = CARTESIAN_POINT ( 'NONE',  ( 164.0796711861443669, 280.3631140631478047, -11.42675980477452136 ) ) ;
#79425 = CARTESIAN_POINT ( 'NONE',  ( 192.1412027652805534, 261.7830949532877298, 4.365074532660510265 ) ) ;
#79426 = CARTESIAN_POINT ( 'NONE',  ( 39.01205572417272549, 91.95295005193447935, 59.99999999999999289 ) ) ;
#79427 = CYLINDRICAL_SURFACE ( 'NONE', #28693, 10.00000000000010658 ) ;
#79428 = CARTESIAN_POINT ( 'NONE',  ( -76.38857681351474582, 54.22815603855766398, -10.00000000000000000 ) ) ;
#79429 = CARTESIAN_POINT ( 'NONE',  ( 152.6945189806187955, 266.1723304187151484, 16.62409282110771613 ) ) ;
#79430 = CARTESIAN_POINT ( 'NONE',  ( 73.91288345017510153, 68.57868192222672121, 11.39134523673511623 ) ) ;
#79431 = VECTOR ( 'NONE', #59030, 1000.000000000000114 ) ;
#79432 = CARTESIAN_POINT ( 'NONE',  ( 44.73065482718367747, 120.5373619841236774, 10.00000000000000000 ) ) ;
#79433 = CARTESIAN_POINT ( 'NONE',  ( -110.0000000000000142, 0.000000000000000000, 9.212605237762145904 ) ) ;
#79434 = CARTESIAN_POINT ( 'NONE',  ( -8.863483026448420787, 159.5643266524160140, 9.188101187500095079 ) ) ;
#79435 = CARTESIAN_POINT ( 'NONE',  ( 81.82518085639701155, 227.2369531367911293, -4.594050593750048428 ) ) ;
#79436 = CARTESIAN_POINT ( 'NONE',  ( 202.9490938173916561, 279.1288534886517709, -16.56031645010252973 ) ) ;
#79437 = CARTESIAN_POINT ( 'NONE',  ( 87.89455619572203204, 44.47450605225177611, -3.950270982313550672 ) ) ;
#79438 = LINE ( 'NONE', #8987, #2702 ) ;
#79439 = DIRECTION ( 'NONE',  ( -0.8660254037844387076, -0.4999999999999998890, -0.000000000000000000 ) ) ;
#79440 = CARTESIAN_POINT ( 'NONE',  ( 78.28440716897011953, 56.29478510322071827, 16.19025749928794156 ) ) ;
#79441 = DIRECTION ( 'NONE',  ( -0.5000000000000014433, 0.8660254037844378194, 0.000000000000000000 ) ) ;
#79443 = CARTESIAN_POINT ( 'NONE',  ( 163.2256942281324541, 247.9317998266098471, -9.780520296312531059 ) ) ;
#79442 = CARTESIAN_POINT ( 'NONE',  ( 77.95436975687957215, 48.11784896437987413, 14.20357318872345331 ) ) ;
#79444 = CARTESIAN_POINT ( 'NONE',  ( 207.7267680070821427, 270.8536790500975826, 4.918728265708383063 ) ) ;
#79445 = CARTESIAN_POINT ( 'NONE',  ( 169.2519802811189891, 252.1610067817271954, -8.894316421355656033 ) ) ;
#79446 = CARTESIAN_POINT ( 'NONE',  ( 170.6278779686246878, 289.8994199495515431, -0.2720655136580445999 ) ) ;
#79447 = CARTESIAN_POINT ( 'NONE',  ( 181.8509774751104544, 266.9677320091309412, 16.09658033613713712 ) ) ;
#79448 = CARTESIAN_POINT ( 'NONE',  ( 165.9983592287585168, 253.7040021870680562, -13.23752916164668569 ) ) ;
#79449 = CARTESIAN_POINT ( 'NONE',  ( 72.80224333330460240, 56.85357120363885031, -15.94159948215087219 ) ) ;
#79450 = DIRECTION ( 'NONE',  ( 1.000000000000000000, 0.000000000000000000, 0.000000000000000000 ) ) ;
#79451 = CARTESIAN_POINT ( 'NONE',  ( 35.03300607999280913, 191.0333772461660544, 9.188101187500095079 ) ) ;
#79452 = CARTESIAN_POINT ( 'NONE',  ( 76.82578666445662918, 64.07401149769333415, -15.18382690731647600 ) ) ;
#79453 = CARTESIAN_POINT ( 'NONE',  ( 66.96803994030899787, 197.2202760586659736, -5.415160957724236172E-17 ) ) ;
#79454 = CARTESIAN_POINT ( 'NONE',  ( 207.5462191418491500, 271.1663988579299485, -5.239401497773396699 ) ) ;
#79455 = CARTESIAN_POINT ( 'NONE',  ( 88.15693819664804209, 44.07453305466302140, 0.5464416844217639957 ) ) ;
#79456 = CARTESIAN_POINT ( 'NONE',  ( 13.67456932412660997, 8.864269794150878568, -3.090169943749474069 ) ) ;
#79458 = CARTESIAN_POINT ( 'NONE',  ( 199.6718038460705031, 284.8052862301161667, 17.94500466126824989 ) ) ;
#79457 = LINE ( 'NONE', #47997, #16087 ) ;
#79459 = CARTESIAN_POINT ( 'NONE',  ( 176.7734426553208777, 270.1971082629633543, -16.99733951863274939 ) ) ;
#79460 = EDGE_CURVE ( 'NONE', #74753, #93745, #51568, .T. ) ;
#79461 = CARTESIAN_POINT ( 'NONE',  ( 27.63686232447692603, 34.14336893147756768, 7.433330006724141015 ) ) ;
#79462 = CARTESIAN_POINT ( 'NONE',  ( 77.93017357788673394, 184.0458036431182052, -30.52142883766498116 ) ) ;
#79463 = CARTESIAN_POINT ( 'NONE',  ( 149.3141802193904368, 272.0272488999566463, -11.40332369054239336 ) ) ;
#79464 = ORIENTED_EDGE ( 'NONE', *, *, #86538, .F. ) ;
#79465 = CARTESIAN_POINT ( 'NONE',  ( 13.87187630571069263, 28.98502408145591502, -5.678558825948271327 ) ) ;
#79466 = CARTESIAN_POINT ( 'NONE',  ( 68.83479979963041728, 219.7369531367911293, -4.594050593750048428 ) ) ;
#79467 = DIRECTION ( 'NONE',  ( 0.8261602328994307465, -0.5634352399127678934, 0.000000000000000000 ) ) ;
#79468 = CARTESIAN_POINT ( 'NONE',  ( 172.4195363219592707, 289.2899927951424388, -1.060142233323475791 ) ) ;
#79469 = LINE ( 'NONE', #79963, #39264 ) ;
#79470 = LINE ( 'NONE', #41407, #47598 ) ;
#79471 = EDGE_CURVE ( 'NONE', #32340, #18263, #64037, .T. ) ;
#79472 = CARTESIAN_POINT ( 'NONE',  ( 86.72314128514305764, 46.93129043413777168, 10.24845158530357558 ) ) ;
#79473 = DIRECTION ( 'NONE',  ( -0.5000000000000013323, 0.8660254037844380415, -0.000000000000000000 ) ) ;
#79474 = CARTESIAN_POINT ( 'NONE',  ( 122.6368883333364010, 241.6115022471902591, 10.00000000000009592 ) ) ;
#79475 = CARTESIAN_POINT ( 'NONE',  ( 20.41989025203908881, 171.0494855054051584, -2.679491924311248496 ) ) ;
#79476 = CARTESIAN_POINT ( 'NONE',  ( 75.14123710989004223, 53.08787395263782827, 16.49283882849012173 ) ) ;
#79477 = ORIENTED_EDGE ( 'NONE', *, *, #50619, .F. ) ;
#79478 = CARTESIAN_POINT ( 'NONE',  ( 82.33309958831539177, 53.73407448881686577, 15.84243556053685786 ) ) ;
#79479 = ORIENTED_EDGE ( 'NONE', *, *, #13111, .T. ) ;
#79480 = CARTESIAN_POINT ( 'NONE',  ( 202.9689790241539242, 279.0944113002206564, 15.85114608332523289 ) ) ;
#79481 = CARTESIAN_POINT ( 'NONE',  ( -71.61465314115659453, 63.06504152958490295, -10.00000000000000888 ) ) ;
#79482 = EDGE_CURVE ( 'NONE', #3700, #38681, #56457, .T. ) ;
#79483 = CARTESIAN_POINT ( 'NONE',  ( 68.35293204362942276, 68.73096724137640479, -5.990830183022922029 ) ) ;
#79484 = ORIENTED_EDGE ( 'NONE', *, *, #41041, .T. ) ;
#79485 = CARTESIAN_POINT ( 'NONE',  ( 173.3282377161554848, 251.6955198918108749, -0.2234702318904273066 ) ) ;
#79486 = ORIENTED_EDGE ( 'NONE', *, *, #48612, .T. ) ;
#79487 = CARTESIAN_POINT ( 'NONE',  ( 72.29720748969889144, 71.75793896413090067, 5.568862843245712568 ) ) ;
#79488 = CARTESIAN_POINT ( 'NONE',  ( 170.1765561332687184, 250.1434207139878652, 3.414147863577436048 ) ) ;
#79489 = CARTESIAN_POINT ( 'NONE',  ( 206.9676577495037577, 271.5526395553730481, -5.460015649064563270 ) ) ;
#79490 = ORIENTED_EDGE ( 'NONE', *, *, #15697, .F. ) ;
#79491 = B_SPLINE_CURVE_WITH_KNOTS ( 'NONE', 3,
 ( #30960, #37552, #52268, #30465, #22862, #77059, #7667, #92797, #38553, #69463 ),
 .UNSPECIFIED., .F., .F.,
 ( 4, 2, 2, 2, 4 ),
 ( 0.000000000000000000, 0.0002622400424273620893, 0.0005244800848547241786, 0.0007867201272820862137, 0.001048960169709448357 ),
 .UNSPECIFIED. ) ;
#79492 = CARTESIAN_POINT ( 'NONE',  ( 31.43713336585798146, 20.01110640527293683, 2.839279412974134775 ) ) ;
#79493 = CARTESIAN_POINT ( 'NONE',  ( 75.30311887994048448, 66.55154771318241558, -13.10674181759690704 ) ) ;
#79494 = CARTESIAN_POINT ( 'NONE',  ( 82.15597685699214026, 48.58689493459846176, -13.20209974158375488 ) ) ;
#79495 = DIRECTION ( 'NONE',  ( 0.5000000000000014433, -0.8660254037844378194, 0.000000000000000000 ) ) ;
#79496 = ADVANCED_FACE ( 'NONE', ( #31245 ), #40336, .T. ) ;
#79497 = CYLINDRICAL_SURFACE ( 'NONE', #33538, 10.00000000000010658 ) ;
#79498 = ORIENTED_EDGE ( 'NONE', *, *, #46049, .T. ) ;
#79499 = VECTOR ( 'NONE', #68349, 1000.000000000000000 ) ;
#79500 = VERTEX_POINT ( 'NONE', #46955 ) ;
#79501 = CARTESIAN_POINT ( 'NONE',  ( 183.1229191643124921, 295.7565714162242330, 0.9213203475738164228 ) ) ;
#79503 = CARTESIAN_POINT ( 'NONE',  ( 194.6782745185928434, 293.4543327343926080, -14.56555309295305634 ) ) ;
#79502 = CARTESIAN_POINT ( 'NONE',  ( 162.6948115306194893, 284.8132865779174949, -2.619575048482838397 ) ) ;
#79504 = LINE ( 'NONE', #87133, #27065 ) ;
#79505 = CARTESIAN_POINT ( 'NONE',  ( 155.2695601165254402, 261.7122283397445131, 16.98599069618989077 ) ) ;
#79506 = CARTESIAN_POINT ( 'NONE',  ( 32.36713501728652176, 42.18528772668521043, -1.583844403245329602 ) ) ;
#79507 = CARTESIAN_POINT ( 'NONE',  ( 205.0520875136525376, 275.4863615587311756, -14.16385635411862509 ) ) ;
#79508 = CARTESIAN_POINT ( 'NONE',  ( 164.7499588712500724, 245.2916960205490398, 5.222210624224128850 ) ) ;
#79509 = CARTESIAN_POINT ( 'NONE',  ( 71.38852909611460973, 62.80635017521332486, -14.35756287307077805 ) ) ;
#79510 = PLANE ( 'NONE',  #40229 ) ;
#79511 = CARTESIAN_POINT ( 'NONE',  ( 88.91628449352961638, 212.9548013555409796, -4.594050593750042211 ) ) ;
#79512 = ORIENTED_EDGE ( 'NONE', *, *, #67003, .T. ) ;
#79513 = CARTESIAN_POINT ( 'NONE',  ( 190.8264243556038195, 300.1259329198319961, 8.466983560044813117 ) ) ;
#79514 = CARTESIAN_POINT ( 'NONE',  ( 197.4151212697929907, 279.2547988841874371, -17.17267392321700470 ) ) ;
#79515 = LINE ( 'NONE', #93197, #70689 ) ;
#79516 = ORIENTED_EDGE ( 'NONE', *, *, #97429, .T. ) ;
#79517 = CARTESIAN_POINT ( 'NONE',  ( 164.9124716213052864, 264.7286630427709042, -16.72847895078608360 ) ) ;
#79518 = VERTEX_POINT ( 'NONE', #1865 ) ;
#79519 = EDGE_CURVE ( 'NONE', #41986, #39534, #22928, .T. ) ;
#79520 = CARTESIAN_POINT ( 'NONE',  ( 185.1252552835508425, 268.3045509528566299, -15.86481251201890608 ) ) ;
#79521 = CARTESIAN_POINT ( 'NONE',  ( 66.64560853618554859, 67.51366659840367390, 6.429781813620476072 ) ) ;
#79522 = B_SPLINE_CURVE_WITH_KNOTS ( 'NONE', 3,
 ( #8424, #323, #24616, #46405 ),
 .UNSPECIFIED., .F., .F.,
 ( 4, 4 ),
 ( 0.000000000000000000, 0.007199726097782813139 ),
 .UNSPECIFIED. ) ;
#79523 = CARTESIAN_POINT ( 'NONE',  ( 147.1447476476323004, 275.7848163378367872, 0.6373001129109078233 ) ) ;
#79524 = DIRECTION ( 'NONE',  ( -0.4999999999999987232, 0.8660254037844394848, 0.000000000000000000 ) ) ;
#79525 = CARTESIAN_POINT ( 'NONE',  ( 82.18974175748606115, 47.92037233983167965, -12.77561182005171858 ) ) ;
#79526 = CARTESIAN_POINT ( 'NONE',  ( 163.1177074157340030, 248.1188384722309195, 11.53923137679231026 ) ) ;
#79527 = VERTEX_POINT ( 'NONE', #62634 ) ;
#79528 = ADVANCED_FACE ( 'NONE', ( #93589, #78374 ), #24157, .T. ) ;
#79529 =( BOUNDED_CURVE ( )  B_SPLINE_CURVE ( 2, ( #31934, #85713, #86706, #85189, #39521, #40535, #46641, #16747, #77566 ),
 .UNSPECIFIED., .F., .T. ) 
 B_SPLINE_CURVE_WITH_KNOTS ( ( 3, 2, 2, 2, 3 ),
 ( 0.08467741935483871774, 0.08602150537634409289, 0.08870967741935484319, 0.09139784946236559349, 0.09274193548387096864 ),
 .UNSPECIFIED. ) 
 CURVE ( )  GEOMETRIC_REPRESENTATION_ITEM ( )  RATIONAL_B_SPLINE_CURVE ( ( 0.9330127018922192983, 0.9330127018922196314, 1.000000000000000000, 0.8660254037844387076, 1.000000000000000000, 0.8660254037844387076, 1.000000000000000000, 0.9330127018922194093, 0.9330127018922194093 ) ) 
 REPRESENTATION_ITEM ( '' )  );
#79530 = ORIENTED_EDGE ( 'NONE', *, *, #86236, .F. ) ;
#79531 = CARTESIAN_POINT ( 'NONE',  ( 161.5872815829137608, 250.7696137718916134, -14.26133658251064951 ) ) ;
#79532 = ORIENTED_EDGE ( 'NONE', *, *, #57949, .T. ) ;
#79533 = B_SPLINE_CURVE_WITH_KNOTS ( 'NONE', 3,
 ( #13590, #14585, #52563, #37856 ),
 .UNSPECIFIED., .F., .F.,
 ( 4, 4 ),
 ( 0.000000000000000000, 0.006921230768823173965 ),
 .UNSPECIFIED. ) ;
#79534 = EDGE_CURVE ( 'NONE', #90906, #95819, #48431, .T. ) ;
#79535 = ADVANCED_FACE ( 'NONE', ( #89035 ), #2376, .F. ) ;
#79536 = CARTESIAN_POINT ( 'NONE',  ( 149.1653648461108617, 275.5304674000249179, 7.618651205328232479 ) ) ;
#79537 = DIRECTION ( 'NONE',  ( -0.6911977992267216431, 0.7226656227773233798, 0.000000000000000000 ) ) ;
#79538 = CARTESIAN_POINT ( 'NONE',  ( -19.65312891409030271, 93.06504152958497400, 60.00000000000000000 ) ) ;
#79539 = CARTESIAN_POINT ( 'NONE',  ( 87.71763047028392180, 44.72620838780621000, 5.018703809423653794 ) ) ;
#79540 = ORIENTED_EDGE ( 'NONE', *, *, #42578, .F. ) ;
#79541 = CARTESIAN_POINT ( 'NONE',  ( 205.0993130461165777, 275.4045645370890156, 13.92529057593422337 ) ) ;
#79542 = EDGE_CURVE ( 'NONE', #71064, #37080, #67615, .T. ) ;
#79543 = CARTESIAN_POINT ( 'NONE',  ( 158.6510112063557756, 274.6825264219753535, 12.95479408922676257 ) ) ;
#79544 = CARTESIAN_POINT ( 'NONE',  ( 206.8313602288537538, 272.4045708154811791, -9.607337080360906612 ) ) ;
#79545 = EDGE_CURVE ( 'NONE', #28883, #7026, #96738, .T. ) ;
#79546 = LINE ( 'NONE', #33917, #52918 ) ;
#79547 = CARTESIAN_POINT ( 'NONE',  ( 71.55773796007210308, 59.00899692431989507, -15.84486509706986190 ) ) ;
#79548 = DIRECTION ( 'NONE',  ( -0.8660254037844387076, -0.4999999999999998890, -0.000000000000000000 ) ) ;
#79549 = CARTESIAN_POINT ( 'NONE',  ( 144.5581563630820767, 254.2677522451418781, 10.00000000000009592 ) ) ;
#79550 = ORIENTED_EDGE ( 'NONE', *, *, #8433, .T. ) ;
#79551 = DIRECTION ( 'NONE',  ( -1.850371707708595795E-16, -7.401486830834383181E-16, 1.000000000000000000 ) ) ;
#79552 = CARTESIAN_POINT ( 'NONE',  ( 161.7587802986029999, 250.4725692828850754, 14.33336164792646450 ) ) ;
#79553 = LINE ( 'NONE', #10108, #4249 ) ;
#79554 = CARTESIAN_POINT ( 'NONE',  ( 168.7662487658844839, 250.5857779709543820, 6.949784551538230382 ) ) ;
#79555 = CARTESIAN_POINT ( 'NONE',  ( 78.25353035412973668, 61.73196396808427266, 15.76132319596081111 ) ) ;
#79556 = CARTESIAN_POINT ( 'NONE',  ( 178.1182393013862395, 291.3468047747071523, -6.134831094139173935 ) ) ;
#79557 = CARTESIAN_POINT ( 'NONE',  ( 202.6713589670606552, 279.6099043604578469, -16.15432042160254511 ) ) ;
#79558 = ORIENTED_EDGE ( 'NONE', *, *, #12926, .T. ) ;
#79559 = CARTESIAN_POINT ( 'NONE',  ( 75.68675361614918984, 63.43720209078236394, -14.77468968376273395 ) ) ;
#79560 = CARTESIAN_POINT ( 'NONE',  ( 181.9757784701835135, 264.1876005812737844, 13.64994279689907231 ) ) ;
#79561 = CARTESIAN_POINT ( 'NONE',  ( 79.78867003348828746, 55.35328538066816861, 16.44695013865527855 ) ) ;
#79562 = CARTESIAN_POINT ( 'NONE',  ( 36.61341721041482344, 22.10801979619931501, 3.090169943749476733 ) ) ;
#79563 = CARTESIAN_POINT ( 'NONE',  ( 192.3401793061076717, 297.5040324353506094, 12.56432540404525611 ) ) ;
#79564 = CARTESIAN_POINT ( 'NONE',  ( 168.6481342183708705, 273.1260240405907211, 15.95224985717143618 ) ) ;
#79565 = CARTESIAN_POINT ( 'NONE',  ( 86.96434452339640586, 43.30424524822677768, 3.123802667395221722 ) ) ;
#79566 = CARTESIAN_POINT ( 'NONE',  ( 188.4534122740155624, 260.4225287015167396, 3.718312834711502202 ) ) ;
#79567 = VECTOR ( 'NONE', #12533, 1000.000000000000000 ) ;
#79568 = CARTESIAN_POINT ( 'NONE',  ( 162.6991225460172927, 284.8212170328912975, -3.897741803361528756 ) ) ;
#79569 = CARTESIAN_POINT ( 'NONE',  ( 2.719259653403430121, 178.5024278399160949, -9.188101187500093303 ) ) ;
#79570 = CARTESIAN_POINT ( 'NONE',  ( 82.37317549191088517, 48.42277367534339305, 13.04792507358340359 ) ) ;
#79571 = ORIENTED_EDGE ( 'NONE', *, *, #20648, .F. ) ;
#79572 = CARTESIAN_POINT ( 'NONE',  ( 177.8840711869828510, 256.7301028248324997, 8.353015782577163151 ) ) ;
#79573 = DIRECTION ( 'NONE',  ( -0.000000000000000000, 0.000000000000000000, -1.000000000000000000 ) ) ;
#79574 = CARTESIAN_POINT ( 'NONE',  ( 164.4698008747318738, 245.7769439046653019, -6.272955660526681854 ) ) ;
#79575 = CARTESIAN_POINT ( 'NONE',  ( 42.17466224797323804, 36.30066082961425877, -10.00000000000000533 ) ) ;
#79576 = CARTESIAN_POINT ( 'NONE',  ( 31.83936385565518279, 195.3149278399160664, 9.188101187500093303 ) ) ;
#79577 = CARTESIAN_POINT ( 'NONE',  ( 164.3602934812760452, 245.9666162739349318, -7.171958108566009571 ) ) ;
#79578 = CARTESIAN_POINT ( 'NONE',  ( 190.1752790837055045, 301.2537496138681945, -5.177773110520776711 ) ) ;
#79579 = CARTESIAN_POINT ( 'NONE',  ( 31.59942275858663407, 40.01751292744058475, 6.180339887498949913 ) ) ;
#79580 = CARTESIAN_POINT ( 'NONE',  ( 181.1863822141313562, 293.5084475425986739, 6.203074340371671269 ) ) ;
#79581 = CARTESIAN_POINT ( 'NONE',  ( 173.3588497307663374, 273.3242272104048993, -16.64521848681001259 ) ) ;
#79582 = CARTESIAN_POINT ( 'NONE',  ( 196.9684447319790479, 289.4876415668271648, 17.73978044655682851 ) ) ;
#79583 = CARTESIAN_POINT ( 'NONE',  ( 81.40062866174868361, 56.12702037940537991, 16.07990521299680609 ) ) ;
#79584 = CARTESIAN_POINT ( 'NONE',  ( 13.24385365016830107, 12.81029122506292772, 8.090169943749479842 ) ) ;
#79585 = CARTESIAN_POINT ( 'NONE',  ( 187.0591251360168883, 296.0433128962568503, -7.698390371408583732 ) ) ;
#79586 = CARTESIAN_POINT ( 'NONE',  ( 66.47763888060634940, 67.99612994687967671, 6.463816603905435443 ) ) ;
#79587 = CARTESIAN_POINT ( 'NONE',  ( 87.49069069641797114, 207.9865022471901455, 1.119607411625061291E-15 ) ) ;
#79588 = CARTESIAN_POINT ( 'NONE',  ( 69.74736874176301171, 66.77905827124916982, -10.09415051326821811 ) ) ;
#79589 = CARTESIAN_POINT ( 'NONE',  ( 205.9537632452105242, 271.2264420391654198, 6.128872511909795762 ) ) ;
#79590 = CARTESIAN_POINT ( 'NONE',  ( 45.45211389745056607, 206.2369531367911293, -4.594050593750048428 ) ) ;
#79591 = CARTESIAN_POINT ( 'NONE',  ( 159.4889735931715222, 254.4039898200529706, 16.88104032092801887 ) ) ;
#79592 = VERTEX_POINT ( 'NONE', #58844 ) ;
#79593 = CARTESIAN_POINT ( 'NONE',  ( -8.440768550191725339, 84.85656262831267327, 13.91600492330110228 ) ) ;
#79594 = CARTESIAN_POINT ( 'NONE',  ( 198.7501991201633018, 286.4015524398827779, -18.58948563601804693 ) ) ;
#79595 = EDGE_CURVE ( 'NONE', #21922, #6854, #10793, .T. ) ;
#79596 = CARTESIAN_POINT ( 'NONE',  ( 32.61785165683026122, 46.50599740114041225, -10.00000000000000000 ) ) ;
#79597 = ORIENTED_EDGE ( 'NONE', *, *, #63333, .T. ) ;
#79598 = CARTESIAN_POINT ( 'NONE',  ( 72.97386446981147401, 70.68132344495336383, 8.316175787459508584 ) ) ;
#79599 = CARTESIAN_POINT ( 'NONE',  ( -5.792922669062946284, 155.9155109091896065, 2.679491924311252937 ) ) ;
#79600 = FACE_OUTER_BOUND ( 'NONE', #42887, .T. ) ;
#79601 = CARTESIAN_POINT ( 'NONE',  ( -12.95261720355844126, 24.63757726406876714, -10.00000000000000000 ) ) ;
#79602 = CARTESIAN_POINT ( 'NONE',  ( 25.06043674821822265, 32.65586893147757053, -7.433330006724137462 ) ) ;
#79603 = CARTESIAN_POINT ( 'NONE',  ( 202.9689790241539242, 279.0944113002206564, 15.85114608332523289 ) ) ;
#79604 = CARTESIAN_POINT ( 'NONE',  ( 149.6890529486499872, 271.3779502865075983, -12.51465682618088593 ) ) ;
#79605 = CARTESIAN_POINT ( 'NONE',  ( 171.3306725491475504, 255.7550868248229960, 12.09612247527935125 ) ) ;
#79606 = EDGE_LOOP ( 'NONE', ( #67979, #96978, #60612, #36726 ) ) ;
#79607 = CARTESIAN_POINT ( 'NONE',  ( 6.417452267959404821, 25.74646525600388003, 2.839279412974139660 ) ) ;
#79608 = CARTESIAN_POINT ( 'NONE',  ( 15.66239703771868719, 191.3967562850346837, -4.648177544792955347E-16 ) ) ;
#79609 = CARTESIAN_POINT ( 'NONE',  ( 71.95078207959971905, 72.63412948483367870, -0.9918729297793668076 ) ) ;
#79610 = EDGE_CURVE ( 'NONE', #25756, #55485, #96925, .T. ) ;
#79611 = ORIENTED_EDGE ( 'NONE', *, *, #70651, .T. ) ;
#79612 = CARTESIAN_POINT ( 'NONE',  ( 72.26425284656475867, 71.11905259567225812, -6.027786176564315035 ) ) ;
#79613 = CARTESIAN_POINT ( 'NONE',  ( 190.8001679306945277, 300.1714103817999444, 7.815449226872675403 ) ) ;
#79614 = EDGE_CURVE ( 'NONE', #56696, #66291, #73588, .T. ) ;
#79615 = CARTESIAN_POINT ( 'NONE',  ( -19.71336475592354986, 93.19343694228106756, 59.99999999999999289 ) ) ;
#79616 = DIRECTION ( 'NONE',  ( -0.8660254037844387076, -0.4999999999999998890, -0.000000000000000000 ) ) ;
#79617 = ORIENTED_EDGE ( 'NONE', *, *, #80161, .F. ) ;
#79618 = EDGE_LOOP ( 'NONE', ( #65364, #36102, #33527, #6290 ) ) ;
#79620 =( NAMED_UNIT ( * ) PLANE_ANGLE_UNIT ( ) SI_UNIT ( $, .RADIAN. ) );
#79619 = CARTESIAN_POINT ( 'NONE',  ( 189.6306422694777893, 274.4800867691382678, -15.80158207961506278 ) ) ;
#79621 = B_SPLINE_CURVE_WITH_KNOTS ( 'NONE', 3,
 ( #22481, #5296, #91416, #21979, #68079, #30079, #53373, #37663, #98002, #83322, #51382, #12916, #90443, #82348, #4810, #13884 ),
 .UNSPECIFIED., .F., .F.,
 ( 4, 2, 2, 2, 2, 2, 2, 4 ),
 ( 0.000000000000000000, 0.0005379944778325431451, 0.0008069917167488165066, 0.001075988955665089977, 0.001344986194581363446, 0.001613983433497636916, 0.001882980672413910386, 0.002151977911330183856 ),
 .UNSPECIFIED. ) ;
#79622 = VERTEX_POINT ( 'NONE', #49288 ) ;
#79623 = CARTESIAN_POINT ( 'NONE',  ( 152.7691010214056462, 266.0431505347400503, -16.40662330462167162 ) ) ;
#79624 = CARTESIAN_POINT ( 'NONE',  ( 48.98007068238331385, 88.97864505566217019, -10.00000000000000000 ) ) ;
#79625 = CARTESIAN_POINT ( 'NONE',  ( 73.10654890674743456, 57.42163371433187535, -15.88130622537231673 ) ) ;
#79626 = CARTESIAN_POINT ( 'NONE',  ( 76.98684284838461167, 63.68060895951392553, 15.36346902396294745 ) ) ;
#79627 = CARTESIAN_POINT ( 'NONE',  ( 204.7764732025852084, 275.9637395487929439, -14.02287343454361412 ) ) ;
#79628 = CARTESIAN_POINT ( 'NONE',  ( 105.9656389868882513, 241.1744531367911577, 4.594050593750047540 ) ) ;
#79629 = CARTESIAN_POINT ( 'NONE',  ( 181.0301937916765667, 287.8052501752913486, -14.12606483171538052 ) ) ;
#79630 = ORIENTED_EDGE ( 'NONE', *, *, #64053, .F. ) ;
#79631 = CARTESIAN_POINT ( 'NONE',  ( 161.7844122638997533, 267.0814880858553124, 16.49944467494395894 ) ) ;
#79632 = VERTEX_POINT ( 'NONE', #89812 ) ;
#79633 = CARTESIAN_POINT ( 'NONE',  ( 34.35336353842534152, 22.76004757982091320, 5.678558825948272215 ) ) ;
#79634 = CARTESIAN_POINT ( 'NONE',  ( 197.9002057575219453, 287.8737841300738296, 18.01270164875645818 ) ) ;
#79635 = CARTESIAN_POINT ( 'NONE',  ( 78.24597377814070853, 47.77139718876669860, -14.49689961856089759 ) ) ;
#79636 = CARTESIAN_POINT ( 'NONE',  ( 47.26526781268299260, 210.3464784336661637, 1.353441290958777525E-15 ) ) ;
#79637 = CARTESIAN_POINT ( 'NONE',  ( 73.86986929274216607, 68.54753403896816621, 11.39714278534123437 ) ) ;
#79638 = CARTESIAN_POINT ( 'NONE',  ( 150.6655900823359389, 269.6865383554857090, 15.31288044136207205 ) ) ;
#79639 = CARTESIAN_POINT ( 'NONE',  ( 198.0167861310041530, 287.6718610000373246, 18.15276047493383160 ) ) ;
#79640 = CARTESIAN_POINT ( 'NONE',  ( 176.4464654933624104, 273.1633176496665101, 16.93181923922713494 ) ) ;
#79641 = ORIENTED_EDGE ( 'NONE', *, *, #16463, .F. ) ;
#79642 = EDGE_CURVE ( 'NONE', #88756, #85510, #83449, .T. ) ;
#79643 = CARTESIAN_POINT ( 'NONE',  ( 81.45669997382150029, 55.98862135975878118, -16.04303691645969820 ) ) ;
#79644 = CARTESIAN_POINT ( 'NONE',  ( 178.0221171495884676, 288.7633432952653152, 10.91361327765725342 ) ) ;
#79645 = CARTESIAN_POINT ( 'NONE',  ( 78.49844431995686023, 56.32831885670888994, 16.60005998789102577 ) ) ;
#79646 = VERTEX_POINT ( 'NONE', #82222 ) ;
#79647 = CARTESIAN_POINT ( 'NONE',  ( 172.2516114191509189, 258.4199449647830420, -14.42867330110744462 ) ) ;
#79648 = CARTESIAN_POINT ( 'NONE',  ( 67.75753012590708124, 69.25273034730335553, -3.573886548774661165 ) ) ;
#79649 = CARTESIAN_POINT ( 'NONE',  ( 207.1158949475991164, 271.9117422260973740, -5.823035679195911918 ) ) ;
#79650 = CARTESIAN_POINT ( 'NONE',  ( 206.7474862253485526, 270.1292977026819813, 1.793960490934114471 ) ) ;
#79651 = EDGE_CURVE ( 'NONE', #6303, #29146, #27963, .T. ) ;
#79652 = ADVANCED_FACE ( 'NONE', ( #64988 ), #11311, .T. ) ;
#79653 = CARTESIAN_POINT ( 'NONE',  ( 149.5633513747893346, 271.5956717990251832, 12.83777201928511325 ) ) ;
#79654 = CARTESIAN_POINT ( 'NONE',  ( 180.6100108800816599, 271.2853514182555728, 16.55563358471784596 ) ) ;
#79655 = CARTESIAN_POINT ( 'NONE',  ( 156.6812872898450735, 261.2670451491295012, 0.000000000000000000 ) ) ;
#79656 = DIRECTION ( 'NONE',  ( -0.9506327454577400138, -0.3103181967972222788, 0.000000000000000000 ) ) ;
#79657 = CARTESIAN_POINT ( 'NONE',  ( 165.3419214322780135, 255.1043459237804996, 13.90808614669940901 ) ) ;
#79658 = DIRECTION ( 'NONE',  ( 1.000000000000000000, 0.000000000000000000, 0.000000000000000000 ) ) ;
#79659 = ADVANCED_FACE ( 'NONE', ( #34098 ), #85530, .F. ) ;
#79660 = CARTESIAN_POINT ( 'NONE',  ( 119.9849458542963561, 230.8923013555409796, 4.594050593750050204 ) ) ;
#79661 = VERTEX_POINT ( 'NONE', #45154 ) ;
#79662 = CARTESIAN_POINT ( 'NONE',  ( 191.3041230083617563, 299.2985345825480863, -9.819045872446528378 ) ) ;
#79663 = FACE_OUTER_BOUND ( 'NONE', #4180, .T. ) ;
#79664 = EDGE_CURVE ( 'NONE', #44895, #27272, #28461, .T. ) ;
#79665 = DIRECTION ( 'NONE',  ( 0.8653701635463924013, -0.5011331959107180323, 0.000000000000000000 ) ) ;
#79666 = CARTESIAN_POINT ( 'NONE',  ( 28.46864935082047410, 149.7156766241961350, 37.50000000000000000 ) ) ;
#79667 = CARTESIAN_POINT ( 'NONE',  ( 83.91646131505093820, 51.73966832772509861, -14.43249324666324895 ) ) ;
#79668 = CARTESIAN_POINT ( 'NONE',  ( 177.6813079280251202, 255.2054228243137004, 4.880324467531951704 ) ) ;
#79669 = VERTEX_POINT ( 'NONE', #21371 ) ;
#79670 = CARTESIAN_POINT ( 'NONE',  ( 80.61962873213096259, 57.61924663962614090, -16.24249425847791173 ) ) ;
#79671 = CARTESIAN_POINT ( 'NONE',  ( 154.6163025329676088, 273.5610833407037035, -13.37509610506471702 ) ) ;
#79673 = CARTESIAN_POINT ( 'NONE',  ( 71.96464922262767061, 71.55750601381073750, 5.589292941210060484 ) ) ;
#79672 = CARTESIAN_POINT ( 'NONE',  ( 72.44020731426283533, 70.76712560363094440, 7.696415609646552802 ) ) ;
#79674 = CARTESIAN_POINT ( 'NONE',  ( 164.4118148411678817, 245.8773786609274623, -1.109947685176164045 ) ) ;
#79675 = CARTESIAN_POINT ( 'NONE',  ( -22.03161396778968140, 40.09437670360522077, 59.99999999999999289 ) ) ;
#79676 = CARTESIAN_POINT ( 'NONE',  ( 198.7829547491859330, 286.3448180261817129, -18.59838968157616179 ) ) ;
#79677 = DIRECTION ( 'NONE',  ( 0.4999999999999992784, -0.8660254037844390407, 0.000000000000000000 ) ) ;
#79678 = CARTESIAN_POINT ( 'NONE',  ( 190.7685386727469279, 298.2261938635710976, -9.678376712886644029 ) ) ;
#79679 = CARTESIAN_POINT ( 'NONE',  ( 64.42391676880970408, 201.8768266524159856, -9.188101187500091527 ) ) ;
#79680 = AXIS2_PLACEMENT_3D ( 'NONE', #20660, #51549, #28244 ) ;
#79681 = CARTESIAN_POINT ( 'NONE',  ( 164.9586510554008782, 244.9302305544571823, -1.717556444319656039 ) ) ;
#79682 = CARTESIAN_POINT ( 'NONE',  ( 193.8354046899084153, 268.4885937380259406, 12.87375928640720524 ) ) ;
#79683 = B_SPLINE_SURFACE_WITH_KNOTS ( 'NONE', 3, 1, ( 
 ( #87291, #47690 ),
 ( #17822, #48723 ),
 ( #85776, #23897 ),
 ( #62902, #64411 ),
 ( #10219, #47198 ),
 ( #86768, #41087 ),
 ( #39579, #78625 ),
 ( #93854, #49220 ),
 ( #24409, #33515 ),
 ( #79154, #95374 ),
 ( #56799, #70500 ),
 ( #1631, #87784 ),
 ( #41594, #86265 ),
 ( #610, #8710 ),
 ( #31492, #62384 ),
 ( #55285, #16803 ),
 ( #9211, #93341 ),
 ( #32515, #80655 ),
 ( #35499, #89271 ),
 ( #52557, #44960 ),
 ( #43075, #73517 ),
 ( #11234, #64915 ),
 ( #88770, #65404 ),
 ( #97329, #34028 ),
 ( #65894, #57297 ),
 ( #22171, #42098 ),
 ( #73031, #4100 ),
 ( #83513, #95860 ),
 ( #66401, #68259 ),
 ( #96850, #27417 ),
 ( #19820, #50690 ),
 ( #99184, #34502 ),
 ( #91111, #29283 ),
 ( #96345, #37358 ) ),
 .UNSPECIFIED., .T., .F., .F.,
 ( 4, 2, 2, 2, 2, 2, 2, 2, 2, 2, 2, 2, 2, 2, 2, 2, 4 ),
 ( 2, 2 ),
 ( 0.000000000000000000, 0.06250000000000000000, 0.1250000000000000000, 0.1875000000000000000, 0.2500000000000000000, 0.3125000000000000000, 0.3750000000000000000, 0.4375000000000000000, 0.5000000000000000000, 0.5625000000000000000, 0.6250000000000000000, 0.6875000000000000000, 0.7500000000000000000, 0.8125000000000000000, 0.8750000000000000000, 0.9375000000000000000, 1.000000000000000000 ),
 ( 0.000000000000000000, 1.000000000000000000 ),
 .UNSPECIFIED. ) ;
#79684 = CARTESIAN_POINT ( 'NONE',  ( 80.01034338638787347, 44.43011396636085664, -11.60714397506079720 ) ) ;
#79685 = CARTESIAN_POINT ( 'NONE',  ( 174.8968804999455244, 261.5766033592863096, 14.34024671999864964 ) ) ;
#79686 = CARTESIAN_POINT ( 'NONE',  ( 155.1231266014676180, 279.5326577215706152, -1.580077478444769534 ) ) ;
#79687 = FACE_OUTER_BOUND ( 'NONE', #64521, .T. ) ;
#79688 = CARTESIAN_POINT ( 'NONE',  ( 155.4661767250933622, 261.3716783840932294, -17.10192542004562810 ) ) ;
#79689 = CARTESIAN_POINT ( 'NONE',  ( 193.5197837783914281, 288.6179979435178211, 16.03724552212410970 ) ) ;
#79690 = CARTESIAN_POINT ( 'NONE',  ( 129.4748805805031395, 238.8927522451418781, 10.00000000000009592 ) ) ;
#79691 = CARTESIAN_POINT ( 'NONE',  ( 81.21734643817387678, 51.70401989366683893, -14.96604167157805598 ) ) ;
#79692 = VERTEX_POINT ( 'NONE', #75575 ) ;
#79693 = EDGE_CURVE ( 'NONE', #59645, #75836, #10947, .T. ) ;
#79694 = CARTESIAN_POINT ( 'NONE',  ( 189.8171280724701546, 301.8740853621098950, -0.4360232994423257624 ) ) ;
#79695 = CARTESIAN_POINT ( 'NONE',  ( -16.90171517502901466, 170.2369531367911293, -4.594050593750048428 ) ) ;
#79696 = CARTESIAN_POINT ( 'NONE',  ( 46.72434903108273119, 197.7833772461660828, -9.188101187500095079 ) ) ;
#79697 = CARTESIAN_POINT ( 'NONE',  ( 15.66455532895297331, 30.81751292744056059, -6.180339887498951690 ) ) ;
#79698 = CARTESIAN_POINT ( 'NONE',  ( 138.1418008908465822, 79.75620593067000641, 17.47570218321536117 ) ) ;
#79699 = CARTESIAN_POINT ( 'NONE',  ( 85.33699565288863198, 48.33901173460944278, -12.30238903177781395 ) ) ;
#79700 = CARTESIAN_POINT ( 'NONE',  ( 190.9335643195044838, 299.9403610588350944, -4.692880224846124548 ) ) ;
#79701 = CARTESIAN_POINT ( 'NONE',  ( 45.60499120716188060, 26.73415679381826138, -6.890680421881970419E-14 ) ) ;
#79703 = CARTESIAN_POINT ( 'NONE',  ( 56.65657787896151376, 213.5177522451419065, 5.000000000000046185 ) ) ;
#79702 = CARTESIAN_POINT ( 'NONE',  ( 195.8285188278500470, 273.2427770020486832, 15.26130794574777383 ) ) ;
#79704 = CARTESIAN_POINT ( 'NONE',  ( 9.667034506031535912, 13.78052372038638396, -10.00000000000000355 ) ) ;
#79705 = CARTESIAN_POINT ( 'NONE',  ( 180.8537919486467160, 256.3066541963624445, 1.346842808816189452 ) ) ;
#79706 = CARTESIAN_POINT ( 'NONE',  ( 205.3704330671644414, 274.9349708856848338, -13.01557521325596944 ) ) ;
#79707 = CARTESIAN_POINT ( 'NONE',  ( 162.1316038200447736, 252.0640768520765960, -13.69825752773376770 ) ) ;
#79708 = CARTESIAN_POINT ( 'NONE',  ( 179.2389850949382151, 294.6081512498237771, 1.073768896970125786 ) ) ;
#79709 = CARTESIAN_POINT ( 'NONE',  ( 49.89075441544358824, 189.6115022471902023, -5.000000000000041744 ) ) ;
#79710 = CARTESIAN_POINT ( 'NONE',  ( 150.8371008641169908, 248.7048013555409511, 4.594050593750051981 ) ) ;
#79711 = CARTESIAN_POINT ( 'NONE',  ( 202.4943568615953779, 279.9164810001701085, 17.09064351659286984 ) ) ;
#79712 = CARTESIAN_POINT ( 'NONE',  ( 2.773212693257451900, 184.6589784336661637, -6.496448406907675876E-16 ) ) ;
#79713 = CARTESIAN_POINT ( 'NONE',  ( 36.84800447571193160, 26.98920272979929180, 7.433330006724137462 ) ) ;
#79715 = FACE_OUTER_BOUND ( 'NONE', #39671, .T. ) ;
#79714 = DIRECTION ( 'NONE',  ( 0.3887219701523905169, 0.9213551052231946370, 0.000000000000000000 ) ) ;
#79716 = CARTESIAN_POINT ( 'NONE',  ( 152.7618747630824885, 266.0556667813044101, 16.41480086888796919 ) ) ;
#79717 = CARTESIAN_POINT ( 'NONE',  ( 27.04628097738780212, 27.56628583063842086, 9.188101187500006262 ) ) ;
#79718 = CARTESIAN_POINT ( 'NONE',  ( 156.3551087084618700, 261.3239775484371989, -17.56576820129662053 ) ) ;
#79719 = EDGE_CURVE ( 'NONE', #90599, #66772, #84705, .T. ) ;
#79720 = CARTESIAN_POINT ( 'NONE',  ( 186.8774594610050599, 259.3182782412434335, -2.380209424388837647 ) ) ;
#79721 = LINE ( 'NONE', #19884, #23859 ) ;
#79722 = CARTESIAN_POINT ( 'NONE',  ( 43.27754793094329244, 25.39040679176986970, -6.890680421881970419E-14 ) ) ;
#79723 = CARTESIAN_POINT ( 'NONE',  ( 181.7505021599577333, 256.6548486136064753, -6.673752474138594515 ) ) ;
#79724 = CARTESIAN_POINT ( 'NONE',  ( 12.38457448260035143, 9.011106405272903075, 2.839279412974134775 ) ) ;
#79725 = CARTESIAN_POINT ( 'NONE',  ( 166.3255300953076414, 285.8001061038755779, 0.4975669204057207584 ) ) ;
#79726 = CARTESIAN_POINT ( 'NONE',  ( 18.23327619575285041, 19.03085787977761711, 9.188101187500006262 ) ) ;
#79727 = CARTESIAN_POINT ( 'NONE',  ( 11.76667899187106059, 31.90941714274742225, 10.00000000000000000 ) ) ;
#79728 = CARTESIAN_POINT ( 'NONE',  ( 153.0911466228407392, 274.9737743950042841, 10.66320493477942044 ) ) ;
#79729 = CARTESIAN_POINT ( 'NONE',  ( 87.86832398745416128, 44.01541417138756884, -1.805110452858952552 ) ) ;
#79730 = CARTESIAN_POINT ( 'NONE',  ( 54.63354020801843092, 213.8967562850347122, -4.648177544792955347E-16 ) ) ;
#79731 = ADVANCED_FACE ( 'NONE', ( #69453 ), #39034, .T. ) ;
#79732 = ORIENTED_EDGE ( 'NONE', *, *, #52985, .F. ) ;
#79733 = CARTESIAN_POINT ( 'NONE',  ( 152.9920137376499838, 265.6570543845515431, 16.15798175643282164 ) ) ;
#79734 = CARTESIAN_POINT ( 'NONE',  ( 165.0156970625405108, 244.8314239717225007, -1.890480716182876719 ) ) ;
#79735 = CARTESIAN_POINT ( 'NONE',  ( 47.84007798744509898, 106.1754093786579318, 10.00000000000000000 ) ) ;
#79736 = EDGE_CURVE ( 'NONE', #81147, #30467, #14518, .T. ) ;
#79737 = CARTESIAN_POINT ( 'NONE',  ( 87.39182636385071135, 45.50004596871073659, 7.088608641304300129 ) ) ;
#79738 = CARTESIAN_POINT ( 'NONE',  ( 155.5660013421004919, 261.1987770755905558, 17.28709111629370199 ) ) ;
#79739 = ORIENTED_EDGE ( 'NONE', *, *, #43374, .T. ) ;
#79740 = ORIENTED_EDGE ( 'NONE', *, *, #78752, .T. ) ;
#79741 = DIRECTION ( 'NONE',  ( 0.000000000000000000, 0.000000000000000000, 1.000000000000000000 ) ) ;
#79742 = CARTESIAN_POINT ( 'NONE',  ( 86.37991722458738764, 47.25272401055813276, 10.79753792097408116 ) ) ;
#79743 = EDGE_LOOP ( 'NONE', ( #14908, #97783, #86389, #74445 ) ) ;
#79744 = CARTESIAN_POINT ( 'NONE',  ( 76.48640248419295062, 51.58918322513654431, 15.64831315713033355 ) ) ;
#79745 = DIRECTION ( 'NONE',  ( -0.7510153523339188064, 0.6602847420308604054, 0.000000000000000000 ) ) ;
#79746 = VERTEX_POINT ( 'NONE', #73964 ) ;
#79747 = CARTESIAN_POINT ( 'NONE',  ( 78.39991307920188035, 61.32441222751918986, -15.87033061864282324 ) ) ;
#79748 = CARTESIAN_POINT ( 'NONE',  ( 79.26974131400611157, 59.52036692680491115, -16.53359576550787224 ) ) ;
#79750 = VECTOR ( 'NONE', #50057, 1000.000000000000000 ) ;
#79749 = CARTESIAN_POINT ( 'NONE',  ( 12.79584618246493477, 29.16126292948894516, -6.180339887498951690 ) ) ;
#79751 = ORIENTED_EDGE ( 'NONE', *, *, #30786, .F. ) ;
#79752 = CARTESIAN_POINT ( 'NONE',  ( 200.6800100461949228, 283.0590218669948399, 18.32402613046234308 ) ) ;
#79753 = CARTESIAN_POINT ( 'NONE',  ( 169.1532419530282141, 276.3814789465369586, -16.13320117031923573 ) ) ;
#79754 = CARTESIAN_POINT ( 'NONE',  ( -24.63924516542741827, 141.7012482093459198, 37.49999999999996447 ) ) ;
#79755 = CARTESIAN_POINT ( 'NONE',  ( 29.87413333957346140, 40.18080186712595747, 3.090169943749475401 ) ) ;
#79756 = ORIENTED_EDGE ( 'NONE', *, *, #82136, .T. ) ;
#79757 = DIRECTION ( 'NONE',  ( -0.8660254037844387076, -0.4999999999999998890, -0.000000000000000000 ) ) ;
#79758 = CARTESIAN_POINT ( 'NONE',  ( 32.96252748593624915, 42.52903772873360566, -1.583844403245329602 ) ) ;
#79759 = AXIS2_PLACEMENT_3D ( 'NONE', #9289, #24482, #39654 ) ;
#79760 = ORIENTED_EDGE ( 'NONE', *, *, #91287, .T. ) ;
#79761 = ORIENTED_EDGE ( 'NONE', *, *, #92568, .F. ) ;
#79762 = LINE ( 'NONE', #10327, #72541 ) ;
#79763 = VERTEX_POINT ( 'NONE', #17771 ) ;
#79764 = DIRECTION ( 'NONE',  ( -0.3978777116982094575, -0.7304723483372487225, 0.5550706935593536784 ) ) ;
#79765 = VERTEX_POINT ( 'NONE', #87734 ) ;
#79766 = ADVANCED_FACE ( 'NONE', ( #12162 ), #97285, .T. ) ;
#79767 = CARTESIAN_POINT ( 'NONE',  ( 159.1165150567399280, 259.5332163835566917, 16.70623555518022840 ) ) ;
#79768 = CARTESIAN_POINT ( 'NONE',  ( 194.0370204994606524, 294.5650172760874170, 14.49136610471935604 ) ) ;
#79769 = CARTESIAN_POINT ( 'NONE',  ( 177.5977857591645090, 289.0201305223690156, -9.328731151047037429 ) ) ;
#79770 = CARTESIAN_POINT ( 'NONE',  ( 69.20971128213882650, 64.50273501078117988, 11.88834065357228731 ) ) ;
#79771 = LINE ( 'NONE', #10831, #25867 ) ;
#79772 = CARTESIAN_POINT ( 'NONE',  ( 174.5517021171108638, 290.1645060665484266, 6.371634131280785596 ) ) ;
#79773 = CARTESIAN_POINT ( 'NONE',  ( 79.14312167556931854, 57.64441083166269664, 0.000000000000000000 ) ) ;
#79774 = VERTEX_POINT ( 'NONE', #66351 ) ;
#79775 = CARTESIAN_POINT ( 'NONE',  ( 165.0952264510788154, 281.4963861521250124, -11.84807672454148886 ) ) ;
#79776 = CARTESIAN_POINT ( 'NONE',  ( 17.01121839442928163, 30.79752408145592568, -5.678558825948271327 ) ) ;
#79777 = CARTESIAN_POINT ( 'NONE',  ( 164.3754245770190039, 245.9404084473339083, 1.667926061651832992 ) ) ;
#79778 = CARTESIAN_POINT ( 'NONE',  ( 206.4768661561222984, 273.0185725604343361, 11.39716120335626925 ) ) ;
#79780 = ORIENTED_EDGE ( 'NONE', *, *, #41389, .T. ) ;
#79779 = CARTESIAN_POINT ( 'NONE',  ( 159.6610344727618269, 254.1059716346071866, 15.33388637456589620 ) ) ;
#79781 = VERTEX_POINT ( 'NONE', #65353 ) ;
#79782 = CARTESIAN_POINT ( 'NONE',  ( 190.5278607951618710, 300.6430601758063403, 5.309934257482836095 ) ) ;
#79783 = CARTESIAN_POINT ( 'NONE',  ( 81.19243458941035385, 52.42165318742301139, -15.24367534770689225 ) ) ;
#79784 = EDGE_CURVE ( 'NONE', #64892, #83079, #33461, .T. ) ;
#79785 = CARTESIAN_POINT ( 'NONE',  ( 36.44916501977947831, 42.81751292744058901, -6.180339887498951690 ) ) ;
#79786 = CARTESIAN_POINT ( 'NONE',  ( -69.61464189717713680, 45.83092310410447112, -10.00000000000000000 ) ) ;
#79787 = CARTESIAN_POINT ( 'NONE',  ( 200.6129772034685175, 283.1751261563724142, 18.36811917402039640 ) ) ;
#79788 = CARTESIAN_POINT ( 'NONE',  ( 190.7970923485466699, 261.9842811066119452, -0.6382846533130664968 ) ) ;
#79789 = ORIENTED_EDGE ( 'NONE', *, *, #44241, .T. ) ;
#79790 = LINE ( 'NONE', #33658, #83471 ) ;
#79791 = FACE_OUTER_BOUND ( 'NONE', #83574, .T. ) ;
#79792 = DIRECTION ( 'NONE',  ( -0.8660254037844378194, -0.5000000000000013323, -0.000000000000000000 ) ) ;
#79793 = CARTESIAN_POINT ( 'NONE',  ( -5.997209913151932525, 43.16835788936899831, 59.99999999999999289 ) ) ;
#79794 = CARTESIAN_POINT ( 'NONE',  ( 11.55108809852201013, 184.1427522451419350, 10.00000000000009237 ) ) ;
#79795 = CARTESIAN_POINT ( 'NONE',  ( 100.7969837277561282, 222.8768266524159856, -9.188101187500093303 ) ) ;
#79796 = FACE_OUTER_BOUND ( 'NONE', #25383, .T. ) ;
#79797 = CARTESIAN_POINT ( 'NONE',  ( 197.4842693130445923, 286.5942071846287149, -17.75505217046438489 ) ) ;
#79798 = CARTESIAN_POINT ( 'NONE',  ( 167.0636792507274322, 277.9578970009563932, -14.05280382147244644 ) ) ;
#79799 = ADVANCED_FACE ( 'NONE', ( #26861 ), #70094, .F. ) ;
#79800 = CARTESIAN_POINT ( 'NONE',  ( 18.84898279888859918, 187.8149278399161233, 9.188101187500093303 ) ) ;
#79801 = CARTESIAN_POINT ( 'NONE',  ( 174.6617384230121104, 289.1922761299584863, -9.320811169396549190 ) ) ;
#79802 = ORIENTED_EDGE ( 'NONE', *, *, #40418, .T. ) ;
#79804 = ORIENTED_EDGE ( 'NONE', *, *, #64033, .T. ) ;
#79803 = UNCERTAINTY_MEASURE_WITH_UNIT (LENGTH_MEASURE( 1.000000000000000082E-05 ), #80219, 'distance_accuracy_value', 'NONE');
#79805 = CARTESIAN_POINT ( 'NONE',  ( 200.8942821848932851, 267.7847592425025027, -2.908898627582254370 ) ) ;
#79806 = CARTESIAN_POINT ( 'NONE',  ( 68.57836289805518959, 70.07438557745322782, 1.916984831344509699 ) ) ;
#79807 = CARTESIAN_POINT ( 'NONE',  ( 81.96547941067910870, 41.17040324926905015, 3.814626384468428721 ) ) ;
#79808 = CARTESIAN_POINT ( 'NONE',  ( 205.4334751569798811, 272.0530277678294624, -9.567426915989852176 ) ) ;
#79809 = CARTESIAN_POINT ( 'NONE',  ( 207.4218731373931632, 271.3817724553659332, -5.249531240730909154 ) ) ;
#79810 =( BOUNDED_CURVE ( )  B_SPLINE_CURVE ( 2, ( #47375, #87954, #2812, #94026, #71204, #777, #2304, #10396, #49385 ),
 .UNSPECIFIED., .F., .T. ) 
 B_SPLINE_CURVE_WITH_KNOTS ( ( 3, 2, 2, 2, 3 ),
 ( 0.1572580645161290314, 0.1586021505376344065, 0.1612903225806451568, 0.1639784946236559071, 0.1653225806451612823 ),
 .UNSPECIFIED. ) 
 CURVE ( )  GEOMETRIC_REPRESENTATION_ITEM ( )  RATIONAL_B_SPLINE_CURVE ( ( 0.9330127018922194093, 0.9330127018922194093, 1.000000000000000000, 0.8660254037844387076, 1.000000000000000000, 0.8660254037844387076, 1.000000000000000000, 0.9330127018922194093, 0.9330127018922194093 ) ) 
 REPRESENTATION_ITEM ( '' )  );
#79811 = CARTESIAN_POINT ( 'NONE',  ( 182.7656509685662343, 284.3849974448608577, 14.96600143269570182 ) ) ;
#79812 = CARTESIAN_POINT ( 'NONE',  ( 74.31626339567910122, 68.46754964620755857, -11.19101123510062301 ) ) ;
#79813 = CARTESIAN_POINT ( 'NONE',  ( 40.98727782677583065, 182.2202760586659451, -5.415160957724236172E-17 ) ) ;
#79814 = ORIENTED_EDGE ( 'NONE', *, *, #69136, .F. ) ;
#79815 = CARTESIAN_POINT ( 'NONE',  ( 79.18418104304701899, 60.10533407485776536, -16.47260471942688653 ) ) ;
#79816 = CARTESIAN_POINT ( 'NONE',  ( 179.4361089452441433, 259.6094657833778001, -10.31148828265781603 ) ) ;
#79817 = CARTESIAN_POINT ( 'NONE',  ( -3.938137090306929711, 168.5333772461660828, 9.188101187500095079 ) ) ;
#79818 = CARTESIAN_POINT ( 'NONE',  ( 68.49197605392033950, 64.33996568623787482, -12.33092966291259174 ) ) ;
#79819 = CARTESIAN_POINT ( 'NONE',  ( 198.9832789858017463, 285.9978462703757600, -18.55676541969546278 ) ) ;
#79820 = FACE_OUTER_BOUND ( 'NONE', #92108, .T. ) ;
#79821 = AXIS2_PLACEMENT_3D ( 'NONE', #63465, #33063, #78682 ) ;
#79822 = CARTESIAN_POINT ( 'NONE',  ( 66.90909321525144549, 68.17756947874360662, -6.600776075497404527 ) ) ;
#79823 = CARTESIAN_POINT ( 'NONE',  ( 163.7064929935861244, 247.0990319366274548, 6.401263337036986023 ) ) ;
#79824 = CARTESIAN_POINT ( 'NONE',  ( 146.5865263025993954, 276.7516840693029962, 0.4918294119671828835 ) ) ;
#79825 = CARTESIAN_POINT ( 'NONE',  ( 164.3524132573224392, 245.9802652221976587, -2.749586949851067441 ) ) ;
#79826 = EDGE_LOOP ( 'NONE', ( #17908, #49810, #86644, #69209 ) ) ;
#79827 = CARTESIAN_POINT ( 'NONE',  ( 148.2390246527636748, 247.2048013555409511, 4.594050593750051981 ) ) ;
#79828 = CARTESIAN_POINT ( 'NONE',  ( 181.3453648331101817, 267.8634245393459423, 16.44187752845164141 ) ) ;
#79829 = CARTESIAN_POINT ( 'NONE',  ( 106.4801018922090066, 232.2833772461660544, -9.188101187500095079 ) ) ;
#79830 = CARTESIAN_POINT ( 'NONE',  ( 13.87187630571069263, 28.98502408145591502, -5.678558825948271327 ) ) ;
#79831 = B_SPLINE_CURVE_WITH_KNOTS ( 'NONE', 3,
 ( #76780, #4510, #51614, #35905, #92036, #59180, #97733, #20728, #58692, #82065, #81072, #12124, #5024, #66805, #50603, #6879 ),
 .UNSPECIFIED., .F., .F.,
 ( 4, 1, 2, 2, 2, 1, 2, 2, 4 ),
 ( 0.000000000000000000, 0.1250000000000001388, 0.1875000000000002220, 0.2500000000000002776, 0.5000000000000001110, 0.6249999999999991118, 0.6874999999999985567, 0.7499999999999978906, 1.000000000000000000 ),
 .UNSPECIFIED. ) ;
#79832 = CARTESIAN_POINT ( 'NONE',  ( 75.22447641198338886, 66.97122069168695191, 13.23119059164782030 ) ) ;
#79833 = DIRECTION ( 'NONE',  ( -1.000000000000000000, -9.785293164094327883E-14, 0.000000000000000000 ) ) ;
#79834 = VECTOR ( 'NONE', #84093, 1000.000000000000227 ) ;
#79836 = DIRECTION ( 'NONE',  ( -1.000000000000000000, 0.000000000000000000, 0.000000000000000000 ) ) ;
#79835 = CARTESIAN_POINT ( 'NONE',  ( 157.1135969804030310, 258.5182628004787944, 17.19660297500358226 ) ) ;
#79837 = CARTESIAN_POINT ( 'NONE',  ( 150.4620166971273534, 270.0391378017355919, -15.22190817129291673 ) ) ;
#79838 = VERTEX_POINT ( 'NONE', #6044 ) ;
#79839 = CARTESIAN_POINT ( 'NONE',  ( 192.9140677929238166, 263.8636187812822982, -4.540140315059590925 ) ) ;
#79840 = CARTESIAN_POINT ( 'NONE',  ( 196.4501996009505831, 290.3852684645433442, -17.82325615854289680 ) ) ;
#79841 = CARTESIAN_POINT ( 'NONE',  ( 189.7709616952058695, 300.0996391715700611, 4.806025422203243025 ) ) ;
#79842 = CARTESIAN_POINT ( 'NONE',  ( 173.4032705993685965, 289.8532102436319633, -1.071672375802585675 ) ) ;
#79843 = CARTESIAN_POINT ( 'NONE',  ( 81.57862098688173091, 55.52127002482139062, -16.32346926850663493 ) ) ;
#79844 = ORIENTED_EDGE ( 'NONE', *, *, #20682, .T. ) ;
#79845 = CARTESIAN_POINT ( 'NONE',  ( 71.77426126090318803, 65.60551381397631587, -12.81782449613754515 ) ) ;
#79846 = CARTESIAN_POINT ( 'NONE',  ( 175.0839093973710305, 279.4057055686774902, 15.99633660845799987 ) ) ;
#79847 = CARTESIAN_POINT ( 'NONE',  ( 191.9986677257686836, 264.8169910582080888, -10.25568683636180189 ) ) ;
#79848 = CARTESIAN_POINT ( 'NONE',  ( 71.96242732416023102, 72.61395932958829746, 1.324942441655030834 ) ) ;
#79849 = EDGE_CURVE ( 'NONE', #93478, #38611, #68812, .T. ) ;
#79850 = CARTESIAN_POINT ( 'NONE',  ( 80.23209172613701412, 54.97481774069060378, 15.95603643075370748 ) ) ;
#79851 = CARTESIAN_POINT ( 'NONE',  ( 83.55710330194072810, 51.48266744151908370, -14.41134322998550310 ) ) ;
#79852 = EDGE_CURVE ( 'NONE', #67548, #44339, #24203, .T. ) ;
#79853 = CARTESIAN_POINT ( 'NONE',  ( 71.96639307748559133, 71.49757472301890004, -5.734781593071435424 ) ) ;
#79854 = CARTESIAN_POINT ( 'NONE',  ( 148.6023484834014425, 275.2601776331305814, 7.517535991345212665 ) ) ;
#79855 = VERTEX_POINT ( 'NONE', #10934 ) ;
#79856 = CARTESIAN_POINT ( 'NONE',  ( 86.46048006423905008, 47.32182001325401188, 10.26516935212321968 ) ) ;
#79857 = EDGE_CURVE ( 'NONE', #10835, #1376, #69401, .T. ) ;
#79858 = CARTESIAN_POINT ( 'NONE',  ( 40.57792791151964451, 35.37878583063844218, 9.188101187500006262 ) ) ;
#79859 = CARTESIAN_POINT ( 'NONE',  ( 194.7451511902013124, 289.8320772759159354, -16.28529254116144287 ) ) ;
#79860 = ORIENTED_EDGE ( 'NONE', *, *, #2646, .T. ) ;
#79861 = CARTESIAN_POINT ( 'NONE',  ( 77.74340892523753155, 61.62887588481113710, 16.08014808546132102 ) ) ;
#79862 = EDGE_CURVE ( 'NONE', #34753, #87476, #78585, .T. ) ;
#79863 = CARTESIAN_POINT ( 'NONE',  ( 194.3442947553755005, 294.0328026529847421, -15.97648891113594871 ) ) ;
#79864 = CYLINDRICAL_SURFACE ( 'NONE', #67811, 17.82106496071139645 ) ;
#79865 = VERTEX_POINT ( 'NONE', #87499 ) ;
#79866 = CARTESIAN_POINT ( 'NONE',  ( 78.90607854399013377, 60.09749198675558546, 16.11258120454802523 ) ) ;
#79867 = CARTESIAN_POINT ( 'NONE',  ( 187.2435932563332415, 292.1887571869974636, 12.29041050614439001 ) ) ;
#79868 = CARTESIAN_POINT ( 'NONE',  ( 191.4685399627163633, 299.0137560639802814, 7.545791216288330716 ) ) ;
#79869 = DIRECTION ( 'NONE',  ( 0.5000000000000014433, -0.8660254037844378194, 0.000000000000000000 ) ) ;
#79870 = B_SPLINE_CURVE_WITH_KNOTS ( 'NONE', 3,
 ( #33349, #19670, #41435, #72376 ),
 .UNSPECIFIED., .F., .F.,
 ( 4, 4 ),
 ( 0.8924449491999673079, 1.000000000000000000 ),
 .UNSPECIFIED. ) ;
#79871 = CARTESIAN_POINT ( 'NONE',  ( 80.53677833458100110, 44.48879437267268599, 11.38558430043868697 ) ) ;
#79872 = CARTESIAN_POINT ( 'NONE',  ( 84.79995857201339504, 49.88899232450376786, -13.17356253177934455 ) ) ;
#79873 = CARTESIAN_POINT ( 'NONE',  ( 202.9881971861223917, 279.0611244672630278, -15.16231470264511927 ) ) ;
#79874 = VERTEX_POINT ( 'NONE', #80362 ) ;
#79875 = ORIENTED_EDGE ( 'NONE', *, *, #46640, .F. ) ;
#79876 = CARTESIAN_POINT ( 'NONE',  ( 97.28760307318144385, 233.6427522451419065, 10.00000000000009415 ) ) ;
#79877 = ORIENTED_EDGE ( 'NONE', *, *, #59265, .F. ) ;
#79878 = DIRECTION ( 'NONE',  ( 0.000000000000000000, -0.6050222638427448230, 0.7962085532412974676 ) ) ;
#79879 = ORIENTED_EDGE ( 'NONE', *, *, #69340, .F. ) ;
#79880 = CARTESIAN_POINT ( 'NONE',  ( -70.00000000000000000, 20.00000000000000000, 59.99999999999999289 ) ) ;
#79881 = CARTESIAN_POINT ( 'NONE',  ( 79.58877750526134776, 55.57171882432602672, 16.09998944077883110 ) ) ;
#79882 = ORIENTED_EDGE ( 'NONE', *, *, #58549, .F. ) ;
#79883 = CARTESIAN_POINT ( 'NONE',  ( 147.9167952901743206, 274.4475905950902188, -6.349683594314821100 ) ) ;
#79884 = CARTESIAN_POINT ( 'NONE',  ( 189.7726967107949747, 264.4065126852114531, 11.24316165915873000 ) ) ;
#79885 = CARTESIAN_POINT ( 'NONE',  ( 192.6170194583582429, 297.0245312260774995, -11.90166228306590490 ) ) ;
#79886 = DIRECTION ( 'NONE',  ( -0.000000000000000000, -0.000000000000000000, 1.000000000000000000 ) ) ;
#79887 = DIRECTION ( 'NONE',  ( 0.9505498757754579087, -0.3105719460338643434, 0.000000000000000000 ) ) ;
#79888 = DIRECTION ( 'NONE',  ( 0.000000000000000000, 1.000000000000000000, 3.433861939970638790E-16 ) ) ;
#79889 = CARTESIAN_POINT ( 'NONE',  ( 131.9738982639959488, 240.8768266524160140, -9.188101187500091527 ) ) ;
#79890 = ORIENTED_EDGE ( 'NONE', *, *, #24910, .T. ) ;
#79891 = CARTESIAN_POINT ( 'NONE',  ( 185.7372650184451857, 257.4645284076796656, -2.264991511946413505E-12 ) ) ;
#79892 = EDGE_LOOP ( 'NONE', ( #57908, #61874, #21631, #37226 ) ) ;
#79894 = ORIENTED_EDGE ( 'NONE', *, *, #6952, .F. ) ;
#79893 = CARTESIAN_POINT ( 'NONE',  ( -77.42978507651396569, 55.80833764325424085, -10.00000000000000000 ) ) ;
#79895 = CARTESIAN_POINT ( 'NONE',  ( 200.4137396061031211, 274.1951937318462456, 13.51466377508595507 ) ) ;
#79896 = CARTESIAN_POINT ( 'NONE',  ( -22.42236680055709641, 157.8615022471902591, 0.000000000000000000 ) ) ;
#79897 = CARTESIAN_POINT ( 'NONE',  ( -55.56624327025929944, 44.99999999999998579, 59.99999999999999289 ) ) ;
#79898 = CARTESIAN_POINT ( 'NONE',  ( 192.3158717363151595, 297.5461343812397104, 12.57290801860991003 ) ) ;
#79899 = CARTESIAN_POINT ( 'NONE',  ( 156.0982710278114496, 278.5911654470725125, 7.232040771136105661 ) ) ;
#79900 = DIRECTION ( 'NONE',  ( 0.000000000000000000, 0.000000000000000000, 1.000000000000000000 ) ) ;
#79901 = CARTESIAN_POINT ( 'NONE',  ( -19.65312891409030271, 93.06504152958497400, 10.00000000000000888 ) ) ;
#79902 = CARTESIAN_POINT ( 'NONE',  ( 171.6386966857738230, 280.0180265567518063, 13.87489842761215009 ) ) ;
#79903 = CARTESIAN_POINT ( 'NONE',  ( 82.28003896795380001, 40.62557011406286733, -3.142018250819525793 ) ) ;
#79904 = CARTESIAN_POINT ( 'NONE',  ( 177.5869845173387773, 255.5126858138248451, -8.405682457315087674 ) ) ;
#79905 = ORIENTED_EDGE ( 'NONE', *, *, #19477, .F. ) ;
#79906 = LINE ( 'NONE', #27172, #70475 ) ;
#79907 = CARTESIAN_POINT ( 'NONE',  ( 152.5049231584100653, 273.3283623610165023, 11.85969823726709826 ) ) ;
#79908 = AXIS2_PLACEMENT_3D ( 'NONE', #15996, #16985, #15478 ) ;
#79909 = VERTEX_POINT ( 'NONE', #85984 ) ;
#79910 = DIRECTION ( 'NONE',  ( -0.2168075248790319320, -0.9762143704923770260, 0.000000000000000000 ) ) ;
#79911 = VECTOR ( 'NONE', #91319, 1000.000000000000114 ) ;
#79912 = CARTESIAN_POINT ( 'NONE',  ( 205.0859877718122561, 268.9368413191317586, -3.038556538008958974 ) ) ;
#79913 = CARTESIAN_POINT ( 'NONE',  ( 152.3230865050459784, 266.8156703379880810, -15.53149103319956303 ) ) ;
#79914 = DIRECTION ( 'NONE',  ( -1.000000000000000000, 0.000000000000000000, 0.000000000000000000 ) ) ;
#79915 = EDGE_CURVE ( 'NONE', #48468, #39339, #78333, .T. ) ;
#79916 = CARTESIAN_POINT ( 'NONE',  ( 202.8167949821795446, 279.3580017930215149, 15.61966256214195070 ) ) ;
#79918 = CARTESIAN_POINT ( 'NONE',  ( 154.8138742624348367, 277.2620699001403750, -8.801558155086558699 ) ) ;
#79917 = CARTESIAN_POINT ( 'NONE',  ( -19.76310821406011797, 93.15458644692216694, 59.99999999999999289 ) ) ;
#79919 = DIRECTION ( 'NONE',  ( -0.8660254037844387076, -0.4999999999999998890, -0.000000000000000000 ) ) ;
#79920 = ORIENTED_EDGE ( 'NONE', *, *, #89482, .T. ) ;
#79921 = B_SPLINE_SURFACE_WITH_KNOTS ( 'NONE', 3, 1, ( 
 ( #60360, #67482 ),
 ( #37081, #67986 ),
 ( #84719, #39053 ),
 ( #7680, #38057 ),
 ( #86237, #54248 ),
 ( #40057, #38567 ),
 ( #77072, #60856 ),
 ( #91821, #78090 ),
 ( #47167, #16771 ),
 ( #8679, #29979 ),
 ( #45662, #62867 ),
 ( #16273, #47663 ),
 ( #23867, #76586 ),
 ( #92326, #68970 ),
 ( #15258, #69966 ),
 ( #84232, #61861 ),
 ( #24382, #77597 ),
 ( #14779, #8185 ),
 ( #85221, #61369 ),
 ( #99401, #89 ),
 ( #69476, #22380 ),
 ( #580, #78597 ),
 ( #85745, #31464 ),
 ( #23364, #46155 ),
 ( #53278, #39548 ),
 ( #99893, #31963 ),
 ( #93823, #30479 ),
 ( #7171, #9182 ),
 ( #55254, #62356 ),
 ( #93310, #22874 ),
 ( #53759, #30972 ),
 ( #92810, #54759 ),
 ( #15766, #46671 ),
 ( #70471, #1086 ) ),
 .UNSPECIFIED., .T., .F., .F.,
 ( 4, 2, 2, 2, 2, 2, 2, 2, 2, 2, 2, 2, 2, 2, 2, 2, 4 ),
 ( 2, 2 ),
 ( 0.000000000000000000, 0.06250000000000000000, 0.1250000000000000000, 0.1875000000000000000, 0.2500000000000000000, 0.3125000000000000000, 0.3750000000000000000, 0.4375000000000000000, 0.5000000000000000000, 0.5625000000000000000, 0.6250000000000000000, 0.6875000000000000000, 0.7500000000000000000, 0.8125000000000000000, 0.8750000000000000000, 0.9375000000000000000, 1.000000000000000000 ),
 ( 0.000000000000000000, 1.000000000000000000 ),
 .UNSPECIFIED. ) ;
#79922 = B_SPLINE_CURVE_WITH_KNOTS ( 'NONE', 3,
 ( #1315, #63100, #40282, #94046, #55481, #24599 ),
 .UNSPECIFIED., .F., .F.,
 ( 4, 2, 4 ),
 ( 0.01862806261678935302, 0.02313791776344208823, 0.02764777291009481996 ),
 .UNSPECIFIED. ) ;
#79923 = CARTESIAN_POINT ( 'NONE',  ( 71.14215440105562038, 62.56599120317326879, -13.86464812710125294 ) ) ;
#79924 = CARTESIAN_POINT ( 'NONE',  ( 152.7122812589697958, 277.9324518551267147, 6.933031942251369983 ) ) ;
#79925 = CARTESIAN_POINT ( 'NONE',  ( 78.41477381122238910, 47.32040575024741713, -14.22103711499937262 ) ) ;
#79926 = CARTESIAN_POINT ( 'NONE',  ( 152.7153488183568300, 266.1362520814392951, 17.33540622643059237 ) ) ;
#79927 = CARTESIAN_POINT ( 'NONE',  ( 80.66106005736661189, 43.24916060877089308, -9.240259099883365579 ) ) ;
#79928 = CARTESIAN_POINT ( 'NONE',  ( 70.58472459542726085, 71.29540112946914121, -2.020767390530186614 ) ) ;
#79929 = CARTESIAN_POINT ( 'NONE',  ( -13.54586673536430830, 172.1744531367911293, 4.594050593750047540 ) ) ;
#79930 = CARTESIAN_POINT ( 'NONE',  ( 91.59511671678144751, 229.8149278399160664, 9.188101187500093303 ) ) ;
#79931 = CARTESIAN_POINT ( 'NONE',  ( 203.3740894404336927, 278.3927394765486838, -15.19753795879846869 ) ) ;
#79932 = CARTESIAN_POINT ( 'NONE',  ( 88.05369993652286098, 44.62252207614050548, -4.124069452546489600 ) ) ;
#79933 = DIRECTION ( 'NONE',  ( 1.000000000000000000, 0.000000000000000000, 0.000000000000000000 ) ) ;
#79934 = EDGE_CURVE ( 'NONE', #31705, #98801, #36211, .T. ) ;
#79935 = CARTESIAN_POINT ( 'NONE',  ( 33.22460751122017086, 89.13141723973357955, 59.99999999999999289 ) ) ;
#79936 = CARTESIAN_POINT ( 'NONE',  ( 205.7872507830675204, 272.2130214242461079, -9.506855900917111413 ) ) ;
#79937 = CARTESIAN_POINT ( 'NONE',  ( 164.1570551735447623, 284.3421986849189693, 5.865652139141318777 ) ) ;
#79939 = CARTESIAN_POINT ( 'NONE',  ( 208.3863431123642727, 269.7112614563416173, -1.693909372230378851 ) ) ;
#79938 = CARTESIAN_POINT ( 'NONE',  ( 189.8897621674675804, 300.5079289680896864, -1.468582484996752147 ) ) ;
#79940 = CARTESIAN_POINT ( 'NONE',  ( 178.0890608223913603, 290.4326850333343373, 9.911865951459251534 ) ) ;
#79941 = CARTESIAN_POINT ( 'NONE',  ( -22.42236680055709641, 157.8615022471902591, 0.000000000000000000 ) ) ;
#79942 = CARTESIAN_POINT ( 'NONE',  ( 77.44921057498504524, 55.30942947506500218, -16.14045094355945054 ) ) ;
#79943 = CARTESIAN_POINT ( 'NONE',  ( 79.15179632339811633, 45.85242797515901714, -13.09306047831970510 ) ) ;
#79944 = CARTESIAN_POINT ( 'NONE',  ( 83.43119661263041564, 225.6427522451419065, -10.00000000000009592 ) ) ;
#79945 = CARTESIAN_POINT ( 'NONE',  ( 73.61926920126447271, 69.75873974038962899, 10.00767910897496193 ) ) ;
#79946 = CARTESIAN_POINT ( 'NONE',  ( 50.62146334811270521, 200.0333772461660544, 9.188101187500095079 ) ) ;
#79947 = CARTESIAN_POINT ( 'NONE',  ( 76.86986466358051473, 64.04458250793000218, -15.20481942635857742 ) ) ;
#79948 = CARTESIAN_POINT ( 'NONE',  ( 71.05451054047556170, 202.6423013555409796, -4.594050593750043987 ) ) ;
#79949 = CARTESIAN_POINT ( 'NONE',  ( 207.6129110656513035, 271.0508850574501025, -5.265106572941297358 ) ) ;
#79950 = CARTESIAN_POINT ( 'NONE',  ( 87.90060490056963260, 43.92552512120865771, 0.4375478113261034308 ) ) ;
#79951 = CARTESIAN_POINT ( 'NONE',  ( 163.5572657305692132, 257.9363112301150522, 15.55976473370433766 ) ) ;
#79953 = CARTESIAN_POINT ( 'NONE',  ( 152.1502187761652749, 267.1150860273985472, 15.41609850895314615 ) ) ;
#79952 = CARTESIAN_POINT ( 'NONE',  ( 84.14312167556933275, 48.98415679381830756, 0.000000000000000000 ) ) ;
#79954 = CARTESIAN_POINT ( 'NONE',  ( 176.4985344937902880, 269.9855544425572020, -17.33307642928837566 ) ) ;
#79955 = CARTESIAN_POINT ( 'NONE',  ( 31.53879454291322304, 39.18502408145594273, 5.678558825948276656 ) ) ;
#79956 = CARTESIAN_POINT ( 'NONE',  ( 82.47767859619965236, 50.30750760982864733, 14.54247616347400296 ) ) ;
#79957 = LINE ( 'NONE', #43397, #68493 ) ;
#79958 = ORIENTED_EDGE ( 'NONE', *, *, #36443, .T. ) ;
#79959 = CARTESIAN_POINT ( 'NONE',  ( 19.43607595823839418, 14.14754757982089473, -5.678558825948276656 ) ) ;
#79960 = CARTESIAN_POINT ( 'NONE',  ( 79.14634863314513780, 210.3768266524160140, 9.188101187500096856 ) ) ;
#79961 = CARTESIAN_POINT ( 'NONE',  ( 74.23555041547365363, 68.49601928387087924, -11.11897725275786719 ) ) ;
#79962 = CARTESIAN_POINT ( 'NONE',  ( -13.11024591527734628, 6.000000000000000000, -32.50000000000000000 ) ) ;
#79963 = CARTESIAN_POINT ( 'NONE',  ( -21.13165894407813994, 132.6259306620403322, 2.598076211353400833 ) ) ;
#79964 = CARTESIAN_POINT ( 'NONE',  ( 201.8494044615141547, 281.0335713255741439, 17.80331436090332176 ) ) ;
#79965 = ORIENTED_EDGE ( 'NONE', *, *, #31281, .T. ) ;
#79966 = DIRECTION ( 'NONE',  ( 0.000000000000000000, 0.000000000000000000, 1.000000000000000000 ) ) ;
#79967 = CARTESIAN_POINT ( 'NONE',  ( 193.3835840830572295, 288.4008497395175254, 16.05775961610054026 ) ) ;
#79968 = CARTESIAN_POINT ( 'NONE',  ( 0.2713214620000473087, 45.32428913435456508, 59.99999999999999289 ) ) ;
#79969 = CARTESIAN_POINT ( 'NONE',  ( 130.4311169673963775, 246.1115022471902591, 10.00000000000009592 ) ) ;
#79970 = CARTESIAN_POINT ( 'NONE',  ( 21.76528272068881265, 171.8262482093457777, 3.021315404115420679E-15 ) ) ;
#79971 = CARTESIAN_POINT ( 'NONE',  ( 74.73487060833782891, 53.69418506457893159, 16.08953207461605217 ) ) ;
#79972 = VERTEX_POINT ( 'NONE', #1830 ) ;
#79973 = CARTESIAN_POINT ( 'NONE',  ( 184.7218640569926720, 271.1400913308660279, 16.40603036354897171 ) ) ;
#79974 = EDGE_LOOP ( 'NONE', ( #62533, #95594, #8254, #69224 ) ) ;
#79975 = CARTESIAN_POINT ( 'NONE',  ( 162.6774150396764469, 248.8814472377480911, 10.88033986792731689 ) ) ;
#79976 = DIRECTION ( 'NONE',  ( -0.3956464567955659817, 0.9184028970038772277, 0.000000000000000000 ) ) ;
#79977 = CARTESIAN_POINT ( 'NONE',  ( 201.1388841337167435, 282.2642286331299601, -18.17233400608081340 ) ) ;
#79978 = ADVANCED_FACE ( 'NONE', ( #8913 ), #79864, .T. ) ;
#79979 = VERTEX_POINT ( 'NONE', #86984 ) ;
#79980 = DIRECTION ( 'NONE',  ( 1.000000000000000000, 0.000000000000000000, 0.000000000000000000 ) ) ;
#79982 = VERTEX_POINT ( 'NONE', #78837 ) ;
#79981 = VECTOR ( 'NONE', #21741, 1000.000000000000000 ) ;
#79983 = CARTESIAN_POINT ( 'NONE',  ( 188.9102852820520582, 290.7616905290360023, 14.53875897011772445 ) ) ;
#79984 = CARTESIAN_POINT ( 'NONE',  ( 171.0307695606911125, 249.8159844473073861, 2.774073808362228721 ) ) ;
#79985 = CARTESIAN_POINT ( 'NONE',  ( 178.9281327940277606, 284.0931116521168747, -15.58854622419240243 ) ) ;
#79986 = ORIENTED_EDGE ( 'NONE', *, *, #71734, .T. ) ;
#79987 = CARTESIAN_POINT ( 'NONE',  ( 30.49295849316677831, 39.64646525600392835, -2.839279412974133887 ) ) ;
#79988 = CARTESIAN_POINT ( 'NONE',  ( 79.91974514325150381, 44.69068051420087073, 11.20237123581853744 ) ) ;
#79989 = CARTESIAN_POINT ( 'NONE',  ( 84.83352707183692587, 50.23671165375215253, -13.78554283518410095 ) ) ;
#79990 = CARTESIAN_POINT ( 'NONE',  ( 78.73344330045726736, 49.45143681483339293, -14.59549011545008490 ) ) ;
#79991 = DIRECTION ( 'NONE',  ( -1.000000000000000000, 0.000000000000000000, 0.000000000000000000 ) ) ;
#79992 = CARTESIAN_POINT ( 'NONE',  ( 17.60357497223980516, 35.28838536716092023, -10.00000000000000000 ) ) ;
#79993 = ORIENTED_EDGE ( 'NONE', *, *, #2200, .T. ) ;
#79994 = ORIENTED_EDGE ( 'NONE', *, *, #57821, .F. ) ;
#79995 = CARTESIAN_POINT ( 'NONE',  ( 183.0367609120576162, 295.8830680031519478, 0.5753348830509616985 ) ) ;
#79997 = CARTESIAN_POINT ( 'NONE',  ( 194.6356465353167948, 293.5281665672507643, -16.13180903283129197 ) ) ;
#79996 = CARTESIAN_POINT ( 'NONE',  ( 163.7707306762541748, 246.9877690064858484, 7.021959502997312086 ) ) ;
#79998 = CARTESIAN_POINT ( 'NONE',  ( 81.71134522782797660, 55.74075304576283685, -15.99172648312053369 ) ) ;
#79999 = CARTESIAN_POINT ( 'NONE',  ( 194.3562588153086779, 294.0120802933159325, 14.11474987148825200 ) ) ;
#80000 = LINE ( 'NONE', #65254, #83683 ) ;
#80001 = CARTESIAN_POINT ( 'NONE',  ( 167.2638507335506688, 272.3832265362266867, -17.29346045784080133 ) ) ;
#80002 = CARTESIAN_POINT ( 'NONE',  ( 164.5410109126144960, 245.6536045010434748, 5.739447577850491200 ) ) ;
#80003 = CARTESIAN_POINT ( 'NONE',  ( 166.2521479564098854, 265.4651998704476341, 16.55286243553473469 ) ) ;
#80004 = DIRECTION ( 'NONE',  ( 0.5000000000000011102, 0.8660254037844380415, 0.000000000000000000 ) ) ;
#80005 = CARTESIAN_POINT ( 'NONE',  ( 82.25819355828922141, 227.4869531367911293, 4.594050593750046652 ) ) ;
#80006 = ORIENTED_EDGE ( 'NONE', *, *, #74081, .F. ) ;
#80007 = CARTESIAN_POINT ( 'NONE',  ( 183.6422324172568210, 264.5785696717482551, 14.31652553825990104 ) ) ;
#80008 = LINE ( 'NONE', #62751, #98196 ) ;
#80009 = ORIENTED_EDGE ( 'NONE', *, *, #89430, .T. ) ;
#80010 = PRODUCT_DEFINITION ( 'UNKNOWN', '', #47866, #77774 ) ;
#80011 = CARTESIAN_POINT ( 'NONE',  ( 165.8785007526746540, 265.8076673077522969, -16.62180286104441507 ) ) ;
#80012 = ORIENTED_EDGE ( 'NONE', *, *, #26555, .F. ) ;
#80013 = CARTESIAN_POINT ( 'NONE',  ( 79.96962623824013860, 44.78594355328343823, -11.26070751024680661 ) ) ;
#80014 = CARTESIAN_POINT ( 'NONE',  ( 66.66342508697567837, 67.67433879810248243, 6.129251300726011209 ) ) ;
#80015 = LINE ( 'NONE', #24278, #22267 ) ;
#80016 = CARTESIAN_POINT ( 'NONE',  ( 85.47913374364790684, 42.62622548008751266, 0.2499991700750583967 ) ) ;
#80017 = CARTESIAN_POINT ( 'NONE',  ( 206.2313482792274328, 273.4438219973828268, -9.403385562213845361 ) ) ;
#80018 = CARTESIAN_POINT ( 'NONE',  ( 160.3733185927383715, 282.5102941377067509, 6.606729549618552078 ) ) ;
#80019 = CARTESIAN_POINT ( 'NONE',  ( 92.19068272976576850, 224.0333772461660544, 9.188101187500095079 ) ) ;
#80020 = EDGE_LOOP ( 'NONE', ( #80754, #62483, #46915, #7794 ) ) ;
#80021 = EDGE_LOOP ( 'NONE', ( #65109, #96170, #68254, #37512 ) ) ;
#80022 = CARTESIAN_POINT ( 'NONE',  ( 161.9020140854683234, 250.2244810866738760, -14.08518779869104343 ) ) ;
#80023 = ORIENTED_EDGE ( 'NONE', *, *, #14602, .F. ) ;
#80024 = B_SPLINE_CURVE_WITH_KNOTS ( 'NONE', 3,
 ( #41209, #42214, #66026, #27038 ),
 .UNSPECIFIED., .F., .F.,
 ( 4, 4 ),
 ( 0.006155465570655065458, 0.01116048267587303570 ),
 .UNSPECIFIED. ) ;
#80025 = CARTESIAN_POINT ( 'NONE',  ( 75.91502559367474134, 65.16891969575354437, -14.48077610374784996 ) ) ;
#80026 = EDGE_CURVE ( 'NONE', #4372, #82839, #79237, .T. ) ;
#80027 = CARTESIAN_POINT ( 'NONE',  ( 165.5845933190392998, 285.3686551174989745, 0.6228737942997026877 ) ) ;
#80028 = CARTESIAN_POINT ( 'NONE',  ( 87.68902078672120126, 44.98529012857299136, -6.607530655827392074 ) ) ;
#80029 = CARTESIAN_POINT ( 'NONE',  ( -15.29569941879559281, 168.6427522451418781, -10.00000000000009415 ) ) ;
#80030 = CARTESIAN_POINT ( 'NONE',  ( 87.62752662085767952, 44.66923158952226203, 5.004374079557546651 ) ) ;
#80031 = ORIENTED_EDGE ( 'NONE', *, *, #85082, .T. ) ;
#80032 = CARTESIAN_POINT ( 'NONE',  ( 204.3227106360847927, 276.7496793685443208, 13.60086062244164573 ) ) ;
#80033 = CARTESIAN_POINT ( 'NONE',  ( 160.5595428929208310, 275.8229991552611864, 14.13237683250033605 ) ) ;
#80034 = CARTESIAN_POINT ( 'NONE',  ( 67.44257088943838596, 67.25355904234817217, -8.657396272410824878 ) ) ;
#80035 = CARTESIAN_POINT ( 'NONE',  ( 189.1550430427957110, 269.9471506065882522, 14.45832818640694484 ) ) ;
#80036 = CARTESIAN_POINT ( 'NONE',  ( 174.6413940958611875, 283.8768656314015857, 13.74801433323937694 ) ) ;
#80037 = CARTESIAN_POINT ( 'NONE',  ( 76.20493386330700503, 51.02659346225095049, -16.05104161519640371 ) ) ;
#80038 = PRESENTATION_LAYER_ASSIGNMENT (  '', '', ( #23353 ) ) ;
#80039 = EDGE_CURVE ( 'NONE', #30740, #67256, #11221, .T. ) ;
#80040 = DIRECTION ( 'NONE',  ( 0.4999999999999998890, -0.8660254037844385966, 0.000000000000000000 ) ) ;
#80041 = ORIENTED_EDGE ( 'NONE', *, *, #24734, .T. ) ;
#80042 = CARTESIAN_POINT ( 'NONE',  ( 203.3946109532447224, 276.3571951737117729, -14.55139583984842133 ) ) ;
#80043 = CARTESIAN_POINT ( 'NONE',  ( 200.1385401540174769, 283.9968752310148830, 17.30012534137638625 ) ) ;
#80044 = CARTESIAN_POINT ( 'NONE',  ( 84.09950503289748269, 42.51577704912055111, 4.332266723902765904 ) ) ;
#80045 = CARTESIAN_POINT ( 'NONE',  ( 193.5910456581822814, 274.5466812142672097, -16.41199759748324283 ) ) ;
#80046 = CARTESIAN_POINT ( 'NONE',  ( 77.90166149968712261, 61.78270738046986565, 16.06607043079731767 ) ) ;
#80047 = CARTESIAN_POINT ( 'NONE',  ( 174.9064783932017235, 290.1930726575905055, -6.379950440565356651 ) ) ;
#80048 = EDGE_CURVE ( 'NONE', #49899, #14660, #57504, .T. ) ;
#80049 = FACE_OUTER_BOUND ( 'NONE', #75092, .T. ) ;
#80050 = VERTEX_POINT ( 'NONE', #11446 ) ;
#80051 = AXIS2_PLACEMENT_3D ( 'NONE', #17412, #79764, #24510 ) ;
#80052 = CARTESIAN_POINT ( 'NONE',  ( 74.61052374806135390, 63.82185717549396031, -14.32275223664241715 ) ) ;
#80054 = CARTESIAN_POINT ( 'NONE',  ( 184.9023284419889137, 266.2659532107462041, 13.18801441717285883 ) ) ;
#80053 = CARTESIAN_POINT ( 'NONE',  ( 180.6167065349397944, 266.8569723307038544, -14.77775250061756296 ) ) ;
#80055 = CARTESIAN_POINT ( 'NONE',  ( 199.1341087029324513, 281.8436105099906968, -16.59105901670938010 ) ) ;
#80056 = CARTESIAN_POINT ( 'NONE',  ( 40.25072390630947439, 24.20801979619931998, -3.090169943749474069 ) ) ;
#80057 = CARTESIAN_POINT ( 'NONE',  ( 78.56719005003022005, 47.98515344134877836, 13.96283253221395704 ) ) ;
#80058 = CARTESIAN_POINT ( 'NONE',  ( 81.19656099875513178, 43.43094936621162105, -9.896970666190503252 ) ) ;
#80059 = DIRECTION ( 'NONE',  ( -1.000000000000000000, 0.000000000000000000, 0.000000000000000000 ) ) ;
#80060 = CARTESIAN_POINT ( 'NONE',  ( 159.4413293807720606, 272.0932757909793622, -14.74450807601864888 ) ) ;
#80061 = CARTESIAN_POINT ( 'NONE',  ( 83.14648767797254436, 43.23107607431138177, -7.173306651377752807 ) ) ;
#80062 = CARTESIAN_POINT ( 'NONE',  ( 207.1770866921659717, 271.8057550155037347, -5.569195235244989384 ) ) ;
#80063 = CARTESIAN_POINT ( 'NONE',  ( -0.9884983804899494242, 179.4244531367911577, -4.594050593750046652 ) ) ;
#80064 = CARTESIAN_POINT ( 'NONE',  ( -19.65312891409030271, 93.06504152958497400, 59.99999999999999289 ) ) ;
#80065 = ORIENTED_EDGE ( 'NONE', *, *, #11339, .T. ) ;
#80066 = CARTESIAN_POINT ( 'NONE',  ( 86.79190430688251467, 45.84585087985657736, 8.866399834819148396 ) ) ;
#80067 = CARTESIAN_POINT ( 'NONE',  ( 29.10770312285472983, 32.50829794293882458, -10.00000000000000355 ) ) ;
#80068 = CARTESIAN_POINT ( 'NONE',  ( 81.67161923058380069, 41.61203830614370247, 5.543601729363009767 ) ) ;
#80069 = CARTESIAN_POINT ( 'NONE',  ( 30.81113223654366706, 188.5958772461660544, -9.188101187500095079 ) ) ;
#80070 = CARTESIAN_POINT ( 'NONE',  ( 161.1884843536000744, 251.4603508349806873, 13.21272898143761942 ) ) ;
#80071 = FACE_OUTER_BOUND ( 'NONE', #72145, .T. ) ;
#80072 = CARTESIAN_POINT ( 'NONE',  ( 33.70846307691164156, 35.16454794089043645, -10.00000000000000355 ) ) ;
#80073 = CARTESIAN_POINT ( 'NONE',  ( 199.5204482824095464, 267.4377498580035422, -6.650170480489714819 ) ) ;
#80074 = CARTESIAN_POINT ( 'NONE',  ( 191.3610003135137276, 299.2000202002271294, -9.855749861282104618 ) ) ;
#80075 = CARTESIAN_POINT ( 'NONE',  ( 196.3076213506950296, 290.6322212380402448, 17.33673088264725592 ) ) ;
#80076 = CARTESIAN_POINT ( 'NONE',  ( 44.18794977381974576, 118.5901545549086791, -10.00000000000000000 ) ) ;
#80077 = DIRECTION ( 'NONE',  ( -0.5637708215276967527, 0.8259312688075115538, 0.000000000000000000 ) ) ;
#80078 = ADVANCED_FACE ( 'NONE', ( #97060 ), #88482, .F. ) ;
#80079 = EDGE_CURVE ( 'NONE', #62092, #66923, #86876, .T. ) ;
#80080 = CARTESIAN_POINT ( 'NONE',  ( 87.18760076931933156, 46.20468558230229661, -8.391508599297639037 ) ) ;
#80081 = CARTESIAN_POINT ( 'NONE',  ( 83.50487366122874278, 51.96486753097845224, 15.01313857892666626 ) ) ;
#80082 = ADVANCED_FACE ( 'NONE', ( #50407 ), #74739, .F. ) ;
#80083 = CARTESIAN_POINT ( 'NONE',  ( 182.7078241176633639, 296.4455565966184167, 1.853464302320349200 ) ) ;
#80084 = CARTESIAN_POINT ( 'NONE',  ( 82.43887584100873767, 211.7365022471901739, -10.00000000000009059 ) ) ;
#80085 = CARTESIAN_POINT ( 'NONE',  ( 49.07456115661582174, 91.13648234292965356, -10.00000000000000000 ) ) ;
#80086 = CARTESIAN_POINT ( 'NONE',  ( 29.27874087092374111, 39.83705186507756224, 3.090169943749475401 ) ) ;
#80087 = CARTESIAN_POINT ( 'NONE',  ( 33.95012722949724093, 202.6589784336661637, -6.496448406907675876E-16 ) ) ;
#80088 = CARTESIAN_POINT ( 'NONE',  ( 197.8809552785519656, 287.9071269377202498, 17.61728046362068412 ) ) ;
#80089 = ORIENTED_EDGE ( 'NONE', *, *, #95683, .T. ) ;
#80090 = CARTESIAN_POINT ( 'NONE',  ( -12.93060150105072559, 85.35421234851665417, 14.87203518896413357 ) ) ;
#80091 = CARTESIAN_POINT ( 'NONE',  ( 198.4782858197754649, 286.8725200914082620, -17.44895083299520522 ) ) ;
#80092 = CARTESIAN_POINT ( 'NONE',  ( 67.51094951715245429, 66.79118171239792900, -8.453174244170460483 ) ) ;
#80093 = EDGE_CURVE ( 'NONE', #42773, #66517, #43295, .T. ) ;
#80094 = ORIENTED_EDGE ( 'NONE', *, *, #50446, .F. ) ;
#80095 = CARTESIAN_POINT ( 'NONE',  ( 170.0073542471708947, 285.8791242548903142, 7.485010625345761781 ) ) ;
#80096 = CARTESIAN_POINT ( 'NONE',  ( 168.2008345946905479, 248.1884056956802453, -5.064766917302788052 ) ) ;
#80097 = CARTESIAN_POINT ( 'NONE',  ( 147.1485523687439070, 275.7782263675629792, 6.742590758227570369 ) ) ;
#80098 = CARTESIAN_POINT ( 'NONE',  ( 72.19011348444853127, 68.90289858658827882, 10.04383758347407074 ) ) ;
#80099 = CARTESIAN_POINT ( 'NONE',  ( 22.55378097864968012, 33.99752408145592852, 5.678558825948277544 ) ) ;
#80100 = CARTESIAN_POINT ( 'NONE',  ( 163.1691520398773321, 248.0297337694385931, 11.21816141384514331 ) ) ;
#80101 = CARTESIAN_POINT ( 'NONE',  ( 149.0598351764325002, 272.4677874370131576, -11.59078276432863674 ) ) ;
#80102 = CARTESIAN_POINT ( 'NONE',  ( 174.6566889969473948, 257.2801211409499160, 11.41830854748823221 ) ) ;
#80103 = ORIENTED_EDGE ( 'NONE', *, *, #16510, .F. ) ;
#80104 = CARTESIAN_POINT ( 'NONE',  ( 21.21803360120161486, 14.11110640527291871, -2.839279412974138328 ) ) ;
#80105 = EDGE_CURVE ( 'NONE', #75846, #19430, #65104, .T. ) ;
#80106 = CARTESIAN_POINT ( 'NONE',  ( 171.6197681575868899, 252.4849835280233492, 8.664910895864313289 ) ) ;
#80107 = CARTESIAN_POINT ( 'NONE',  ( 71.89122079532039322, 72.62093029633255981, -0.6100853850958146696 ) ) ;
#80108 = EDGE_CURVE ( 'NONE', #68153, #26850, #27616, .T. ) ;
#80109 = ORIENTED_EDGE ( 'NONE', *, *, #79165, .F. ) ;
#80110 = CARTESIAN_POINT ( 'NONE',  ( 179.5754329387666246, 282.6374756363382517, 15.15522646414435926 ) ) ;
#80111 = CARTESIAN_POINT ( 'NONE',  ( 144.9899443387551798, 254.5170451491295296, 0.000000000000000000 ) ) ;
#80112 = CARTESIAN_POINT ( 'NONE',  ( 177.3409152927461889, 255.9687924550131299, -7.086473103942450003 ) ) ;
#80113 = CARTESIAN_POINT ( 'NONE',  ( 167.4035461121217736, 269.8829485561403771, 17.70625493734027600 ) ) ;
#80114 = AXIS2_PLACEMENT_3D ( 'NONE', #74147, #65523, #19940 ) ;
#80115 = ORIENTED_EDGE ( 'NONE', *, *, #12887, .F. ) ;
#80116 = ORIENTED_EDGE ( 'NONE', *, *, #38962, .T. ) ;
#80118 = CARTESIAN_POINT ( 'NONE',  ( 88.67874521539408761, 45.12822637883663646, 1.911324073694122932E-15 ) ) ;
#80117 = CARTESIAN_POINT ( 'NONE',  ( 161.1150691641480535, 251.5875096731584506, -13.48836942566120101 ) ) ;
#80119 = CARTESIAN_POINT ( 'NONE',  ( 9.964077338596862177, 24.49103043416547365, -8.090169943749479842 ) ) ;
#80120 = ORIENTED_EDGE ( 'NONE', *, *, #12713, .F. ) ;
#80121 = CARTESIAN_POINT ( 'NONE',  ( 152.6873874250818517, 266.1846826352417565, -16.66598363829485763 ) ) ;
#80122 = CARTESIAN_POINT ( 'NONE',  ( 72.07791713363762653, 72.33007614824393272, -3.421992246486540434 ) ) ;
#80123 = CARTESIAN_POINT ( 'NONE',  ( 72.83035752141398689, 57.36277735378698850, -15.86473357501050074 ) ) ;
#80124 = CARTESIAN_POINT ( 'NONE',  ( 78.11917150362724271, 61.95746172053952705, -16.05486485196055568 ) ) ;
#80125 = CARTESIAN_POINT ( 'NONE',  ( 157.8719920515997046, 257.2046840049564480, -17.69857783492101433 ) ) ;
#80127 = CARTESIAN_POINT ( 'NONE',  ( 115.3025621453804490, 243.5024278399160949, 9.188101187500095079 ) ) ;
#80126 = VECTOR ( 'NONE', #55274, 1000.000000000000114 ) ;
#80128 = CARTESIAN_POINT ( 'NONE',  ( 196.3507576896697344, 290.5575069072837664, -17.68249398312240928 ) ) ;
#80129 = CARTESIAN_POINT ( 'NONE',  ( 79.03685904533298867, 227.9860189848785126, -2.679491924311252493 ) ) ;
#80130 = ORIENTED_EDGE ( 'NONE', *, *, #99469, .T. ) ;
#80131 = CARTESIAN_POINT ( 'NONE',  ( 164.4678285797544106, 245.7803600197737524, -6.875991496205872799 ) ) ;
#80132 = ORIENTED_EDGE ( 'NONE', *, *, #21354, .T. ) ;
#80133 = CARTESIAN_POINT ( 'NONE',  ( 28.76090768559789979, 38.64646525600391413, -2.839279412974133887 ) ) ;
#80134 = CARTESIAN_POINT ( 'NONE',  ( 157.4027210288906531, 258.5085945389839139, 16.84379666775977213 ) ) ;
#80135 = CARTESIAN_POINT ( 'NONE',  ( 78.21114047790953805, 47.70659236517302304, -14.47520218207839982 ) ) ;
#80136 = CARTESIAN_POINT ( 'NONE',  ( 60.25564886944957976, 217.8464784336661637, 1.353441290958777525E-15 ) ) ;
#80137 = CARTESIAN_POINT ( 'NONE',  ( 74.24116255903008721, 68.58322516222325760, 11.55893809163645614 ) ) ;
#80138 = PLANE ( 'NONE',  #96854 ) ;
#80139 = CARTESIAN_POINT ( 'NONE',  ( 73.04277380876573034, 70.56196896876862468, 7.835544939490341143 ) ) ;
#80140 = CARTESIAN_POINT ( 'NONE',  ( 172.6733913832073597, 271.7377284239155415, 17.68482103120430438 ) ) ;
#80141 = ORIENTED_EDGE ( 'NONE', *, *, #53379, .T. ) ;
#80142 = CARTESIAN_POINT ( 'NONE',  ( 75.91858796819732902, 58.13906729783923311, -16.03854386934378695 ) ) ;
#80143 = CARTESIAN_POINT ( 'NONE',  ( 199.3863224916975412, 265.3452568596479182, 0.1349916258391212209 ) ) ;
#80144 = CARTESIAN_POINT ( 'NONE',  ( 189.0172135941854492, 296.3830391516955274, 10.71955688187805222 ) ) ;
#80145 = VERTEX_POINT ( 'NONE', #2719 ) ;
#80146 = CARTESIAN_POINT ( 'NONE',  ( 171.8062308653840660, 259.5681322378169398, -13.86186043045860394 ) ) ;
#80147 = CARTESIAN_POINT ( 'NONE',  ( 69.06272728912895786, 69.58621347229239973, -4.965237653724661193 ) ) ;
#80148 = CARTESIAN_POINT ( 'NONE',  ( 161.1678764334604921, 258.7517053225153063, -16.56551366227781230 ) ) ;
#80149 = CARTESIAN_POINT ( 'NONE',  ( 206.8409998872672020, 269.9682599439536261, 1.764008356409222156 ) ) ;
#80150 = CARTESIAN_POINT ( 'NONE',  ( 190.6893905452545823, 300.3632824417117604, 3.294993852933539191 ) ) ;
#80151 = CARTESIAN_POINT ( 'NONE',  ( 177.2279885846477328, 269.5037953214600179, 16.10890805395466785 ) ) ;
#80152 = EDGE_CURVE ( 'NONE', #23598, #99548, #56885, .T. ) ;
#80153 = CARTESIAN_POINT ( 'NONE',  ( 87.00029699285249762, 43.25090828054809577, -2.658650631722468294 ) ) ;
#80154 = CARTESIAN_POINT ( 'NONE',  ( 126.3716228836088362, 253.7677522451419065, -5.000000000000047962 ) ) ;
#80155 = CARTESIAN_POINT ( 'NONE',  ( 167.5316711859411214, 256.4999896070169143, 13.69272852843613819 ) ) ;
#80156 = FACE_OUTER_BOUND ( 'NONE', #9199, .T. ) ;
#80157 = CARTESIAN_POINT ( 'NONE',  ( 123.0967907794404113, 248.0024278399161517, 9.188101187500095079 ) ) ;
#80158 = ORIENTED_EDGE ( 'NONE', *, *, #59202, .F. ) ;
#80159 = CARTESIAN_POINT ( 'NONE',  ( 84.83104025798097325, 44.16562702927063100, -7.189586749132937271 ) ) ;
#80160 = DIRECTION ( 'NONE',  ( -0.8660254037844379305, -0.5000000000000014433, -0.000000000000000000 ) ) ;
#80161 = EDGE_CURVE ( 'NONE', #20951, #68688, #24003, .T. ) ;
#80162 = CARTESIAN_POINT ( 'NONE',  ( 164.9101359252495627, 286.5608941336866451, 1.040025780022917790 ) ) ;
#80163 = CARTESIAN_POINT ( 'NONE',  ( 79.47299837911636189, 59.61027691956581975, -16.18668525952085346 ) ) ;
#80164 = CARTESIAN_POINT ( 'NONE',  ( 75.26800218211973004, 63.80269639718548547, 14.51819789563784546 ) ) ;
#80165 = CARTESIAN_POINT ( 'NONE',  ( 177.3593506507800441, 255.0021141411331200, 4.887753322990675997 ) ) ;
#80166 = ORIENTED_EDGE ( 'NONE', *, *, #27009, .F. ) ;
#80167 = CARTESIAN_POINT ( 'NONE',  ( 80.38474943732042277, 57.10871594127473116, -16.23110256588661571 ) ) ;
#80168 = CARTESIAN_POINT ( 'NONE',  ( 158.2519735457114791, 274.8320027810396482, -12.54673606207468950 ) ) ;
#80169 = CARTESIAN_POINT ( 'NONE',  ( 182.8880264097929000, 260.9253942413262735, 9.506296218588019542 ) ) ;
#80170 = CARTESIAN_POINT ( 'NONE',  ( 165.0748171242677245, 244.7290250210644729, -1.867635796467185028 ) ) ;
#80171 = LINE ( 'NONE', #65912, #20793 ) ;
#80172 = EDGE_CURVE ( 'NONE', #70878, #7719, #50027, .T. ) ;
#80173 = CARTESIAN_POINT ( 'NONE',  ( 195.2233764540819152, 263.4883587362652975, 0.8587759651238419112 ) ) ;
#80174 = CARTESIAN_POINT ( 'NONE',  ( 187.4912959212919361, 285.9308727613615133, 16.80547087661522809 ) ) ;
#80175 = CARTESIAN_POINT ( 'NONE',  ( 68.93992071117129683, 69.86581718082992154, 3.903901410921837289 ) ) ;
#80176 = CARTESIAN_POINT ( 'NONE',  ( 67.18419919549008057, 209.5958772461660544, -9.188101187500095079 ) ) ;
#80177 = CARTESIAN_POINT ( 'NONE',  ( 170.6644942104857989, 250.4764242134850463, 3.560033027948075190 ) ) ;
#80178 = EDGE_CURVE ( 'NONE', #92469, #34673, #59698, .T. ) ;
#80179 = EDGE_CURVE ( 'NONE', #55644, #98181, #55864, .T. ) ;
#80180 = CARTESIAN_POINT ( 'NONE',  ( 173.1676448813863374, 261.4169956538293036, 14.42742222810248620 ) ) ;
#80181 = CARTESIAN_POINT ( 'NONE',  ( 152.2460257044392620, 278.3500712430857789, -1.624206099058958630 ) ) ;
#80182 = CARTESIAN_POINT ( 'NONE',  ( 169.4020686296666156, 285.0774647284627576, -8.180577219304280945 ) ) ;
#80183 = AXIS2_PLACEMENT_3D ( 'NONE', #29008, #75114, #29983 ) ;
#80184 = CARTESIAN_POINT ( 'NONE',  ( 203.2732885619977026, 278.5673317194472247, -16.64305493556850024 ) ) ;
#80185 = CARTESIAN_POINT ( 'NONE',  ( 157.3056943055385659, 271.4195445804601263, -14.62320538668267922 ) ) ;
#80186 = CARTESIAN_POINT ( 'NONE',  ( 117.2783561438722586, 238.5177522451418497, -10.00000000000009592 ) ) ;
#80187 = CARTESIAN_POINT ( 'NONE',  ( 81.72375876848666110, 59.17461627083314113, 0.4987820251299118213 ) ) ;
#80188 = ORIENTED_EDGE ( 'NONE', *, *, #68378, .F. ) ;
#80189 = CARTESIAN_POINT ( 'NONE',  ( 148.3707431749605234, 273.6613297946520902, 8.912574527564540716 ) ) ;
#80190 = CARTESIAN_POINT ( 'NONE',  ( -11.70556275232237908, 173.2369531367911293, -4.594050593750048428 ) ) ;
#80191 = CARTESIAN_POINT ( 'NONE',  ( 37.36027580478099708, 198.5024278399160664, 9.188101187500095079 ) ) ;
#80192 = DIRECTION ( 'NONE',  ( 0.4999999999999998890, -0.8660254037844385966, 0.000000000000000000 ) ) ;
#80193 = CARTESIAN_POINT ( 'NONE',  ( 21.57298720112009249, 14.58380873178786885, 6.180339887498953466 ) ) ;
#80194 = CARTESIAN_POINT ( 'NONE',  ( 85.69214519656509310, 48.79468762505698720, 12.02259801017994789 ) ) ;
#80195 = CARTESIAN_POINT ( 'NONE',  ( 66.18996477082612273, 69.34069001910528129, 0.2116841265692433471 ) ) ;
#80196 = CARTESIAN_POINT ( 'NONE',  ( 192.6090810369716166, 292.3580219496548693, -14.34990427975804472 ) ) ;
#80197 = CARTESIAN_POINT ( 'NONE',  ( 147.5492216329511166, 275.0842468449245644, 4.751613690710122739 ) ) ;
#80198 = CARTESIAN_POINT ( 'NONE',  ( 73.87037352680503943, 54.99746270706273776, -16.12935872011092897 ) ) ;
#80199 = EDGE_CURVE ( 'NONE', #63065, #6345, #68670, .T. ) ;
#80201 = CARTESIAN_POINT ( 'NONE',  ( 61.41971759977592171, 216.2677522451419065, -5.000000000000047962 ) ) ;
#80200 = DIRECTION ( 'NONE',  ( -0.9302793824855987159, 0.3668518372888612822, 0.000000000000000000 ) ) ;
#80202 = CARTESIAN_POINT ( 'NONE',  ( 3.517663757265353741, 25.52903772873354171, -1.583844403245363575 ) ) ;
#80203 = CARTESIAN_POINT ( 'NONE',  ( 180.8720737262704290, 256.3169785306307631, 1.340588092569421130 ) ) ;
#80204 = CARTESIAN_POINT ( 'NONE',  ( 204.8057697639265768, 275.9129964160624695, -12.68356524114230766 ) ) ;
#80205 = CARTESIAN_POINT ( 'NONE',  ( 38.38820426754037385, 84.46014300635468430, 59.99999999999999289 ) ) ;
#80206 = EDGE_CURVE ( 'NONE', #12458, #83357, #62470, .T. ) ;
#80207 = CARTESIAN_POINT ( 'NONE',  ( 32.93109025799825673, 196.4865022471903160, -10.00000000000009415 ) ) ;
#80208 = CARTESIAN_POINT ( 'NONE',  ( 185.1158863356004076, 294.2829762544421328, 9.788930817016709085 ) ) ;
#80209 = CARTESIAN_POINT ( 'NONE',  ( 202.9972156839127990, 279.0455039708822937, 16.77197898838388213 ) ) ;
#80210 = CARTESIAN_POINT ( 'NONE',  ( 12.46239254174337852, 171.8768266524160140, -9.188101187500091527 ) ) ;
#80211 = CARTESIAN_POINT ( 'NONE',  ( 32.31339950491288704, 36.84336893147758474, -7.433330006724137462 ) ) ;
#80212 = CARTESIAN_POINT ( 'NONE',  ( 164.0397259771397955, 252.5309334026060242, 13.28083819032488577 ) ) ;
#80213 = CARTESIAN_POINT ( 'NONE',  ( 192.0645969571214096, 297.9813550654635605, 11.46542907566974812 ) ) ;
#80214 = CARTESIAN_POINT ( 'NONE',  ( 26.97895004263468266, 38.68290643055188127, 3.479690158560446702E-15 ) ) ;
#80215 = CARTESIAN_POINT ( 'NONE',  ( 187.1539397334955765, 259.1171307905131584, -2.424303653640247802 ) ) ;
#80216 = EDGE_CURVE ( 'NONE', #68463, #41583, #25497, .T. ) ;
#80217 = CARTESIAN_POINT ( 'NONE',  ( 154.9683083969241011, 262.2340116239618055, 18.33261662430134109 ) ) ;
#80218 = CARTESIAN_POINT ( 'NONE',  ( 149.2593905435863348, 272.1221474021800759, -12.98626158366800176 ) ) ;
#80219 =( LENGTH_UNIT ( ) NAMED_UNIT ( * ) SI_UNIT ( .MILLI., .METRE. ) );
#80220 = CARTESIAN_POINT ( 'NONE',  ( 8.149503075528279794, 26.74646525600388358, 2.839279412974139660 ) ) ;
#80221 = CARTESIAN_POINT ( 'NONE',  ( 153.4346252566255373, 277.7752686862202154, -5.213536763656924755 ) ) ;
#80222 = CARTESIAN_POINT ( 'NONE',  ( 13.26084062165525523, 25.84336893147755276, -7.433330006724137462 ) ) ;
#80223 = CARTESIAN_POINT ( 'NONE',  ( 68.07728789491670796, 220.1115022471903160, -5.000000000000047962 ) ) ;
#80224 = CIRCLE ( 'NONE', #97976, 4.999999999999993783 ) ;
#80225 = CARTESIAN_POINT ( 'NONE',  ( 192.9765683580851885, 270.2547331158643829, -14.50234918781434423 ) ) ;
#80226 = EDGE_CURVE ( 'NONE', #88881, #5812, #71115, .T. ) ;
#80227 = CARTESIAN_POINT ( 'NONE',  ( 84.83229447964083647, 50.15339875539878989, -13.73726727158769023 ) ) ;
#80228 = ADVANCED_FACE ( 'NONE', ( #10307 ), #32598, .F. ) ;
#80229 = CARTESIAN_POINT ( 'NONE',  ( 88.16031874257379286, 44.17530435389893739, -1.747866100070386564 ) ) ;
#80230 = ORIENTED_EDGE ( 'NONE', *, *, #14355, .T. ) ;
#80231 = CARTESIAN_POINT ( 'NONE',  ( 152.8890098693866832, 266.6752310492291826, 15.93618651899761041 ) ) ;
#80232 = CARTESIAN_POINT ( 'NONE',  ( 207.6918009085542849, 270.9142438413412037, 7.009114282139513818 ) ) ;
#80233 = VECTOR ( 'NONE', #81520, 1000.000000000000114 ) ;
#80234 = CARTESIAN_POINT ( 'NONE',  ( 66.08842961843907915, 68.52315484731427375, 4.630389166009985402 ) ) ;
#80235 = CARTESIAN_POINT ( 'NONE',  ( 87.36818918644996756, 45.49344374928407575, 7.101962019857444020 ) ) ;
#80236 = ORIENTED_EDGE ( 'NONE', *, *, #84522, .T. ) ;
#80237 = ORIENTED_EDGE ( 'NONE', *, *, #13159, .F. ) ;
#80238 = CARTESIAN_POINT ( 'NONE',  ( 193.6564271169084464, 262.6014873983580742, -4.146719891036213745 ) ) ;
#80239 = CARTESIAN_POINT ( 'NONE',  ( 86.72415995732357885, 47.00718562526229505, 10.33097223407348686 ) ) ;
#80240 = ORIENTED_EDGE ( 'NONE', *, *, #24594, .T. ) ;
#80241 = CARTESIAN_POINT ( 'NONE',  ( 78.30955769916531040, 61.43963167811126169, 15.82323565659766373 ) ) ;
#80242 = CARTESIAN_POINT ( 'NONE',  ( 174.3997061797743982, 262.4591641033748033, 14.57197903150277796 ) ) ;
#80243 = ORIENTED_EDGE ( 'NONE', *, *, #65535, .F. ) ;
#80244 = DIRECTION ( 'NONE',  ( 8.673617379884080832E-16, -0.000000000000000000, -1.000000000000000000 ) ) ;
#80245 = CARTESIAN_POINT ( 'NONE',  ( 79.11171798038402869, 59.41904482235665341, -16.53441574648433487 ) ) ;
#80246 = CARTESIAN_POINT ( 'NONE',  ( 79.02426040586578893, 48.68606636885871808, -14.72935746379201838 ) ) ;
#80247 = CARTESIAN_POINT ( 'NONE',  ( 15.25129666230372827, 24.50829794293881037, -10.00000000000000355 ) ) ;
#80248 = ORIENTED_EDGE ( 'NONE', *, *, #16276, .T. ) ;
#80249 = CARTESIAN_POINT ( 'NONE',  ( 174.0017767277458347, 267.4700837321790914, 16.54826822959725874 ) ) ;
#80250 = CARTESIAN_POINT ( 'NONE',  ( 166.1418958215914188, 273.9600516718538756, -15.29462885050179644 ) ) ;
#80251 = AXIS2_PLACEMENT_3D ( 'NONE', #31280, #93117, #52582 ) ;
#80252 = CARTESIAN_POINT ( 'NONE',  ( 74.25791966876403194, 62.13065321042455480, 14.88776587584266942 ) ) ;
#80253 = ORIENTED_EDGE ( 'NONE', *, *, #25109, .T. ) ;
#80254 = CARTESIAN_POINT ( 'NONE',  ( -17.42236680055705023, 149.2012482093457777, 0.000000000000000000 ) ) ;
#80255 = CARTESIAN_POINT ( 'NONE',  ( 202.8499463704053198, 279.3005819042728604, 17.04674939340617001 ) ) ;
#80256 = ORIENTED_EDGE ( 'NONE', *, *, #47166, .T. ) ;
#80257 = ORIENTED_EDGE ( 'NONE', *, *, #79849, .F. ) ;
#80258 = CARTESIAN_POINT ( 'NONE',  ( 156.9270364742972959, 266.2560578317317095, -16.47839810797669102 ) ) ;
#80259 = B_SPLINE_CURVE_WITH_KNOTS ( 'NONE', 3,
 ( #72692, #3286, #18473, #63553, #80821, #33672, #26568, #34166, #32655, #55927, #65551, #88423 ),
 .UNSPECIFIED., .F., .F.,
 ( 4, 2, 2, 2, 2, 4 ),
 ( 0.4976197654691878469, 0.6232148241018862223, 0.6860123534182385185, 0.7488098827345908148, 0.8744049413672954074, 1.000000000000000000 ),
 .UNSPECIFIED. ) ;
#80260 = AXIS2_PLACEMENT_3D ( 'NONE', #12112, #81540, #80554 ) ;
#80261 = ORIENTED_EDGE ( 'NONE', *, *, #23907, .T. ) ;
#80262 = CARTESIAN_POINT ( 'NONE',  ( 67.53009088161343243, 67.40294954277804607, 7.576186009010610789 ) ) ;
#80263 = EDGE_LOOP ( 'NONE', ( #65128, #7974, #45349, #96107 ) ) ;
#80264 = CARTESIAN_POINT ( 'NONE',  ( 83.06694468350191585, 50.40823306540413995, -14.42615828136741918 ) ) ;
#80265 = CARTESIAN_POINT ( 'NONE',  ( 147.9374661616566016, 274.4117875954463557, 6.504250773332477920 ) ) ;
#80266 = CARTESIAN_POINT ( 'NONE',  ( 177.6634127208063205, 289.0610186271913449, -9.329510868619479425 ) ) ;
#80267 = CARTESIAN_POINT ( 'NONE',  ( 70.35913297700497537, 67.20083026265126591, 10.03723707890633321 ) ) ;
#80268 = CARTESIAN_POINT ( 'NONE',  ( 200.0350729207520430, 281.2229895077505830, -17.27079589148639371 ) ) ;
#80269 = CARTESIAN_POINT ( 'NONE',  ( 176.3782206303458224, 290.4613412261181793, 6.112157577772562078 ) ) ;
#80270 = CARTESIAN_POINT ( 'NONE',  ( 146.6138605399200117, 276.7043397814778132, -0.5394499176159462950 ) ) ;
#80271 = ORIENTED_EDGE ( 'NONE', *, *, #94634, .F. ) ;
#80272 = CARTESIAN_POINT ( 'NONE',  ( 100.8442274002074441, 217.4824982072973683, 3.021315404115420679E-15 ) ) ;
#80273 = CARTESIAN_POINT ( 'NONE',  ( 19.64056747690256088, 19.84335787977763133, 9.188101187500006262 ) ) ;
#80274 = CARTESIAN_POINT ( 'NONE',  ( 206.3907062969896060, 273.1678058140250300, 11.56942460516550675 ) ) ;
#80276 = CARTESIAN_POINT ( 'NONE',  ( 164.8849641302980444, 245.0578600525887794, 2.884140591399200648 ) ) ;
#80275 = CARTESIAN_POINT ( 'NONE',  ( 77.54361356138011274, 49.75803992512373952, -14.96129575302289716 ) ) ;
#80278 = ORIENTED_EDGE ( 'NONE', *, *, #287, .T. ) ;
#80277 = CARTESIAN_POINT ( 'NONE',  ( 84.74965453446901620, 41.75349613245864333, -1.218611519740888882 ) ) ;
#80279 = ORIENTED_EDGE ( 'NONE', *, *, #71260, .F. ) ;
#80280 = CARTESIAN_POINT ( 'NONE',  ( 147.4586881104295344, 275.2410555057202828, -3.245347276174700202 ) ) ;
#80281 = CARTESIAN_POINT ( 'NONE',  ( 171.3429355605559294, 259.3079905075224474, -13.88314242353945360 ) ) ;
#80282 = CARTESIAN_POINT ( 'NONE',  ( 163.6678477032174044, 247.6361333164444432, 7.542859481152206058 ) ) ;
#80283 = CARTESIAN_POINT ( 'NONE',  ( 9.894862028763428796, 29.21091486745858745, -1.111400068045478839E-16 ) ) ;
#80284 = CARTESIAN_POINT ( 'NONE',  ( 161.1238074876215478, 251.5723744529297505, 13.42537408252843179 ) ) ;
#80285 = CARTESIAN_POINT ( 'NONE',  ( 190.5677878487744863, 300.5739044903526178, -1.037535106822473630 ) ) ;
#80286 = VERTEX_POINT ( 'NONE', #48304 ) ;
#80287 = CARTESIAN_POINT ( 'NONE',  ( -27.42236680055714260, 166.5217562850347406, 1.224646799147364892E-15 ) ) ;
#80288 = DIRECTION ( 'NONE',  ( 0.000000000000000000, 0.000000000000000000, 1.000000000000000000 ) ) ;
#80289 = CARTESIAN_POINT ( 'NONE',  ( 19.85049821812295079, 172.2677522451417929, -5.000000000000041744 ) ) ;
#80290 = CARTESIAN_POINT ( 'NONE',  ( 103.5572661544365332, 230.5958772461660260, -9.188101187500095079 ) ) ;
#80291 = EDGE_CURVE ( 'NONE', #22585, #97093, #72696, .T. ) ;
#80292 = CARTESIAN_POINT ( 'NONE',  ( 183.5238647517005006, 297.0535124292885598, -2.834911233012364473 ) ) ;
#80293 = CARTESIAN_POINT ( 'NONE',  ( 99.95784806818352308, 218.5177522451417929, 5.000000000000051514 ) ) ;
#80294 = CARTESIAN_POINT ( 'NONE',  ( 163.1306191313178431, 248.0964747248268338, 10.50682697533535048 ) ) ;
#80295 = CARTESIAN_POINT ( 'NONE',  ( 16.25090658753528317, 186.3149278399161233, 9.188101187500093303 ) ) ;
#80296 = VECTOR ( 'NONE', #93214, 1000.000000000000000 ) ;
#80297 = CARTESIAN_POINT ( 'NONE',  ( 170.7981279722302190, 250.1199420982161996, 6.208364627926498791 ) ) ;
#80298 = ORIENTED_EDGE ( 'NONE', *, *, #39701, .F. ) ;
#80299 = ORIENTED_EDGE ( 'NONE', *, *, #75237, .T. ) ;
#80300 = CARTESIAN_POINT ( 'NONE',  ( 74.46167478334288603, 68.12047429673633303, -11.58806946105432978 ) ) ;
#80301 = ADVANCED_FACE ( 'NONE', ( #63496 ), #93436, .T. ) ;
#80302 = CARTESIAN_POINT ( 'NONE',  ( 80.77153619337677526, 46.90080847010725051, -12.59910185819319217 ) ) ;
#80303 = VECTOR ( 'NONE', #32278, 1000.000000000000227 ) ;
#80304 = EDGE_CURVE ( 'NONE', #35723, #39680, #45698, .T. ) ;
#80305 = CARTESIAN_POINT ( 'NONE',  ( 82.41840067511127188, 41.61564054470166241, 4.454349221539423809 ) ) ;
#80306 = CARTESIAN_POINT ( 'NONE',  ( -19.79494373018473752, 93.06352608284200301, 59.99999999999999289 ) ) ;
#80307 = CARTESIAN_POINT ( 'NONE',  ( 207.2337123599961899, 271.7076764818092443, -5.443417788256701861 ) ) ;
#80308 = CARTESIAN_POINT ( 'NONE',  ( 182.1091148644272550, 284.7077012260656375, 14.92368712289904487 ) ) ;
#80309 = CARTESIAN_POINT ( 'NONE',  ( 97.45544333237508283, 238.6199935810941213, 2.679491924311251605 ) ) ;
#80310 = CARTESIAN_POINT ( 'NONE',  ( 45.15450443884093090, 203.0024278399160949, 9.188101187500095079 ) ) ;
#80311 = CARTESIAN_POINT ( 'NONE',  ( 72.24503514708140983, 222.5177522451419065, 5.000000000000046185 ) ) ;
#80312 = VERTEX_POINT ( 'NONE', #54887 ) ;
#80313 = CARTESIAN_POINT ( 'NONE',  ( 83.86212765327434226, 46.92509768004335058, 11.25106203221198875 ) ) ;
#80314 = CARTESIAN_POINT ( 'NONE',  ( 181.8515780981809371, 260.7328092829080219, -10.50361218802076024 ) ) ;
#80315 = CARTESIAN_POINT ( 'NONE',  ( -5.074968980656518802, 174.0024278399160664, -9.188101187500093303 ) ) ;
#80316 = CARTESIAN_POINT ( 'NONE',  ( 68.51532939750342166, 64.50022977702580818, -12.21507596867179046 ) ) ;
#80317 = CARTESIAN_POINT ( 'NONE',  ( 198.5954523381739989, 286.6695817285962562, -18.45134152028667174 ) ) ;
#80318 = AXIS2_PLACEMENT_3D ( 'NONE', #5738, #44225, #68037 ) ;
#80319 = DIRECTION ( 'NONE',  ( -1.000000000000000000, 0.000000000000000000, 0.000000000000000000 ) ) ;
#80320 = CARTESIAN_POINT ( 'NONE',  ( 192.7705129102570822, 296.7586727687594816, -13.39629674907774692 ) ) ;
#80321 = FACE_OUTER_BOUND ( 'NONE', #14770, .T. ) ;
#80322 = CARTESIAN_POINT ( 'NONE',  ( 164.0741338217690668, 246.4622593432776796, 7.359073626423302983 ) ) ;
#80323 = CARTESIAN_POINT ( 'NONE',  ( 191.0724301404414689, 299.6998384015373063, -9.342134220577969828 ) ) ;
#80324 = CARTESIAN_POINT ( 'NONE',  ( 164.5416088356626290, 245.6525688679454618, -1.463507744092769292 ) ) ;
#80325 = ORIENTED_EDGE ( 'NONE', *, *, #42972, .F. ) ;
#80326 = VECTOR ( 'NONE', #70292, 1000.000000000000000 ) ;
#80327 = B_SPLINE_CURVE_WITH_KNOTS ( 'NONE', 3,
 ( #49064, #63255, #17150, #56651, #87636, #79998, #39928, #94691, #94196, #10567, #25252, #47547, #56135, #70865, #40440, #62740, #48048, #24750, #69847, #31350, #85613, #93696, #16156, #47054 ),
 .UNSPECIFIED., .F., .F.,
 ( 4, 2, 2, 2, 2, 2, 2, 2, 2, 2, 2, 4 ),
 ( 0.000000000000000000, 0.1249999999999813483, 0.2499999999999626965, 0.3749999999999440448, 0.4374999999999475975, 0.4999999999999511502, 0.5624999999999547029, 0.6249999999999582556, 0.6874999999999618083, 0.7499999999999653610, 0.8749999999999826805, 1.000000000000000000 ),
 .UNSPECIFIED. ) ;
#80328 = ADVANCED_FACE ( 'NONE', ( #97905 ), #49305, .F. ) ;
#80329 = CARTESIAN_POINT ( 'NONE',  ( 1.032487885271483163, 164.7365022471902307, 10.00000000000009592 ) ) ;
#80330 = CARTESIAN_POINT ( 'NONE',  ( 181.1229545130053111, 268.2492853531657602, 15.68939201437969899 ) ) ;
#80331 = CARTESIAN_POINT ( 'NONE',  ( 129.7005815790617760, 239.5643266524159856, -9.188101187500093303 ) ) ;
#80332 = CARTESIAN_POINT ( 'NONE',  ( 23.10163885443276754, 15.19860640527292261, 2.839279412974134775 ) ) ;
#80333 = CARTESIAN_POINT ( 'NONE',  ( 75.10353227920388974, 67.08955699197328215, 13.10598502456514680 ) ) ;
#80334 = DIRECTION ( 'NONE',  ( 0.8660254037844395958, 0.4999999999999985567, 0.000000000000000000 ) ) ;
#80336 = CARTESIAN_POINT ( 'NONE',  ( 113.8346084569740242, 224.9824982072974251, 3.021315404115420679E-15 ) ) ;
#80335 = CARTESIAN_POINT ( 'NONE',  ( 157.3988263959001870, 258.0242309610243865, 16.72376558639979294 ) ) ;
#80337 = EDGE_CURVE ( 'NONE', #9864, #10695, #12009, .T. ) ;
#80338 = CARTESIAN_POINT ( 'NONE',  ( 190.6912771110283131, 300.3600148139396993, -7.801888377467689040 ) ) ;
#80339 = B_SPLINE_CURVE_WITH_KNOTS ( 'NONE', 3,
 ( #41996, #72932, #88663, #19230 ),
 .UNSPECIFIED., .F., .F.,
 ( 4, 4 ),
 ( 0.000000000000000000, 0.0002476878907693983085 ),
 .UNSPECIFIED. ) ;
#80340 = ORIENTED_EDGE ( 'NONE', *, *, #1638, .F. ) ;
#80341 = CARTESIAN_POINT ( 'NONE',  ( 189.6628273826063378, 261.3601078589450708, -4.481571141829256533 ) ) ;
#80342 = CARTESIAN_POINT ( 'NONE',  ( 196.3286486926436680, 290.5958008134369948, -16.58330917766970458 ) ) ;
#80343 = CARTESIAN_POINT ( 'NONE',  ( 206.7596416265183734, 271.4678399409689291, 6.202658291405857227 ) ) ;
#80344 = CARTESIAN_POINT ( 'NONE',  ( 176.3864270403830687, 292.4019977604870064, -1.109940439014482694 ) ) ;
#80345 = CARTESIAN_POINT ( 'NONE',  ( 81.29586503113306151, 55.42867650357229081, -16.33480133305122450 ) ) ;
#80346 = VERTEX_POINT ( 'NONE', #18920 ) ;
#80347 = CARTESIAN_POINT ( 'NONE',  ( 68.11396990072299218, 66.09066184265174115, -10.54551009852403709 ) ) ;
#80348 = CARTESIAN_POINT ( 'NONE',  ( 189.0689802957956260, 269.8288687927027354, -15.50864081522695415 ) ) ;
#80349 = CARTESIAN_POINT ( 'NONE',  ( 167.8099530253072089, 271.3928698661641761, -17.53051755021046532 ) ) ;
#80350 = ADVANCED_FACE ( 'NONE', ( #49793 ), #3712, .T. ) ;
#80351 = CARTESIAN_POINT ( 'NONE',  ( 196.4217682013366186, 270.9315512130719981, 12.02672033859111700 ) ) ;
#80352 = CARTESIAN_POINT ( 'NONE',  ( 83.70511640034648337, 52.20013393807822411, -14.67019430348358888 ) ) ;
#80353 = CARTESIAN_POINT ( 'NONE',  ( 72.13998692144450331, 71.54377819717346654, -5.860361805407116265 ) ) ;
#80354 = CARTESIAN_POINT ( 'NONE',  ( 192.8323852661406761, 296.6515067047851062, 11.86505947732313615 ) ) ;
#80355 = ORIENTED_EDGE ( 'NONE', *, *, #10198, .T. ) ;
#80356 = CARTESIAN_POINT ( 'NONE',  ( 199.9108924079315841, 281.4061427919369294, 17.32562639834143781 ) ) ;
#80357 = CARTESIAN_POINT ( 'NONE',  ( 45.84141126897937824, 27.26216523072498887, -2.296566073217252530E-15 ) ) ;
#80358 = CARTESIAN_POINT ( 'NONE',  ( 173.9975664532395285, 272.8775942563314629, -16.35843707697202021 ) ) ;
#80359 = ORIENTED_EDGE ( 'NONE', *, *, #76524, .F. ) ;
#80360 = CARTESIAN_POINT ( 'NONE',  ( 77.82724693974202523, 61.74329194277088106, 16.06526602017299510 ) ) ;
#80361 = CARTESIAN_POINT ( 'NONE',  ( 148.2670916631250861, 273.8408594794321971, -7.980554973576580835 ) ) ;
#80362 = CARTESIAN_POINT ( 'NONE',  ( 76.62156306105930526, 63.43458379359962152, 15.37592086074861619 ) ) ;
#80363 = ORIENTED_EDGE ( 'NONE', *, *, #61906, .T. ) ;
#80364 = CARTESIAN_POINT ( 'NONE',  ( 78.87398835131222086, 59.62348996268822532, 16.50394892759813814 ) ) ;
#80365 = CARTESIAN_POINT ( 'NONE',  ( 50.18541494347881837, 88.31343213334855591, -10.00000000000000000 ) ) ;
#80366 = CARTESIAN_POINT ( 'NONE',  ( 151.4159295687746294, 268.3869122420484814, 14.78076517566594106 ) ) ;
#80367 = CARTESIAN_POINT ( 'NONE',  ( 84.37825102736907468, 49.99960613749293969, 13.80049582259582763 ) ) ;
#80368 = VECTOR ( 'NONE', #34636, 1000.000000000000227 ) ;
#80369 = CYLINDRICAL_SURFACE ( 'NONE', #38711, 16.60714546451156792 ) ;
#80370 = CIRCLE ( 'NONE', #73821, 0.1418229129684298040 ) ;
#80371 = CARTESIAN_POINT ( 'NONE',  ( 73.45606387015448036, 70.03420106287664737, -9.568701002945239509 ) ) ;
#80372 = CARTESIAN_POINT ( 'NONE',  ( 84.58308955143566266, 49.89698236725671165, -13.67050406800346707 ) ) ;
#80373 = CARTESIAN_POINT ( 'NONE',  ( 203.3349860717029571, 278.4604684979374838, -16.59553970625579566 ) ) ;
#80374 = ORIENTED_EDGE ( 'NONE', *, *, #67003, .F. ) ;
#80375 = VERTEX_POINT ( 'NONE', #38564 ) ;
#80377 = VECTOR ( 'NONE', #95725, 1000.000000000000000 ) ;
#80376 = PLANE ( 'NONE',  #95048 ) ;
#80378 = EDGE_LOOP ( 'NONE', ( #42833, #75364, #82726, #76114 ) ) ;
#80379 = FACE_OUTER_BOUND ( 'NONE', #15375, .T. ) ;
#80381 = ORIENTED_EDGE ( 'NONE', *, *, #24228, .T. ) ;
#80380 = EDGE_CURVE ( 'NONE', #48939, #47538, #60854, .T. ) ;
#80382 = CARTESIAN_POINT ( 'NONE',  ( 172.9882089762378712, 271.0907866236487394, 16.42842503185412539 ) ) ;
#80383 = CARTESIAN_POINT ( 'NONE',  ( 202.9547455376043672, 279.1190644220934018, -15.19669173352461478 ) ) ;
#80384 = ORIENTED_EDGE ( 'NONE', *, *, #92875, .T. ) ;
#80385 = ADVANCED_BREP_SHAPE_REPRESENTATION ( '', ( #45023, #68784 ), #59069 ) ;
#80386 = CARTESIAN_POINT ( 'NONE',  ( 82.28206475745885484, 40.65554467922788007, 3.268909026120783157 ) ) ;
#80387 = CARTESIAN_POINT ( 'NONE',  ( 161.0951265809451627, 254.6677910432329384, -15.15446908189199782 ) ) ;
#80388 = CARTESIAN_POINT ( 'NONE',  ( 6.396987757676594555, 15.64441083166260427, 0.000000000000000000 ) ) ;
#80389 = CARTESIAN_POINT ( 'NONE',  ( 146.8312060062178830, 276.3278863910550172, -4.807241325481028227 ) ) ;
#80391 = EDGE_CURVE ( 'NONE', #49558, #43311, #83256, .T. ) ;
#80390 = CARTESIAN_POINT ( 'NONE',  ( 201.3053499423511425, 281.9759013948520874, -16.75960365258566398 ) ) ;
#80392 = CARTESIAN_POINT ( 'NONE',  ( 82.79552190425015112, 41.59957507336271476, -5.373932124834087887 ) ) ;
#80393 = CARTESIAN_POINT ( 'NONE',  ( 157.6399499600617560, 280.8244316517132120, 2.084453808153418297 ) ) ;
#80394 = CARTESIAN_POINT ( 'NONE',  ( 138.6312950077063135, 250.8458772461660260, 9.188101187500095079 ) ) ;
#80395 = VERTEX_POINT ( 'NONE', #44170 ) ;
#80396 = CARTESIAN_POINT ( 'NONE',  ( 70.60797872409460751, 60.93970780067326132, -14.47325389371336790 ) ) ;
#80397 = CARTESIAN_POINT ( 'NONE',  ( 35.63920408047906818, 43.68290643055190969, 3.479690158560446702E-15 ) ) ;
#80398 = ORIENTED_EDGE ( 'NONE', *, *, #45087, .T. ) ;
#80400 = ORIENTED_EDGE ( 'NONE', *, *, #7786, .T. ) ;
#80399 = CARTESIAN_POINT ( 'NONE',  ( 85.73351810911900373, 48.76173041439603395, -12.45270611261530469 ) ) ;
#80401 = VECTOR ( 'NONE', #44953, 1000.000000000000000 ) ;
#80402 = CARTESIAN_POINT ( 'NONE',  ( 202.4943568615953779, 279.9164810001701085, 17.09064351659286984 ) ) ;
#80403 = LINE ( 'NONE', #64665, #55996 ) ;
#80404 = CARTESIAN_POINT ( 'NONE',  ( 147.4541998938148026, 275.2488293249323874, 3.198773118013638950 ) ) ;
#80405 = CARTESIAN_POINT ( 'NONE',  ( 152.9604666561868669, 277.5026710028543562, 6.707571967777091970 ) ) ;
#80406 = CARTESIAN_POINT ( 'NONE',  ( 152.8721808860877616, 265.8646109718731623, -17.65676496037632504 ) ) ;
#80407 = CARTESIAN_POINT ( 'NONE',  ( 87.38036106307322370, 44.18516793481750682, 5.218929132667811110 ) ) ;
#80408 = VECTOR ( 'NONE', #94700, 1000.000000000000114 ) ;
#80409 = CARTESIAN_POINT ( 'NONE',  ( 172.3025413328323623, 280.3883983834500668, 13.89755669804951133 ) ) ;
#80410 = CARTESIAN_POINT ( 'NONE',  ( 22.42372293028334340, 18.11029122506294442, -8.090169943749478065 ) ) ;
#80411 = CARTESIAN_POINT ( 'NONE',  ( -19.83262083840135759, 133.3759306620403891, -1.732050807568708217 ) ) ;
#80412 =( BOUNDED_CURVE ( )  B_SPLINE_CURVE ( 2, ( #21396, #11332, #42191, #73126, #88874, #34597, #65495, #50292, #81246 ),
 .UNSPECIFIED., .F., .T. ) 
 B_SPLINE_CURVE_WITH_KNOTS ( ( 3, 2, 2, 2, 3 ),
 ( 0.3185483870967741882, 0.3198924731182795633, 0.3225806451612903136, 0.3252688172043010639, 0.3266129032258064391 ),
 .UNSPECIFIED. ) 
 CURVE ( )  GEOMETRIC_REPRESENTATION_ITEM ( )  RATIONAL_B_SPLINE_CURVE ( ( 0.9330127018922194093, 0.9330127018922194093, 1.000000000000000000, 0.8660254037844387076, 1.000000000000000000, 0.8660254037844387076, 1.000000000000000000, 0.9330127018922194093, 0.9330127018922194093 ) ) 
 REPRESENTATION_ITEM ( '' )  );
#80413 = VERTEX_POINT ( 'NONE', #60358 ) ;
#80414 = DIRECTION ( 'NONE',  ( -0.000000000000000000, -0.000000000000000000, -1.000000000000000000 ) ) ;
#80415 = CARTESIAN_POINT ( 'NONE',  ( 65.81325020318384134, 69.12384646711140590, 0.1587991348731422614 ) ) ;
#80416 = VERTEX_POINT ( 'NONE', #6686 ) ;
#80417 = CARTESIAN_POINT ( 'NONE',  ( 13.95435611255089725, 31.55466486950698268, -1.111400068045478839E-16 ) ) ;
#80418 = CARTESIAN_POINT ( 'NONE',  ( 200.9436326478643764, 267.7579332533520073, -2.705820022176459005 ) ) ;
#80419 = CARTESIAN_POINT ( 'NONE',  ( 152.0594748232699658, 267.2722591642930183, -15.41760623154783616 ) ) ;
#80420 = CARTESIAN_POINT ( 'NONE',  ( 148.9517569034208009, 272.6549844970639924, 12.50737104496728236 ) ) ;
#80421 = CARTESIAN_POINT ( 'NONE',  ( 162.7561251957091031, 248.7451172484279027, 11.07313294959361194 ) ) ;
#80423 = CARTESIAN_POINT ( 'NONE',  ( 87.99973427719299934, 43.78392399561505499, 2.406698522940694307 ) ) ;
#80422 = CARTESIAN_POINT ( 'NONE',  ( -19.65312891409030271, 93.06504152958497400, -10.00000000000000888 ) ) ;
#80424 = DIRECTION ( 'NONE',  ( -1.000000000000000000, 0.000000000000000000, 0.000000000000000000 ) ) ;
#80425 = VERTEX_POINT ( 'NONE', #68968 ) ;
#80426 = CARTESIAN_POINT ( 'NONE',  ( 3.756859464462060760, 179.6427522451419350, 10.00000000000009415 ) ) ;
#80427 = CARTESIAN_POINT ( 'NONE',  ( 189.9154251947152545, 274.3351997317865312, -15.66312253186087311 ) ) ;
#80428 = EDGE_CURVE ( 'NONE', #61894, #16667, #29485, .T. ) ;
#80429 = DIRECTION ( 'NONE',  ( -0.9619696745371177915, 0.2731562652969021787, 0.000000000000000000 ) ) ;
#80430 = DIRECTION ( 'NONE',  ( 0.9662637919863205083, 0.2575544297740129385, 0.000000000000000000 ) ) ;
#80431 = EDGE_CURVE ( 'NONE', #65130, #93491, #42122, .T. ) ;
#80432 = CARTESIAN_POINT ( 'NONE',  ( 80.98736875202749275, 43.37942139736701108, -9.977273511710089693 ) ) ;
#80433 = CARTESIAN_POINT ( 'NONE',  ( -19.75075453565523986, 93.16791512511277062, 59.99999999999999289 ) ) ;
#80434 = CARTESIAN_POINT ( 'NONE',  ( -17.05341241735402136, 102.9187400387798874, 44.62585372971393127 ) ) ;
#80435 = CARTESIAN_POINT ( 'NONE',  ( 2.042590532755589994, 181.1744531367911577, 4.594050593750047540 ) ) ;
#80436 = CARTESIAN_POINT ( 'NONE',  ( 103.0428032491157779, 239.4869531367911293, 4.594050593750046652 ) ) ;
#80437 = CARTESIAN_POINT ( 'NONE',  ( 202.9547455376043672, 279.1190644220934018, -15.19669173352461478 ) ) ;
#80438 = CARTESIAN_POINT ( 'NONE',  ( 176.2580550267919932, 278.7780497695933946, -16.99066290002705060 ) ) ;
#80439 = CARTESIAN_POINT ( 'NONE',  ( 185.6624252266433359, 295.2092130351491051, -7.682468391986430056 ) ) ;
#80440 = CARTESIAN_POINT ( 'NONE',  ( 22.66956910419568061, 38.88013629349136835, 10.00000000000000000 ) ) ;
#80441 = CIRCLE ( 'NONE', #88552, 7.500000000000000000 ) ;
#80442 = CARTESIAN_POINT ( 'NONE',  ( 77.34348292206982478, 51.51894111865114212, 15.53773553076495162 ) ) ;
#80443 = AXIS2_PLACEMENT_3D ( 'NONE', #73485, #12180, #43041 ) ;
#80444 = CARTESIAN_POINT ( 'NONE',  ( 163.2163199008810750, 283.1128886150968924, 5.650665759342564876 ) ) ;
#80445 = DIRECTION ( 'NONE',  ( -0.8660254037844379305, -0.5000000000000014433, -0.000000000000000000 ) ) ;
#80446 = CARTESIAN_POINT ( 'NONE',  ( 207.7086642703471568, 270.8850356419295053, 6.393550561233467100 ) ) ;
#80447 = PLANE ( 'NONE',  #74131 ) ;
#80448 = CARTESIAN_POINT ( 'NONE',  ( 41.10966550219802684, 207.8207943907112565, 17.47570218321536117 ) ) ;
#80449 = CARTESIAN_POINT ( 'NONE',  ( 166.1787379219248919, 253.5053611955299004, -13.54722061411465361 ) ) ;
#80450 = VECTOR ( 'NONE', #59267, 1000.000000000000000 ) ;
#80451 = EDGE_CURVE ( 'NONE', #63400, #55233, #61859, .T. ) ;
#80452 = CARTESIAN_POINT ( 'NONE',  ( 175.8597011290570435, 265.2696089897137313, -16.46207262707587304 ) ) ;
#80453 = EDGE_CURVE ( 'NONE', #40327, #62030, #43666, .T. ) ;
#80454 = CARTESIAN_POINT ( 'NONE',  ( 84.12564760914067108, 225.5024278399160664, 9.188101187500095079 ) ) ;
#80455 = CARTESIAN_POINT ( 'NONE',  ( 207.1432938686257046, 271.8642859028066141, -6.405155839440290322 ) ) ;
#80456 = CARTESIAN_POINT ( 'NONE',  ( 81.72770187496514893, 51.60650539560465688, -15.27405233875389179 ) ) ;
#80457 = CARTESIAN_POINT ( 'NONE',  ( -16.76269525828470464, 104.2312461070085021, 12.63376007436041171 ) ) ;
#80459 = CARTESIAN_POINT ( 'NONE',  ( 151.8083138175603892, 267.7072827870618994, 16.72399268212840084 ) ) ;
#80458 = CARTESIAN_POINT ( 'NONE',  ( 87.98594423550160570, 43.75089820288621212, -2.253463800273092676 ) ) ;
#80460 = CARTESIAN_POINT ( 'NONE',  ( 47.72569090598238972, 198.3615022471903728, 4.570193772333722408E-14 ) ) ;
#80461 = CARTESIAN_POINT ( 'NONE',  ( 29.97031301328857467, 32.70171378149920827, -9.188101187500004485 ) ) ;
#80462 = CARTESIAN_POINT ( 'NONE',  ( 83.17871495584169850, 48.30807258732734510, -13.18720427395424011 ) ) ;
#80463 = CARTESIAN_POINT ( 'NONE',  ( 86.98925081226386169, 46.40596221211884398, -8.809588356812493970 ) ) ;
#80464 = VERTEX_POINT ( 'NONE', #36573 ) ;
#80465 = CARTESIAN_POINT ( 'NONE',  ( 18.23327619575285041, 19.03085787977762067, 9.188101187500006262 ) ) ;
#80466 = CARTESIAN_POINT ( 'NONE',  ( 78.60473566001486745, 222.3149278399160664, 9.188101187500093303 ) ) ;
#80467 = CARTESIAN_POINT ( 'NONE',  ( 76.52691452431521668, 63.65543071367928007, 14.90473833858518127 ) ) ;
#80468 = AXIS2_PLACEMENT_3D ( 'NONE', #11965, #64664, #97575 ) ;
#80469 = CARTESIAN_POINT ( 'NONE',  ( 169.2282880876609852, 288.2011917236219460, -1.104675944282350830 ) ) ;
#80470 = DIRECTION ( 'NONE',  ( -0.8660254037844359321, -0.5000000000000051070, -0.000000000000000000 ) ) ;
#80471 = CARTESIAN_POINT ( 'NONE',  ( 153.9523474978568913, 263.9937075196493197, 17.96576651779691147 ) ) ;
#80472 = CARTESIAN_POINT ( 'NONE',  ( 70.37934122712871954, 61.23818324669216651, 14.28954007458889031 ) ) ;
#80473 = DIRECTION ( 'NONE',  ( -0.6361630342459823062, 0.7715546603183375263, 0.000000000000000000 ) ) ;
#80474 = CARTESIAN_POINT ( 'NONE',  ( 204.3825393355489268, 268.3164202310341011, -1.666735346079931457 ) ) ;
#80475 = CARTESIAN_POINT ( 'NONE',  ( 116.9355544250888101, 244.9865022471903160, 10.00000000000009237 ) ) ;
#80476 = CARTESIAN_POINT ( 'NONE',  ( 204.8057697639265768, 275.9129964160624695, -12.68356524114230766 ) ) ;
#80477 = CARTESIAN_POINT ( 'NONE',  ( 27.71094225399020416, 18.12755873383627048, -6.180339887498949025 ) ) ;
#80478 = VERTEX_POINT ( 'NONE', #76112 ) ;
#80479 = CARTESIAN_POINT ( 'NONE',  ( 85.23727002651352791, 45.78824278971900696, 9.273454399903927836 ) ) ;
#80480 = ORIENTED_EDGE ( 'NONE', *, *, #50873, .F. ) ;
#80481 = CARTESIAN_POINT ( 'NONE',  ( 162.6220573360242270, 248.9773295930640131, 10.49878733418918486 ) ) ;
#80482 = DIRECTION ( 'NONE',  ( 0.4999999999999992784, -0.8660254037844390407, 0.000000000000000000 ) ) ;
#80483 = CARTESIAN_POINT ( 'NONE',  ( 201.2949053258274148, 281.9939920013367782, -18.04004790210578335 ) ) ;
#80484 = ORIENTED_EDGE ( 'NONE', *, *, #45491, .T. ) ;
#80485 = CARTESIAN_POINT ( 'NONE',  ( 173.8489725193828690, 250.6783042533247112, 0.4419843250852882877 ) ) ;
#80487 = ORIENTED_EDGE ( 'NONE', *, *, #27009, .T. ) ;
#80486 = B_SPLINE_CURVE_WITH_KNOTS ( 'NONE', 3,
 ( #30390, #21306, #68876, #53191, #5109, #99311, #75509, #51715, #91227, #99805, #61281, #92245, #29890, #83639, #97823, #44078, #83132, #84146, #14692, #98319, #22795, #28910, #21794, #37475, #75017, #52183, #45575, #84628, #59785, #67900, #76025, #36490, #76503, #68386, #35988, #66893, #90754, #7084, #37968, #53674 ),
 .UNSPECIFIED., .F., .F.,
 ( 4, 2, 2, 2, 2, 2, 2, 2, 2, 2, 2, 2, 2, 2, 2, 2, 2, 2, 2, 4 ),
 ( 0.0008933001899280981805, 0.0009882263429314807734, 0.001083152495934863258, 0.001273004801941664006, 0.001652709413955309953, 0.002412118637982602065, 0.003930937086037185856, 0.004690346310064516348, 0.005070050922078181595, 0.005259903228085013351, 0.005354829381088430096, 0.005449755534091846841, 0.005497218610593546106, 0.005544681687095245372, 0.005639607840098596198, 0.005829460146105390657, 0.006019312452112185116, 0.006209164758118979575, 0.006588869370132517320, 0.006968573982146054197 ),
 .UNSPECIFIED. ) ;
#80488 = CARTESIAN_POINT ( 'NONE',  ( 189.5552538188079268, 290.0568273660060186, 14.45120452257448029 ) ) ;
#80489 = CARTESIAN_POINT ( 'NONE',  ( 167.4768688352648383, 247.4600260772554350, 3.619672341560728146 ) ) ;
#80490 = CARTESIAN_POINT ( 'NONE',  ( 193.9727266537411765, 280.6520757818764196, -17.67061856767345063 ) ) ;
#80491 = CARTESIAN_POINT ( 'NONE',  ( 153.3939648708017387, 264.9608545997728015, -16.49556533540763681 ) ) ;
#80492 = EDGE_CURVE ( 'NONE', #20754, #68396, #15256, .T. ) ;
#80493 = EDGE_LOOP ( 'NONE', ( #36421, #44664, #70453, #27999 ) ) ;
#80494 = CARTESIAN_POINT ( 'NONE',  ( 29.13557404741141355, 37.79752408145594700, -5.678558825948271327 ) ) ;
#80495 = PLANE ( 'NONE',  #25174 ) ;
#80496 = DIRECTION ( 'NONE',  ( 0.5000000000000013323, -0.8660254037844378194, 0.000000000000000000 ) ) ;
#80497 = CARTESIAN_POINT ( 'NONE',  ( 77.96441125478906997, 222.4865022471902876, 10.00000000000009415 ) ) ;
#80498 = ORIENTED_EDGE ( 'NONE', *, *, #46941, .F. ) ;
#80499 = EDGE_LOOP ( 'NONE', ( #41696, #98052, #8533, #76372 ) ) ;
#80500 = LINE ( 'NONE', #88614, #34662 ) ;
#80502 = CARTESIAN_POINT ( 'NONE',  ( 175.0296968597178306, 264.6864531019056699, -16.70299667166197466 ) ) ;
#80501 = CARTESIAN_POINT ( 'NONE',  ( 163.8670932201372352, 246.8208641845333773, 5.912697114930636211 ) ) ;
#80503 = CARTESIAN_POINT ( 'NONE',  ( 85.59143893114691082, 48.93292747530462350, -12.17357014060645604 ) ) ;
#80504 = CARTESIAN_POINT ( 'NONE',  ( 155.0197698005585494, 262.1448778582381465, 18.42918111182112284 ) ) ;
#80505 = DIRECTION ( 'NONE',  ( 0.000000000000000000, 0.000000000000000000, 1.000000000000000000 ) ) ;
#80506 = CARTESIAN_POINT ( 'NONE',  ( 187.5797606156519635, 291.4431286935292746, -13.96543404383497489 ) ) ;
#80507 = CARTESIAN_POINT ( 'NONE',  ( 164.0179581270640199, 246.5595585006577153, 4.626773987940105748 ) ) ;
#80508 = CARTESIAN_POINT ( 'NONE',  ( 166.0711008457315359, 265.5911104622053927, 16.59982951413131502 ) ) ;
#80509 = CARTESIAN_POINT ( 'NONE',  ( 26.05470188313195123, 197.3967562850347122, -4.648177544792955347E-16 ) ) ;
#80510 = CARTESIAN_POINT ( 'NONE',  ( 101.9874215621947258, 235.8149278399160664, 9.188101187500093303 ) ) ;
#80511 = ORIENTED_EDGE ( 'NONE', *, *, #85775, .F. ) ;
#80512 = CARTESIAN_POINT ( 'NONE',  ( 150.5224706509996793, 271.7355727819179378, 12.90524344130334455 ) ) ;
#80513 = CARTESIAN_POINT ( 'NONE',  ( 164.0156888896406144, 276.7977823333153538, -13.62624241490914478 ) ) ;
#80514 = AXIS2_PLACEMENT_3D ( 'NONE', #3949, #64249, #25244 ) ;
#80515 = VERTEX_POINT ( 'NONE', #29000 ) ;
#80516 = CARTESIAN_POINT ( 'NONE',  ( 80.17579727260986999, 44.92489227719274680, -11.27803833280161072 ) ) ;
#80518 = B_SPLINE_SURFACE_WITH_KNOTS ( 'NONE', 3, 1, ( 
 ( #25272, #79526 ),
 ( #10587, #87153 ),
 ( #47074, #39450 ),
 ( #10087, #40950 ),
 ( #41460, #93720 ),
 ( #24281, #55157 ),
 ( #9082, #86635 ),
 ( #32871, #86144 ),
 ( #47568, #71897 ),
 ( #94710, #78496 ),
 ( #2493, #39952 ),
 ( #70889, #31370 ),
 ( #1493, #32376 ),
 ( #63275, #481 ),
 ( #56671, #64279 ),
 ( #33376, #87656 ),
 ( #24771, #18188 ),
 ( #71396, #17170 ),
 ( #48070, #79011 ),
 ( #62254, #9598 ),
 ( #40460, #1986 ),
 ( #17685, #48585 ),
 ( #26778, #43460 ),
 ( #65760, #96715 ),
 ( #35366, #12082 ),
 ( #97694, #3498 ),
 ( #34375, #72908 ),
 ( #4473, #26285 ),
 ( #82015, #27777 ),
 ( #11594, #81031 ),
 ( #42453, #27282 ),
 ( #12589, #74401 ),
 ( #81512, #66276 ),
 ( #4986, #58164 ) ),
 .UNSPECIFIED., .T., .F., .F.,
 ( 4, 2, 2, 2, 2, 2, 2, 2, 2, 2, 2, 2, 2, 2, 2, 2, 4 ),
 ( 2, 2 ),
 ( 0.000000000000000000, 0.06250000000000000000, 0.1250000000000000000, 0.1875000000000000000, 0.2500000000000000000, 0.3125000000000000000, 0.3750000000000000000, 0.4375000000000000000, 0.5000000000000000000, 0.5625000000000000000, 0.6250000000000000000, 0.6875000000000000000, 0.7500000000000000000, 0.8125000000000000000, 0.8750000000000000000, 0.9375000000000000000, 1.000000000000000000 ),
 ( 0.000000000000000000, 1.000000000000000000 ),
 .UNSPECIFIED. ) ;
#80517 = CARTESIAN_POINT ( 'NONE',  ( 176.7809350997679871, 292.5586354479191868, -2.749667827406846232 ) ) ;
#80519 = PLANE ( 'NONE',  #1359 ) ;
#80520 = CARTESIAN_POINT ( 'NONE',  ( 12.45916558416763209, 19.14441083166259361, 10.00000000000000533 ) ) ;
#80521 = CARTESIAN_POINT ( 'NONE',  ( 75.15191903148871688, 52.97183600646508239, -16.48001256418180915 ) ) ;
#80522 = CARTESIAN_POINT ( 'NONE',  ( 93.48972083544241229, 224.7833772461660260, -9.188101187500095079 ) ) ;
#80523 = ORIENTED_EDGE ( 'NONE', *, *, #82612, .T. ) ;
#80524 = VECTOR ( 'NONE', #21939, 1000.000000000000000 ) ;
#80525 = ORIENTED_EDGE ( 'NONE', *, *, #84765, .F. ) ;
#80526 = CARTESIAN_POINT ( 'NONE',  ( 208.3586375946586315, 269.7592488206576604, -1.970210487958146128 ) ) ;
#80527 = ORIENTED_EDGE ( 'NONE', *, *, #46979, .T. ) ;
#80528 = B_SPLINE_CURVE_WITH_KNOTS ( 'NONE', 3,
 ( #82441, #19110, #20591, #13004 ),
 .UNSPECIFIED., .F., .F.,
 ( 4, 4 ),
 ( 0.002465106009209366237, 0.007832036753820320954 ),
 .UNSPECIFIED. ) ;
#80529 = CARTESIAN_POINT ( 'NONE',  ( 31.59046986846508887, 19.20801979619930222, -3.090169943749474069 ) ) ;
#80530 = CARTESIAN_POINT ( 'NONE',  ( 154.1661291110820002, 265.4451940853067526, 17.04838890951767283 ) ) ;
#80531 = CARTESIAN_POINT ( 'NONE',  ( 69.10341330002957250, 69.27088624711088016, -5.834800079929739702 ) ) ;
#80533 = CARTESIAN_POINT ( 'NONE',  ( 63.56442718099752653, 219.0530062829863027, -4.648177544792955347E-16 ) ) ;
#80532 = CARTESIAN_POINT ( 'NONE',  ( 133.4351425849996531, 247.8458772461660544, 9.188101187500095079 ) ) ;
#80534 = DIRECTION ( 'NONE',  ( -0.000000000000000000, -0.000000000000000000, 1.000000000000000000 ) ) ;
#80535 = CARTESIAN_POINT ( 'NONE',  ( 179.2808028007571295, 294.7024261520388109, 2.441722445006270892 ) ) ;
#80536 = ORIENTED_EDGE ( 'NONE', *, *, #30034, .T. ) ;
#80537 = VECTOR ( 'NONE', #96858, 1000.000000000000114 ) ;
#80538 = CARTESIAN_POINT ( 'NONE',  ( 87.05064968419601712, 44.04826721231160747, -3.969180055969657950 ) ) ;
#80539 = CARTESIAN_POINT ( 'NONE',  ( 160.3800780026849395, 275.5550921561430755, 12.83098206889909854 ) ) ;
#80540 = CARTESIAN_POINT ( 'NONE',  ( 82.25407785542023476, 40.61683643427734580, -3.170132542450867508 ) ) ;
#80541 = CARTESIAN_POINT ( 'NONE',  ( 190.2764353542772540, 270.7453569036100589, 14.24146154583773871 ) ) ;
#80542 = CARTESIAN_POINT ( 'NONE',  ( 175.9516857479530074, 284.1058583014313967, 13.15626907755806840 ) ) ;
#80543 = ADVANCED_FACE ( 'NONE', ( #76584 ), #59873, .F. ) ;
#80544 = CARTESIAN_POINT ( 'NONE',  ( 41.71240375114939525, 62.05720181600818108, -10.00000000000000000 ) ) ;
#80545 = CARTESIAN_POINT ( 'NONE',  ( 82.18398586331583999, 40.60379566207949154, -3.290968078514205253 ) ) ;
#80546 = EDGE_CURVE ( 'NONE', #58606, #46023, #17634, .T. ) ;
#80547 = CARTESIAN_POINT ( 'NONE',  ( 148.8636819117637629, 274.0699646975406836, 8.926834414297511344 ) ) ;
#80548 = CARTESIAN_POINT ( 'NONE',  ( 161.8873598795597388, 250.2498629158519350, 13.90822209621415873 ) ) ;
#80549 = AXIS2_PLACEMENT_3D ( 'NONE', #73208, #65585, #96533 ) ;
#80550 = CARTESIAN_POINT ( 'NONE',  ( 84.82914023846464602, 43.34880007081749653, 5.509971121964090557 ) ) ;
#80551 = CARTESIAN_POINT ( 'NONE',  ( 167.6084812233214620, 249.9591548999696045, 7.104712731158297601 ) ) ;
#80552 = CARTESIAN_POINT ( 'NONE',  ( 78.29764689744347095, 61.60233437561736736, 15.79145928805303711 ) ) ;
#80553 = CARTESIAN_POINT ( 'NONE',  ( 117.8941025407614802, 227.3262482093458061, 3.021315404115420679E-15 ) ) ;
#80554 = DIRECTION ( 'NONE',  ( 0.000000000000000000, -0.000000000000000000, 1.000000000000000000 ) ) ;
#80555 = EDGE_CURVE ( 'NONE', #89858, #91333, #75596, .T. ) ;
#80556 = CARTESIAN_POINT ( 'NONE',  ( 73.23875918664506912, 64.24404681984078991, -13.68588676845166674 ) ) ;
#80557 = CARTESIAN_POINT ( 'NONE',  ( 184.0314392521297577, 265.7402128651979751, 13.22062658568063576 ) ) ;
#80558 = CARTESIAN_POINT ( 'NONE',  ( 167.4011299790239775, 281.5488363183706042, 12.98604958840868662 ) ) ;
#80559 = CARTESIAN_POINT ( 'NONE',  ( 31.43297906638544603, 41.08080186712595605, -3.090169943749475845 ) ) ;
#80560 = CARTESIAN_POINT ( 'NONE',  ( 152.8134625983922490, 265.9663140294953791, 17.57333028169644251 ) ) ;
#80561 = FILL_AREA_STYLE ('',( #42492 ) ) ;
#80562 = FACE_OUTER_BOUND ( 'NONE', #8597, .T. ) ;
#80563 = DIRECTION ( 'NONE',  ( -1.000000000000000000, 0.000000000000000000, 0.000000000000000000 ) ) ;
#80564 = CARTESIAN_POINT ( 'NONE',  ( 205.8859833147073459, 272.4477355138645862, -9.370556367187116820 ) ) ;
#80565 = CARTESIAN_POINT ( 'NONE',  ( 161.1747502674735415, 251.4841389699472529, -13.25152330924089839 ) ) ;
#80566 = B_SPLINE_CURVE_WITH_KNOTS ( 'NONE', 3,
 ( #7820, #6325, #7312, #52914 ),
 .UNSPECIFIED., .F., .F.,
 ( 4, 4 ),
 ( 0.004697621459670930574, 0.009681921251354225211 ),
 .UNSPECIFIED. ) ;
#80567 = CARTESIAN_POINT ( 'NONE',  ( 12.43489537816885537, 187.1744531367911293, 4.594050593750047540 ) ) ;
#80568 = CARTESIAN_POINT ( 'NONE',  ( 82.71692427225742961, 49.78115959597967333, 13.75658874660800102 ) ) ;
#80569 = ORIENTED_EDGE ( 'NONE', *, *, #795, .T. ) ;
#80570 = AXIS2_PLACEMENT_3D ( 'NONE', #56177, #94236, #71413 ) ;
#80571 = CARTESIAN_POINT ( 'NONE',  ( 86.88058850597731464, 45.96296635460476665, 8.956153083123110648 ) ) ;
#80572 = CARTESIAN_POINT ( 'NONE',  ( 20.50317736733639506, 20.03677371833801502, 10.00000000000000533 ) ) ;
#80573 = CARTESIAN_POINT ( 'NONE',  ( 81.91674078166553841, 41.69822484696639719, 5.406868786614782429 ) ) ;
#80574 = CARTESIAN_POINT ( 'NONE',  ( 33.95012722949724093, 202.6589784336661353, -6.496448406907676862E-16 ) ) ;
#80575 = AXIS2_PLACEMENT_3D ( 'NONE', #73264, #81889, #28144 ) ;
#80576 = CARTESIAN_POINT ( 'NONE',  ( 200.7079229450794173, 283.0106753079404029, 16.90512463913211505 ) ) ;
#80577 = CARTESIAN_POINT ( 'NONE',  ( 146.8201187048455267, 276.3470901603510015, 4.112223577763169047 ) ) ;
#80578 = CARTESIAN_POINT ( 'NONE',  ( 42.94622797204061726, 25.76426979415093044, 3.090169943749476733 ) ) ;
#80579 = CARTESIAN_POINT ( 'NONE',  ( 178.5111704587965846, 291.6673396684018371, 5.951657379714801799 ) ) ;
#80580 = PRODUCT_DEFINITION ( 'UNKNOWN', '', #20351, #86920 ) ;
#80581 = CARTESIAN_POINT ( 'NONE',  ( 191.5893301551938350, 298.8045413135534432, -8.323356515452589477 ) ) ;
#80582 = AXIS2_PLACEMENT_3D ( 'NONE', #58996, #4847, #28122 ) ;
#80583 = CARTESIAN_POINT ( 'NONE',  ( 180.4708198263617760, 279.0196451454304452, -16.21208881180018579 ) ) ;
#80584 = FACE_OUTER_BOUND ( 'NONE', #64921, .T. ) ;
#80585 = LINE ( 'NONE', #50134, #29515 ) ;
#80586 = CARTESIAN_POINT ( 'NONE',  ( -63.30067564770008914, 39.94154026010144065, -10.00000000000000000 ) ) ;
#80587 = VECTOR ( 'NONE', #55488, 1000.000000000000227 ) ;
#80588 = CARTESIAN_POINT ( 'NONE',  ( 86.76900285993090733, 214.2365022471902023, 10.00000000000009592 ) ) ;
#80589 = CARTESIAN_POINT ( 'NONE',  ( 74.83067777111257612, 53.34009888148298728, 16.53286476888989043 ) ) ;
#80590 = CARTESIAN_POINT ( 'NONE',  ( 161.7978640724907677, 267.9030138832445118, -17.43408704942576293 ) ) ;
#80591 = CARTESIAN_POINT ( 'NONE',  ( 47.34706511187656020, 188.9548013555409796, -4.594050593750042211 ) ) ;
#80592 = ORIENTED_EDGE ( 'NONE', *, *, #59323, .F. ) ;
#80593 = CARTESIAN_POINT ( 'NONE',  ( -27.77457187288641904, 24.79904599702367562, 10.00000000000000000 ) ) ;
#80594 = CARTESIAN_POINT ( 'NONE',  ( 146.8516045228164160, 276.2925551239072774, 3.995954059407343273 ) ) ;
#80595 = CARTESIAN_POINT ( 'NONE',  ( 67.09245893241136116, 67.08985158454382258, -8.602705837570949754 ) ) ;
#80596 = VERTEX_POINT ( 'NONE', #99399 ) ;
#80597 = AXIS2_PLACEMENT_3D ( 'NONE', #96299, #72496, #55733 ) ;
#80598 = DIRECTION ( 'NONE',  ( 0.4996954135095463823, -0.8654978445076774163, -0.03489949670249753444 ) ) ;
#80599 = CARTESIAN_POINT ( 'NONE',  ( 164.7694554770609159, 245.2579269087094076, -3.003635650077957742 ) ) ;
#80600 = CARTESIAN_POINT ( 'NONE',  ( 147.2111107388217590, 275.6698720921492622, 6.171440615279542463 ) ) ;
#80601 = CARTESIAN_POINT ( 'NONE',  ( 23.93942162470478863, 34.79752408145593989, -5.678558825948271327 ) ) ;
#80602 = CARTESIAN_POINT ( 'NONE',  ( 33.48063555417975579, 19.73415679381824006, -6.890680421881970419E-14 ) ) ;
#80603 = CARTESIAN_POINT ( 'NONE',  ( 149.0203866098534888, 272.5361143586139860, -12.73049804737905255 ) ) ;
#80604 = EDGE_CURVE ( 'NONE', #96468, #79874, #57929, .T. ) ;
#80605 = CARTESIAN_POINT ( 'NONE',  ( 175.2507534243562759, 257.3665654692601947, 11.62234696046220428 ) ) ;
#80606 = EDGE_LOOP ( 'NONE', ( #62485, #92937, #85071, #5210 ) ) ;
#80607 = CARTESIAN_POINT ( 'NONE',  ( 19.72235211587467063, 17.10170272979926764, -7.433330006724141015 ) ) ;
#80608 = CARTESIAN_POINT ( 'NONE',  ( 171.6446478921618279, 252.6468516832340185, 8.591079895564956104 ) ) ;
#80609 = DIRECTION ( 'NONE',  ( 0.7891516029629116469, -0.6141984594095519778, 0.000000000000000000 ) ) ;
#80610 = ORIENTED_EDGE ( 'NONE', *, *, #32982, .F. ) ;
#80611 = CARTESIAN_POINT ( 'NONE',  ( 179.0976111355799958, 282.8091739615130678, 15.98715785805552159 ) ) ;
#80612 = CARTESIAN_POINT ( 'NONE',  ( 190.9501423151522772, 299.9116471280854626, 8.746938802470586083 ) ) ;
#80613 = PLANE ( 'NONE',  #22631 ) ;
#80614 = CARTESIAN_POINT ( 'NONE',  ( 75.80568730619351925, 63.70677841270451580, -15.10342109092735363 ) ) ;
#80615 = ADVANCED_FACE ( 'NONE', ( #33482 ), #70470, .T. ) ;
#80616 = EDGE_LOOP ( 'NONE', ( #90936, #42060, #42281, #41172, #8576, #63384, #6730, #66979, #61153, #92706, #51787, #68048, #97913, #23579, #98695, #69474, #34703, #93035, #66844, #34136, #42945 ) ) ;
#80617 = ORIENTED_EDGE ( 'NONE', *, *, #33966, .T. ) ;
#80618 = VECTOR ( 'NONE', #77261, 1000.000000000000114 ) ;
#80620 = DIRECTION ( 'NONE',  ( 0.4999999999999998890, -0.8660254037844385966, 0.000000000000000000 ) ) ;
#80619 = CARTESIAN_POINT ( 'NONE',  ( 207.1158949475991164, 271.9117422260973740, -5.823035679195911918 ) ) ;
#80621 = CARTESIAN_POINT ( 'NONE',  ( 149.1004267900891307, 272.3974806997987343, -12.86882154300063341 ) ) ;
#80622 = VERTEX_POINT ( 'NONE', #62866 ) ;
#80623 = CARTESIAN_POINT ( 'NONE',  ( 152.9251141908703175, 265.7729277985770864, -16.20110192949203309 ) ) ;
#80624 = CARTESIAN_POINT ( 'NONE',  ( 159.4285914931787431, 254.5085746851079023, 15.41072477910873673 ) ) ;
#80625 = CARTESIAN_POINT ( 'NONE',  ( 71.59249531027893454, 71.81680186753220596, -4.291330315329808798 ) ) ;
#80626 = CARTESIAN_POINT ( 'NONE',  ( 77.87641386972968860, 61.39850456329286743, -16.14647179981831115 ) ) ;
#80627 = EDGE_CURVE ( 'NONE', #53524, #95233, #14374, .T. ) ;
#80628 = CARTESIAN_POINT ( 'NONE',  ( 205.0716081116550527, 275.4525508911965517, -12.57761053684872188 ) ) ;
#80629 = CARTESIAN_POINT ( 'NONE',  ( 114.7887934315897382, 227.8923013555410080, 4.594050593750050204 ) ) ;
#80630 = DIRECTION ( 'NONE',  ( -0.8660254037844379305, -0.5000000000000014433, -0.000000000000000000 ) ) ;
#80631 = CARTESIAN_POINT ( 'NONE',  ( 70.51298433951257039, 211.5177522451418497, -10.00000000000009592 ) ) ;
#80632 = ORIENTED_EDGE ( 'NONE', *, *, #67984, .T. ) ;
#80633 = CARTESIAN_POINT ( 'NONE',  ( 208.2175703429120688, 270.0035844679667889, 2.257951022351344150 ) ) ;
#80634 = ORIENTED_EDGE ( 'NONE', *, *, #89614, .F. ) ;
#80635 = CARTESIAN_POINT ( 'NONE',  ( 32.22500930073565684, 40.64646525600392835, -2.839279412974133887 ) ) ;
#80636 = FACE_BOUND ( 'NONE', #8587, .T. ) ;
#80637 = CARTESIAN_POINT ( 'NONE',  ( 78.60031580754363745, 47.91716149375564981, -14.46830116769540275 ) ) ;
#80638 = CARTESIAN_POINT ( 'NONE',  ( 69.07880331415105957, 204.5643266524160424, 9.188101187500095079 ) ) ;
#80639 = PLANE ( 'NONE',  #65941 ) ;
#80640 = CARTESIAN_POINT ( 'NONE',  ( 190.8860811105559208, 300.0226043892405414, 8.636347304323541252 ) ) ;
#80641 = CARTESIAN_POINT ( 'NONE',  ( 198.1444248750829047, 287.4507842102791528, 18.42558436659502519 ) ) ;
#80642 = CARTESIAN_POINT ( 'NONE',  ( 172.9572136869028611, 277.5233305075546468, 16.75252092567692230 ) ) ;
#80643 = ORIENTED_EDGE ( 'NONE', *, *, #83127, .F. ) ;
#80644 = CARTESIAN_POINT ( 'NONE',  ( 80.19198528322290542, 56.53738137329634839, -16.16019141255892677 ) ) ;
#80645 = CARTESIAN_POINT ( 'NONE',  ( 189.8238368927809745, 301.8624653444729802, -0.3620111495846872751 ) ) ;
#80646 = VECTOR ( 'NONE', #34771, 1000.000000000000114 ) ;
#80647 = ORIENTED_EDGE ( 'NONE', *, *, #92560, .T. ) ;
#80648 = CARTESIAN_POINT ( 'NONE',  ( 152.3249143222120381, 268.8125044657937792, -15.54600960379902297 ) ) ;
#80649 = CARTESIAN_POINT ( 'NONE',  ( 69.28395859784794197, 69.63058245955254222, -5.196709074601549183 ) ) ;
#80650 = CARTESIAN_POINT ( 'NONE',  ( 160.4244049798018352, 258.1628759096047361, -17.08294313303711220 ) ) ;
#80651 = CARTESIAN_POINT ( 'NONE',  ( 206.5208294064731547, 270.6477873296462349, 2.445619694122634247 ) ) ;
#80652 = CARTESIAN_POINT ( 'NONE',  ( 190.4249800432324662, 300.8212548652687133, 3.085047376053959400 ) ) ;
#80653 = VECTOR ( 'NONE', #26670, 999.9999999999998863 ) ;
#80654 = CARTESIAN_POINT ( 'NONE',  ( 176.9795028420571441, 269.8566753081326510, 16.40411541806681583 ) ) ;
#80655 = CARTESIAN_POINT ( 'NONE',  ( 164.4261001824251878, 245.8526357240660900, 1.583002802772015549 ) ) ;
#80656 = CARTESIAN_POINT ( 'NONE',  ( 130.2687372006388671, 246.0177522451418497, -10.00000000000009592 ) ) ;
#80657 = CARTESIAN_POINT ( 'NONE',  ( 165.7657002015311889, 255.3986422146142274, 13.84715179042893141 ) ) ;
#80658 = ORIENTED_EDGE ( 'NONE', *, *, #78282, .T. ) ;
#80659 = CYLINDRICAL_SURFACE ( 'NONE', #22132, 17.82106496071139645 ) ;
#80660 = CIRCLE ( 'NONE', #90344, 45.00000000000000000 ) ;
#80661 = CARTESIAN_POINT ( 'NONE',  ( 130.3772506997096343, 236.8923013555409796, 4.594050593750050204 ) ) ;
#80662 = ORIENTED_EDGE ( 'NONE', *, *, #24680, .T. ) ;
#80663 = CARTESIAN_POINT ( 'NONE',  ( 191.2211340522693774, 299.4422756709672626, -8.405362570633277741 ) ) ;
#80664 = CARTESIAN_POINT ( 'NONE',  ( 83.97456745667967937, 42.10302139383830422, 2.974818707872815882 ) ) ;
#80665 = EDGE_CURVE ( 'NONE', #58510, #52122, #2090, .T. ) ;
#80666 = LINE ( 'NONE', #11243, #94287 ) ;
#80667 = CARTESIAN_POINT ( 'NONE',  ( 204.9768178125733016, 275.6167325052707611, 13.98665089523138505 ) ) ;
#80668 = CARTESIAN_POINT ( 'NONE',  ( 0.8646476260778407363, 159.7592609112380444, 2.679491924311254714 ) ) ;
#80669 = CARTESIAN_POINT ( 'NONE',  ( 178.0531015906397840, 255.3758172151866574, 4.758062337834783051 ) ) ;
#80670 = ORIENTED_EDGE ( 'NONE', *, *, #11107, .F. ) ;
#80671 = CARTESIAN_POINT ( 'NONE',  ( 80.14460775109067470, 57.42271260518928244, -16.59269094194095473 ) ) ;
#80672 = VECTOR ( 'NONE', #28808, 1000.000000000000000 ) ;
#80673 = CARTESIAN_POINT ( 'NONE',  ( 158.5045327573800478, 274.9905139280085109, -12.52208736651823884 ) ) ;
#80675 = DIRECTION ( 'NONE',  ( 0.5000000000000013323, -0.8660254037844378194, 0.000000000000000000 ) ) ;
#80674 = CARTESIAN_POINT ( 'NONE',  ( 19.39999966495784989, 36.48715600906564305, -10.00000000000000000 ) ) ;
#80676 = CARTESIAN_POINT ( 'NONE',  ( 164.3883575065421496, 245.9180079563093955, -2.230252308397467687 ) ) ;
#80677 = ADVANCED_FACE ( 'NONE', ( #8678 ), #47165, .T. ) ;
#80678 = CARTESIAN_POINT ( 'NONE',  ( 136.0332187963529975, 249.3458772461660544, 9.188101187500095079 ) ) ;
#80679 = EDGE_CURVE ( 'NONE', #35085, #54157, #18542, .T. ) ;
#80680 = CARTESIAN_POINT ( 'NONE',  ( 29.44348595096431609, 176.2592609112380444, 2.679491924311254714 ) ) ;
#80681 = CARTESIAN_POINT ( 'NONE',  ( -19.65312891409030271, 93.06504152958497400, 40.00000000000000000 ) ) ;
#80682 = CARTESIAN_POINT ( 'NONE',  ( 58.09093245575348874, 204.3458772461660544, 9.188101187500095079 ) ) ;
#80683 = CARTESIAN_POINT ( 'NONE',  ( 205.3943609285979051, 274.8935266139653777, -13.14270440534009943 ) ) ;
#80684 = CARTESIAN_POINT ( 'NONE',  ( 174.0516803220720021, 252.0920059681404553, 3.469221368822683615 ) ) ;
#80685 = CARTESIAN_POINT ( 'NONE',  ( 14.21206617776240044, 23.90829794293879118, 10.00000000000000355 ) ) ;
#80686 = CARTESIAN_POINT ( 'NONE',  ( 149.3883679478359454, 271.8987519849911223, 12.99187507659642371 ) ) ;
#80687 = CARTESIAN_POINT ( 'NONE',  ( 155.3185930247096280, 279.9023224415089999, -1.077172130989042520 ) ) ;
#80688 = CARTESIAN_POINT ( 'NONE',  ( 171.7676654267511935, 286.7502147520581275, -8.058579322952500235 ) ) ;
#80689 = CARTESIAN_POINT ( 'NONE',  ( 154.9903553346911735, 262.1958252075976361, -18.39016733948542637 ) ) ;
#80690 = CARTESIAN_POINT ( 'NONE',  ( 157.4489004501168097, 270.9419718275721038, -14.71794672505381385 ) ) ;
#80691 = AXIS2_PLACEMENT_3D ( 'NONE', #23423, #24442, #61429 ) ;
#80692 = CARTESIAN_POINT ( 'NONE',  ( 134.1658515176688127, 258.2677522451419350, -5.000000000000047962 ) ) ;
#80693 = CARTESIAN_POINT ( 'NONE',  ( 82.70224374152380165, 51.20310041363545395, -14.45093331327230146 ) ) ;
#80694 = ORIENTED_EDGE ( 'NONE', *, *, #18828, .T. ) ;
#80695 = DIRECTION ( 'NONE',  ( -0.000000000000000000, 0.000000000000000000, -1.000000000000000000 ) ) ;
#80696 = CARTESIAN_POINT ( 'NONE',  ( 190.2476911738421848, 301.1283281946692796, -1.360079143321618611 ) ) ;
#80697 = CARTESIAN_POINT ( 'NONE',  ( -2.449395605728673875, 160.2048013555409796, 4.594050593750051981 ) ) ;
#80698 = VECTOR ( 'NONE', #16840, 1000.000000000000114 ) ;
#80699 = CARTESIAN_POINT ( 'NONE',  ( 39.87759600423577666, 184.6423013555410080, -4.594050593750043987 ) ) ;
#80700 = CARTESIAN_POINT ( 'NONE',  ( 178.7014608347196827, 259.1862871959719428, -11.32543599931723222 ) ) ;
#80701 = CARTESIAN_POINT ( 'NONE',  ( 25.36820930315042943, 19.81029122506294726, 8.090169943749479842 ) ) ;
#80702 = CARTESIAN_POINT ( 'NONE',  ( 85.94797495143531307, 48.32083425265168586, 12.00338787116683470 ) ) ;
#80703 = CARTESIAN_POINT ( 'NONE',  ( 205.1300674467857164, 275.3512963525735131, -12.60245643603069610 ) ) ;
#80704 = CARTESIAN_POINT ( 'NONE',  ( 72.07791713363762653, 72.33007614824393272, -3.421992246486540434 ) ) ;
#80705 = CARTESIAN_POINT ( 'NONE',  ( 146.8195026170398023, 276.3481572557323034, 4.765869558735466249 ) ) ;
#80706 = CARTESIAN_POINT ( 'NONE',  ( 73.76715751097611928, 55.18302132200656018, -16.59786953572997348 ) ) ;
#80708 = CARTESIAN_POINT ( 'NONE',  ( 48.86234924490155862, 209.0177522451419065, 5.000000000000046185 ) ) ;
#80707 = CARTESIAN_POINT ( 'NONE',  ( 171.3866751883526831, 258.3865106268564773, 14.16928307686719712 ) ) ;
#80709 = CARTESIAN_POINT ( 'NONE',  ( 74.78830374546942039, 67.19102293627160805, 12.47204474763305093 ) ) ;
#80710 = CARTESIAN_POINT ( 'NONE',  ( 49.09806598349715046, 107.5461990276917845, -10.00000000000000000 ) ) ;
#80711 = CARTESIAN_POINT ( 'NONE',  ( 41.71240375114938814, 62.05720181600818108, -10.00000000000000000 ) ) ;
#80712 =( BOUNDED_CURVE ( )  B_SPLINE_CURVE ( 2, ( #94728, #7593, #38481, #69395, #999, #11, #46578, #30895, #8106, #23280, #93226, #54169, #77515 ),
 .UNSPECIFIED., .F., .T. ) 
 B_SPLINE_CURVE_WITH_KNOTS ( ( 3, 2, 2, 2, 2, 2, 3 ),
 ( 0.7375000000000000444, 0.7399999999999999911, 0.7449999999999999956, 0.7500000000000000000, 0.7550000000000000044, 0.7600000000000000089, 0.7625000000000000666 ),
 .UNSPECIFIED. ) 
 CURVE ( )  GEOMETRIC_REPRESENTATION_ITEM ( )  RATIONAL_B_SPLINE_CURVE ( ( 0.9755282581475767101, 0.9755282581475772652, 1.000000000000000000, 0.9510565162951535312, 1.000000000000000000, 0.9510565162951535312, 1.000000000000000000, 0.9510565162951535312, 1.000000000000000000, 0.9510565162951535312, 1.000000000000000000, 0.9755282581475761550, 0.9755282581475767101 ) ) 
 REPRESENTATION_ITEM ( '' )  );
#80713 = B_SPLINE_CURVE_WITH_KNOTS ( 'NONE', 3,
 ( #84501, #98187, #61647, #83008, #36861, #76854, #5474, #7450, #13580, #75384 ),
 .UNSPECIFIED., .F., .F.,
 ( 4, 2, 2, 2, 4 ),
 ( 0.000000000000000000, 0.2500000000000000000, 0.5000000000000000000, 0.7500000000000000000, 1.000000000000000000 ),
 .UNSPECIFIED. ) ;
#80714 = CARTESIAN_POINT ( 'NONE',  ( 161.8918814713609891, 267.1929759636259405, 16.48806508481699140 ) ) ;
#80715 = CARTESIAN_POINT ( 'NONE',  ( 44.18942050719595471, 202.9865022471903160, 10.00000000000009237 ) ) ;
#80716 = CARTESIAN_POINT ( 'NONE',  ( -19.92236680055716391, 153.5313752282681605, 5.249404841173988696E-14 ) ) ;
#80717 = CARTESIAN_POINT ( 'NONE',  ( 164.9959905715102479, 284.7368986600080234, -7.507006057201434324 ) ) ;
#80718 = VECTOR ( 'NONE', #5383, 1000.000000000000000 ) ;
#80719 = CARTESIAN_POINT ( 'NONE',  ( 2.746756816977958593, 163.2048013555410080, 4.594050593750051981 ) ) ;
#80720 = CARTESIAN_POINT ( 'NONE',  ( 36.89851624356406745, 36.70171378149922248, -9.188101187500004485 ) ) ;
#80721 = B_SPLINE_CURVE_WITH_KNOTS ( 'NONE', 3,
 ( #65569, #42257, #4266, #28061 ),
 .UNSPECIFIED., .F., .F.,
 ( 4, 4 ),
 ( 0.03005457668816597858, 0.03915685978210869944 ),
 .UNSPECIFIED. ) ;
#80722 = CARTESIAN_POINT ( 'NONE',  ( 164.6637257444425302, 246.8187871797005926, 5.850462324949956106 ) ) ;
#80723 = CARTESIAN_POINT ( 'NONE',  ( 153.4578721839791342, 264.8501638863745029, 16.85421393845643223 ) ) ;
#80724 = CARTESIAN_POINT ( 'NONE',  ( 33.97448420766330202, 31.56628583063843152, 9.188101187500006262 ) ) ;
#80725 = CARTESIAN_POINT ( 'NONE',  ( 73.95673202641080479, 225.0530062829863311, -4.648177544792955347E-16 ) ) ;
#80726 = CARTESIAN_POINT ( 'NONE',  ( 183.2734392787317290, 278.9810903348750344, 16.96010398477730519 ) ) ;
#80727 = LINE ( 'NONE', #81216, #36740 ) ;
#80728 = DIRECTION ( 'NONE',  ( -0.9184028970038814466, -0.3956464567955564338, 0.000000000000000000 ) ) ;
#80729 = CARTESIAN_POINT ( 'NONE',  ( 179.3470654816431136, 262.5477174050944882, -12.85649373009148277 ) ) ;
#80730 = DIRECTION ( 'NONE',  ( 1.000000000000000000, 0.000000000000000000, 0.000000000000000000 ) ) ;
#80731 = CIRCLE ( 'NONE', #53189, 17.82106496071138224 ) ;
#80732 = CARTESIAN_POINT ( 'NONE',  ( 2.405479210251257438, 24.49540643055184930, 3.479690158560446702E-15 ) ) ;
#80733 = CARTESIAN_POINT ( 'NONE',  ( 168.6642430148957885, 288.2074250805146107, 0.5276533672608759717 ) ) ;
#80734 = CARTESIAN_POINT ( 'NONE',  ( 11.76515913632831101, 28.83396525600389282, -2.839279412974133887 ) ) ;
#80735 = CARTESIAN_POINT ( 'NONE',  ( 76.44090856289290059, 203.3932355074535963, -2.679491924311248496 ) ) ;
#80736 = EDGE_CURVE ( 'NONE', #46169, #70584, #94317, .T. ) ;
#80737 = CARTESIAN_POINT ( 'NONE',  ( 84.14312167556933275, 48.98415679381830756, 0.000000000000000000 ) ) ;
#80738 = VECTOR ( 'NONE', #93040, 1000.000000000000000 ) ;
#80739 = CARTESIAN_POINT ( 'NONE',  ( 156.6823154307097070, 276.4438179710489862, 10.26594267860235554 ) ) ;
#80740 = CARTESIAN_POINT ( 'NONE',  ( 159.2122473525774069, 254.8832937285494609, -16.22689353966294590 ) ) ;
#80741 = LINE ( 'NONE', #11314, #15452 ) ;
#80742 = EDGE_CURVE ( 'NONE', #10473, #77961, #63875, .T. ) ;
#80743 = ORIENTED_EDGE ( 'NONE', *, *, #43638, .T. ) ;
#80744 = CARTESIAN_POINT ( 'NONE',  ( 34.81516168915606357, 51.10768172523390973, -10.00000000000000000 ) ) ;
#80745 = CARTESIAN_POINT ( 'NONE',  ( 164.2578067403839555, 246.1441285162624126, -2.322300236470859591 ) ) ;
#80746 = CARTESIAN_POINT ( 'NONE',  ( 66.13301673674520487, 68.52568730408864894, 4.698905408680452922 ) ) ;
#80747 = CARTESIAN_POINT ( 'NONE',  ( 87.59998515009166908, 45.09196136326725224, 6.914658723149486264 ) ) ;
#80748 = VERTEX_POINT ( 'NONE', #17273 ) ;
#80749 = AXIS2_PLACEMENT_3D ( 'NONE', #38671, #7781, #68080 ) ;
#80750 = ORIENTED_EDGE ( 'NONE', *, *, #33134, .F. ) ;
#80752 = DIRECTION ( 'NONE',  ( 0.4999999999999992784, -0.8660254037844390407, 0.000000000000000000 ) ) ;
#80751 = CARTESIAN_POINT ( 'NONE',  ( 165.3118168859175796, 246.3185293925050701, -4.432402497422931020 ) ) ;
#80753 = CARTESIAN_POINT ( 'NONE',  ( 85.92471682701912528, 47.57321576112601491, 10.85901928151990958 ) ) ;
#80754 = ORIENTED_EDGE ( 'NONE', *, *, #2178, .T. ) ;
#80755 = CARTESIAN_POINT ( 'NONE',  ( 78.26871893555610882, 61.06000381536296118, 15.88849461485118297 ) ) ;
#80756 = CARTESIAN_POINT ( 'NONE',  ( 174.4138743697411371, 262.4381095864849840, 14.53967419496388658 ) ) ;
#80758 = ADVANCED_FACE ( 'NONE', ( #1599 ), #56265, .T. ) ;
#80757 = ORIENTED_EDGE ( 'NONE', *, *, #95672, .F. ) ;
#80759 = CARTESIAN_POINT ( 'NONE',  ( -0.3272207041121033000, 38.43844835668754456, 59.99999999999999289 ) ) ;
#80760 = CARTESIAN_POINT ( 'NONE',  ( 77.15553965011207538, 50.73118323507032557, -15.35405348121969560 ) ) ;
#80761 = CARTESIAN_POINT ( 'NONE',  ( 80.81174745787325264, 43.46938007122601277, 9.396612886052723823 ) ) ;
#80762 = ORIENTED_EDGE ( 'NONE', *, *, #66773, .T. ) ;
#80763 = CARTESIAN_POINT ( 'NONE',  ( 161.7101619467568980, 250.5567787384628389, 13.05644392949610655 ) ) ;
#80764 = CARTESIAN_POINT ( 'NONE',  ( 166.3426357552802983, 274.2843506083544298, -15.18163831355469107 ) ) ;
#80765 = CARTESIAN_POINT ( 'NONE',  ( -17.42236680055705023, 149.2012482093457777, 0.000000000000000000 ) ) ;
#80766 = B_SPLINE_SURFACE_WITH_KNOTS ( 'NONE', 3, 1, ( 
 ( #74520, #5099 ),
 ( #16055, #36980 ),
 ( #92595, #44068 ),
 ( #28898, #75502 ),
 ( #82651, #98309 ),
 ( #13210, #69748 ),
 ( #69251, #28382 ),
 ( #58770, #66883 ),
 ( #89741, #20305 ),
 ( #51178, #97814 ),
 ( #59261, #84990 ),
 ( #90239, #20810 ),
 ( #7969, #359 ),
 ( #67382, #62133 ),
 ( #85508, #51702 ),
 ( #31246, #75008 ),
 ( #82146, #43585 ),
 ( #23141, #54527 ),
 ( #23635, #5588 ),
 ( #54034, #77364 ),
 ( #6087, #36478 ),
 ( #90743, #21300 ),
 ( #46956, #8458 ),
 ( #52175, #83123 ),
 ( #44567, #64156 ),
 ( #56552, #55532 ),
 ( #57042, #95107 ),
 ( #33783, #80406 ),
 ( #64668, #41848 ),
 ( #48463, #26165 ),
 ( #32750, #25671 ),
 ( #71276, #10977 ),
 ( #87025, #95617 ),
 ( #86024, #853 ) ),
 .UNSPECIFIED., .T., .F., .F.,
 ( 4, 2, 2, 2, 2, 2, 2, 2, 2, 2, 2, 2, 2, 2, 2, 2, 4 ),
 ( 2, 2 ),
 ( 0.000000000000000000, 0.06250000000000000000, 0.1250000000000000000, 0.1875000000000000000, 0.2500000000000000000, 0.3125000000000000000, 0.3750000000000000000, 0.4375000000000000000, 0.5000000000000000000, 0.5625000000000000000, 0.6250000000000000000, 0.6875000000000000000, 0.7500000000000000000, 0.8125000000000000000, 0.8750000000000000000, 0.9375000000000000000, 1.000000000000000000 ),
 ( 0.000000000000000000, 1.000000000000000000 ),
 .UNSPECIFIED. ) ;
#80767 = VERTEX_POINT ( 'NONE', #43562 ) ;
#80768 = CARTESIAN_POINT ( 'NONE',  ( 174.5488994031076970, 277.2909221230937646, -15.64416576916768165 ) ) ;
#80769 = ADVANCED_FACE ( 'NONE', ( #65861 ), #29619, .T. ) ;
#80770 = ORIENTED_EDGE ( 'NONE', *, *, #30786, .T. ) ;
#80771 = EDGE_CURVE ( 'NONE', #46611, #94086, #16830, .T. ) ;
#80772 = CARTESIAN_POINT ( 'NONE',  ( 156.8809214077219281, 266.3341492759256539, -16.38455355822726389 ) ) ;
#80773 = VERTEX_POINT ( 'NONE', #13673 ) ;
#80774 = DIRECTION ( 'NONE',  ( -0.7713848165480284846, 0.6363689690731033632, 0.000000000000000000 ) ) ;
#80775 = ORIENTED_EDGE ( 'NONE', *, *, #3280, .F. ) ;
#80776 = CARTESIAN_POINT ( 'NONE',  ( 147.1780374576129589, 275.7271566955758999, 6.941191638535834763 ) ) ;
#80777 = CARTESIAN_POINT ( 'NONE',  ( 176.8917175299031896, 289.5346434493817469, -10.53293604869262978 ) ) ;
#80778 = CARTESIAN_POINT ( 'NONE',  ( 69.96053279364318200, 66.30487250405448663, 10.70721000888415020 ) ) ;
#80779 = CARTESIAN_POINT ( 'NONE',  ( 199.7320992005288360, 281.1146086494965175, -17.28530500821910820 ) ) ;
#80780 = CARTESIAN_POINT ( 'NONE',  ( 175.6385077117528226, 290.1657555888949673, 6.156910366948349811 ) ) ;
#80781 = CARTESIAN_POINT ( 'NONE',  ( 197.3013163403698798, 288.9110910286968306, -18.25968461953811328 ) ) ;
#80782 = ORIENTED_EDGE ( 'NONE', *, *, #68344, .T. ) ;
#80783 = DIRECTION ( 'NONE',  ( -0.5000000000000003331, 0.8660254037844383745, 0.000000000000000000 ) ) ;
#80784 = CARTESIAN_POINT ( 'NONE',  ( 30.25295400085950703, 18.26216523072495690, -2.296566073217252530E-15 ) ) ;
#80785 = CARTESIAN_POINT ( 'NONE',  ( 206.3106310032756596, 273.3065002911688453, 10.17860425536756175 ) ) ;
#80787 = CARTESIAN_POINT ( 'NONE',  ( 205.8379285891498682, 274.1252448892948905, 10.44730901608240181 ) ) ;
#80786 = CARTESIAN_POINT ( 'NONE',  ( 77.43554664961604317, 49.73530731850063802, -15.48705580038115848 ) ) ;
#80788 = CARTESIAN_POINT ( 'NONE',  ( 159.9628729326222754, 253.5831720864507588, 15.75051413866357386 ) ) ;
#80789 = ORIENTED_EDGE ( 'NONE', *, *, #99796, .T. ) ;
#80790 = CARTESIAN_POINT ( 'NONE',  ( 146.7539121514467695, 276.4617632746314371, -2.866763085982500403 ) ) ;
#80791 = EDGE_CURVE ( 'NONE', #77592, #23277, #4694, .T. ) ;
#80792 = CARTESIAN_POINT ( 'NONE',  ( 171.5798264516812424, 259.4877759030353559, -13.89750514209113064 ) ) ;
#80793 = CARTESIAN_POINT ( 'NONE',  ( 164.3996301846870267, 247.3020492865104529, 7.248807534621905191 ) ) ;
#80794 = CARTESIAN_POINT ( 'NONE',  ( -38.02969130575858259, 25.52022711230254970, 10.00000000000000000 ) ) ;
#80795 = CARTESIAN_POINT ( 'NONE',  ( 160.6390625115447222, 252.4119773802086968, -15.11156539429256362 ) ) ;
#80796 = CARTESIAN_POINT ( 'NONE',  ( 91.89298649898879034, 233.8615022471903160, 5.000000000000046185 ) ) ;
#80797 = ORIENTED_EDGE ( 'NONE', *, *, #92994, .F. ) ;
#80799 = EDGE_CURVE ( 'NONE', #941, #65003, #9492, .T. ) ;
#80798 = CARTESIAN_POINT ( 'NONE',  ( 182.2991478702006134, 275.2734891516705034, -17.80812521087705846 ) ) ;
#80800 = CARTESIAN_POINT ( 'NONE',  ( 14.47246418079440389, 8.759783934591627741, -1.583844403245366905 ) ) ;
#80801 = LINE ( 'NONE', #81285, #98121 ) ;
#80802 = VECTOR ( 'NONE', #6843, 1000.000000000000000 ) ;
#80803 = DIRECTION ( 'NONE',  ( 0.000000000000000000, 0.000000000000000000, 1.000000000000000000 ) ) ;
#80804 = CARTESIAN_POINT ( 'NONE',  ( 29.01593374150824189, 180.8927522451417929, -10.00000000000009059 ) ) ;
#80805 = CARTESIAN_POINT ( 'NONE',  ( 103.0163473728362504, 218.0327760586659451, 1.948934522072302763E-15 ) ) ;
#80806 = CARTESIAN_POINT ( 'NONE',  ( 180.7869751407568231, 294.0814949767770941, -2.848415450199388577 ) ) ;
#80807 = VECTOR ( 'NONE', #21025, 1000.000000000000000 ) ;
#80808 = ADVANCED_FACE ( 'NONE', ( #37444 ), #67869, .T. ) ;
#80809 = CARTESIAN_POINT ( 'NONE',  ( -13.11024591527734628, 27.99999999999999645, 17.00000000000000000 ) ) ;
#80810 = CARTESIAN_POINT ( 'NONE',  ( 208.1864700626310025, 270.0574517335433598, 2.990990977286084096 ) ) ;
#80811 = CIRCLE ( 'NONE', #93501, 10.99999999999989164 ) ;
#80812 = CARTESIAN_POINT ( 'NONE',  ( 17.98295739510416524, 187.3149278399160949, -9.188101187500095079 ) ) ;
#80813 = EDGE_CURVE ( 'NONE', #80879, #44657, #20445, .T. ) ;
#80814 = CARTESIAN_POINT ( 'NONE',  ( 25.95703985525452850, 15.39040679176983240, 1.333680081654574804E-15 ) ) ;
#80815 = ORIENTED_EDGE ( 'NONE', *, *, #47859, .F. ) ;
#80816 = VECTOR ( 'NONE', #76864, 1000.000000000000227 ) ;
#80817 = ORIENTED_EDGE ( 'NONE', *, *, #20929, .F. ) ;
#80818 = ADVANCED_FACE ( 'NONE', ( #77476 ), #32093, .F. ) ;
#80819 = CARTESIAN_POINT ( 'NONE',  ( 185.1518460011666889, 259.9031676633314873, -5.660721190095883593 ) ) ;
#80820 = EDGE_CURVE ( 'NONE', #5854, #59206, #78396, .T. ) ;
#80821 = CARTESIAN_POINT ( 'NONE',  ( 88.20356954673827943, 44.10112916931887383, 0.5196327138970232573 ) ) ;
#80822 = CARTESIAN_POINT ( 'NONE',  ( 205.2564848266901834, 271.9733254596621350, -9.597888780111448526 ) ) ;
#80823 = CARTESIAN_POINT ( 'NONE',  ( 69.68017357788663446, 198.3352228055616706, 5.322883649122824736E-14 ) ) ;
#80824 = CARTESIAN_POINT ( 'NONE',  ( 182.2583020200309818, 284.4576732326586921, 14.88072139987983711 ) ) ;
#80825 = CARTESIAN_POINT ( 'NONE',  ( 106.0921946783233096, 225.3927522451418213, 10.00000000000009948 ) ) ;
#80826 = CARTESIAN_POINT ( 'NONE',  ( 45.42531092540608029, 197.0333772461660828, 9.188101187500095079 ) ) ;
#80827 = CARTESIAN_POINT ( 'NONE',  ( 82.20432729060244981, 228.2677522451419350, -5.000000000000047962 ) ) ;
#80828 = ORIENTED_EDGE ( 'NONE', *, *, #91055, .F. ) ;
#80829 = CARTESIAN_POINT ( 'NONE',  ( 150.0694502760089222, 271.4680435213315945, -12.17790201236558545 ) ) ;
#80830 = CARTESIAN_POINT ( 'NONE',  ( 158.7081735734057872, 282.4546237173937016, -1.655763827236318209 ) ) ;
#80831 = VECTOR ( 'NONE', #11419, 1000.000000000000114 ) ;
#80832 = CARTESIAN_POINT ( 'NONE',  ( -0.2032289886040369309, 164.5643266524160140, -9.188101187500093303 ) ) ;
#80833 = CARTESIAN_POINT ( 'NONE',  ( 68.48614760541654789, 64.37018547164757365, -12.30469093693554150 ) ) ;
#80834 = CARTESIAN_POINT ( 'NONE',  ( 150.6438662863770332, 269.7241650738195631, -14.92510732909997628 ) ) ;
#80835 = LINE ( 'NONE', #57459, #85642 ) ;
#80836 = CARTESIAN_POINT ( 'NONE',  ( 147.2658550951450422, 275.5750520855697800, -5.215660180131691526 ) ) ;
#80837 = FACE_OUTER_BOUND ( 'NONE', #17269, .T. ) ;
#80838 = CARTESIAN_POINT ( 'NONE',  ( 204.0890941988925817, 276.4630862285632702, 13.35479316431303687 ) ) ;
#80839 = CARTESIAN_POINT ( 'NONE',  ( 147.1447476476323004, 275.7848163378367872, 0.6373001129109078233 ) ) ;
#80840 = CARTESIAN_POINT ( 'NONE',  ( 164.9779129355220562, 244.8968679994381148, -1.771286574179712803 ) ) ;
#80841 = ORIENTED_EDGE ( 'NONE', *, *, #41016, .T. ) ;
#80842 = CARTESIAN_POINT ( 'NONE',  ( -0.8439004895948557516, 176.9865022471903444, -10.00000000000009415 ) ) ;
#80843 = CARTESIAN_POINT ( 'NONE',  ( 83.36691583440136810, 43.49436753249096910, 8.332904630864705453 ) ) ;
#80844 = CARTESIAN_POINT ( 'NONE',  ( 113.3268549190559753, 245.4244531367911293, -4.594050593750046652 ) ) ;
#80845 = CARTESIAN_POINT ( 'NONE',  ( 25.00689474275853286, 16.29860640527292759, -2.839279412974138328 ) ) ;
#80846 = CARTESIAN_POINT ( 'NONE',  ( 74.83456390391278035, 67.20231954166843025, 12.48272054267759046 ) ) ;
#80847 = LINE ( 'NONE', #41269, #80831 ) ;
#80849 = CARTESIAN_POINT ( 'NONE',  ( -22.42236680055709641, 157.8615022471902591, 0.000000000000000000 ) ) ;
#80848 = CARTESIAN_POINT ( 'NONE',  ( 184.5194340083631346, 296.1660737835977102, -7.201245168507500516 ) ) ;
#80850 = CYLINDRICAL_SURFACE ( 'NONE', #80549, 16.60714546451156792 ) ;
#80851 = ORIENTED_EDGE ( 'NONE', *, *, #66425, .F. ) ;
#80852 = CARTESIAN_POINT ( 'NONE',  ( 151.0036289208911171, 269.1010379121764799, 14.24595189915657478 ) ) ;
#80853 = CARTESIAN_POINT ( 'NONE',  ( 149.0164813726494799, 272.5428784278667536, -11.67305721329070423 ) ) ;
#80854 = CARTESIAN_POINT ( 'NONE',  ( -43.70040200909112116, 27.32518560721127088, 10.00000000000000000 ) ) ;
#80855 = CARTESIAN_POINT ( 'NONE',  ( 173.1997439627015467, 289.7296588321038939, -1.111478199152324375 ) ) ;
#80856 = CARTESIAN_POINT ( 'NONE',  ( 81.71476302640699885, 55.72971451982099467, -15.98982683184117448 ) ) ;
#80857 = ORIENTED_EDGE ( 'NONE', *, *, #25618, .T. ) ;
#80858 = CARTESIAN_POINT ( 'NONE',  ( 189.1697036996914960, 265.4656734670753053, 11.91601115033013514 ) ) ;
#80859 = CARTESIAN_POINT ( 'NONE',  ( 165.4340772170561991, 269.7433133579526157, -16.28799140846306415 ) ) ;
#80860 = CARTESIAN_POINT ( 'NONE',  ( 71.87514149713709344, 72.22094621771665857, 0.5828543197166242695 ) ) ;
#80861 = CARTESIAN_POINT ( 'NONE',  ( 84.75074989694867611, 43.95653813994506720, 6.843521681741808749 ) ) ;
#80862 = CARTESIAN_POINT ( 'NONE',  ( 199.9868610850537607, 272.4588406731110126, 12.49652601812552533 ) ) ;
#80863 = CARTESIAN_POINT ( 'NONE',  ( 50.51697681462041345, 96.61285555410614734, 10.00000000000000000 ) ) ;
#80864 = CARTESIAN_POINT ( 'NONE',  ( 71.98137461515177904, 71.49844079294172161, -5.753101040561137580 ) ) ;
#80865 = CARTESIAN_POINT ( 'NONE',  ( 148.0808017092188607, 274.9439814809830409, 5.964600266013551533 ) ) ;
#80866 = ORIENTED_EDGE ( 'NONE', *, *, #66320, .F. ) ;
#80867 = CARTESIAN_POINT ( 'NONE',  ( 29.12701137275935181, 44.61184105132205957, 10.00000000000000000 ) ) ;
#80868 = CARTESIAN_POINT ( 'NONE',  ( 8.974214183003983436, 13.38052372038638538, 10.00000000000000533 ) ) ;
#80869 = CARTESIAN_POINT ( 'NONE',  ( -19.65312891409030271, 93.06504152958497400, 177.5919119679930134 ) ) ;
#80870 = EDGE_LOOP ( 'NONE', ( #68467, #77880, #65277, #51449 ) ) ;
#80871 = CARTESIAN_POINT ( 'NONE',  ( 164.4183836189802435, 279.4556777148490028, 11.95241060903501484 ) ) ;
#80872 = CARTESIAN_POINT ( 'NONE',  ( 147.6884207308302450, 274.8431469350302336, -8.096293592099874203 ) ) ;
#80873 = CARTESIAN_POINT ( 'NONE',  ( 156.0226403810962097, 261.9271281158086140, -16.96797176191799394 ) ) ;
#80875 = EDGE_CURVE ( 'NONE', #23251, #59397, #65743, .T. ) ;
#80874 = EDGE_LOOP ( 'NONE', ( #48364, #93471, #43712, #30139 ) ) ;
#80876 = VECTOR ( 'NONE', #59829, 1000.000000000000114 ) ;
#80877 = CARTESIAN_POINT ( 'NONE',  ( 79.27109561811333549, 59.78567773455861811, 16.51039248270449633 ) ) ;
#80878 = CARTESIAN_POINT ( 'NONE',  ( 204.9314961322898228, 273.1004059617595203, -9.763055590748432877 ) ) ;
#80879 = VERTEX_POINT ( 'NONE', #50059 ) ;
#80880 = VECTOR ( 'NONE', #22822, 1000.000000000000114 ) ;
#80881 = DIRECTION ( 'NONE',  ( 0.6118251767726274881, 0.7909930170786233505, 0.000000000000000000 ) ) ;
#80882 = CARTESIAN_POINT ( 'NONE',  ( 73.47333430897622009, 69.87645613598228067, -9.771583980831868743 ) ) ;
#80883 = CARTESIAN_POINT ( 'NONE',  ( 84.68112478133504339, 49.92754082849447883, -13.65492077727069820 ) ) ;
#80884 = CARTESIAN_POINT ( 'NONE',  ( 185.6713631041849055, 258.9584525764907426, -6.747383155299178092 ) ) ;
#80885 = ORIENTED_EDGE ( 'NONE', *, *, #69723, .F. ) ;
#80886 = EDGE_CURVE ( 'NONE', #79277, #54166, #38526, .T. ) ;
#80887 = ORIENTED_EDGE ( 'NONE', *, *, #4156, .T. ) ;
#80888 = DIRECTION ( 'NONE',  ( -0.8660254037844387076, -0.4999999999999998890, -0.000000000000000000 ) ) ;
#80889 = EDGE_CURVE ( 'NONE', #7425, #63624, #42924, .T. ) ;
#80890 = EDGE_LOOP ( 'NONE', ( #29958, #55245, #55726, #56094 ) ) ;
#80891 = CARTESIAN_POINT ( 'NONE',  ( 81.53393849378393554, 59.50339463092494441, -0.2795964517353782819 ) ) ;
#80892 = EDGE_LOOP ( 'NONE', ( #43778, #89148, #12973, #66162 ) ) ;
#80893 = DIRECTION ( 'NONE',  ( -0.000000000000000000, 0.000000000000000000, -1.000000000000000000 ) ) ;
#80895 = CARTESIAN_POINT ( 'NONE',  ( 202.8874463667715133, 279.2356300052831557, -15.29930322226033468 ) ) ;
#80894 = VECTOR ( 'NONE', #66356, 1000.000000000000114 ) ;
#80896 = ORIENTED_EDGE ( 'NONE', *, *, #32054, .T. ) ;
#80897 = CARTESIAN_POINT ( 'NONE',  ( 82.16505394594395284, 40.63743801994069571, 3.475557980665269664 ) ) ;
#80898 = CARTESIAN_POINT ( 'NONE',  ( 147.1439969174920464, 275.7861166405825770, -6.562009323313376719 ) ) ;
#80899 = CARTESIAN_POINT ( 'NONE',  ( 161.8890841478012135, 277.2149579922602243, -12.83564633500961882 ) ) ;
#80900 = CARTESIAN_POINT ( 'NONE',  ( 147.3379027498079381, 275.4502618871274535, -3.695260257281167249 ) ) ;
#80901 = CARTESIAN_POINT ( 'NONE',  ( 200.6583719735737645, 283.0965001081523269, -17.35266956530146132 ) ) ;
#80902 = CARTESIAN_POINT ( 'NONE',  ( 205.2564848266901834, 271.9733254596621350, -9.597888780111448526 ) ) ;
#80903 = DIRECTION ( 'NONE',  ( -0.8660254037844363761, -0.5000000000000039968, 0.000000000000000000 ) ) ;
#80904 = CARTESIAN_POINT ( 'NONE',  ( 135.7624123097878623, 255.3149278399160949, 9.188101187500093303 ) ) ;
#80905 = CARTESIAN_POINT ( 'NONE',  ( 70.40520854310760512, 61.17034131612381032, -14.85613665266377836 ) ) ;
#80906 = CARTESIAN_POINT ( 'NONE',  ( 6.965323710529800927, 24.99752408145590366, 5.678558825948277544 ) ) ;
#80907 = ORIENTED_EDGE ( 'NONE', *, *, #17792, .T. ) ;
#80908 = VECTOR ( 'NONE', #71731, 1000.000000000000000 ) ;
#80910 = EDGE_LOOP ( 'NONE', ( #76447, #74467, #89839, #99799, #39902 ) ) ;
#80909 = CARTESIAN_POINT ( 'NONE',  ( 85.61005001132002690, 48.37664482377094544, -12.20733655019925479 ) ) ;
#80911 = CARTESIAN_POINT ( 'NONE',  ( -14.09895056762408494, 105.0318923338749642, 10.41638685176045698 ) ) ;
#80912 = CARTESIAN_POINT ( 'NONE',  ( -22.42236680055709641, 157.8615022471902591, 0.000000000000000000 ) ) ;
#80913 = AXIS2_PLACEMENT_3D ( 'NONE', #61803, #85159, #77537 ) ;
#80914 = CARTESIAN_POINT ( 'NONE',  ( 170.8882927430364020, 288.0602046512401557, -5.525210371943358290 ) ) ;
#80915 = CARTESIAN_POINT ( 'NONE',  ( 157.3345317626142048, 280.0779076120791160, -6.962135762735354838 ) ) ;
#80916 = DIRECTION ( 'NONE',  ( -0.8660254037844387076, -0.4999999999999998890, -0.000000000000000000 ) ) ;
#80917 = CARTESIAN_POINT ( 'NONE',  ( 171.3649617487770911, 251.0102673366500596, 7.372720983288576946 ) ) ;
#80918 = CARTESIAN_POINT ( 'NONE',  ( 168.2134749413384327, 253.2945090417912866, 11.62816938842056125 ) ) ;
#80919 = CARTESIAN_POINT ( 'NONE',  ( 195.0180713635390930, 292.4506560729497551, 15.11837988040635672 ) ) ;
#80920 = ORIENTED_EDGE ( 'NONE', *, *, #15071, .F. ) ;
#80922 = ADVANCED_FACE ( 'NONE', ( #27266 ), #58634, .T. ) ;
#80921 = DIRECTION ( 'NONE',  ( 0.000000000000000000, 0.000000000000000000, 1.000000000000000000 ) ) ;
#80923 = CARTESIAN_POINT ( 'NONE',  ( 66.13011622596867767, 68.75667804639587644, 0.07765751491501762804 ) ) ;
#80924 = ORIENTED_EDGE ( 'NONE', *, *, #66557, .F. ) ;
#80925 = CARTESIAN_POINT ( 'NONE',  ( 163.6306258414269621, 278.1771990602612163, 13.60634061194307520 ) ) ;
#80926 = EDGE_CURVE ( 'NONE', #65117, #33343, #88620, .T. ) ;
#80927 = EDGE_CURVE ( 'NONE', #8776, #51452, #81016, .T. ) ;
#80928 = CARTESIAN_POINT ( 'NONE',  ( 201.0972691433344437, 267.4835988171084864, -2.316786570161582404 ) ) ;
#80929 = CARTESIAN_POINT ( 'NONE',  ( 87.04122873496829982, 46.31593380912286761, -9.298662157179395038 ) ) ;
#80930 = CARTESIAN_POINT ( 'NONE',  ( 190.4163244163388242, 300.8362468508201459, 4.691083071570470331 ) ) ;
#80931 = CARTESIAN_POINT ( 'NONE',  ( 163.3854574543125580, 247.6550818016845597, 10.82482370245618775 ) ) ;
#80933 = CARTESIAN_POINT ( 'NONE',  ( 88.35595341439740480, 43.98873182231152157, 2.401576318819961919 ) ) ;
#80932 = CARTESIAN_POINT ( 'NONE',  ( 173.2337249902883798, 270.7486416191997023, 17.82094672905207133 ) ) ;
#80934 = CARTESIAN_POINT ( 'NONE',  ( 203.3277680582037590, 270.0362633623805664, 6.010087534169584522 ) ) ;
#80935 = ORIENTED_EDGE ( 'NONE', *, *, #58424, .F. ) ;
#80936 = CARTESIAN_POINT ( 'NONE',  ( 73.35598197599438208, 62.01013554246837600, -14.72002716710399817 ) ) ;
#80937 = EDGE_CURVE ( 'NONE', #43692, #76267, #35351, .T. ) ;
#80938 = CARTESIAN_POINT ( 'NONE',  ( 80.09759165418883242, 58.14035731840515098, 16.26729025684296204 ) ) ;
#80939 = CARTESIAN_POINT ( 'NONE',  ( 72.81152980648018058, 65.70600229248903190, -12.63635638373012782 ) ) ;
#80940 = CARTESIAN_POINT ( 'NONE',  ( -38.68484055605311056, 44.96122434458596473, 59.99999999999999289 ) ) ;
#80941 = CARTESIAN_POINT ( 'NONE',  ( 81.08346246620165232, 43.41693178244018014, -9.956532816971719768 ) ) ;
#80942 = DIRECTION ( 'NONE',  ( 0.8660254037844379305, 0.5000000000000015543, 0.000000000000000000 ) ) ;
#80943 = CARTESIAN_POINT ( 'NONE',  ( 6.102605256642664067, 165.1423013555410080, -4.594050593750043987 ) ) ;
#80944 = CARTESIAN_POINT ( 'NONE',  ( 112.2989703957094605, 226.4548013555409796, -4.594050593750042211 ) ) ;
#80945 = CARTESIAN_POINT ( 'NONE',  ( 155.0619429961492983, 262.0718317407570339, -17.08853361476647592 ) ) ;
#80946 = CARTESIAN_POINT ( 'NONE',  ( 87.98075804981249348, 44.53981909570472908, -3.999110579342586291 ) ) ;
#80947 = CARTESIAN_POINT ( 'NONE',  ( 186.7302140808759816, 295.8439017956092698, -7.678039062033136020 ) ) ;
#80949 = CYLINDRICAL_SURFACE ( 'NONE', #33460, 10.00000000000001066 ) ;
#80948 = VECTOR ( 'NONE', #19069, 1000.000000000000000 ) ;
#80950 = CARTESIAN_POINT ( 'NONE',  ( 76.48640248419295062, 51.58918322513654431, 15.64831315713033355 ) ) ;
#80951 = B_SPLINE_CURVE_WITH_KNOTS ( 'NONE', 3,
 ( #93562, #54501, #99648, #77845 ),
 .UNSPECIFIED., .F., .F.,
 ( 4, 4 ),
 ( 0.009075473815016553078, 0.01512968392534322706 ),
 .UNSPECIFIED. ) ;
#80952 = CARTESIAN_POINT ( 'NONE',  ( 162.9598982752141296, 282.9239241067374451, 5.638055053146040052 ) ) ;
#80953 = CARTESIAN_POINT ( 'NONE',  ( 194.6943296385021824, 293.4265244509877562, -16.10917128197217352 ) ) ;
#80954 = CARTESIAN_POINT ( 'NONE',  ( 181.8289026455834971, 291.5239361404854321, 9.451350534620820198 ) ) ;
#80955 = DIRECTION ( 'NONE',  ( -0.000000000000000000, -0.000000000000000000, -1.000000000000000000 ) ) ;
#80956 = CARTESIAN_POINT ( 'NONE',  ( 81.49432349081075699, 53.73119012861440780, -15.59150876117132256 ) ) ;
#80957 = CARTESIAN_POINT ( 'NONE',  ( 145.9293632524074553, 248.3927522451417929, -10.00000000000009237 ) ) ;
#80958 = CIRCLE ( 'NONE', #19474, 50.00000000000000711 ) ;
#80959 = CARTESIAN_POINT ( 'NONE',  ( 172.5583743051683996, 263.7812420529770066, -15.44831042087596984 ) ) ;
#80960 = EDGE_CURVE ( 'NONE', #58917, #53525, #64259, .T. ) ;
#80961 = CARTESIAN_POINT ( 'NONE',  ( 76.60222546164588664, 215.0333772461660544, 9.188101187500095079 ) ) ;
#80962 = CARTESIAN_POINT ( 'NONE',  ( 207.8844858873204657, 270.5805036682629066, -6.251308616122969397 ) ) ;
#80963 = LINE ( 'NONE', #11527, #31454 ) ;
#80964 = CARTESIAN_POINT ( 'NONE',  ( 163.3102869483862492, 258.1249230757383657, 15.76774596908120074 ) ) ;
#80965 = CARTESIAN_POINT ( 'NONE',  ( 198.0502297282944824, 286.6154393603603694, -17.27411237049796355 ) ) ;
#80966 = CARTESIAN_POINT ( 'NONE',  ( 151.1451503555562113, 268.8559155969762742, -15.81507177720227553 ) ) ;
#80967 = CARTESIAN_POINT ( 'NONE',  ( 14.14916430987532969, 185.6427522451419350, 10.00000000000009415 ) ) ;
#80968 = CARTESIAN_POINT ( 'NONE',  ( 29.46033357383057449, 37.98502408145594700, -5.678558825948271327 ) ) ;
#80969 = DIRECTION ( 'NONE',  ( 0.000000000000000000, 0.000000000000000000, -1.000000000000000000 ) ) ;
#80970 = CARTESIAN_POINT ( 'NONE',  ( 43.87294039959300562, 25.73415679381825427, 1.333680081654574804E-15 ) ) ;
#80971 = VERTEX_POINT ( 'NONE', #71879 ) ;
#80972 = CARTESIAN_POINT ( 'NONE',  ( 17.24455747906367264, 28.14336893147755347, 7.433330006724141015 ) ) ;
#80973 = CARTESIAN_POINT ( 'NONE',  ( 77.57650404090335883, 215.5958772461660544, -9.188101187500095079 ) ) ;
#80974 = CARTESIAN_POINT ( 'NONE',  ( 172.8631597400377018, 289.5366941478733338, -1.054817492037981141 ) ) ;
#80975 = LINE ( 'NONE', #4414, #71717 ) ;
#80976 = CARTESIAN_POINT ( 'NONE',  ( 191.3415583986349873, 288.7194663682888631, -16.11500851257928346 ) ) ;
#80977 = B_SPLINE_CURVE_WITH_KNOTS ( 'NONE', 3,
 ( #29850, #53145, #84101, #52634, #46021, #8059 ),
 .UNSPECIFIED., .F., .F.,
 ( 4, 2, 4 ),
 ( 0.01929493135631588779, 0.02382575134946158385, 0.02835657134260728338 ),
 .UNSPECIFIED. ) ;
#80978 = CARTESIAN_POINT ( 'NONE',  ( 86.37991722458738764, 47.25272401055813276, 10.79753792097408116 ) ) ;
#80979 = CARTESIAN_POINT ( 'NONE',  ( 193.6219581044664722, 288.4232849465348067, 16.10596218273157021 ) ) ;
#80980 = CARTESIAN_POINT ( 'NONE',  ( 72.47349332888545348, 71.58927234190268507, 5.197985995894253364 ) ) ;
#80981 = CARTESIAN_POINT ( 'NONE',  ( 127.8330407560430473, 244.6115022471902591, 10.00000000000009592 ) ) ;
#80982 = CARTESIAN_POINT ( 'NONE',  ( 21.31191609055711211, 173.1115022471901739, -5.000000000000041744 ) ) ;
#80983 = CARTESIAN_POINT ( 'NONE',  ( 74.73210197474243444, 53.53813011673200606, 16.07754455680917616 ) ) ;
#80984 = VERTEX_POINT ( 'NONE', #2478 ) ;
#80985 = CARTESIAN_POINT ( 'NONE',  ( 168.0032770494077283, 248.2778096739003502, -1.874811026054818308 ) ) ;
#80986 = VERTEX_POINT ( 'NONE', #19681 ) ;
#80987 = CARTESIAN_POINT ( 'NONE',  ( 163.1008115941903895, 248.1481028935802442, 11.25332017433677834 ) ) ;
#80988 = CARTESIAN_POINT ( 'NONE',  ( 207.4369976298412155, 270.8980557713372832, -0.6764754127990474375 ) ) ;
#80989 = CARTESIAN_POINT ( 'NONE',  ( 72.61953979799211822, 57.46676429237049177, -16.31386327007983539 ) ) ;
#80990 = EDGE_LOOP ( 'NONE', ( #49417, #9622, #74773, #5087 ) ) ;
#80991 = DIRECTION ( 'NONE',  ( 4.336808689942034499E-16, 7.511572993685835585E-16, -1.000000000000000000 ) ) ;
#80993 = EDGE_CURVE ( 'NONE', #53916, #64894, #55386, .T. ) ;
#80992 = ORIENTED_EDGE ( 'NONE', *, *, #78555, .F. ) ;
#80994 = CARTESIAN_POINT ( 'NONE',  ( 189.6374659733051260, 290.1052907212381911, 14.45593141723346342 ) ) ;
#80995 = CARTESIAN_POINT ( 'NONE',  ( 205.7538280185135307, 274.2709113505826508, 12.26218269827389307 ) ) ;
#80996 = CARTESIAN_POINT ( 'NONE',  ( 146.7502831681854332, 255.5333772461660260, 9.188101187500095079 ) ) ;
#80997 = CARTESIAN_POINT ( 'NONE',  ( 193.3021154463603750, 295.8379101667960072, -12.81235253903514959 ) ) ;
#80998 = CARTESIAN_POINT ( 'NONE',  ( 82.78738711968594544, 46.53022027656172099, 12.04865083719906593 ) ) ;
#80999 = CARTESIAN_POINT ( 'NONE',  ( 112.6979501180548766, 224.3262482093458061, 3.021315404115420679E-15 ) ) ;
#81000 = CARTESIAN_POINT ( 'NONE',  ( 37.18115723113500337, 22.26216523072496756, -2.296566073217252530E-15 ) ) ;
#81001 = CARTESIAN_POINT ( 'NONE',  ( 74.41277528214355641, 60.17971584258503270, -15.50566959064950190 ) ) ;
#81003 = EDGE_CURVE ( 'NONE', #61940, #51575, #73540, .T. ) ;
#81002 = CARTESIAN_POINT ( 'NONE',  ( 164.0586374769217741, 275.4376342846808257, 15.48247449835999312 ) ) ;
#81004 = FACE_OUTER_BOUND ( 'NONE', #13774, .T. ) ;
#81005 = EDGE_CURVE ( 'NONE', #79500, #42726, #85005, .T. ) ;
#81006 = VERTEX_POINT ( 'NONE', #75394 ) ;
#81007 = VERTEX_POINT ( 'NONE', #5977 ) ;
#81008 = CARTESIAN_POINT ( 'NONE',  ( 74.06414817410222895, 188.7419560658248656, -18.47570218321542868 ) ) ;
#81009 = ADVANCED_FACE ( 'NONE', ( #29288 ), #60153, .T. ) ;
#81010 =( BOUNDED_CURVE ( )  B_SPLINE_CURVE ( 2, ( #83116, #98805, #62250, #71893, #40946, #62758, #32867, #18183, #86631 ),
 .UNSPECIFIED., .F., .T. ) 
 B_SPLINE_CURVE_WITH_KNOTS ( ( 3, 2, 2, 2, 3 ),
 ( 0.5685483870967742437, 0.5698924731182796188, 0.5725806451612903691, 0.5752688172043011194, 0.5766129032258064946 ),
 .UNSPECIFIED. ) 
 CURVE ( )  GEOMETRIC_REPRESENTATION_ITEM ( )  RATIONAL_B_SPLINE_CURVE ( ( 0.9330127018922194093, 0.9330127018922194093, 1.000000000000000000, 0.8660254037844387076, 1.000000000000000000, 0.8660254037844387076, 1.000000000000000000, 0.9330127018922194093, 0.9330127018922194093 ) ) 
 REPRESENTATION_ITEM ( '' )  );
#81012 = CARTESIAN_POINT ( 'NONE',  ( 148.1829914015846157, 273.9865254053503349, -9.304102644963160529 ) ) ;
#81011 = CARTESIAN_POINT ( 'NONE',  ( 164.2297246530060875, 246.1927681183832988, 5.803160395959773510 ) ) ;
#81013 = CARTESIAN_POINT ( 'NONE',  ( 85.74798619856123594, 48.50762779557322801, -11.78128263942436327 ) ) ;
#81014 = CARTESIAN_POINT ( 'NONE',  ( 201.3053657339852691, 274.7141922394133076, -14.27644254562359372 ) ) ;
#81015 = DIRECTION ( 'NONE',  ( -0.3696446237802353263, -0.9291732088853875693, 0.000000000000000000 ) ) ;
#81016 = LINE ( 'NONE', #11080, #29066 ) ;
#81017 = CARTESIAN_POINT ( 'NONE',  ( 87.51647913336857698, 44.56403561216112053, 4.883618514853080406 ) ) ;
#81018 = VECTOR ( 'NONE', #56106, 1000.000000000000227 ) ;
#81019 = CARTESIAN_POINT ( 'NONE',  ( 156.9763224152064822, 271.9908631200777904, -15.29896765642516776 ) ) ;
#81020 = CARTESIAN_POINT ( 'NONE',  ( 181.9878657410701237, 256.9700144498582972, 5.080659748315781599 ) ) ;
#81021 = CARTESIAN_POINT ( 'NONE',  ( 101.9066655502961964, 220.4548013555409511, -4.594050593750042211 ) ) ;
#81022 = EDGE_LOOP ( 'NONE', ( #150, #26002, #52876, #73063 ) ) ;
#81023 = CARTESIAN_POINT ( 'NONE',  ( 149.8275266058892896, 271.5268038298542592, 11.74484678564449780 ) ) ;
#81024 = CARTESIAN_POINT ( 'NONE',  ( 114.6802799325189284, 237.0177522451418497, -10.00000000000009592 ) ) ;
#81025 = VERTEX_POINT ( 'NONE', #21682 ) ;
#81026 = EDGE_LOOP ( 'NONE', ( #7606, #11461, #27408, #54789 ) ) ;
#81027 = DIRECTION ( 'NONE',  ( -0.8660254037844387076, -0.4999999999999998890, -0.000000000000000000 ) ) ;
#81028 = CARTESIAN_POINT ( 'NONE',  ( 195.5855337169582242, 285.9052202549062258, -17.72130995818495336 ) ) ;
#81029 = CARTESIAN_POINT ( 'NONE',  ( -19.65312891409030271, 93.06504152958497400, 59.99999999999999289 ) ) ;
#81030 = CARTESIAN_POINT ( 'NONE',  ( 159.9531724557437826, 253.5999738052623229, -15.71074128491364874 ) ) ;
#81031 = CARTESIAN_POINT ( 'NONE',  ( 163.2109138634145609, 247.9574001692554077, 11.18215713980082171 ) ) ;
#81032 = CARTESIAN_POINT ( 'NONE',  ( 89.94416901687610277, 231.9244531367911009, -4.594050593750046652 ) ) ;
#81033 = ORIENTED_EDGE ( 'NONE', *, *, #64163, .T. ) ;
#81034 = CIRCLE ( 'NONE', #19538, 0.1418229129680863287 ) ;
#81035 = ORIENTED_EDGE ( 'NONE', *, *, #35397, .F. ) ;
#81036 = ADVANCED_FACE ( 'NONE', ( #52561 ), #83517, .T. ) ;
#81037 = CARTESIAN_POINT ( 'NONE',  ( 163.4084407101100851, 247.6152736349200438, -10.68829614238923931 ) ) ;
#81038 = ORIENTED_EDGE ( 'NONE', *, *, #41742, .F. ) ;
#81039 = CARTESIAN_POINT ( 'NONE',  ( 194.6615252313652888, 266.3370749013627687, -7.769244936135564217 ) ) ;
#81040 = CARTESIAN_POINT ( 'NONE',  ( 13.18034623014981044, 189.9637435831424739, 2.679491924311251605 ) ) ;
#81041 = CARTESIAN_POINT ( 'NONE',  ( 69.77718044168689460, 69.34802543791555252, -6.518941176212923239 ) ) ;
#81043 = CARTESIAN_POINT ( 'NONE',  ( 69.53286917118612109, 63.07419471374822706, -13.61637355923466686 ) ) ;
#81042 = CARTESIAN_POINT ( 'NONE',  ( 136.3847812948166336, 258.7369531367911009, -4.594050593750048428 ) ) ;
#81044 = CARTESIAN_POINT ( 'NONE',  ( -13.11024591527723437, 15.00000000000000000, -25.00000000000017053 ) ) ;
#81045 = DIRECTION ( 'NONE',  ( 1.000000000000000000, 0.000000000000000000, 0.000000000000000000 ) ) ;
#81046 = ORIENTED_EDGE ( 'NONE', *, *, #51635, .F. ) ;
#81047 = CARTESIAN_POINT ( 'NONE',  ( 157.2014865449050660, 258.3660336093062142, 16.87758714513496017 ) ) ;
#81048 = CARTESIAN_POINT ( 'NONE',  ( 80.71282890952170419, 45.80828928750833029, 11.77677843188879869 ) ) ;
#81049 = CARTESIAN_POINT ( 'NONE',  ( 82.06353261700769508, 41.00057011406288154, -2.892018250819526237 ) ) ;
#81050 = DIRECTION ( 'NONE',  ( -0.000000000000000000, -0.000000000000000000, -1.000000000000000000 ) ) ;
#81051 = CARTESIAN_POINT ( 'NONE',  ( 178.4805428241997163, 285.3359289386864930, 13.12455424698817907 ) ) ;
#81052 = CARTESIAN_POINT ( 'NONE',  ( 40.96864935082037817, 128.0650415295850735, 177.5919119679930134 ) ) ;
#81053 = CARTESIAN_POINT ( 'NONE',  ( 5.871984111234073822, 29.22396284167520619, -10.00000000000000000 ) ) ;
#81054 = LINE ( 'NONE', #13601, #9090 ) ;
#81055 = CARTESIAN_POINT ( 'NONE',  ( 161.4726291907278721, 250.9681975403669867, 14.52346149734912117 ) ) ;
#81056 = CARTESIAN_POINT ( 'NONE',  ( 67.21612508256824015, 69.36607345415896475, -0.9029263575005446185 ) ) ;
#81057 = CARTESIAN_POINT ( 'NONE',  ( 206.8313602288537538, 272.4045708154811791, -9.607337080360906612 ) ) ;
#81058 = CARTESIAN_POINT ( 'NONE',  ( 83.38731009417298878, 51.80618739314797239, 14.97569794390972575 ) ) ;
#81059 = CARTESIAN_POINT ( 'NONE',  ( 163.4139553296302267, 247.6057220337265505, -10.31482883765270842 ) ) ;
#81060 = CARTESIAN_POINT ( 'NONE',  ( -22.42236680055709641, 157.8615022471902591, 0.000000000000000000 ) ) ;
#81061 = CARTESIAN_POINT ( 'NONE',  ( 192.4380962356868281, 295.3344353383980661, 13.50754959408193656 ) ) ;
#81062 = EDGE_CURVE ( 'NONE', #98305, #68897, #6484, .T. ) ;
#81063 = CARTESIAN_POINT ( 'NONE',  ( 71.50988583758216066, 64.67014808439049034, -12.78853484773171978 ) ) ;
#81064 = CARTESIAN_POINT ( 'NONE',  ( 182.0281585185019537, 264.2490478462352712, 13.61349246500957477 ) ) ;
#81065 = CARTESIAN_POINT ( 'NONE',  ( 170.6241101913971079, 249.1812156342870708, -3.705643032328568953 ) ) ;
#81066 = CARTESIAN_POINT ( 'NONE',  ( 34.99667586858890189, 35.90829794293883737, 10.00000000000000355 ) ) ;
#81067 = LINE ( 'NONE', #49608, #91941 ) ;
#81068 = CARTESIAN_POINT ( 'NONE',  ( -73.66720466879951346, 50.53642055324488780, 10.00000000000000000 ) ) ;
#81069 = CARTESIAN_POINT ( 'NONE',  ( 160.8610131809898860, 273.3839308686426648, -15.49656964745045329 ) ) ;
#81070 = CARTESIAN_POINT ( 'NONE',  ( 84.78050178888084076, 43.36151058244004020, -5.604529421430612501 ) ) ;
#81071 = CARTESIAN_POINT ( 'NONE',  ( 23.17945691357580529, 178.0643266524160424, -9.188101187500093303 ) ) ;
#81072 = CARTESIAN_POINT ( 'NONE',  ( 68.47825347583855660, 69.28228719442910233, 6.190467033948801046 ) ) ;
#81073 = VERTEX_POINT ( 'NONE', #60648 ) ;
#81074 = CARTESIAN_POINT ( 'NONE',  ( 87.37996854902368682, 45.84054858551529321, 8.374939902689632731 ) ) ;
#81075 = CARTESIAN_POINT ( 'NONE',  ( 200.6117230619925635, 269.0360104864248001, 9.242361455687714056 ) ) ;
#81076 = CARTESIAN_POINT ( 'NONE',  ( 208.2777459429579210, 269.8993572713111462, 3.129643751043610589 ) ) ;
#81077 = CARTESIAN_POINT ( 'NONE',  ( 82.35222073790458808, 41.40766035265922795, 5.511273014246758528 ) ) ;
#81078 = CARTESIAN_POINT ( 'NONE',  ( 37.57712925149209582, 186.3768266524160140, 9.188101187500096856 ) ) ;
#81079 = CARTESIAN_POINT ( 'NONE',  ( 161.6673510627899191, 250.6309293646106653, 13.01175935005004192 ) ) ;
#81080 = CARTESIAN_POINT ( 'NONE',  ( 147.3154503175461514, 275.4891506405583073, 3.671329888160011823 ) ) ;
#81081 = CARTESIAN_POINT ( 'NONE',  ( 36.97850982526662023, 33.30066082961424456, -10.00000000000000533 ) ) ;
#81082 = CARTESIAN_POINT ( 'NONE',  ( 199.5198787286983872, 267.5021379205973631, -6.627115275362054803 ) ) ;
#81083 = CARTESIAN_POINT ( 'NONE',  ( 178.6383753932449281, 293.9108930832058491, 2.721302933230898002 ) ) ;
#81084 = CARTESIAN_POINT ( 'NONE',  ( 179.0373480721268038, 278.3843228141229815, -16.99121447468398216 ) ) ;
#81085 = CARTESIAN_POINT ( 'NONE',  ( 69.10630519318601728, 67.88941290928615047, -8.241121219118390684 ) ) ;
#81086 = CARTESIAN_POINT ( 'NONE',  ( 87.17079100176395912, 46.10763928714972337, -8.270830193046910139 ) ) ;
#81087 = CARTESIAN_POINT ( 'NONE',  ( 83.95452371275135306, 51.84303909528518517, 14.85259985614519884 ) ) ;
#81088 = VECTOR ( 'NONE', #34109, 1000.000000000000000 ) ;
#81089 = CARTESIAN_POINT ( 'NONE',  ( 87.57362070123205910, 45.45821687468009742, -6.782828800802978897 ) ) ;
#81090 = CARTESIAN_POINT ( 'NONE',  ( 74.64464720694869015, 227.2365022471903444, 2.944929066748280225E-16 ) ) ;
#81091 = CARTESIAN_POINT ( 'NONE',  ( 74.81623774949822803, 53.43188568764122692, 16.54077080093535557 ) ) ;
#81092 = CARTESIAN_POINT ( 'NONE',  ( 179.7389585068036979, 283.2694176073634935, 16.15404047216739514 ) ) ;
#81093 = EDGE_LOOP ( 'NONE', ( #10444, #24864, #30552, #89487 ) ) ;
#81094 = CARTESIAN_POINT ( 'NONE',  ( 38.60536087060361154, 193.0958772461660544, -9.188101187500095079 ) ) ;
#81095 = ORIENTED_EDGE ( 'NONE', *, *, #89498, .F. ) ;
#81096 = CARTESIAN_POINT ( 'NONE',  ( -12.28238420462231950, 85.48259521052763432, 14.78036012837727142 ) ) ;
#81097 = CARTESIAN_POINT ( 'NONE',  ( 147.3154503175461514, 275.4891506405583073, 3.671329888160011823 ) ) ;
#81098 = CARTESIAN_POINT ( 'NONE',  ( 67.43651257506147090, 67.25343589811649281, -8.652612161161503224 ) ) ;
#81099 = EDGE_LOOP ( 'NONE', ( #99760, #89190, #54139, #51928 ) ) ;
#81100 = CARTESIAN_POINT ( 'NONE',  ( 171.0568157338405229, 286.4360392956926944, 7.470701674589402153 ) ) ;
#81101 = CARTESIAN_POINT ( 'NONE',  ( 206.9408877595175511, 272.2148635675444552, 6.707071080545934372 ) ) ;
#81102 = CYLINDRICAL_SURFACE ( 'NONE', #47665, 17.82106496071139645 ) ;
#81103 = CARTESIAN_POINT ( 'NONE',  ( 26.87427219475921092, 30.91421378149919974, 9.188101187500008038 ) ) ;
#81104 = CARTESIAN_POINT ( 'NONE',  ( 189.1716578938339524, 265.4390178063673034, 10.58420148173503783 ) ) ;
#81105 = CARTESIAN_POINT ( 'NONE',  ( 86.46843151262319793, 47.10573899677975618, -10.05275782589266065 ) ) ;
#81106 = CARTESIAN_POINT ( 'NONE',  ( 173.6854900591675346, 256.8832444864495983, 11.28848571671958467 ) ) ;
#81107 = ORIENTED_EDGE ( 'NONE', *, *, #89571, .T. ) ;
#81108 = CARTESIAN_POINT ( 'NONE',  ( 15.18774714507562962, 26.95586893147754992, 7.433330006724141015 ) ) ;
#81109 = CARTESIAN_POINT ( 'NONE',  ( -12.82842912691854309, 163.4005647456539521, -9.594050593750095501 ) ) ;
#81110 = CARTESIAN_POINT ( 'NONE',  ( 174.7340118358694951, 255.1271270684982824, 8.232752107466076552 ) ) ;
#81111 = CARTESIAN_POINT ( 'NONE',  ( 20.80527494242019060, 12.41603393254324494, -1.583844403245362020 ) ) ;
#81112 = VERTEX_POINT ( 'NONE', #22176 ) ;
#81114 = EDGE_CURVE ( 'NONE', #76868, #27771, #4631, .T. ) ;
#81113 = CARTESIAN_POINT ( 'NONE',  ( 178.6460525542210007, 282.3916330005288842, 15.69558721233099341 ) ) ;
#81115 = CARTESIAN_POINT ( 'NONE',  ( 191.5451565139252068, 298.8810523045859213, 7.782291334092181323 ) ) ;
#81116 = DIRECTION ( 'NONE',  ( -0.8660254037844387076, -0.4999999999999998890, -0.000000000000000000 ) ) ;
#81117 = EDGE_CURVE ( 'NONE', #34750, #100037, #21500, .T. ) ;
#81118 = EDGE_LOOP ( 'NONE', ( #93173, #25531, #66717, #29634 ) ) ;
#81119 = ORIENTED_EDGE ( 'NONE', *, *, #92211, .F. ) ;
#81121 = DIRECTION ( 'NONE',  ( 0.9874311856918874808, -0.1580495287025984186, 0.000000000000000000 ) ) ;
#81120 = CARTESIAN_POINT ( 'NONE',  ( 207.7836085030675690, 270.7552284231231852, -5.468305433308493058 ) ) ;
#81122 = CARTESIAN_POINT ( 'NONE',  ( 148.9194629746633893, 272.7109192224475009, -12.27648025871169679 ) ) ;
#81123 = ORIENTED_EDGE ( 'NONE', *, *, #38899, .T. ) ;
#81124 = CARTESIAN_POINT ( 'NONE',  ( 65.82416590051595051, 68.93390312404366682, -2.375186792701355021 ) ) ;
#81125 = EDGE_CURVE ( 'NONE', #41317, #99059, #50462, .T. ) ;
#81126 = CARTESIAN_POINT ( 'NONE',  ( 198.0858447170796524, 287.5522480202560018, 18.44384186289807559 ) ) ;
#81127 = CARTESIAN_POINT ( 'NONE',  ( 72.77243010704501103, 56.90600714599002430, -15.93123261131951196 ) ) ;
#81128 = CARTESIAN_POINT ( 'NONE',  ( 78.17919853682799669, 61.76234676664309120, -16.10619035535653509 ) ) ;
#81130 = EDGE_CURVE ( 'NONE', #67131, #89517, #23804, .T. ) ;
#81129 = CARTESIAN_POINT ( 'NONE',  ( 157.8429099974857195, 257.2550556002704525, -17.85752049034686095 ) ) ;
#81131 = CARTESIAN_POINT ( 'NONE',  ( 111.1617914095948692, 244.1744531367911293, 4.594050593750047540 ) ) ;
#81132 = CARTESIAN_POINT ( 'NONE',  ( 117.8941025407614802, 227.3262482093458061, 3.021315404115420679E-15 ) ) ;
#81133 = ORIENTED_EDGE ( 'NONE', *, *, #40577, .F. ) ;
#81134 = CARTESIAN_POINT ( 'NONE',  ( 201.5248099939757651, 280.9651160740240812, 16.27600578877254733 ) ) ;
#81135 = EDGE_LOOP ( 'NONE', ( #98149, #58943, #47520, #6584, #1730 ) ) ;
#81136 = CARTESIAN_POINT ( 'NONE',  ( 34.79119414172389213, 25.80170272979928470, 7.433330006724137462 ) ) ;
#81137 = CARTESIAN_POINT ( 'NONE',  ( 159.9880386575927957, 253.5395837721924863, 15.85893018594752846 ) ) ;
#81138 = CARTESIAN_POINT ( 'NONE',  ( 75.22346589584923038, 66.43729998232824130, -13.15201661418532098 ) ) ;
#81139 = CARTESIAN_POINT ( 'NONE',  ( 70.64795371486285092, 223.8464784336661353, 1.353441290958777525E-15 ) ) ;
#81140 = CARTESIAN_POINT ( 'NONE',  ( 172.2305375516802144, 289.0099938022871129, 7.323606124671270479 ) ) ;
#81141 = CARTESIAN_POINT ( 'NONE',  ( 151.4384131719918685, 268.3479694989391078, 14.98299707687648841 ) ) ;
#81142 = CARTESIAN_POINT ( 'NONE',  ( 196.9080397933726942, 269.7016881256661804, 12.39056067425276630 ) ) ;
#81143 = CARTESIAN_POINT ( 'NONE',  ( 171.8895305906860358, 276.7362633202488382, 16.33455527369717686 ) ) ;
#81144 = ORIENTED_EDGE ( 'NONE', *, *, #39328, .T. ) ;
#81145 = CARTESIAN_POINT ( 'NONE',  ( 40.48539884740146277, 126.3902902409112556, -10.00000000000000000 ) ) ;
#81146 = CARTESIAN_POINT ( 'NONE',  ( 155.6535436963908694, 261.0471492701456668, -17.87366571046205976 ) ) ;
#81147 = VERTEX_POINT ( 'NONE', #27685 ) ;
#81148 = CARTESIAN_POINT ( 'NONE',  ( 195.1612419366965128, 292.6178086278368369, 15.12635622767516352 ) ) ;
#81149 = CARTESIAN_POINT ( 'NONE',  ( 70.75593123090459358, 69.82372255332346356, -6.700183475668088917 ) ) ;
#81150 = CARTESIAN_POINT ( 'NONE',  ( 163.4196212193596978, 260.1667154333714507, -16.20002750279465431 ) ) ;
#81151 = CARTESIAN_POINT ( 'NONE',  ( 79.03898477424621660, 204.8932355074535963, -2.679491924311248496 ) ) ;
#81152 = DIRECTION ( 'NONE',  ( -0.000000000000000000, 0.000000000000000000, 1.000000000000000000 ) ) ;
#81153 = CARTESIAN_POINT ( 'NONE',  ( 57.74716087599451697, 218.0038070926034948, -17.47570218321534341 ) ) ;
#81154 = CARTESIAN_POINT ( 'NONE',  ( 152.1095568868906298, 269.8383682962399348, -14.43354909618994419 ) ) ;
#81155 = CARTESIAN_POINT ( 'NONE',  ( -61.60412911085353471, 37.02832515102500111, -10.00000000000000000 ) ) ;
#81156 = CARTESIAN_POINT ( 'NONE',  ( 167.5740236991643712, 256.4854641017122958, 13.67099374824216973 ) ) ;
#81157 = VERTEX_POINT ( 'NONE', #27182 ) ;
#81158 = CARTESIAN_POINT ( 'NONE',  ( 207.6471633721571379, 270.9915583223058206, 2.196965492132801678 ) ) ;
#81159 = CARTESIAN_POINT ( 'NONE',  ( 128.5637496887121927, 245.0333772461660544, 9.188101187500095079 ) ) ;
#81160 = VERTEX_POINT ( 'NONE', #18589 ) ;
#81161 = CARTESIAN_POINT ( 'NONE',  ( 191.3413020738616410, 299.2341385521244774, -8.295023558158421295 ) ) ;
#81162 = CARTESIAN_POINT ( 'NONE',  ( 82.89276890572784851, 41.25948029148610630, 1.516552898798564364 ) ) ;
#81163 = DIRECTION ( 'NONE',  ( -0.9862134920484688649, -0.1654779384134468789, 0.000000000000000000 ) ) ;
#81164 = B_SPLINE_CURVE_WITH_KNOTS ( 'NONE', 3,
 ( #45623, #76552, #98868, #13745, #69436, #30438, #92772, #37039, #61327, #61821 ),
 .UNSPECIFIED., .F., .F.,
 ( 4, 2, 2, 2, 4 ),
 ( 0.000000000000000000, 0.0002622400424273282080, 0.0005244800848546564160, 0.0007867201272819846240, 0.001048960169709312832 ),
 .UNSPECIFIED. ) ;
#81165 = CARTESIAN_POINT ( 'NONE',  ( 204.7610021263893429, 275.9905362388115577, 13.36619428527026976 ) ) ;
#81166 = CARTESIAN_POINT ( 'NONE',  ( 75.40315211601793521, 64.63645072480072429, 14.18768813069354273 ) ) ;
#81167 = AXIS2_PLACEMENT_3D ( 'NONE', #37292, #68187, #46369 ) ;
#81168 = CARTESIAN_POINT ( 'NONE',  ( -19.65312891409030271, 93.06504152958497400, 177.5919119679930134 ) ) ;
#81169 = EDGE_LOOP ( 'NONE', ( #32914, #93195, #64010, #31102 ) ) ;
#81170 = CARTESIAN_POINT ( 'NONE',  ( 80.17693862949111860, 57.41387879531588112, -16.59169664258510224 ) ) ;
#81171 = CARTESIAN_POINT ( 'NONE',  ( 165.8535204196604695, 247.9869754089129970, -5.534111939223802068 ) ) ;
#81172 = CARTESIAN_POINT ( 'NONE',  ( 206.3559632282955647, 273.2279825742143089, -11.28941701449801904 ) ) ;
#81173 = CARTESIAN_POINT ( 'NONE',  ( -32.94356256989595977, 94.88921800892812541, 45.19948692389422717 ) ) ;
#81174 = B_SPLINE_CURVE_WITH_KNOTS ( 'NONE', 3,
 ( #597, #68001, #15278, #92829, #46173, #98925, #62374, #30992, #60379, #52785, #76131, #68492, #41074, #2109, #87774, #64905, #49691, #39567, #95363, #2616, #86253, #94831, #63397, #9724, #1105, #71519, #86758, #17292, #33504, #64399, #71019, #9201, #32505, #42089, #65885, #20304, #74519, #27406, #20809, #5098, #65394, #96335, #82145, #82650, #11712, #58285 ),
 .UNSPECIFIED., .F., .F.,
 ( 4, 1, 1, 1, 2, 2, 1, 1, 1, 2, 2, 1, 1, 2, 2, 1, 1, 2, 2, 1, 1, 2, 2, 1, 2, 2, 1, 2, 2, 4 ),
 ( 0.000000000000000000, 0.06250000000001434963, 0.09375000000002152445, 0.1093750000000235229, 0.1171875000000245359, 0.1250000000000255351, 0.1875000000000333344, 0.2187500000000385247, 0.2343750000000410505, 0.2421875000000424660, 0.2500000000000439093, 0.3125000000000414113, 0.3437500000000416334, 0.3593750000000416889, 0.3750000000000417999, 0.4375000000000413558, 0.4687500000000399125, 0.4843750000000404676, 0.5000000000000410783, 0.5625000000000393019, 0.5937500000000383027, 0.6093750000000375255, 0.6250000000000367484, 0.6875000000000319744, 0.7187500000000293099, 0.7500000000000267564, 0.8125000000000188738, 0.8437500000000152101, 0.8750000000000114353, 1.000000000000000000 ),
 .UNSPECIFIED. ) ;
#81175 = CARTESIAN_POINT ( 'NONE',  ( -32.80726662848048392, 94.24456392606165878, 43.88975813191157016 ) ) ;
#81176 = CARTESIAN_POINT ( 'NONE',  ( 68.86548415544730517, 69.78790591026515244, 4.016893358874391140 ) ) ;
#81177 = EDGE_CURVE ( 'NONE', #73688, #54866, #35766, .T. ) ;
#81178 = CARTESIAN_POINT ( 'NONE',  ( 204.6470611188870521, 276.1878878528713130, -13.02652554726987866 ) ) ;
#81179 = CARTESIAN_POINT ( 'NONE',  ( 174.4045371546278886, 252.1404095536752834, 3.497397249627876459 ) ) ;
#81180 = CARTESIAN_POINT ( 'NONE',  ( 17.65531800687426056, 22.14441083166260427, 10.00000000000000533 ) ) ;
#81181 = CARTESIAN_POINT ( 'NONE',  ( 149.4491471355718772, 271.7934793437897270, 11.43912701239353780 ) ) ;
#81182 = CARTESIAN_POINT ( 'NONE',  ( 153.7448948813404570, 278.8794451890384494, -1.595968573229418874 ) ) ;
#81183 = CARTESIAN_POINT ( 'NONE',  ( 172.5430877045778288, 287.8837544777731523, -8.388212238523923503 ) ) ;
#81184 = CARTESIAN_POINT ( 'NONE',  ( -8.517573342504920930, 41.22347591502147424, 59.99999999999999289 ) ) ;
#81185 = CARTESIAN_POINT ( 'NONE',  ( 193.6779244371759603, 288.5814230932801365, 16.06948571431362893 ) ) ;
#81186 = CARTESIAN_POINT ( 'NONE',  ( 127.7428297729341580, 257.8927522451419918, 2.944929066748280225E-16 ) ) ;
#81187 = CARTESIAN_POINT ( 'NONE',  ( 80.05875441287906824, 52.08331270771197552, -15.29290510163803418 ) ) ;
#81188 = ORIENTED_EDGE ( 'NONE', *, *, #94341, .T. ) ;
#81189 = EDGE_CURVE ( 'NONE', #72634, #28659, #58554, .T. ) ;
#81190 = CARTESIAN_POINT ( 'NONE',  ( 196.0034224882197975, 291.1591091234520263, 17.53794140922627776 ) ) ;
#81191 = CARTESIAN_POINT ( 'NONE',  ( 189.8763472015711216, 301.7715148217271803, -0.1184663095182975079 ) ) ;
#81192 = CARTESIAN_POINT ( 'NONE',  ( -9.107486540969064848, 174.7369531367911293, -4.594050593750048428 ) ) ;
#81193 = CARTESIAN_POINT ( 'NONE',  ( 32.16412338207434374, 195.5024278399160949, 9.188101187500095079 ) ) ;
#81194 = CARTESIAN_POINT ( 'NONE',  ( 86.27526515939862861, 45.76759053229242369, 9.183507728554419103 ) ) ;
#81195 = CARTESIAN_POINT ( 'NONE',  ( 22.33482336197099016, 13.86426979415089455, -3.090169943749474069 ) ) ;
#81196 = CARTESIAN_POINT ( 'NONE',  ( 189.6855683962509147, 268.4063607128787794, 14.53388648619876378 ) ) ;
#81197 = CARTESIAN_POINT ( 'NONE',  ( 204.8057697639265768, 275.9129964160624695, -12.68356524114230766 ) ) ;
#81198 = CARTESIAN_POINT ( 'NONE',  ( 192.5978738290548051, 292.4115197693782875, -14.32134620733571495 ) ) ;
#81199 = CARTESIAN_POINT ( 'NONE',  ( 146.7879906441258129, 276.4027375938661635, 4.347255311287614887 ) ) ;
#81200 = CARTESIAN_POINT ( 'NONE',  ( 73.99193044287086707, 55.63566381354063139, -16.58609767700729165 ) ) ;
#81202 = CARTESIAN_POINT ( 'NONE',  ( 71.81202244518927102, 202.2677522451417929, -5.000000000000041744 ) ) ;
#81201 = CARTESIAN_POINT ( 'NONE',  ( -66.55019942848203129, 42.78701949053055387, -10.00000000000000000 ) ) ;
#81203 = CARTESIAN_POINT ( 'NONE',  ( 76.41665957711717283, 57.56464406158257674, 16.56912583713305764 ) ) ;
#81204 = CARTESIAN_POINT ( 'NONE',  ( 34.28597393419622819, 20.76426979415091978, 3.090169943749476733 ) ) ;
#81205 = CARTESIAN_POINT ( 'NONE',  ( 174.3103273403459070, 251.6799977031412539, 4.969826440491621256 ) ) ;
#81206 = CARTESIAN_POINT ( 'NONE',  ( 39.49844957003027446, 193.6115022471902591, 10.00000000000009592 ) ) ;
#81207 = CARTESIAN_POINT ( 'NONE',  ( 199.1165320752825494, 285.7670451491295580, 0.000000000000000000 ) ) ;
#81208 = CARTESIAN_POINT ( 'NONE',  ( 163.2835940097493790, 247.8315144631017404, 11.08416305054517359 ) ) ;
#81209 = CARTESIAN_POINT ( 'NONE',  ( 7.266240119036749157, 168.8768266524159856, -9.188101187500091527 ) ) ;
#81210 = CARTESIAN_POINT ( 'NONE',  ( 166.6849293799611758, 285.4799480694566682, 4.101407758763460976 ) ) ;
#81211 = CARTESIAN_POINT ( 'NONE',  ( 164.2873127220971128, 252.5483806906220252, 13.40952729246955677 ) ) ;
#81212 = CARTESIAN_POINT ( 'NONE',  ( 153.4242699508872647, 264.9083646613370320, 16.62000820703435267 ) ) ;
#81213 = CARTESIAN_POINT ( 'NONE',  ( 32.39518414388500389, 34.10171378149920685, 9.188101187500008038 ) ) ;
#81214 = CARTESIAN_POINT ( 'NONE',  ( 19.14394661871191161, 29.79103043416549212, 8.090169943749478065 ) ) ;
#81215 = CARTESIAN_POINT ( 'NONE',  ( 179.6991264753519317, 277.0039691112309015, 16.29786852896214100 ) ) ;
#81216 = CARTESIAN_POINT ( 'NONE',  ( -104.9999999999999858, 93.06504152958497400, -54.99999999999999289 ) ) ;
#81217 = CARTESIAN_POINT ( 'NONE',  ( 149.1429535397850827, 272.3238222086447990, -12.91457852089092384 ) ) ;
#81218 = CARTESIAN_POINT ( 'NONE',  ( 177.2089533061429734, 260.4205850299505300, -13.82133967672870511 ) ) ;
#81219 = CARTESIAN_POINT ( 'NONE',  ( 2.953350652821653988, 23.74646525600387648, 2.839279412974139660 ) ) ;
#81220 = CARTESIAN_POINT ( 'NONE',  ( 71.80888402837305762, 72.55032655444114198, 1.016447747306844285 ) ) ;
#81221 = CARTESIAN_POINT ( 'NONE',  ( 15.07467606819624173, 24.10171378149917842, 9.188101187500008038 ) ) ;
#81222 = CARTESIAN_POINT ( 'NONE',  ( 12.00096474099108690, 32.03863464977599307, -10.00000000000000000 ) ) ;
#81223 = CARTESIAN_POINT ( 'NONE',  ( 154.8596847415876994, 262.4221533139083817, 17.65401077761399762 ) ) ;
#81224 = EDGE_LOOP ( 'NONE', ( #42239, #77846, #49616, #83983 ) ) ;
#81225 = CARTESIAN_POINT ( 'NONE',  ( 156.8182864210080538, 276.5001846890115758, 10.28252859274006248 ) ) ;
#81226 = CARTESIAN_POINT ( 'NONE',  ( 206.6268150440956504, 272.7588534679261443, -10.76664753678610609 ) ) ;
#81227 = EDGE_CURVE ( 'NONE', #11943, #43088, #49467, .T. ) ;
#81228 = VERTEX_POINT ( 'NONE', #33798 ) ;
#81229 = CARTESIAN_POINT ( 'NONE',  ( 153.3703256797887775, 265.0017988796566897, 16.44314709207578318 ) ) ;
#81230 = CARTESIAN_POINT ( 'NONE',  ( 206.9408877595175511, 272.2148635675444552, 6.707071080545934372 ) ) ;
#81231 = CARTESIAN_POINT ( 'NONE',  ( 66.53923092494953551, 68.73325766750851074, 4.777391229452033095 ) ) ;
#81232 = CARTESIAN_POINT ( 'NONE',  ( 87.10876144644647923, 45.29703821539081332, 7.013113301196394644 ) ) ;
#81233 = VECTOR ( 'NONE', #76555, 1000.000000000000000 ) ;
#81234 = VERTEX_POINT ( 'NONE', #81908 ) ;
#81235 = ORIENTED_EDGE ( 'NONE', *, *, #31033, .F. ) ;
#81237 = CARTESIAN_POINT ( 'NONE',  ( 204.6780326111993986, 276.1342436545999703, 14.85609018352459287 ) ) ;
#81236 = DIRECTION ( 'NONE',  ( -0.000000000000000000, -0.000000000000000000, -1.000000000000000000 ) ) ;
#81238 = CARTESIAN_POINT ( 'NONE',  ( 192.7259387352017939, 296.8358775046606297, 11.24705370801146209 ) ) ;
#81239 = ORIENTED_EDGE ( 'NONE', *, *, #29360, .T. ) ;
#81240 = CARTESIAN_POINT ( 'NONE',  ( 77.31184969415271269, 55.15837166631282429, 16.11507958877023583 ) ) ;
#81241 = CARTESIAN_POINT ( 'NONE',  ( 177.7988474914041035, 263.9390705747547941, 14.66591618048462209 ) ) ;
#81242 = ORIENTED_EDGE ( 'NONE', *, *, #72364, .F. ) ;
#81244 = EDGE_CURVE ( 'NONE', #22484, #44226, #32299, .T. ) ;
#81243 = CARTESIAN_POINT ( 'NONE',  ( 30.13164393277487818, 36.13478043621390157, 8.090169943749478065 ) ) ;
#81245 = CARTESIAN_POINT ( 'NONE',  ( 77.92555521731604529, 50.51076232770562058, -15.15948202354326568 ) ) ;
#81246 = CARTESIAN_POINT ( 'NONE',  ( 34.98558885611105751, 202.5530062829863027, -4.648177544792955347E-16 ) ) ;
#81247 = ORIENTED_EDGE ( 'NONE', *, *, #34866, .T. ) ;
#81248 = LINE ( 'NONE', #19439, #92149 ) ;
#81249 = CARTESIAN_POINT ( 'NONE',  ( 168.1388140323589937, 275.3731239741051127, -15.27220439302207211 ) ) ;
#81250 = CYLINDRICAL_SURFACE ( 'NONE', #41286, 10.00000000000010658 ) ;
#81251 = ORIENTED_EDGE ( 'NONE', *, *, #98036, .T. ) ;
#81252 = CARTESIAN_POINT ( 'NONE',  ( 174.6227982317619478, 277.3332904828302503, -15.64528549635424071 ) ) ;
#81253 = CARTESIAN_POINT ( 'NONE',  ( 202.9689790241539242, 279.0944113002206564, 15.85114608332523289 ) ) ;
#81254 = VERTEX_POINT ( 'NONE', #12487 ) ;
#81255 = CARTESIAN_POINT ( 'NONE',  ( 159.7740173431952542, 268.4189001149085811, -16.40494236134203376 ) ) ;
#81256 = VERTEX_POINT ( 'NONE', #10479 ) ;
#81257 = DIRECTION ( 'NONE',  ( -0.3177184104407523857, 0.9481851146622171100, 0.000000000000000000 ) ) ;
#81258 = ORIENTED_EDGE ( 'NONE', *, *, #20214, .T. ) ;
#81259 = CARTESIAN_POINT ( 'NONE',  ( 158.8346295283509733, 260.0021606417885778, 17.18667582297067042 ) ) ;
#81260 = CARTESIAN_POINT ( 'NONE',  ( 88.01831552501732858, 44.11100423982306751, 1.674833614738614695 ) ) ;
#81261 = CARTESIAN_POINT ( 'NONE',  ( 147.8921479301010038, 274.4902810750095341, 6.237421762629938193 ) ) ;
#81262 = CARTESIAN_POINT ( 'NONE',  ( 82.88482919494256862, 53.69580434870786689, 15.74208873548984400 ) ) ;
#81263 = DIRECTION ( 'NONE',  ( -0.000000000000000000, -0.000000000000000000, -1.000000000000000000 ) ) ;
#81264 = CARTESIAN_POINT ( 'NONE',  ( 152.7153488183568300, 266.1362520814392951, 17.33540622643059237 ) ) ;
#81265 = CARTESIAN_POINT ( 'NONE',  ( 29.53915742650918830, 197.8615022471903160, 5.000000000000046185 ) ) ;
#81266 = CARTESIAN_POINT ( 'NONE',  ( 196.3956310503436953, 264.1850728776087180, 4.154333235580330630 ) ) ;
#81267 = ORIENTED_EDGE ( 'NONE', *, *, #9042, .T. ) ;
#81268 = CARTESIAN_POINT ( 'NONE',  ( -112.5954152546897262, 74.04580364311806306, -21.50000000000000000 ) ) ;
#81269 = CARTESIAN_POINT ( 'NONE',  ( 19.72598728594001116, 34.49540643055188127, 3.479690158560446702E-15 ) ) ;
#81270 = CARTESIAN_POINT ( 'NONE',  ( 150.6217811227348875, 274.8790014839793230, -9.901424828548254453 ) ) ;
#81271 = VECTOR ( 'NONE', #17923, 1000.000000000000000 ) ;
#81272 = CARTESIAN_POINT ( 'NONE',  ( 164.6869624841032191, 245.4008089637804346, 1.435659848726088317 ) ) ;
#81274 = EDGE_LOOP ( 'NONE', ( #197, #63448, #14576, #26377 ) ) ;
#81273 = LINE ( 'NONE', #52309, #46059 ) ;
#81275 = ORIENTED_EDGE ( 'NONE', *, *, #40418, .F. ) ;
#81276 = CARTESIAN_POINT ( 'NONE',  ( 186.2313097042465699, 276.3922763046537057, 16.55972454784547310 ) ) ;
#81277 = CARTESIAN_POINT ( 'NONE',  ( 171.5203192281751967, 259.6685845591893553, -14.08447829917957073 ) ) ;
#81278 = CARTESIAN_POINT ( 'NONE',  ( -17.33262083840142509, 129.0458036431182904, -30.52142883766501669 ) ) ;
#81279 = LINE ( 'NONE', #42222, #8496 ) ;
#81280 = CARTESIAN_POINT ( 'NONE',  ( 199.4224781028189000, 285.2371310850626287, -17.75806834606089168 ) ) ;
#81281 = CARTESIAN_POINT ( 'NONE',  ( 148.3108110047529919, 273.7651353584593608, -10.43768245379277104 ) ) ;
#81282 = ORIENTED_EDGE ( 'NONE', *, *, #74431, .F. ) ;
#81283 = CARTESIAN_POINT ( 'NONE',  ( 167.3067612288924124, 252.8339271406035493, -12.30798038737281175 ) ) ;
#81284 = DIRECTION ( 'NONE',  ( -0.7561390817803280706, 0.6544109481086042290, 0.000000000000000000 ) ) ;
#81285 = CARTESIAN_POINT ( 'NONE',  ( -56.14442822474985206, 33.32908021129814813, 177.5919119679930134 ) ) ;
#81286 = VECTOR ( 'NONE', #21963, 1000.000000000000114 ) ;
#81287 = CYLINDRICAL_SURFACE ( 'NONE', #16009, 10.00000000000010658 ) ;
#81288 = CARTESIAN_POINT ( 'NONE',  ( 35.00594278435062989, 181.0177522451417929, 5.000000000000051514 ) ) ;
#81290 = CARTESIAN_POINT ( 'NONE',  ( 107.4543804714665072, 232.8458772461660544, 9.188101187500095079 ) ) ;
#81289 = B_SPLINE_CURVE_WITH_KNOTS ( 'NONE', 3,
 ( #76024, #5598, #37474, #85647, #47082, #30889, #86154, #93733, #992, #31872, #92724, #23779, #15676, #68875, #46571, #24778, #92244, #85128 ),
 .UNSPECIFIED., .F., .F.,
 ( 4, 2, 2, 2, 2, 2, 2, 2, 4 ),
 ( 0.006884441260529831907, 0.007422657591717915157, 0.007960873922905998407, 0.008499090254094083391, 0.009037306585282166640, 0.009575522916470241216, 0.01011373924765832447, 0.01065195557884640945, 0.01119017191003449270 ),
 .UNSPECIFIED. ) ;
#81291 = CARTESIAN_POINT ( 'NONE',  ( 6.176825452568912134, 162.8262482093457777, 3.021315404115420679E-15 ) ) ;
#81292 = CARTESIAN_POINT ( 'NONE',  ( 167.8847406357959358, 281.9191505512837352, -10.89945309425706021 ) ) ;
#81293 = CARTESIAN_POINT ( 'NONE',  ( -22.42236680055709641, 157.8615022471902591, 0.000000000000000000 ) ) ;
#81294 = CARTESIAN_POINT ( 'NONE',  ( 208.0366075493969902, 270.3170212206142082, 1.570844709476715284 ) ) ;
#81295 = CARTESIAN_POINT ( 'NONE',  ( 21.98867198337220685, 177.3768266524160140, 9.188101187500098632 ) ) ;
#81296 = ADVANCED_FACE ( 'NONE', ( #19602 ), #64682, .T. ) ;
#81297 = CARTESIAN_POINT ( 'NONE',  ( 73.65729962767424865, 69.49757902785616182, 9.740712345197151123 ) ) ;
#81298 = ORIENTED_EDGE ( 'NONE', *, *, #6493, .T. ) ;
#81299 = ORIENTED_EDGE ( 'NONE', *, *, #53158, .T. ) ;
#81300 = DIRECTION ( 'NONE',  ( -0.5435407515102007592, 0.8393827800519415572, 0.000000000000000000 ) ) ;
#81301 = CARTESIAN_POINT ( 'NONE',  ( 185.1558638909941408, 259.8922561614027700, -5.643363702243105351 ) ) ;
#81302 = EDGE_CURVE ( 'NONE', #84216, #54173, #64646, .T. ) ;
#81303 =( BOUNDED_CURVE ( )  B_SPLINE_CURVE ( 2, ( #23985, #87864, #94429, #40172, #41678, #62991, #54883, #93935, #64498 ),
 .UNSPECIFIED., .F., .T. ) 
 B_SPLINE_CURVE_WITH_KNOTS ( ( 3, 2, 2, 2, 3 ),
 ( 0.9153225806451612545, 0.9166666666666666297, 0.9193548387096773800, 0.9220430107526881303, 0.9233870967741935054 ),
 .UNSPECIFIED. ) 
 CURVE ( )  GEOMETRIC_REPRESENTATION_ITEM ( )  RATIONAL_B_SPLINE_CURVE ( ( 0.9330127018922194093, 0.9330127018922194093, 1.000000000000000000, 0.8660254037844387076, 1.000000000000000000, 0.8660254037844387076, 1.000000000000000000, 0.9330127018922194093, 0.9330127018922194093 ) ) 
 REPRESENTATION_ITEM ( '' )  );
#81304 = CARTESIAN_POINT ( 'NONE',  ( 203.6925490392534925, 269.5270927311577793, 7.084861529579629114 ) ) ;
#81305 = CARTESIAN_POINT ( 'NONE',  ( 147.3154503175461514, 275.4891506405583073, 3.671329888160011823 ) ) ;
#81306 = DIRECTION ( 'NONE',  ( 0.4999999999999992784, -0.8660254037844390407, 0.000000000000000000 ) ) ;
#81307 = CARTESIAN_POINT ( 'NONE',  ( 161.5083988044524119, 250.9062427520286178, -14.53522982831775856 ) ) ;
#81308 = CARTESIAN_POINT ( 'NONE',  ( 183.7164175811012115, 284.9638087483388063, 15.03005855678972047 ) ) ;
#81309 = FACE_OUTER_BOUND ( 'NONE', #33017, .T. ) ;
#81310 = CARTESIAN_POINT ( 'NONE',  ( 36.87296296726972855, 204.3464784336661637, 1.353441290958777525E-15 ) ) ;
#81311 = CARTESIAN_POINT ( 'NONE',  ( 99.09182266439904652, 228.0177522451418781, -10.00000000000009592 ) ) ;
#81312 = ORIENTED_EDGE ( 'NONE', *, *, #93824, .F. ) ;
#81313 = ADVANCED_FACE ( 'NONE', ( #81413 ), #26180, .F. ) ;
#81314 = CARTESIAN_POINT ( 'NONE',  ( 83.90681972514065023, 47.04571552257464617, 11.33789640138802035 ) ) ;
#81315 = CARTESIAN_POINT ( 'NONE',  ( 180.3229202803501323, 260.0783157291148200, -10.34379025228027338 ) ) ;
#81316 = CARTESIAN_POINT ( 'NONE',  ( 0.4998960083233069396, 183.3464784336661353, 1.353441290958777327E-15 ) ) ;
#81317 = CARTESIAN_POINT ( 'NONE',  ( 68.72553068027684731, 64.68746542795034316, -12.16225929270542494 ) ) ;
#81318 = CARTESIAN_POINT ( 'NONE',  ( 199.1526122334580862, 285.7045524820243259, -17.32174362185583050 ) ) ;
#81319 = CARTESIAN_POINT ( 'NONE',  ( 80.22169496146727852, 49.80210241725078646, 14.90787428718167185 ) ) ;
#81320 = CARTESIAN_POINT ( 'NONE',  ( 192.4212750754384160, 297.3635704425909125, -12.73704185013552248 ) ) ;
#81321 = DIRECTION ( 'NONE',  ( -0.5000000000000012212, 0.8660254037844379305, 0.000000000000000000 ) ) ;
#81322 = CARTESIAN_POINT ( 'NONE',  ( 203.7037101912997059, 276.1473598535747556, 13.26654772282832973 ) ) ;
#81323 = CARTESIAN_POINT ( 'NONE',  ( 69.36807548234968124, 68.59810528570370991, 7.418719991931705948 ) ) ;
#81324 = CARTESIAN_POINT ( 'NONE',  ( 147.6207754342248961, 274.9603120256437592, 8.795690793376332195 ) ) ;
#81325 = EDGE_CURVE ( 'NONE', #59759, #79145, #51636, .T. ) ;
#81326 = VERTEX_POINT ( 'NONE', #88535 ) ;
#81327 = B_SPLINE_CURVE_WITH_KNOTS ( 'NONE', 3,
 ( #14884, #45289, #32079, #70078, #77715, #23986, #85338 ),
 .UNSPECIFIED., .F., .F.,
 ( 4, 3, 4 ),
 ( 0.0009084163136891124438, 0.001498048609634153143, 0.001783312035702471800 ),
 .UNSPECIFIED. ) ;
#81328 = CARTESIAN_POINT ( 'NONE',  ( -11.09186776771074001, 177.7365022471903444, 2.944929066748280225E-16 ) ) ;
#81329 = CARTESIAN_POINT ( 'NONE',  ( 199.9642529041454395, 269.6475505498956977, -10.52657023967446470 ) ) ;
#81330 = CARTESIAN_POINT ( 'NONE',  ( 118.5230073417626073, 248.4244531367911293, -4.594050593750046652 ) ) ;
#81331 = CARTESIAN_POINT ( 'NONE',  ( 16.58664519722142927, 32.68290643055186706, 3.479690158560446702E-15 ) ) ;
#81332 = CARTESIAN_POINT ( 'NONE',  ( 74.72957723844164946, 67.16412678672320169, 12.46718536312577719 ) ) ;
#81333 = CARTESIAN_POINT ( 'NONE',  ( -7.521556465916533263, 24.12430647450514343, 177.5919119679930134 ) ) ;
#81335 = CARTESIAN_POINT ( 'NONE',  ( 75.28739987566954994, 66.81623516066271407, 13.35525127813182067 ) ) ;
#81334 = CARTESIAN_POINT ( 'NONE',  ( 157.4656258344471098, 257.9085309395441641, 18.30485740784190796 ) ) ;
#81336 = DIRECTION ( 'NONE',  ( 0.000000000000000000, 0.000000000000000000, 1.000000000000000000 ) ) ;
#81337 = ORIENTED_EDGE ( 'NONE', *, *, #41323, .F. ) ;
#81338 = CARTESIAN_POINT ( 'NONE',  ( 195.3619008497734058, 263.0282990088426800, -0.5392206530015204446 ) ) ;
#81339 = CARTESIAN_POINT ( 'NONE',  ( 163.4778819063952540, 247.4949979548153465, 8.784095219806332011 ) ) ;
#81340 = CARTESIAN_POINT ( 'NONE',  ( 192.9343601389454932, 263.4285982009681106, -7.324792422444850182 ) ) ;
#81341 = CARTESIAN_POINT ( 'NONE',  ( 172.8644463536523972, 268.0606821319897790, -16.30213415373016517 ) ) ;
#81342 = CARTESIAN_POINT ( 'NONE',  ( 81.25101512611533394, 55.44295246005403754, -16.34115372143417133 ) ) ;
#81343 = VERTEX_POINT ( 'NONE', #3877 ) ;
#81344 = CARTESIAN_POINT ( 'NONE',  ( 70.15248158267399958, 69.03648656905426151, 7.442703178729979996 ) ) ;
#81345 = AXIS2_PLACEMENT_3D ( 'NONE', #13888, #36675, #37183 ) ;
#81346 = DIRECTION ( 'NONE',  ( 0.000000000000000000, 0.000000000000000000, 1.000000000000000000 ) ) ;
#81347 = ADVANCED_FACE ( 'NONE', ( #34760 ), #59929, .T. ) ;
#81348 = EDGE_CURVE ( 'NONE', #5719, #90285, #22617, .T. ) ;
#81349 = B_SPLINE_SURFACE_WITH_KNOTS ( 'NONE', 3, 1, ( 
 ( #38195, #69111 ),
 ( #7823, #83870 ),
 ( #75744, #45799 ),
 ( #77219, #100038 ),
 ( #85361, #31103 ),
 ( #39188, #15397 ),
 ( #52917, #14433 ),
 ( #76720, #99539 ),
 ( #6328, #91973 ),
 ( #53413, #93456 ),
 ( #7314, #31597 ),
 ( #84855, #30626 ),
 ( #37219, #61002 ),
 ( #46290, #61511 ),
 ( #46814, #69614 ),
 ( #712, #91458 ),
 ( #23004, #62490 ),
 ( #45314, #76249 ),
 ( #92459, #53897 ),
 ( #30120, #6822 ),
 ( #219, #22520 ),
 ( #61990, #92943 ),
 ( #23497, #37706 ),
 ( #84361, #77738 ),
 ( #54387, #24009 ),
 ( #15909, #8323 ),
 ( #70102, #54907 ),
 ( #68119, #99044 ),
 ( #29627, #60501 ),
 ( #63014, #16412 ),
 ( #70610, #1223 ),
 ( #78234, #32103 ),
 ( #24512, #8814 ),
 ( #93960, #85887 ) ),
 .UNSPECIFIED., .T., .F., .F.,
 ( 4, 2, 2, 2, 2, 2, 2, 2, 2, 2, 2, 2, 2, 2, 2, 2, 4 ),
 ( 2, 2 ),
 ( 0.000000000000000000, 0.06250000000000000000, 0.1250000000000000000, 0.1875000000000000000, 0.2500000000000000000, 0.3125000000000000000, 0.3750000000000000000, 0.4375000000000000000, 0.5000000000000000000, 0.5625000000000000000, 0.6250000000000000000, 0.6875000000000000000, 0.7500000000000000000, 0.8125000000000000000, 0.8750000000000000000, 0.9375000000000000000, 1.000000000000000000 ),
 ( 0.000000000000000000, 1.000000000000000000 ),
 .UNSPECIFIED. ) ;
#81350 = CARTESIAN_POINT ( 'NONE',  ( 85.72180487497212198, 45.58971590517442252, 8.620633354355701883 ) ) ;
#81351 = CARTESIAN_POINT ( 'NONE',  ( 200.1567857842741773, 272.1619586071154799, 12.85406770604015492 ) ) ;
#81352 = CARTESIAN_POINT ( 'NONE',  ( 185.8939863203812308, 296.6946888721068945, 4.888489570743712598 ) ) ;
#81353 = CARTESIAN_POINT ( 'NONE',  ( 71.56199657794928726, 71.97676475843201160, -1.390604029342513925 ) ) ;
#81354 = CARTESIAN_POINT ( 'NONE',  ( 147.4771206202524354, 275.6046823160672830, -0.001107820683494442279 ) ) ;
#81355 = ADVANCED_FACE ( 'NONE', ( #23096 ), #60592, .F. ) ;
#81356 = DIRECTION ( 'NONE',  ( -0.8660254037844387076, -0.4999999999999998890, -0.000000000000000000 ) ) ;
#81357 = CARTESIAN_POINT ( 'NONE',  ( 4.858991816890471327, 18.50829794293877839, -10.00000000000000355 ) ) ;
#81358 = CARTESIAN_POINT ( 'NONE',  ( 173.8858844611855829, 272.4353729945644318, -16.46099354089476563 ) ) ;
#81359 = ORIENTED_EDGE ( 'NONE', *, *, #90152, .F. ) ;
#81360 = FACE_OUTER_BOUND ( 'NONE', #48594, .T. ) ;
#81361 = CARTESIAN_POINT ( 'NONE',  ( 194.8067605455144076, 293.2317884077015151, -16.00245909155922774 ) ) ;
#81362 = DIRECTION ( 'NONE',  ( 1.000000000000000000, 0.000000000000000000, 0.000000000000000000 ) ) ;
#81364 = ORIENTED_EDGE ( 'NONE', *, *, #6952, .T. ) ;
#81363 = B_SPLINE_CURVE_WITH_KNOTS ( 'NONE', 3,
 ( #15816, #32012, #24430, #32534, #87310, #9229, #10238, #85270, #71048, #63922, #85795, #94367, #630, #48227, #94861, #77648, #79174, #25421, #48744, #46721 ),
 .UNSPECIFIED., .F., .F.,
 ( 4, 2, 2, 2, 2, 2, 2, 2, 2, 4 ),
 ( 0.003680063676163143182, 0.003801481233049108874, 0.003922898789935074133, 0.004044316346821039826, 0.004165733903707005518, 0.004408569017478878790, 0.004651404131250752062, 0.005137074358794497739, 0.005622744586338243415, 0.007565425496513157599 ),
 .UNSPECIFIED. ) ;
#81366 = EDGE_CURVE ( 'NONE', #81007, #3700, #100130, .T. ) ;
#81365 = CARTESIAN_POINT ( 'NONE',  ( 78.96564777457507489, 59.77152385746119023, 16.49451479044647328 ) ) ;
#81367 = CARTESIAN_POINT ( 'NONE',  ( 185.0905594003060060, 291.6090161883107044, 11.96356110993400002 ) ) ;
#81368 = VECTOR ( 'NONE', #65040, 1000.000000000000000 ) ;
#81369 = CARTESIAN_POINT ( 'NONE',  ( 75.05438881318511335, 53.25138768964912828, 16.03402430238056908 ) ) ;
#81370 = ORIENTED_EDGE ( 'NONE', *, *, #89907, .F. ) ;
#81371 = CARTESIAN_POINT ( 'NONE',  ( 84.39645409570583467, 219.5333772461660544, 9.188101187500095079 ) ) ;
#81372 = CARTESIAN_POINT ( 'NONE',  ( 77.77188545216394289, 52.09635595759155535, -15.62539252360470954 ) ) ;
#81373 = LINE ( 'NONE', #73731, #53712 ) ;
#81374 = CARTESIAN_POINT ( 'NONE',  ( 185.5992489932250464, 259.0872182414688609, -6.824291053258027873 ) ) ;
#81375 = EDGE_CURVE ( 'NONE', #14896, #47944, #52882, .T. ) ;
#81376 = ORIENTED_EDGE ( 'NONE', *, *, #52749, .F. ) ;
#81377 = CARTESIAN_POINT ( 'NONE',  ( 88.48047015690482908, 43.85905421517757929, 0.03257650617625663936 ) ) ;
#81378 = ORIENTED_EDGE ( 'NONE', *, *, #3657, .F. ) ;
#81379 = CARTESIAN_POINT ( 'NONE',  ( 76.91786011064853312, 49.72511384082106645, 15.07646197409581390 ) ) ;
#81380 = ORIENTED_EDGE ( 'NONE', *, *, #29047, .T. ) ;
#81381 = CARTESIAN_POINT ( 'NONE',  ( 75.34515349063467227, 60.38358704892218043, 15.60396358203763967 ) ) ;
#81382 = CARTESIAN_POINT ( 'NONE',  ( 202.7973612924478743, 279.3916619310153919, -15.54732529288344089 ) ) ;
#81383 = EDGE_LOOP ( 'NONE', ( #97644, #81, #59132, #40507 ) ) ;
#81384 = DIRECTION ( 'NONE',  ( -1.000000000000000000, 0.000000000000000000, 1.082076799516502080E-16 ) ) ;
#81385 = CARTESIAN_POINT ( 'NONE',  ( 161.9514198990980560, 255.2405834741430226, -15.02415447469453724 ) ) ;
#81386 = CARTESIAN_POINT ( 'NONE',  ( 162.0346552423833941, 277.4622592605515479, -12.99750001863938031 ) ) ;
#81387 = CARTESIAN_POINT ( 'NONE',  ( 201.1060504099706350, 282.3210983108598384, -18.18000168485860257 ) ) ;
#81388 = DIRECTION ( 'NONE',  ( 0.000000000000000000, 0.000000000000000000, 1.000000000000000000 ) ) ;
#81389 = CARTESIAN_POINT ( 'NONE',  ( 73.44130805767331083, 68.03446431250019089, -11.12216700113787127 ) ) ;
#81390 = CARTESIAN_POINT ( 'NONE',  ( 140.4447960187037552, 242.7048013555409796, 4.594050593750051981 ) ) ;
#81391 = VERTEX_POINT ( 'NONE', #39283 ) ;
#81392 = CARTESIAN_POINT ( 'NONE',  ( 75.72846040655473132, 54.99831286504160488, 16.13249358657354193 ) ) ;
#81393 = CARTESIAN_POINT ( 'NONE',  ( 6.618913549016022912, 24.79752408145590081, -5.678558825948271327 ) ) ;
#81394 = EDGE_LOOP ( 'NONE', ( #12060, #43964, #70892, #15265 ) ) ;
#81396 = VERTEX_POINT ( 'NONE', #24104 ) ;
#81395 = CARTESIAN_POINT ( 'NONE',  ( -19.65312891409030271, 93.06504152958497400, -10.00000000000000888 ) ) ;
#81397 = DIRECTION ( 'NONE',  ( -0.5000000000000003331, 0.8660254037844385966, -2.273449890178237515E-16 ) ) ;
#81398 = DIRECTION ( 'NONE',  ( -0.1550826972584532226, -0.9879014915521905360, 0.000000000000000000 ) ) ;
#81399 = CARTESIAN_POINT ( 'NONE',  ( -17.42236680055705023, 149.2012482093457777, 0.000000000000000000 ) ) ;
#81400 = LINE ( 'NONE', #87540, #68957 ) ;
#81401 = CARTESIAN_POINT ( 'NONE',  ( 87.11157952361327261, 44.55241027477293869, 5.348311053102904999 ) ) ;
#81402 = CARTESIAN_POINT ( 'NONE',  ( 88.04428041263226135, 44.10238440132638971, -1.708206819958570044 ) ) ;
#81403 = ORIENTED_EDGE ( 'NONE', *, *, #23068, .T. ) ;
#81404 = CARTESIAN_POINT ( 'NONE',  ( 185.1126663572763675, 273.1539052423648286, -16.71538631548864018 ) ) ;
#81405 = CARTESIAN_POINT ( 'NONE',  ( 66.18888642898470209, 69.34007213467177166, 0.2082648703207360674 ) ) ;
#81406 = ORIENTED_EDGE ( 'NONE', *, *, #60899, .T. ) ;
#81407 = CARTESIAN_POINT ( 'NONE',  ( 194.3193926313213638, 293.6800862088419422, -14.28503170336555428 ) ) ;
#81408 = CARTESIAN_POINT ( 'NONE',  ( 200.9494940653346191, 267.7474625779211124, -2.675924154422841816 ) ) ;
#81409 = LINE ( 'NONE', #44347, #6186 ) ;
#81410 = CARTESIAN_POINT ( 'NONE',  ( -35.27139336136212933, 24.82964151130203945, 177.5919119679930134 ) ) ;
#81412 = AXIS2_PLACEMENT_3D ( 'NONE', #17069, #16573, #57064 ) ;
#81411 = CARTESIAN_POINT ( 'NONE',  ( 164.6805913154744587, 274.3217421407699703, 14.82948928037302672 ) ) ;
#81414 = CARTESIAN_POINT ( 'NONE',  ( 88.28948486398485329, 44.33448523864236535, 2.244918718876048214 ) ) ;
#81413 = FACE_OUTER_BOUND ( 'NONE', #90981, .T. ) ;
#81415 = EDGE_CURVE ( 'NONE', #81073, #83731, #31683, .T. ) ;
#81416 = CARTESIAN_POINT ( 'NONE',  ( 200.0126145424869719, 267.7195842788145228, 6.153478395924335764 ) ) ;
#81417 = EDGE_LOOP ( 'NONE', ( #65346, #60009, #63235, #67106 ) ) ;
#81418 = CARTESIAN_POINT ( 'NONE',  ( 78.84444043921700995, 60.06282491878221919, -16.09152508400769932 ) ) ;
#81419 = CARTESIAN_POINT ( 'NONE',  ( 191.9824032073976241, 287.6194387751458521, -17.05427143794285882 ) ) ;
#81420 = AXIS2_PLACEMENT_3D ( 'NONE', #21378, #99878, #37066 ) ;
#81421 = EDGE_CURVE ( 'NONE', #89705, #1456, #23590, .T. ) ;
#81422 = PLANE ( 'NONE',  #6338 ) ;
#81423 = CARTESIAN_POINT ( 'NONE',  ( 152.9489295551198893, 265.7316783776963121, 17.71675637597311237 ) ) ;
#81424 = CARTESIAN_POINT ( 'NONE',  ( 80.84042243888920609, 43.63393987770743365, -9.572765014343259438 ) ) ;
#81425 = CARTESIAN_POINT ( 'NONE',  ( 50.39593590098449738, 193.2365022471902307, 10.00000000000009948 ) ) ;
#81426 = CARTESIAN_POINT ( 'NONE',  ( 8.267668766103758671, 166.3923013555410080, 4.594050593750050204 ) ) ;
#81427 = CARTESIAN_POINT ( 'NONE',  ( 114.4640339051705666, 227.7048013555410080, 4.594050593750051981 ) ) ;
#81428 = CARTESIAN_POINT ( 'NONE',  ( 155.0453531195792038, 262.1005662498678817, -18.46987289964740953 ) ) ;
#81429 = CARTESIAN_POINT ( 'NONE',  ( 87.89481703180801730, 44.20627101738029552, -4.400163950806250668 ) ) ;
#81430 = CARTESIAN_POINT ( 'NONE',  ( 186.1869626216079894, 296.9195626386382969, -7.441086137094660380 ) ) ;
#81431 = EDGE_CURVE ( 'NONE', #32592, #26456, #16504, .T. ) ;
#81432 = CARTESIAN_POINT ( 'NONE',  ( 77.70006599894800559, 50.25350553986154978, 15.10357061109865917 ) ) ;
#81433 = AXIS2_PLACEMENT_3D ( 'NONE', #29239, #83465, #44419 ) ;
#81434 = CARTESIAN_POINT ( 'NONE',  ( -27.42236680055714260, 166.5217562850347406, 1.224646799147364892E-15 ) ) ;
#81435 = CARTESIAN_POINT ( 'NONE',  ( 163.9287928004966375, 283.7425982196886594, 5.719485170213416403 ) ) ;
#81436 = CARTESIAN_POINT ( 'NONE',  ( 148.4042165687623083, 273.6033521758856750, -8.709765892313745539 ) ) ;
#81437 = ADVANCED_FACE ( 'NONE', ( #1318 ), #16733, .F. ) ;
#81438 = CARTESIAN_POINT ( 'NONE',  ( 84.24654968840980018, 50.62473343291171801, 13.78984717790371661 ) ) ;
#81439 = CARTESIAN_POINT ( 'NONE',  ( 48.58805178314242568, 84.67719436603331928, -10.00000000000000000 ) ) ;
#81440 = FACE_OUTER_BOUND ( 'NONE', #23148, .T. ) ;
#81441 = EDGE_CURVE ( 'NONE', #11960, #24507, #28664, .T. ) ;
#81442 = CARTESIAN_POINT ( 'NONE',  ( 172.8108118737807786, 263.0936288908736174, -15.55104684167783091 ) ) ;
#81443 = CARTESIAN_POINT ( 'NONE',  ( 80.33713356334875755, 211.0643266524159856, -9.188101187500093303 ) ) ;
#81444 = CARTESIAN_POINT ( 'NONE',  ( 207.8575108622103755, 270.6272257822888037, -6.381720258959569847 ) ) ;
#81445 = CARTESIAN_POINT ( 'NONE',  ( 83.19206654810436419, 51.10784717693168488, -14.73575672656897240 ) ) ;
#81446 = DIRECTION ( 'NONE',  ( 1.000000000000000000, 0.000000000000000000, 0.000000000000000000 ) ) ;
#81448 = DIRECTION ( 'NONE',  ( 0.7440200784635646603, 0.6681572590663601430, 0.000000000000000000 ) ) ;
#81447 = CARTESIAN_POINT ( 'NONE',  ( 196.3519702320103590, 290.5554067223432639, 17.39042812051341969 ) ) ;
#81449 = CARTESIAN_POINT ( 'NONE',  ( 151.1230807375396807, 268.8941412966845519, -14.26613110909109849 ) ) ;
#81450 = CARTESIAN_POINT ( 'NONE',  ( 79.98829826350832661, 44.59498145193617802, 11.76229303994366049 ) ) ;
#81451 = CARTESIAN_POINT ( 'NONE',  ( 38.48863484149603664, 25.14754757982092670, -5.678558825948275768 ) ) ;
#81452 = CARTESIAN_POINT ( 'NONE',  ( 193.1169444172380167, 296.1586357973259283, -13.13373377033755318 ) ) ;
#81453 = CARTESIAN_POINT ( 'NONE',  ( 76.26946404230704957, 64.97317754398874001, 14.67006731301515998 ) ) ;
#81454 = ORIENTED_EDGE ( 'NONE', *, *, #13247, .T. ) ;
#81455 = CARTESIAN_POINT ( 'NONE',  ( 22.71615395846560759, 25.06628583063842086, -9.188101187500006262 ) ) ;
#81456 = EDGE_CURVE ( 'NONE', #35189, #89364, #22756, .T. ) ;
#81457 = CARTESIAN_POINT ( 'NONE',  ( 173.0357146759456271, 289.9031501978675465, -0.5316909439790075131 ) ) ;
#81458 = DIRECTION ( 'NONE',  ( -0.7499999999999995559, -0.4330127018922196314, 0.5000000000000004441 ) ) ;
#81459 = CARTESIAN_POINT ( 'NONE',  ( 188.0020763875417629, 286.0549491211741042, -16.57088730622232120 ) ) ;
#81460 = PLANE ( 'NONE',  #93941 ) ;
#81461 = CARTESIAN_POINT ( 'NONE',  ( 74.68164300898216368, 63.81063734443356594, 14.78194474382439694 ) ) ;
#81462 = DIRECTION ( 'NONE',  ( 0.4851478631379963491, -0.8403007481384849875, 0.2419218955996714493 ) ) ;
#81463 = CARTESIAN_POINT ( 'NONE',  ( 143.9266795097038596, 247.2365022471902023, 10.00000000000009592 ) ) ;
#81464 = DIRECTION ( 'NONE',  ( 0.8660254037844378194, 0.5000000000000014433, 0.000000000000000000 ) ) ;
#81465 = EDGE_CURVE ( 'NONE', #49648, #46249, #54124, .T. ) ;
#81466 = CARTESIAN_POINT ( 'NONE',  ( 75.11518065281146050, 53.26383345445703554, 16.03154839982004631 ) ) ;
#81467 = EDGE_LOOP ( 'NONE', ( #11247, #1076, #88607 ) ) ;
#81468 = CARTESIAN_POINT ( 'NONE',  ( 165.7517492418863014, 246.5407772836408355, -1.235758156293855103 ) ) ;
#81469 = ORIENTED_EDGE ( 'NONE', *, *, #46783, .T. ) ;
#81470 = CARTESIAN_POINT ( 'NONE',  ( 162.6264071486809542, 248.9697954965390920, 10.36322805486644683 ) ) ;
#81471 = CARTESIAN_POINT ( 'NONE',  ( 83.08202181667390107, 41.27958953865602609, 0.4477113809661833477 ) ) ;
#81472 = VERTEX_POINT ( 'NONE', #50400 ) ;
#81473 = LINE ( 'NONE', #49045, #19240 ) ;
#81474 = B_SPLINE_CURVE_WITH_KNOTS ( 'NONE', 3,
 ( #9080, #70887, #84134, #14683, #45564, #7071, #37956, #41458, #41969, #88637 ),
 .UNSPECIFIED., .F., .F.,
 ( 4, 2, 2, 2, 4 ),
 ( 0.000000000000000000, 0.2500000000000000000, 0.5000000000000000000, 0.7500000000000000000, 1.000000000000000000 ),
 .UNSPECIFIED. ) ;
#81475 = VERTEX_POINT ( 'NONE', #13418 ) ;
#81477 = EDGE_CURVE ( 'NONE', #56511, #21034, #37141, .T. ) ;
#81476 = CARTESIAN_POINT ( 'NONE',  ( 191.5566566914955331, 291.3450863069615480, 14.65428652378087371 ) ) ;
#81478 = CARTESIAN_POINT ( 'NONE',  ( 6.688470478837180266, 19.56454794089038884, 10.00000000000000355 ) ) ;
#81479 = CARTESIAN_POINT ( 'NONE',  ( 145.4512450625087467, 254.7833772461660544, -9.188101187500095079 ) ) ;
#81480 = CARTESIAN_POINT ( 'NONE',  ( 88.01192408641850307, 44.27121890238829138, -4.391744778743009725 ) ) ;
#81481 = CARTESIAN_POINT ( 'NONE',  ( 202.3879523842396111, 275.1512786724707098, -14.15337613030473918 ) ) ;
#81482 = VECTOR ( 'NONE', #31187, 1000.000000000000114 ) ;
#81483 = CARTESIAN_POINT ( 'NONE',  ( 43.68655075043449898, 184.4824982072973967, 3.021315404115420679E-15 ) ) ;
#81484 = ADVANCED_FACE ( 'NONE', ( #82847 ), #11924, .T. ) ;
#81485 = CARTESIAN_POINT ( 'NONE',  ( 37.81746515356308436, 24.76004757982092386, 5.678558825948272215 ) ) ;
#81486 = CARTESIAN_POINT ( 'NONE',  ( 73.91582071829171241, 60.33129874575597995, -15.38455064745800449 ) ) ;
#81487 = VECTOR ( 'NONE', #73306, 1000.000000000000000 ) ;
#81488 = DIRECTION ( 'NONE',  ( 0.8660254037844395958, 0.4999999999999985567, 0.000000000000000000 ) ) ;
#81489 = CARTESIAN_POINT ( 'NONE',  ( 44.69460199273685674, 206.6115022471903160, -5.000000000000047962 ) ) ;
#81490 = ORIENTED_EDGE ( 'NONE', *, *, #69772, .T. ) ;
#81491 = ORIENTED_EDGE ( 'NONE', *, *, #21677, .T. ) ;
#81492 = CARTESIAN_POINT ( 'NONE',  ( 87.11651898459504650, 46.29685661633757832, -9.218154771921559743 ) ) ;
#81494 = CYLINDRICAL_SURFACE ( 'NONE', #28151, 70.00000000000002842 ) ;
#81493 = CARTESIAN_POINT ( 'NONE',  ( 163.7136804588959649, 247.0865828815331042, 6.783386239354816105 ) ) ;
#81495 = DIRECTION ( 'NONE',  ( 0.000000000000000000, 0.000000000000000000, 1.000000000000000000 ) ) ;
#81496 = CARTESIAN_POINT ( 'NONE',  ( 66.06609959339904492, 68.51740553072025364, -2.387806098926052556 ) ) ;
#81497 = AXIS2_PLACEMENT_3D ( 'NONE', #68803, #45989, #67824 ) ;
#81498 = CARTESIAN_POINT ( 'NONE',  ( 147.7840666256145425, 276.6774833857293174, 0.9737628777943441172 ) ) ;
#81499 = DIRECTION ( 'NONE',  ( 0.5000000000000001110, -0.8660254037844385966, 2.065951763267645480E-16 ) ) ;
#81500 = CARTESIAN_POINT ( 'NONE',  ( 164.0303808347895256, 246.5380417397093140, 5.465094127736859875 ) ) ;
#81501 = CARTESIAN_POINT ( 'NONE',  ( 168.8523083975146903, 266.9327454831334876, 16.71699773333943284 ) ) ;
#81502 = AXIS2_PLACEMENT_3D ( 'NONE', #7804, #31085, #93942 ) ;
#81503 = DIRECTION ( 'NONE',  ( -0.000000000000000000, 0.000000000000000000, 1.000000000000000000 ) ) ;
#81504 = ORIENTED_EDGE ( 'NONE', *, *, #82054, .T. ) ;
#81505 = CARTESIAN_POINT ( 'NONE',  ( 190.8443993347725325, 300.0947993426467519, 8.522468760355437212 ) ) ;
#81506 = CARTESIAN_POINT ( 'NONE',  ( 163.3750637014402400, 276.5743216800318010, -13.80359379715451773 ) ) ;
#81507 = ORIENTED_EDGE ( 'NONE', *, *, #79651, .F. ) ;
#81508 = CARTESIAN_POINT ( 'NONE',  ( 87.02238245971742003, 45.93041326596856777, -8.141809006855861952 ) ) ;
#81509 = CARTESIAN_POINT ( 'NONE',  ( 177.8737369365807410, 292.6277481362276944, -2.671055768360467209 ) ) ;
#81510 = CARTESIAN_POINT ( 'NONE',  ( 196.2255671652529259, 290.7743432561995860, 16.01325193769018185 ) ) ;
#81511 = CARTESIAN_POINT ( 'NONE',  ( 9.347034241948367850, 24.13478043621386604, 8.090169943749478065 ) ) ;
#81512 = CARTESIAN_POINT ( 'NONE',  ( 208.1864700626310025, 270.0574517335433598, 2.990990977286084096 ) ) ;
#81513 = B_SPLINE_CURVE_WITH_KNOTS ( 'NONE', 3,
 ( #99709, #36893, #14605, #98730 ),
 .UNSPECIFIED., .F., .F.,
 ( 4, 4 ),
 ( 0.000000000000000000, 0.0003401861652890088511 ),
 .UNSPECIFIED. ) ;
#81514 = VERTEX_POINT ( 'NONE', #97053 ) ;
#81515 = ORIENTED_EDGE ( 'NONE', *, *, #42742, .F. ) ;
#81516 = CARTESIAN_POINT ( 'NONE',  ( 207.6067494229581314, 271.0615573356529353, -1.924113146155245868 ) ) ;
#81517 = ORIENTED_EDGE ( 'NONE', *, *, #49835, .F. ) ;
#81518 = ADVANCED_FACE ( 'NONE', ( #53740 ), #38039, .F. ) ;
#81519 = CARTESIAN_POINT ( 'NONE',  ( 194.6851553498462124, 266.4313783899017380, -7.994026154862396538 ) ) ;
#81520 = DIRECTION ( 'NONE',  ( 0.4999999999999987788, -0.8660254037844392627, -0.000000000000000000 ) ) ;
#81521 = CARTESIAN_POINT ( 'NONE',  ( 71.84099058795369785, 69.36843466522826418, -8.537052276230351566 ) ) ;
#81523 = DIRECTION ( 'NONE',  ( -0.8660254037844387076, -0.4999999999999998890, -0.000000000000000000 ) ) ;
#81522 = CARTESIAN_POINT ( 'NONE',  ( 140.4447960187037552, 242.7048013555409796, 4.594050593750051981 ) ) ;
#81524 = CARTESIAN_POINT ( 'NONE',  ( -10.89340361622470610, 174.5177522451419350, 5.000000000000046185 ) ) ;
#81525 = CARTESIAN_POINT ( 'NONE',  ( 180.9226702965857783, 295.6987777469875027, 2.116087624927042388 ) ) ;
#81526 = ORIENTED_EDGE ( 'NONE', *, *, #91560, .T. ) ;
#81527 = CARTESIAN_POINT ( 'NONE',  ( 156.8993174718108605, 258.8894057963813680, 16.93179113901802069 ) ) ;
#81528 = CARTESIAN_POINT ( 'NONE',  ( 82.50650581714903353, 51.91895525678945233, 14.80017960748231154 ) ) ;
#81529 = CARTESIAN_POINT ( 'NONE',  ( 82.41933087055697627, 40.38430946167127900, -0.8419157719606891188 ) ) ;
#81530 = CARTESIAN_POINT ( 'NONE',  ( 189.2738920610548803, 270.0414595828373763, 14.42171763143272756 ) ) ;
#81531 = CARTESIAN_POINT ( 'NONE',  ( 42.60170726692454224, 188.7365022471902023, 10.00000000000009948 ) ) ;
#81532 = FACE_OUTER_BOUND ( 'NONE', #71899, .T. ) ;
#81533 = CARTESIAN_POINT ( 'NONE',  ( 82.22136387774217781, 40.60583099706693133, -3.205559772122553497 ) ) ;
#81534 = DIRECTION ( 'NONE',  ( 0.4999999999999998890, -0.8660254037844385966, 0.000000000000000000 ) ) ;
#81535 = CARTESIAN_POINT ( 'NONE',  ( 79.50423164993438263, 48.29920615383874605, 13.87520480776860055 ) ) ;
#81536 = CYLINDRICAL_SURFACE ( 'NONE', #18804, 17.82106496071139645 ) ;
#81537 = CARTESIAN_POINT ( 'NONE',  ( 160.0081047537594543, 253.5048282741223602, -16.11956848123596941 ) ) ;
#81538 = CARTESIAN_POINT ( 'NONE',  ( -37.40701240123934213, 25.35389310390295137, 10.00000000000000000 ) ) ;
#81539 = CARTESIAN_POINT ( 'NONE',  ( 208.2874212803407090, 269.8825990953837390, -1.143705256421198690 ) ) ;
#81540 = DIRECTION ( 'NONE',  ( 0.000000000000000000, 1.000000000000000000, 0.000000000000000000 ) ) ;
#81541 = EDGE_CURVE ( 'NONE', #58155, #32950, #39590, .T. ) ;
#81542 = VECTOR ( 'NONE', #28452, 1000.000000000000000 ) ;
#81543 = CARTESIAN_POINT ( 'NONE',  ( 70.13236730935095409, 70.74420383565504267, -3.402677824215883717 ) ) ;
#81545 = CARTESIAN_POINT ( 'NONE',  ( 185.4417336918466219, 266.3141122328166830, 13.06621773694827837 ) ) ;
#81544 = FACE_OUTER_BOUND ( 'NONE', #14354, .T. ) ;
#81546 = DIRECTION ( 'NONE',  ( -0.8660254037844378194, -0.5000000000000014433, -0.000000000000000000 ) ) ;
#81547 = EDGE_CURVE ( 'NONE', #57418, #40435, #20018, .T. ) ;
#81548 = CARTESIAN_POINT ( 'NONE',  ( 32.57180473799248688, 34.50829794293882458, -10.00000000000000355 ) ) ;
#81549 = FACE_OUTER_BOUND ( 'NONE', #50651, .T. ) ;
#81550 = CARTESIAN_POINT ( 'NONE',  ( 38.90713690219553200, 54.71539658304152454, -10.00000000000000000 ) ) ;
#81551 = CARTESIAN_POINT ( 'NONE',  ( 86.01409551425155087, 42.49941138162544263, 1.569904702652799910 ) ) ;
#81552 = CARTESIAN_POINT ( 'NONE',  ( 49.10122569834316408, 93.29622288527660601, -10.00000000000000000 ) ) ;
#81553 = ADVANCED_FACE ( 'NONE', ( #43287 ), #5309, .F. ) ;
#81554 = CIRCLE ( 'NONE', #97731, 0.1418229129680828593 ) ;
#81555 = CARTESIAN_POINT ( 'NONE',  ( 11.65032017781297036, 177.5333772461660544, 9.188101187500095079 ) ) ;
#81556 = DIRECTION ( 'NONE',  ( -0.8660254037844387076, -0.4999999999999998890, -0.000000000000000000 ) ) ;
#81557 = VERTEX_POINT ( 'NONE', #66602 ) ;
#81559 = CARTESIAN_POINT ( 'NONE',  ( 86.98337649904340196, 46.47637665038675436, 8.932041053647461482 ) ) ;
#81558 = VECTOR ( 'NONE', #39293, 999.9999999999998863 ) ;
#81560 = CARTESIAN_POINT ( 'NONE',  ( 28.53675269070083331, 198.8297689869269220, -2.679491924311252493 ) ) ;
#81561 = CARTESIAN_POINT ( 'NONE',  ( 38.60757266705294910, 27.45404122711136452, -8.090169943749478065 ) ) ;
#81562 = CARTESIAN_POINT ( 'NONE',  ( 38.44315465527655107, 186.8768266524159856, -9.188101187500093303 ) ) ;
#81563 = CARTESIAN_POINT ( 'NONE',  ( 87.32537421964468649, 46.00455475262659633, 8.658505635391252397 ) ) ;
#81564 = CARTESIAN_POINT ( 'NONE',  ( 190.6218339396177441, 300.4802939150614520, -4.178005820806754755 ) ) ;
#81565 = CARTESIAN_POINT ( 'NONE',  ( 39.23990543832260869, 24.78380873178790011, -6.180339887498949025 ) ) ;
#81566 = CARTESIAN_POINT ( 'NONE',  ( 202.9297445357156278, 270.0237240353077937, -6.443924261151921407 ) ) ;
#81567 = CARTESIAN_POINT ( 'NONE',  ( 147.1447476476323004, 275.7848163378367872, 0.6373001129109078233 ) ) ;
#81568 = CARTESIAN_POINT ( 'NONE',  ( 87.35606880162970356, 45.77061481740687299, 8.290963297571641633 ) ) ;
#81569 = CARTESIAN_POINT ( 'NONE',  ( 70.54949879551072911, 67.86437491032424418, -9.416702132505674783 ) ) ;
#81570 = PRODUCT_DEFINITION_SHAPE ( 'NONE', 'NONE',  #21642 ) ;
#81571 = CARTESIAN_POINT ( 'NONE',  ( 166.8565011125344597, 257.6213196747827965, -15.76983133553760297 ) ) ;
#81572 = CARTESIAN_POINT ( 'NONE',  ( -34.16292631813981728, 25.86630820016799248, 10.00000000000000000 ) ) ;
#81573 = CARTESIAN_POINT ( 'NONE',  ( 200.2362722391634975, 283.4274695507068600, 16.82377321601456899 ) ) ;
#81574 = CARTESIAN_POINT ( 'NONE',  ( 87.62133583293774564, 45.31115884160844587, -7.293173845241980757 ) ) ;
#81576 =( BOUNDED_CURVE ( )  B_SPLINE_CURVE ( 2, ( #70253, #62641, #32756, #10472, #9474, #2383, #93598, #63660, #40343 ),
 .UNSPECIFIED., .F., .T. ) 
 B_SPLINE_CURVE_WITH_KNOTS ( ( 3, 2, 2, 2, 3 ),
 ( 0.1250000000000000000, 0.1263440860215053752, 0.1290322580645161255, 0.1317204301075268758, 0.1330645161290322509 ),
 .UNSPECIFIED. ) 
 CURVE ( )  GEOMETRIC_REPRESENTATION_ITEM ( )  RATIONAL_B_SPLINE_CURVE ( ( 0.9330127018922194093, 0.9330127018922194093, 1.000000000000000000, 0.8660254037844387076, 1.000000000000000000, 0.8660254037844387076, 1.000000000000000000, 0.9330127018922194093, 0.9330127018922194093 ) ) 
 REPRESENTATION_ITEM ( '' )  );
#81575 = CARTESIAN_POINT ( 'NONE',  ( 80.63465624979117763, 207.3615022471901739, 5.000000000000051514 ) ) ;
#81577 = CARTESIAN_POINT ( 'NONE',  ( 183.5953950971229744, 289.9057545191589043, -13.74357891376704544 ) ) ;
#81578 = ADVANCED_FACE ( 'NONE', ( #98015 ), #59474, .T. ) ;
#81579 = DIRECTION ( 'NONE',  ( -0.8660254037844378194, -0.5000000000000014433, -0.000000000000000000 ) ) ;
#81580 = ORIENTED_EDGE ( 'NONE', *, *, #24112, .T. ) ;
#81581 = CARTESIAN_POINT ( 'NONE',  ( 44.82974491242176640, 202.8149278399160664, 9.188101187500093303 ) ) ;
#81582 = EDGE_LOOP ( 'NONE', ( #19005, #13314, #29570, #76129 ) ) ;
#81583 = CYLINDRICAL_SURFACE ( 'NONE', #56183, 3.300000000000010925 ) ;
#81584 = CARTESIAN_POINT ( 'NONE',  ( 190.3791419447713906, 300.9006487807255326, -5.688668718458480988 ) ) ;
#81585 = CARTESIAN_POINT ( 'NONE',  ( 67.68514482100738405, 66.83340866827893478, -8.536435324610973652 ) ) ;
#81586 = ORIENTED_EDGE ( 'NONE', *, *, #62011, .F. ) ;
#81587 = CARTESIAN_POINT ( 'NONE',  ( 170.8851693353173005, 287.3571709677545982, 8.586156227924460538 ) ) ;
#81588 = CARTESIAN_POINT ( 'NONE',  ( 206.8986117509267899, 272.2880877623646825, 6.975890063856878598 ) ) ;
#81589 = DIRECTION ( 'NONE',  ( 1.000000000000000000, 7.930164461608259453E-16, 0.000000000000000000 ) ) ;
#81590 = CARTESIAN_POINT ( 'NONE',  ( 29.04415360562664361, 34.95586893147757479, 7.433330006724141015 ) ) ;
#81591 = CARTESIAN_POINT ( 'NONE',  ( 72.93270222632347100, 70.75261854202813083, -7.421515863126944446 ) ) ;
#81592 = DIRECTION ( 'NONE',  ( 0.000000000000000000, -0.000000000000000000, -1.000000000000000000 ) ) ;
#81593 = CARTESIAN_POINT ( 'NONE',  ( 171.6154833087297789, 255.2606305366970503, 12.53362356821959978 ) ) ;
#81594 = EDGE_LOOP ( 'NONE', ( #67148, #53269, #319, #40051 ) ) ;
#81595 = CARTESIAN_POINT ( 'NONE',  ( 16.32921660555538423, 21.37878583063840310, 9.188101187500006262 ) ) ;
#81596 = DIRECTION ( 'NONE',  ( -0.6544109481086123337, -0.7561390817803210762, 0.000000000000000000 ) ) ;
#81597 = CARTESIAN_POINT ( 'NONE',  ( 174.8904491429100574, 255.1896265538727846, 8.186123047353046189 ) ) ;
#81598 = PLANE ( 'NONE',  #32695 ) ;
#81599 = EDGE_CURVE ( 'NONE', #6177, #73699, #82014, .T. ) ;
#81600 = ORIENTED_EDGE ( 'NONE', *, *, #96875, .F. ) ;
#81601 = CARTESIAN_POINT ( 'NONE',  ( 180.2906877376209138, 282.9895530604892997, 15.04284179662483645 ) ) ;
#81602 = CARTESIAN_POINT ( 'NONE',  ( 191.3375250863502970, 299.2406804863936145, 8.828791580707859410 ) ) ;
#81603 = CARTESIAN_POINT ( 'NONE',  ( -40.14225747417106760, 26.13077817479420872, -10.00000000000000000 ) ) ;
#81604 = VERTEX_POINT ( 'NONE', #77579 ) ;
#81606 = DIRECTION ( 'NONE',  ( -0.5000000000000002220, 0.8660254037844385966, 0.000000000000000000 ) ) ;
#81605 = CARTESIAN_POINT ( 'NONE',  ( 161.1232569692349443, 251.5733279787459367, -14.02750397520710557 ) ) ;
#81607 = CARTESIAN_POINT ( 'NONE',  ( 196.3286486926436680, 290.5958008134369948, -16.58330917766970458 ) ) ;
#81608 = ORIENTED_EDGE ( 'NONE', *, *, #74132, .T. ) ;
#81609 = CARTESIAN_POINT ( 'NONE',  ( 65.84838944952173279, 68.97303637434430357, -2.219146741909078457 ) ) ;
#81610 = FACE_OUTER_BOUND ( 'NONE', #18123, .T. ) ;
#81611 = CARTESIAN_POINT ( 'NONE',  ( 58.97569090598252473, 178.8759306620404175, -18.47570218321542868 ) ) ;
#81612 = CARTESIAN_POINT ( 'NONE',  ( 78.17116731237634042, 61.83023861435394508, -16.09040300007290725 ) ) ;
#81613 = CARTESIAN_POINT ( 'NONE',  ( 72.12219891194473576, 72.29872703567703240, -1.398582990988473718 ) ) ;
#81614 = CARTESIAN_POINT ( 'NONE',  ( 107.5083335113205578, 239.0024278399160949, 9.188101187500095079 ) ) ;
#81615 = CYLINDRICAL_SURFACE ( 'NONE', #97445, 49.99999999999999289 ) ;
#81616 = DIRECTION ( 'NONE',  ( 0.5000000000000001110, -0.8660254037844384856, -0.000000000000000000 ) ) ;
#81617 = ORIENTED_EDGE ( 'NONE', *, *, #95627, .F. ) ;
#81618 = CARTESIAN_POINT ( 'NONE',  ( 208.0287371622045782, 270.3306531311065442, 3.558879245883286746 ) ) ;
#81619 = VERTEX_POINT ( 'NONE', #94796 ) ;
#81620 = CARTESIAN_POINT ( 'NONE',  ( 32.07042461746584650, 33.91421378149919974, 9.188101187500008038 ) ) ;
#81621 = FACE_BOUND ( 'NONE', #40286, .T. ) ;
#81622 = CARTESIAN_POINT ( 'NONE',  ( 75.28408590364399799, 66.87309274870622744, -12.87999511164833244 ) ) ;
#81623 = CARTESIAN_POINT ( 'NONE',  ( 65.93911412966745900, 215.0024278399160664, 9.188101187500095079 ) ) ;
#81624 = ORIENTED_EDGE ( 'NONE', *, *, #52578, .F. ) ;
#81625 = CARTESIAN_POINT ( 'NONE',  ( -30.49513100206280569, 95.94612159648924887, 12.72072555747216249 ) ) ;
#81626 = CARTESIAN_POINT ( 'NONE',  ( 119.6057994200909036, 229.8615022471901739, 5.000000000000051514 ) ) ;
#81627 = CARTESIAN_POINT ( 'NONE',  ( 154.8838596469624349, 262.3802811495310152, 18.07457254681616021 ) ) ;
#81628 = CARTESIAN_POINT ( 'NONE',  ( 172.2631232552246843, 276.7629437217855752, 15.87404649013240210 ) ) ;
#81629 = ORIENTED_EDGE ( 'NONE', *, *, #23271, .T. ) ;
#81630 = AXIS2_PLACEMENT_3D ( 'NONE', #45495, #28304, #22209 ) ;
#81631 = EDGE_CURVE ( 'NONE', #315, #20041, #56248, .T. ) ;
#81632 = B_SPLINE_CURVE_WITH_KNOTS ( 'NONE', 3,
 ( #46642, #7648, #77567, #53249, #62840, #84205, #92297, #9154, #16249, #40030, #22848, #68939, #70970, #77041, #84690, #8155, #99865, #31935, #1572, #15735, #53731, #46127, #92782, #69446, #8651, #63352, #22353, #70447, #76560, #554, #30449, #23336, #47139, #63, #30946, #54224, #85190, #39029, #78064, #69937, #31436, #93282, #23838, #54731, #26857, #56239, #11669, #72484, #25346, #10163 ),
 .UNSPECIFIED., .F., .F.,
 ( 4, 2, 2, 2, 2, 2, 2, 2, 2, 2, 2, 2, 2, 2, 2, 2, 2, 2, 2, 2, 2, 2, 2, 2, 4 ),
 ( 0.001466970120733069325, 0.001928437086138543640, 0.002389904051544017739, 0.002620637534246755655, 0.002736004275598119193, 0.002851371016949482730, 0.002966737758300846267, 0.003082104499652209804, 0.003312837982354939481, 0.003774304947760222760, 0.004235771913165505172, 0.005158705843975971983, 0.006081639774786438794, 0.006543106740191636204, 0.007004573705596833615, 0.007119940446948069650, 0.007177623817623719760, 0.007235307188299369870, 0.007350673929650749887, 0.007466040671002129904, 0.007696774153704884734, 0.007927507636407640432, 0.008158241119110395262, 0.008388974601813150092, 0.008850441567218573016 ),
 .UNSPECIFIED. ) ;
#81633 = CARTESIAN_POINT ( 'NONE',  ( 121.6288370910339864, 229.4824982072973398, 3.021315404115420679E-15 ) ) ;
#81634 = CARTESIAN_POINT ( 'NONE',  ( 47.05668214639808156, 76.45164061169337799, 10.00000000000000000 ) ) ;
#81635 = CARTESIAN_POINT ( 'NONE',  ( 155.5211745099813356, 261.2764194263634749, -17.18163098020766810 ) ) ;
#81636 = VERTEX_POINT ( 'NONE', #72 ) ;
#81637 = CARTESIAN_POINT ( 'NONE',  ( 148.7149237849385770, 273.0651914911900917, 9.533111688205226031 ) ) ;
#81638 = CARTESIAN_POINT ( 'NONE',  ( 44.08135397534552169, 118.8355609772188188, -10.00000000000000000 ) ) ;
#81639 = EDGE_CURVE ( 'NONE', #85118, #66481, #66180, .T. ) ;
#81640 = CARTESIAN_POINT ( 'NONE',  ( 207.1007598919583472, 271.9379569114424271, -6.086525981869248092 ) ) ;
#81641 = CARTESIAN_POINT ( 'NONE',  ( 83.42542119994750749, 51.64995580955420706, -14.90072893730332027 ) ) ;
#81642 = CIRCLE ( 'NONE', #88171, 70.00000000000001421 ) ;
#81643 = LINE ( 'NONE', #82152, #73678 ) ;
#81644 = CARTESIAN_POINT ( 'NONE',  ( 153.0305350670531936, 277.3750776671890890, 8.290292975357761662 ) ) ;
#81645 = CARTESIAN_POINT ( 'NONE',  ( 152.3606757194620229, 270.2396459880571342, -14.76350148286496555 ) ) ;
#81646 = DIRECTION ( 'NONE',  ( 6.938893903907209642E-16, -1.201851678989722492E-15, 1.000000000000000000 ) ) ;
#81647 = CARTESIAN_POINT ( 'NONE',  ( 208.0692320075777957, 270.2605140014760536, 2.043861372130216569 ) ) ;
#81648 = CARTESIAN_POINT ( 'NONE',  ( 129.8627877943888791, 245.7833772461660544, -9.188101187500095079 ) ) ;
#81649 = VERTEX_POINT ( 'NONE', #31946 ) ;
#81650 = CARTESIAN_POINT ( 'NONE',  ( 82.31194215350321031, 44.23274708058759330, -9.322014020231229381 ) ) ;
#81651 = CARTESIAN_POINT ( 'NONE',  ( 84.29722201641486379, 226.1427522451419065, 10.00000000000009415 ) ) ;
#81652 = CARTESIAN_POINT ( 'NONE',  ( 205.5208005306483017, 273.6775489442410390, -10.63251936667145081 ) ) ;
#81653 = CARTESIAN_POINT ( 'NONE',  ( 204.5831314780710954, 276.2986172388744421, 13.28075685133257089 ) ) ;
#81654 = CARTESIAN_POINT ( 'NONE',  ( 74.41657139711887226, 59.28711007250513632, 15.72167588865270105 ) ) ;
#81655 = DIRECTION ( 'NONE',  ( -1.000000000000000000, 0.000000000000000000, 0.000000000000000000 ) ) ;
#81656 = ORIENTED_EDGE ( 'NONE', *, *, #77673, .F. ) ;
#81657 = CARTESIAN_POINT ( 'NONE',  ( 77.57184175184252695, 61.56740756872861198, 15.71511318425823589 ) ) ;
#81658 = CARTESIAN_POINT ( 'NONE',  ( 167.5947507133649310, 249.2327294981003263, -5.855345954056704549 ) ) ;
#81659 = CARTESIAN_POINT ( 'NONE',  ( 147.6281730237836882, 275.3355110443876583, 3.207598580681599643 ) ) ;
#81660 = CARTESIAN_POINT ( 'NONE',  ( 206.7156906810202770, 272.6049163492177740, -10.59685249612386571 ) ) ;
#81661 = CARTESIAN_POINT ( 'NONE',  ( 166.2786698706664765, 279.3007919285489606, -14.16120680810289301 ) ) ;
#81662 = CARTESIAN_POINT ( 'NONE',  ( 196.0043407458614126, 263.5071561960751865, 0.8773891917627181236 ) ) ;
#81663 = B_SPLINE_CURVE_WITH_KNOTS ( 'NONE', 3,
 ( #46008, #14640, #30836, #8538, #85068, #24726, #76925, #7526, #61722, #38921, #31326, #38418, #69333, #22741, #55116, #39410, #39907, #62716, #45520, #69826, #62213, #15114, #1451, #23222, #54111, #99749, #61224, #437, #86103, #93165, #100254, #94175, #23715, #76451, #84089, #53620, #7028, #70325, #54610, #16629, #85593, #30334, #47032, #92188, #16134, #31815 ),
 .UNSPECIFIED., .F., .F.,
 ( 4, 2, 2, 2, 2, 2, 2, 2, 2, 2, 2, 2, 2, 2, 2, 2, 2, 2, 2, 2, 2, 2, 4 ),
 ( 0.001735191271250833937, 0.002191273913610610868, 0.002647356555970387798, 0.002875397877150307271, 0.002989418537740283922, 0.003103439198330260572, 0.003331480519510220811, 0.003559521840690181918, 0.004015604483050082447, 0.004471687125409982977, 0.005383852410129784036, 0.006296017694849584227, 0.006752100337209405827, 0.007208182979569228294, 0.007322203640159166346, 0.007379213970454106750, 0.007436224300749048888, 0.007550244961338901939, 0.007664265621928754990, 0.008120348264288413526, 0.008576430906648068592, 0.008804472227827903064, 0.009032513549007735801 ),
 .UNSPECIFIED. ) ;
#81664 = CARTESIAN_POINT ( 'NONE',  ( 182.4004271739244700, 284.1903799708203451, 16.39187655311515002 ) ) ;
#81665 = CARTESIAN_POINT ( 'NONE',  ( 70.02381739212118816, 70.89375414050529400, 2.247727738370168371 ) ) ;
#81666 = CARTESIAN_POINT ( 'NONE',  ( 204.7237927799493775, 276.0549847173622879, -12.81020997223575364 ) ) ;
#81667 = CARTESIAN_POINT ( 'NONE',  ( 174.5969907055684018, 251.7067686988808077, 3.596065318713836945 ) ) ;
#81668 = EDGE_CURVE ( 'NONE', #84261, #4682, #92791, .T. ) ;
#81669 = CARTESIAN_POINT ( 'NONE',  ( 23.90043047733868420, 15.92755873383626408, 6.180339887498953466 ) ) ;
#81670 = CARTESIAN_POINT ( 'NONE',  ( 190.2318383114841254, 301.1557861577188078, 3.177919994438449525 ) ) ;
#81671 = CARTESIAN_POINT ( 'NONE',  ( 168.8563211758018099, 286.0187424789903048, -9.056861680415359217 ) ) ;
#81672 = CARTESIAN_POINT ( 'NONE',  ( 155.4810912439522212, 261.3458456796594760, -18.44218279064527266 ) ) ;
#81673 = EDGE_CURVE ( 'NONE', #97425, #7077, #16755, .T. ) ;
#81674 = CARTESIAN_POINT ( 'NONE',  ( 193.2549072042652938, 289.0724932029194747, 16.12968917536251112 ) ) ;
#81675 = CARTESIAN_POINT ( 'NONE',  ( 131.0625938207745662, 253.1427522451419350, 10.00000000000009237 ) ) ;
#81676 = EDGE_CURVE ( 'NONE', #48903, #7154, #24366, .T. ) ;
#81677 = CARTESIAN_POINT ( 'NONE',  ( 182.0338464029501040, 278.3680066549227945, 17.69288446120480174 ) ) ;
#81678 = EDGE_LOOP ( 'NONE', ( #57904, #76719, #67370, #93008 ) ) ;
#81679 = EDGE_CURVE ( 'NONE', #73728, #56977, #60519, .T. ) ;
#81680 = CARTESIAN_POINT ( 'NONE',  ( 93.96857342517718337, 10.00000000000001243, -14.21260523776213347 ) ) ;
#81681 = CARTESIAN_POINT ( 'NONE',  ( 148.4049257185216106, 273.6021238924720365, 8.639190357831699529 ) ) ;
#81682 = CARTESIAN_POINT ( 'NONE',  ( 2.070087696330116689, 165.8768266524159856, -9.188101187500093303 ) ) ;
#81683 = CARTESIAN_POINT ( 'NONE',  ( 46.20988612576196175, 206.6744531367911009, 4.594050593750047540 ) ) ;
#81684 = CARTESIAN_POINT ( 'NONE',  ( 178.3284622040489182, 258.9725433493954938, -10.32068595145413070 ) ) ;
#81685 = CARTESIAN_POINT ( 'NONE',  ( 19.46394688279507079, 19.43677371833800649, -10.00000000000000355 ) ) ;
#81686 = CARTESIAN_POINT ( 'NONE',  ( 85.77117071415351290, 48.61266522586591776, 12.32040783412941920 ) ) ;
#81687 = CARTESIAN_POINT ( 'NONE',  ( 205.3943609285979051, 274.8935266139653777, -13.14270440534009943 ) ) ;
#81688 = CARTESIAN_POINT ( 'NONE',  ( 72.25715799891941060, 71.93417405212122162, -3.785998945288025830 ) ) ;
#81689 = CARTESIAN_POINT ( 'NONE',  ( 147.5813496936708020, 275.0285994114094592, 4.516581957185684004 ) ) ;
#81690 = CARTESIAN_POINT ( 'NONE',  ( 149.8523222352334585, 276.3723033856174993, 3.703967980727939757 ) ) ;
#81692 = CARTESIAN_POINT ( 'NONE',  ( 72.31720393073018727, 205.8927522451418213, 10.00000000000009592 ) ) ;
#81691 = CARTESIAN_POINT ( 'NONE',  ( 66.27852879613530490, 220.6199935810940644, 2.679491924311251605 ) ) ;
#81693 = CARTESIAN_POINT ( 'NONE',  ( 75.24745298538975646, 66.90968352439989530, 12.83700467311895999 ) ) ;
#81694 = DIRECTION ( 'NONE',  ( 0.03277852384265239616, -0.9994626398093610087, 0.000000000000000000 ) ) ;
#81695 = CARTESIAN_POINT ( 'NONE',  ( 198.0384979254556015, 287.6342550689238351, 17.28192639992792579 ) ) ;
#81696 = VECTOR ( 'NONE', #91347, 1000.000000000000000 ) ;
#81697 = CARTESIAN_POINT ( 'NONE',  ( 34.73530984921583098, 200.8615022471903160, 5.000000000000046185 ) ) ;
#81698 = CARTESIAN_POINT ( 'NONE',  ( 183.0123155676400017, 292.3663792116327045, 9.373780817324643522 ) ) ;
#81699 = CARTESIAN_POINT ( 'NONE',  ( 149.7247407264208618, 272.0633196944937140, -11.44969454563192279 ) ) ;
#81700 = CARTESIAN_POINT ( 'NONE',  ( 9.485603764116877556, 164.0327760586659451, 1.948934522072303157E-15 ) ) ;
#81701 = CARTESIAN_POINT ( 'NONE',  ( 167.8403557585028238, 287.0638538939059572, 5.056128628522604807 ) ) ;
#81702 = CARTESIAN_POINT ( 'NONE',  ( 79.33995266210858688, 59.84812545430209951, 16.15734818946814144 ) ) ;
#81703 = CARTESIAN_POINT ( 'NONE',  ( 38.58005528328081368, 27.98920272979929535, 7.433330006724137462 ) ) ;
#81704 = CARTESIAN_POINT ( 'NONE',  ( 82.43887584100872346, 211.7365022471901455, -10.00000000000009237 ) ) ;
#81705 = CIRCLE ( 'NONE', #21852, 12.50000000000000000 ) ;
#81706 = CARTESIAN_POINT ( 'NONE',  ( 164.4781197247689306, 245.7625352337404649, -1.511762618280499515 ) ) ;
#81707 = CARTESIAN_POINT ( 'NONE',  ( 154.9226727788713731, 262.3130548330639726, 18.22497199616848818 ) ) ;
#81708 = CARTESIAN_POINT ( 'NONE',  ( 148.7899746831494951, 275.3503135630597285, 7.551395034694676767 ) ) ;
#81709 = DIRECTION ( 'NONE',  ( -0.000000000000000000, -0.000000000000000000, 1.000000000000000000 ) ) ;
#81710 = DIRECTION ( 'NONE',  ( 1.000000000000000000, 0.000000000000000000, 0.000000000000000000 ) ) ;
#81711 = CARTESIAN_POINT ( 'NONE',  ( 21.04482852044473162, 14.01110640527291906, 2.839279412974134775 ) ) ;
#81712 = CARTESIAN_POINT ( 'NONE',  ( 71.88106639363310535, 72.58558382077730187, 1.103795272596830968 ) ) ;
#81713 = CARTESIAN_POINT ( 'NONE',  ( 204.1541407990405332, 272.6956988606675623, 11.22829397770025395 ) ) ;
#81714 = DIRECTION ( 'NONE',  ( -0.000000000000000000, -0.000000000000000000, -1.000000000000000000 ) ) ;
#81715 = CARTESIAN_POINT ( 'NONE',  ( 152.7451086342026372, 277.4192470735611664, -5.215848642440160887 ) ) ;
#81716 = ORIENTED_EDGE ( 'NONE', *, *, #67191, .F. ) ;
#81717 = CARTESIAN_POINT ( 'NONE',  ( 156.9269804116493674, 276.4015752635256717, 10.91086647732385906 ) ) ;
#81718 = CARTESIAN_POINT ( 'NONE',  ( 206.7408728089182546, 272.5612996242556960, -10.63134519248043475 ) ) ;
#81719 = ORIENTED_EDGE ( 'NONE', *, *, #52413, .T. ) ;
#81720 = CARTESIAN_POINT ( 'NONE',  ( 192.6773196027083372, 296.9200883123592689, 11.15745042875121484 ) ) ;
#81721 = CARTESIAN_POINT ( 'NONE',  ( 68.30695491555283638, 70.04613929395418381, -0.05533233183379759196 ) ) ;
#81722 = CARTESIAN_POINT ( 'NONE',  ( 66.37497810201837467, 68.61734744729311331, 4.837691964654595722 ) ) ;
#81723 = CARTESIAN_POINT ( 'NONE',  ( 87.22363864817131685, 45.41812704280852131, 7.117319539031738529 ) ) ;
#81724 = VERTEX_POINT ( 'NONE', #33985 ) ;
#81725 = ORIENTED_EDGE ( 'NONE', *, *, #79664, .F. ) ;
#81727 = CARTESIAN_POINT ( 'NONE',  ( 204.5730103890532519, 276.3161474792809145, 14.88139715235883109 ) ) ;
#81726 = CARTESIAN_POINT ( 'NONE',  ( 159.7739451486069129, 278.5727107813384578, -9.701063066010021885 ) ) ;
#81728 = CARTESIAN_POINT ( 'NONE',  ( 192.6797324865049745, 296.9159090750308110, 12.42053959885222625 ) ) ;
#81729 = ORIENTED_EDGE ( 'NONE', *, *, #94905, .F. ) ;
#81730 = CARTESIAN_POINT ( 'NONE',  ( 80.73437012277888414, 57.38180594535328538, 16.57560423861647791 ) ) ;
#81731 = CARTESIAN_POINT ( 'NONE',  ( 176.1222898868072377, 263.1452895647582295, 14.39881833071060591 ) ) ;
#81732 = ORIENTED_EDGE ( 'NONE', *, *, #11590, .T. ) ;
#81733 = CARTESIAN_POINT ( 'NONE',  ( 87.64894182299636327, 45.42967476813434757, -6.652927784817597612 ) ) ;
#81734 = CARTESIAN_POINT ( 'NONE',  ( 77.58272377184611912, 50.60896635146917077, -15.24740917957588060 ) ) ;
#81735 = B_SPLINE_CURVE_WITH_KNOTS ( 'NONE', 3,
 ( #50321, #72663, #73636, #35118, #80277, #58412, #57416, #10842 ),
 .UNSPECIFIED., .F., .F.,
 ( 4, 2, 2, 4 ),
 ( 0.000000000000000000, 0.2371517132195850586, 0.3557275698293775879, 0.4743034264391701171 ),
 .UNSPECIFIED. ) ;
#81736 = EDGE_CURVE ( 'NONE', #63400, #32826, #88220, .T. ) ;
#81737 = CARTESIAN_POINT ( 'NONE',  ( 80.64280233791232888, 43.43830871627009316, 9.478028014899054554 ) ) ;
#81738 = AXIS2_PLACEMENT_3D ( 'NONE', #90828, #6675, #61849 ) ;
#81739 = ORIENTED_EDGE ( 'NONE', *, *, #59213, .T. ) ;
#81740 = CARTESIAN_POINT ( 'NONE',  ( 203.0389248067080814, 268.2143839803633227, 2.500499824216583011 ) ) ;
#81741 = CARTESIAN_POINT ( 'NONE',  ( 164.9103019330012216, 245.0139736909548560, 2.841678961959298810 ) ) ;
#81742 = CYLINDRICAL_SURFACE ( 'NONE', #15392, 70.00000000000002842 ) ;
#81743 = EDGE_LOOP ( 'NONE', ( #42523, #31067, #87415, #57959 ) ) ;
#81744 = CARTESIAN_POINT ( 'NONE',  ( 148.9498507103374152, 272.6582861203333437, 11.90061892622094852 ) ) ;
#81745 = CARTESIAN_POINT ( 'NONE',  ( 168.9465774574146053, 261.3817357245186486, -16.22414195487736777 ) ) ;
#81746 = ORIENTED_EDGE ( 'NONE', *, *, #82570, .T. ) ;
#81747 = CARTESIAN_POINT ( 'NONE',  ( 156.8020845273852615, 266.4781374791638768, -16.27585026529224521 ) ) ;
#81748 = ORIENTED_EDGE ( 'NONE', *, *, #86935, .T. ) ;
#81749 = CARTESIAN_POINT ( 'NONE',  ( -19.65312891409030271, 93.06504152958497400, 177.5919119679930134 ) ) ;
#81750 = ORIENTED_EDGE ( 'NONE', *, *, #74547, .F. ) ;
#81751 = CARTESIAN_POINT ( 'NONE',  ( 48.98810889288134263, 89.24608170897542436, 10.00000000000000000 ) ) ;
#81752 = CARTESIAN_POINT ( 'NONE',  ( 87.14941533941508567, 43.54552546780055877, 0.3078308432578384934 ) ) ;
#81753 = FACE_OUTER_BOUND ( 'NONE', #54483, .T. ) ;
#81754 = FACE_OUTER_BOUND ( 'NONE', #78489, .T. ) ;
#81755 = DIRECTION ( 'NONE',  ( -0.8660254037844387076, -0.4999999999999998890, -0.000000000000000000 ) ) ;
#81756 = CARTESIAN_POINT ( 'NONE',  ( 153.3100492430090753, 265.1062007306585997, 16.32434963471121492 ) ) ;
#81757 = CARTESIAN_POINT ( 'NONE',  ( 34.30229714732364954, 190.6115022471902591, 10.00000000000009592 ) ) ;
#81758 = CARTESIAN_POINT ( 'NONE',  ( 197.5317255130193246, 288.5120106351379832, -18.16135075925290465 ) ) ;
#81759 = VERTEX_POINT ( 'NONE', #73969 ) ;
#81760 = LINE ( 'NONE', #43198, #82037 ) ;
#81761 = CARTESIAN_POINT ( 'NONE',  ( 206.5280879940269756, 272.9298537347264642, 11.21709153681466731 ) ) ;
#81763 = CARTESIAN_POINT ( 'NONE',  ( 164.4261001824251878, 245.8526357240660900, 1.583002802772015549 ) ) ;
#81762 = CARTESIAN_POINT ( 'NONE',  ( 149.3253462891332219, 272.0079086998416074, -12.99539319630191336 ) ) ;
#81765 = ORIENTED_EDGE ( 'NONE', *, *, #80431, .F. ) ;
#81764 = CYLINDRICAL_SURFACE ( 'NONE', #80114, 10.00000000000010658 ) ;
#81766 = ORIENTED_EDGE ( 'NONE', *, *, #99221, .T. ) ;
#81767 = CARTESIAN_POINT ( 'NONE',  ( 184.5921257832661126, 275.4691417599202055, 16.38528715067328179 ) ) ;
#81768 = CARTESIAN_POINT ( 'NONE',  ( 82.29245928123272336, 51.99578426057395575, -14.89862599341149263 ) ) ;
#81769 = CARTESIAN_POINT ( 'NONE',  ( -71.61465314115659453, 63.06504152958490295, -10.00000000000000888 ) ) ;
#81770 = LINE ( 'NONE', #35125, #11757 ) ;
#81771 = CIRCLE ( 'NONE', #89870, 70.00000000000001421 ) ;
#81772 = B_SPLINE_CURVE_WITH_KNOTS ( 'NONE', 3,
 ( #90859, #44681, #53294, #6202, #90355, #75126, #68000, #21411, #22399, #37582, #59378, #68491, #29503, #52294, #60378, #20935, #5702, #84247, #36592, #91336, #99417, #29994, #20426, #43190 ),
 .UNSPECIFIED., .F., .F.,
 ( 4, 2, 2, 2, 2, 2, 2, 2, 2, 2, 2, 4 ),
 ( 0.000000000000000000, 0.1249999999999881206, 0.2499999999999762412, 0.3749999999999643618, 0.4374999999999651390, 0.4999999999999659162, 0.5624999999999665823, 0.6249999999999673594, 0.6874999999999680256, 0.7499999999999688027, 0.8749999999999843459, 1.000000000000000000 ),
 .UNSPECIFIED. ) ;
#81773 = CARTESIAN_POINT ( 'NONE',  ( 160.2441359297705219, 253.0960102851007605, -14.63485326429217537 ) ) ;
#81774 = CARTESIAN_POINT ( 'NONE',  ( 148.3276789103558997, 273.7359192889379074, -8.831907802783907968 ) ) ;
#81775 = ORIENTED_EDGE ( 'NONE', *, *, #28208, .T. ) ;
#81776 = CARTESIAN_POINT ( 'NONE',  ( 170.5504771200006076, 255.5552483777219095, -11.63320334257268840 ) ) ;
#81777 = CARTESIAN_POINT ( 'NONE',  ( 205.7578342874187740, 273.6337450154945827, 10.12066660866375400 ) ) ;
#81778 = CARTESIAN_POINT ( 'NONE',  ( 82.39721099668476256, 40.42262220707492304, 1.474573639734339192 ) ) ;
#81779 = CARTESIAN_POINT ( 'NONE',  ( 165.0387478276132072, 244.7914988754632191, -2.473354058663827626 ) ) ;
#81780 = CARTESIAN_POINT ( 'NONE',  ( 34.13991738056614622, 190.5177522451418497, -10.00000000000009592 ) ) ;
#81781 = CARTESIAN_POINT ( 'NONE',  ( 95.92524373570365981, 232.3149278399160949, -9.188101187500095079 ) ) ;
#81782 =( GEOMETRIC_REPRESENTATION_CONTEXT ( 3 ) GLOBAL_UNCERTAINTY_ASSIGNED_CONTEXT ( ( #95000 ) ) GLOBAL_UNIT_ASSIGNED_CONTEXT ( ( #76207, #84324, #61468 ) ) REPRESENTATION_CONTEXT ( 'NONE', 'WORKASPACE' ) );
#81783 = PLANE ( 'NONE',  #85088 ) ;
#81784 = CARTESIAN_POINT ( 'NONE',  ( 162.8265537361057795, 249.1312387917435558, -10.34784883127201915 ) ) ;
#81785 = CARTESIAN_POINT ( 'NONE',  ( 84.21326495356250064, 50.60090342464640401, 13.78724288159853728 ) ) ;
#81786 = DIRECTION ( 'NONE',  ( 1.000000000000000000, 0.000000000000000000, 0.000000000000000000 ) ) ;
#81787 = CARTESIAN_POINT ( 'NONE',  ( 30.64892602121659593, 182.3768266524159856, -9.188101187500091527 ) ) ;
#81788 = CARTESIAN_POINT ( 'NONE',  ( 204.6350011963004647, 275.7068757420208271, -12.64342396695018245 ) ) ;
#81789 = EDGE_LOOP ( 'NONE', ( #1871, #45587, #15923, #78589 ) ) ;
#81790 = VERTEX_POINT ( 'NONE', #64870 ) ;
#81791 = LINE ( 'NONE', #63682, #81885 ) ;
#81792 = CARTESIAN_POINT ( 'NONE',  ( 74.31200754921134433, 68.46947570921950899, -11.18681609572362134 ) ) ;
#81793 = EDGE_CURVE ( 'NONE', #49527, #71581, #4553, .T. ) ;
#81794 = CARTESIAN_POINT ( 'NONE',  ( 74.27061467689566143, 65.15629350404239517, 13.99533241632264158 ) ) ;
#81795 = CARTESIAN_POINT ( 'NONE',  ( -11.70629829599211646, 23.25616956148705938, -10.00000000000000000 ) ) ;
#81796 = CARTESIAN_POINT ( 'NONE',  ( 161.7412967960748915, 250.5028515975580774, -14.36228887024421041 ) ) ;
#81797 = EDGE_CURVE ( 'NONE', #61780, #37352, #33466, .T. ) ;
#81798 = CARTESIAN_POINT ( 'NONE',  ( 68.65239601531978053, 64.10048622081454539, 11.94980523598330358 ) ) ;
#81799 = CARTESIAN_POINT ( 'NONE',  ( -62.95439910331221256, 68.06504152958493137, 25.00000000000000000 ) ) ;
#81800 = CARTESIAN_POINT ( 'NONE',  ( 47.23881193640350062, 188.8923013555410080, 4.594050593750050204 ) ) ;
#81801 = CARTESIAN_POINT ( 'NONE',  ( 93.10181362155671536, 217.8927522451418213, 10.00000000000009592 ) ) ;
#81802 = ORIENTED_EDGE ( 'NONE', *, *, #58549, .T. ) ;
#81803 = CARTESIAN_POINT ( 'NONE',  ( 197.3520635096637648, 267.5934713644667795, -7.874698761606322428 ) ) ;
#81804 = EDGE_CURVE ( 'NONE', #38056, #74380, #11289, .T. ) ;
#81805 = DIRECTION ( 'NONE',  ( -0.000000000000000000, 0.000000000000000000, -1.000000000000000000 ) ) ;
#81806 = CARTESIAN_POINT ( 'NONE',  ( 23.64814127513154673, 118.0650415295851019, -20.00000000000000355 ) ) ;
#81807 = VECTOR ( 'NONE', #34635, 1000.000000000000227 ) ;
#81808 = CARTESIAN_POINT ( 'NONE',  ( 2.557053438076354990, 172.2833772461660828, -9.188101187500095079 ) ) ;
#81809 = CARTESIAN_POINT ( 'NONE',  ( 150.9003228897357189, 269.2799692068659283, -14.30003212299500781 ) ) ;
#81810 = DIRECTION ( 'NONE',  ( 0.000000000000000000, 0.000000000000000000, 1.000000000000000000 ) ) ;
#81811 = CARTESIAN_POINT ( 'NONE',  ( 192.6679047218190135, 296.9363953644068488, -13.34486378385621386 ) ) ;
#81812 = CARTESIAN_POINT ( 'NONE',  ( 73.57209063514699210, 69.79607308722023618, 9.344099467940562675 ) ) ;
#81813 = CARTESIAN_POINT ( 'NONE',  ( 58.06412948370898164, 195.1423013555410080, -4.594050593750043987 ) ) ;
#81814 = CARTESIAN_POINT ( 'NONE',  ( 208.2777459429579210, 269.8993572713111462, 3.129643751043610589 ) ) ;
#81815 = CARTESIAN_POINT ( 'NONE',  ( 203.7776468208327003, 276.2971780117193248, 13.33764639693685616 ) ) ;
#81816 = CARTESIAN_POINT ( 'NONE',  ( 71.19846455806460028, 71.21114677313781272, 4.076820472404566686 ) ) ;
#81817 = CARTESIAN_POINT ( 'NONE',  ( 147.6140518775699491, 274.9719575673779559, 8.457032797753797126 ) ) ;
#81818 = ORIENTED_EDGE ( 'NONE', *, *, #23403, .T. ) ;
#81819 = AXIS2_PLACEMENT_3D ( 'NONE', #85628, #17681, #32372 ) ;
#81820 = CARTESIAN_POINT ( 'NONE',  ( -0.6995629222974718564, 183.7365022471903444, 2.944929066748280225E-16 ) ) ;
#81821 = CARTESIAN_POINT ( 'NONE',  ( 83.11015170815555564, 43.06723244532030748, 7.901789092622347965 ) ) ;
#81822 = CARTESIAN_POINT ( 'NONE',  ( 124.1521724663614492, 251.6744531367911577, 4.594050593750047540 ) ) ;
#81823 = CARTESIAN_POINT ( 'NONE',  ( 31.76189289227714951, 20.19860640527293683, 2.839279412974134775 ) ) ;
#81824 = CARTESIAN_POINT ( 'NONE',  ( 206.9146873713863783, 272.2602439709654618, -8.162908012510746047 ) ) ;
#81825 = CARTESIAN_POINT ( 'NONE',  ( 150.9988863956583600, 269.5412616643368438, 13.78873124909360293 ) ) ;
#81827 = CARTESIAN_POINT ( 'NONE',  ( 75.29548954665729354, 66.77148020061324019, 13.38688763123640690 ) ) ;
#81826 = LINE ( 'NONE', #51374, #63019 ) ;
#81828 = CARTESIAN_POINT ( 'NONE',  ( 190.6426292480107350, 300.4442753843661080, -6.777079808125155758 ) ) ;
#81829 = ORIENTED_EDGE ( 'NONE', *, *, #63047, .T. ) ;
#81830 = CARTESIAN_POINT ( 'NONE',  ( 191.3638605175971747, 299.1950661814348678, 7.382965314423603154 ) ) ;
#81831 = CARTESIAN_POINT ( 'NONE',  ( 208.2584889301005546, 269.9327113959824374, -1.669397994094046211 ) ) ;
#81832 = CARTESIAN_POINT ( 'NONE',  ( 185.2961235551778714, 291.2460235572835927, 13.48139818756336616 ) ) ;
#81833 = CARTESIAN_POINT ( 'NONE',  ( 170.4818684897218759, 266.4664816474689246, -17.63139018167740701 ) ) ;
#81834 = CARTESIAN_POINT ( 'NONE',  ( 81.59199138121388728, 55.54565483415311888, -16.32615847003737741 ) ) ;
#81835 = EDGE_LOOP ( 'NONE', ( #17912, #22970, #38051, #92205 ) ) ;
#81836 = CARTESIAN_POINT ( 'NONE',  ( 71.92247502996752928, 71.58450950858453155, 4.220300433249585481 ) ) ;
#81837 = CARTESIAN_POINT ( 'NONE',  ( 49.83874514172082826, 101.4840343560034057, 177.5919119679930134 ) ) ;
#81838 = VECTOR ( 'NONE', #57009, 999.9999999999998863 ) ;
#81839 = CARTESIAN_POINT ( 'NONE',  ( 83.62813027309111646, 42.52490326476596039, 5.061828679325668823 ) ) ;
#81840 = CARTESIAN_POINT ( 'NONE',  ( 79.81418777460577019, 52.70850083650530848, 15.50782481748570341 ) ) ;
#81841 = AXIS2_PLACEMENT_3D ( 'NONE', #27658, #66142, #73749 ) ;
#81842 = CARTESIAN_POINT ( 'NONE',  ( 184.5043411789232266, 295.9227417631768731, 4.662132045941501879 ) ) ;
#81843 = CARTESIAN_POINT ( 'NONE',  ( 69.97041834188608789, 71.02470767604341972, 1.098024261663877565 ) ) ;
#81844 = CARTESIAN_POINT ( 'NONE',  ( 19.18375657693640335, 36.32959363016014720, -10.00000000000000000 ) ) ;
#81845 = VERTEX_POINT ( 'NONE', #89708 ) ;
#81846 = CARTESIAN_POINT ( 'NONE',  ( 193.8615474287298355, 282.6207621793728322, 17.07927997190257940 ) ) ;
#81847 = CARTESIAN_POINT ( 'NONE',  ( 2.161320418471442739, 24.18080186712590418, 3.090169943749475401 ) ) ;
#81848 = CARTESIAN_POINT ( 'NONE',  ( 191.9828369562736441, 287.6126897466953665, -16.13172383425306933 ) ) ;
#81849 = ORIENTED_EDGE ( 'NONE', *, *, #75290, .F. ) ;
#81850 = CARTESIAN_POINT ( 'NONE',  ( -19.65312891409030271, 93.06504152958497400, 10.00000000000000888 ) ) ;
#81851 = CARTESIAN_POINT ( 'NONE',  ( 194.7576540903134799, 293.3168432830895540, -14.62421624641040196 ) ) ;
#81852 = ORIENTED_EDGE ( 'NONE', *, *, #43882, .T. ) ;
#81853 = CARTESIAN_POINT ( 'NONE',  ( 79.15253416805734332, 60.03979343371569399, 16.13189369385897720 ) ) ;
#81854 = CARTESIAN_POINT ( 'NONE',  ( 185.4551394198477681, 291.0484231367762504, 12.14165578421975233 ) ) ;
#81855 = CARTESIAN_POINT ( 'NONE',  ( 204.9780665305064531, 275.6145696623662502, 14.10615427165218883 ) ) ;
#81856 = EDGE_CURVE ( 'NONE', #63287, #70064, #16646, .T. ) ;
#81857 = DIRECTION ( 'NONE',  ( 0.000000000000000000, 0.000000000000000000, 1.000000000000000000 ) ) ;
#81858 = EDGE_LOOP ( 'NONE', ( #42305, #79558, #60586, #80617, #88261 ) ) ;
#81859 = CARTESIAN_POINT ( 'NONE',  ( 86.20995510670323370, 211.3923013555409796, 4.594050593750050204 ) ) ;
#81860 = CARTESIAN_POINT ( 'NONE',  ( 202.8905955564125065, 279.2301754488222514, 15.56958316349127358 ) ) ;
#81861 = CARTESIAN_POINT ( 'NONE',  ( 189.4199209167946663, 300.3895034224956930, 3.306026617473488027 ) ) ;
#81862 = CARTESIAN_POINT ( 'NONE',  ( 81.50142252913457241, 41.92047369999142603, -7.540709297637336661 ) ) ;
#81863 = VERTEX_POINT ( 'NONE', #21261 ) ;
#81864 = ORIENTED_EDGE ( 'NONE', *, *, #16727, .T. ) ;
#81865 = CARTESIAN_POINT ( 'NONE',  ( 88.44311045277898131, 43.83777140359737956, 0.09123111681703664766 ) ) ;
#81866 = ORIENTED_EDGE ( 'NONE', *, *, #29720, .F. ) ;
#81867 = CARTESIAN_POINT ( 'NONE',  ( 192.7041411452173918, 293.9924959157295916, 14.27507663239260971 ) ) ;
#81869 = EDGE_CURVE ( 'NONE', #21409, #87939, #43184, .T. ) ;
#81868 = ORIENTED_EDGE ( 'NONE', *, *, #6057, .T. ) ;
#81870 = CARTESIAN_POINT ( 'NONE',  ( 75.99000472157059960, 63.81542519772441580, 14.67834632195794775 ) ) ;
#81871 = CARTESIAN_POINT ( 'NONE',  ( 155.4495868485232108, 261.4004128932040203, -18.48326470492642315 ) ) ;
#81872 = ORIENTED_EDGE ( 'NONE', *, *, #30226, .F. ) ;
#81873 = CARTESIAN_POINT ( 'NONE',  ( 165.0633574835339346, 244.7488737010519628, 1.949578632198007977 ) ) ;
#81874 = CARTESIAN_POINT ( 'NONE',  ( 82.15600053271296588, 41.14106544737295224, 3.251814095246992498 ) ) ;
#81875 = CARTESIAN_POINT ( 'NONE',  ( 147.1692232402260174, 275.7424233679190593, -6.897157937245698811 ) ) ;
#81877 = EDGE_CURVE ( 'NONE', #96813, #99018, #44452, .T. ) ;
#81876 = CARTESIAN_POINT ( 'NONE',  ( 45.11483101423407049, 69.99284853207299761, -10.00000000000000000 ) ) ;
#81878 = CARTESIAN_POINT ( 'NONE',  ( 170.2835531134608686, 278.8928912914798275, -15.69417418368842654 ) ) ;
#81879 = CARTESIAN_POINT ( 'NONE',  ( 32.30839531297598910, 123.0650415295850593, 25.00000000000000000 ) ) ;
#81880 = CARTESIAN_POINT ( 'NONE',  ( 147.1836429658426084, 243.5327760586659451, 1.948934522072303157E-15 ) ) ;
#81881 = CARTESIAN_POINT ( 'NONE',  ( 164.9790521326853536, 265.2878599192118827, -16.61474165352627352 ) ) ;
#81882 = CARTESIAN_POINT ( 'NONE',  ( 77.17961428966242465, 62.94638840390226164, 15.26134952368941633 ) ) ;
#81883 = CARTESIAN_POINT ( 'NONE',  ( 16.02188117849498639, 11.11110640527290983, -2.839279412974138328 ) ) ;
#81884 = ORIENTED_EDGE ( 'NONE', *, *, #19895, .F. ) ;
#81885 = VECTOR ( 'NONE', #17584, 1000.000000000000341 ) ;
#81886 = CARTESIAN_POINT ( 'NONE',  ( 167.3703416170141338, 284.2892190735486224, 9.299199617839436272 ) ) ;
#81888 = EDGE_LOOP ( 'NONE', ( #41299, #90194, #29873, #54535 ) ) ;
#81887 = CARTESIAN_POINT ( 'NONE',  ( 201.8432742760849123, 271.0906551529850503, 9.350329334099363621 ) ) ;
#81889 = DIRECTION ( 'NONE',  ( -0.000000000000000000, -0.000000000000000000, -1.000000000000000000 ) ) ;
#81890 = CARTESIAN_POINT ( 'NONE',  ( 78.55537653917157570, 48.00561504237174404, -13.97647359956260082 ) ) ;
#81891 = CARTESIAN_POINT ( 'NONE',  ( 76.28161175289729101, 64.99341775040052482, -14.27466362150210522 ) ) ;
#81892 = CARTESIAN_POINT ( 'NONE',  ( 153.3922461054063433, 276.8823880860896338, 7.152063237113233996 ) ) ;
#81893 = CARTESIAN_POINT ( 'NONE',  ( 81.64977529549180701, 50.14798347333574213, -14.69385758784257767 ) ) ;
#81894 =( BOUNDED_CURVE ( )  B_SPLINE_CURVE ( 2, ( #99730, #92651, #30317, #61204, #100235, #84558, #61699, #15097, #15595 ),
 .UNSPECIFIED., .F., .T. ) 
 B_SPLINE_CURVE_WITH_KNOTS ( ( 3, 2, 2, 2, 3 ),
 ( 0.02016129032258064807, 0.02150537634408602322, 0.02419354838709677352, 0.02688172043010752729, 0.02822580645161290591 ),
 .UNSPECIFIED. ) 
 CURVE ( )  GEOMETRIC_REPRESENTATION_ITEM ( )  RATIONAL_B_SPLINE_CURVE ( ( 0.9330127018922192983, 0.9330127018922194093, 1.000000000000000000, 0.8660254037844387076, 1.000000000000000000, 0.8660254037844387076, 1.000000000000000000, 0.9330127018922191873, 0.9330127018922192983 ) ) 
 REPRESENTATION_ITEM ( '' )  );
#81895 = AXIS2_PLACEMENT_3D ( 'NONE', #20173, #35853, #4970 ) ;
#81896 = FACE_OUTER_BOUND ( 'NONE', #8849, .T. ) ;
#81897 = CARTESIAN_POINT ( 'NONE',  ( 84.39300954678499522, 42.06444689919337776, 1.116208777756559023 ) ) ;
#81898 = CARTESIAN_POINT ( 'NONE',  ( 88.36930832042526163, 44.08004549128393990, -2.853748190838125254 ) ) ;
#81899 = ORIENTED_EDGE ( 'NONE', *, *, #57951, .F. ) ;
#81900 = CARTESIAN_POINT ( 'NONE',  ( 185.0763070350663781, 273.0824188773292462, -16.90268598921084120 ) ) ;
#81901 = CARTESIAN_POINT ( 'NONE',  ( 66.21124237162977977, 69.35328529186524804, 0.1844046320002812600 ) ) ;
#81902 = VERTEX_POINT ( 'NONE', #16145 ) ;
#81903 = CARTESIAN_POINT ( 'NONE',  ( 160.1979016687359092, 276.4615463954939401, 12.73367540184897351 ) ) ;
#81904 = CARTESIAN_POINT ( 'NONE',  ( 156.5654777510188183, 277.0389622341601807, 9.949659676293464372 ) ) ;
#81905 = CARTESIAN_POINT ( 'NONE',  ( 190.1758200331204876, 279.2204749713225169, -17.78067544974210890 ) ) ;
#81906 = CARTESIAN_POINT ( 'NONE',  ( 81.38310835580871583, 44.82813863409449340, -10.54473920995311786 ) ) ;
#81907 = CARTESIAN_POINT ( 'NONE',  ( 160.8137364596917109, 272.7584256728402465, 15.66121798818901567 ) ) ;
#81909 = CARTESIAN_POINT ( 'NONE',  ( 88.48648755238653507, 43.99326657310298572, 1.937087981213218457 ) ) ;
#81908 = CARTESIAN_POINT ( 'NONE',  ( -20.01016364259690405, 23.06595206263087050, 10.00000000000000000 ) ) ;
#81910 = CARTESIAN_POINT ( 'NONE',  ( 200.1347818429666177, 267.8741717063466581, 6.125758183920250843 ) ) ;
#81911 = VERTEX_POINT ( 'NONE', #9048 ) ;
#81912 = CIRCLE ( 'NONE', #17138, 45.00000000000000000 ) ;
#81913 = ORIENTED_EDGE ( 'NONE', *, *, #67764, .T. ) ;
#81914 = ADVANCED_FACE ( 'NONE', ( #84587 ), #61732, .F. ) ;
#81915 = CARTESIAN_POINT ( 'NONE',  ( -16.99542894172669349, 24.36904009834038476, 10.00000000000000000 ) ) ;
#81916 = CARTESIAN_POINT ( 'NONE',  ( 125.7401460302306759, 236.7365022471902307, 10.00000000000009948 ) ) ;
#81917 = ADVANCED_FACE ( 'NONE', ( #63245 ), #6428, .F. ) ;
#81918 = CARTESIAN_POINT ( 'NONE',  ( 86.81641918289878390, 45.77657501471897206, -8.750901752256124766 ) ) ;
#81919 = CARTESIAN_POINT ( 'NONE',  ( 171.9101151227116020, 289.4071025166348932, 2.638113784258313554 ) ) ;
#81920 = PLANE ( 'NONE',  #6498 ) ;
#81921 = CARTESIAN_POINT ( 'NONE',  ( 80.70489193592369759, 43.22441507702991004, -9.179128504869353833 ) ) ;
#81922 = CARTESIAN_POINT ( 'NONE',  ( 66.30954113569532637, 68.28728378170326607, 3.992301261007330737 ) ) ;
#81923 = CARTESIAN_POINT ( 'NONE',  ( 4.614210867829411811, 161.2202760586659451, -5.415160957724236172E-17 ) ) ;
#81924 = CARTESIAN_POINT ( 'NONE',  ( 98.52331994705694740, 233.8149278399160949, -9.188101187500095079 ) ) ;
#81925 = DIRECTION ( 'NONE',  ( -0.000000000000000000, 1.000000000000000000, -0.000000000000000000 ) ) ;
#81926 = CARTESIAN_POINT ( 'NONE',  ( 179.9282632979647474, 254.9894960794134136, -2.420314024967571864 ) ) ;
#81927 = CARTESIAN_POINT ( 'NONE',  ( 78.24153046963442648, 52.40082309350520973, 15.62826166183230114 ) ) ;
#81928 = EDGE_CURVE ( 'NONE', #57417, #41328, #76803, .T. ) ;
#81929 = DIRECTION ( 'NONE',  ( -0.8660254037844379305, -0.5000000000000014433, -0.000000000000000000 ) ) ;
#81930 = CARTESIAN_POINT ( 'NONE',  ( 167.6146168596400514, 252.8497314824998909, -12.44459218179994231 ) ) ;
#81931 = CARTESIAN_POINT ( 'NONE',  ( 194.1852025340051284, 294.3083584634874796, -15.46421316575964688 ) ) ;
#81932 = CARTESIAN_POINT ( 'NONE',  ( 84.41999685182091184, 50.11946239824889915, 13.85565564441014708 ) ) ;
#81933 = CARTESIAN_POINT ( 'NONE',  ( 74.56414817410227158, 187.8759306620403322, 17.47570218321536473 ) ) ;
#81934 = CARTESIAN_POINT ( 'NONE',  ( 182.0171333322937528, 267.6076494233564063, -14.80649776740987278 ) ) ;
#81935 = CARTESIAN_POINT ( 'NONE',  ( 172.5499481646635331, 263.5659312731885962, -15.40879909798235836 ) ) ;
#81936 = CARTESIAN_POINT ( 'NONE',  ( 83.09741599002914825, 218.7833772461660544, -9.188101187500095079 ) ) ;
#81937 = CARTESIAN_POINT ( 'NONE',  ( 5.721601707324312613, 18.70171378149916563, -9.188101187500004485 ) ) ;
#81938 = CARTESIAN_POINT ( 'NONE',  ( 191.4685399627163633, 299.0137560639802814, 7.545791216288330716 ) ) ;
#81939 = CARTESIAN_POINT ( 'NONE',  ( -14.12104474639061458, 103.3883419700267865, 11.22454184241338027 ) ) ;
#81941 = CARTESIAN_POINT ( 'NONE',  ( 86.26068559980312500, 43.08597108666732112, -0.9339882263466466883 ) ) ;
#81940 = CARTESIAN_POINT ( 'NONE',  ( 157.6335212189247557, 257.6177276032722716, 16.76495363836117036 ) ) ;
#81942 = CARTESIAN_POINT ( 'NONE',  ( 149.1585757751420829, 272.2967637032783728, 11.60936825230297842 ) ) ;
#81943 = CARTESIAN_POINT ( 'NONE',  ( 151.3681950933278983, 268.4695907787949523, -15.50699599486383917 ) ) ;
#81944 = CARTESIAN_POINT ( 'NONE',  ( 204.1506106421540494, 276.0852532772063341, -13.43628313753478487 ) ) ;
#81945 = VECTOR ( 'NONE', #25155, 1000.000000000000114 ) ;
#81946 = CARTESIAN_POINT ( 'NONE',  ( 38.14222467998226307, 24.94754757982092386, 5.678558825948272215 ) ) ;
#81947 = CARTESIAN_POINT ( 'NONE',  ( 147.5851099763508216, 275.0220864107570264, -4.372720440640867956 ) ) ;
#81948 = CARTESIAN_POINT ( 'NONE',  ( 86.02630325614639162, 46.55013779904520987, -9.649467063894148211 ) ) ;
#81949 = EDGE_LOOP ( 'NONE', ( #52630, #47174, #89164, #29488, #35825, #21895, #49806, #9934 ) ) ;
#81950 = CARTESIAN_POINT ( 'NONE',  ( 17.68238808236222326, 31.18502408145591787, 5.678558825948277544 ) ) ;
#81951 = CARTESIAN_POINT ( 'NONE',  ( 181.8509774751104544, 266.9677320091309412, 16.09658033613713712 ) ) ;
#81952 = AXIS2_PLACEMENT_3D ( 'NONE', #84987, #6469, #46432 ) ;
#81953 = CARTESIAN_POINT ( 'NONE',  ( 192.4335622838504207, 297.3422883733380786, -12.83044365323471325 ) ) ;
#81954 = CARTESIAN_POINT ( 'NONE',  ( 65.04619898167126735, 198.3615022471901739, 5.000000000000051514 ) ) ;
#81955 = ORIENTED_EDGE ( 'NONE', *, *, #37382, .T. ) ;
#81956 = VECTOR ( 'NONE', #52435, 1000.000000000000000 ) ;
#81957 = CARTESIAN_POINT ( 'NONE',  ( 70.95735205513742017, 61.13278218173532963, 15.00632081318293132 ) ) ;
#81958 = CARTESIAN_POINT ( 'NONE',  ( 67.24138620688670187, 66.48174940271749733, -8.670771479132932669 ) ) ;
#81959 = CARTESIAN_POINT ( 'NONE',  ( 193.8003511027313550, 288.1208047801705447, 17.19107869180001913 ) ) ;
#81960 = CARTESIAN_POINT ( 'NONE',  ( 182.7847760313759409, 280.0284915794045446, -17.53211380394024843 ) ) ;
#81961 = CARTESIAN_POINT ( 'NONE',  ( 133.0291931787496367, 257.6115022471902876, -5.000000000000047962 ) ) ;
#81962 = CARTESIAN_POINT ( 'NONE',  ( 204.6713671561005299, 276.1457885614869951, -12.94307097876490431 ) ) ;
#81963 = CARTESIAN_POINT ( 'NONE',  ( 75.47623563632357957, 53.31721590068422501, 16.49647974421704433 ) ) ;
#81964 = ORIENTED_EDGE ( 'NONE', *, *, #44894, .F. ) ;
#81965 = CARTESIAN_POINT ( 'NONE',  ( 190.8228695072887149, 299.3521595973184617, -6.560059525124882995 ) ) ;
#81966 = CARTESIAN_POINT ( 'NONE',  ( 169.4432399169915016, 248.6629731721966436, -1.917647540753971480 ) ) ;
#81967 = ORIENTED_EDGE ( 'NONE', *, *, #62181, .F. ) ;
#81968 = CARTESIAN_POINT ( 'NONE',  ( 196.5171250811640675, 264.4500657306584230, -4.685409136380966899 ) ) ;
#81969 = CARTESIAN_POINT ( 'NONE',  ( 85.69585619780065144, 43.36699593673009190, 4.244564163715101479 ) ) ;
#81970 = EDGE_LOOP ( 'NONE', ( #66437, #89995, #824, #62615 ) ) ;
#81971 = CARTESIAN_POINT ( 'NONE',  ( 86.32087919958600253, 43.16070745389085772, 1.433418542445278776 ) ) ;
#81972 = ORIENTED_EDGE ( 'NONE', *, *, #14634, .F. ) ;
#81973 = CARTESIAN_POINT ( 'NONE',  ( 72.16868224958085420, 71.71251872039211150, 5.498261171115576218 ) ) ;
#81974 = CARTESIAN_POINT ( 'NONE',  ( 158.3301009428178361, 256.4112161299673858, 16.93297520252109933 ) ) ;
#81975 = DIRECTION ( 'NONE',  ( -0.000000000000000000, 0.000000000000000000, -1.000000000000000000 ) ) ;
#81976 = CARTESIAN_POINT ( 'NONE',  ( 88.11938802471243548, 44.55983648551643483, -5.053413235213815469 ) ) ;
#81977 = CARTESIAN_POINT ( 'NONE',  ( 202.8483755843326719, 275.3371640334334529, -14.10040576359822317 ) ) ;
#81978 = DIRECTION ( 'NONE',  ( 0.4999999999999998890, -0.8660254037844385966, 0.000000000000000000 ) ) ;
#81979 = EDGE_CURVE ( 'NONE', #34461, #40710, #22752, .T. ) ;
#81980 = VECTOR ( 'NONE', #27, 1000.000000000000114 ) ;
#81981 = CARTESIAN_POINT ( 'NONE',  ( 28.60632300232808589, 31.91421378149921040, 9.188101187500008038 ) ) ;
#81982 = AXIS2_PLACEMENT_3D ( 'NONE', #77992, #95230, #981 ) ;
#81983 = CARTESIAN_POINT ( 'NONE',  ( 73.23331724570277856, 60.52924755718257188, -15.20160680498939598 ) ) ;
#81984 = EDGE_CURVE ( 'NONE', #92543, #23591, #8058, .T. ) ;
#81985 = DIRECTION ( 'NONE',  ( 0.4999999999999998890, -0.8660254037844385966, 0.000000000000000000 ) ) ;
#81986 = CARTESIAN_POINT ( 'NONE',  ( 87.60638430035473334, 45.49210694301174840, 6.833128380864941676 ) ) ;
#81987 = VECTOR ( 'NONE', #45506, 1000.000000000000227 ) ;
#81988 = VERTEX_POINT ( 'NONE', #7539 ) ;
#81989 = VERTEX_POINT ( 'NONE', #62728 ) ;
#81990 = FACE_OUTER_BOUND ( 'NONE', #21298, .T. ) ;
#81992 = CARTESIAN_POINT ( 'NONE',  ( 162.2535035907551730, 272.2911684813469151, -15.91294751376331007 ) ) ;
#81991 = CARTESIAN_POINT ( 'NONE',  ( 163.8990931530087494, 246.7654386749614162, 5.873176884778091633 ) ) ;
#81993 = CARTESIAN_POINT ( 'NONE',  ( 85.74084692921037743, 48.48815037812249784, -11.76915627900790540 ) ) ;
#81994 = DIRECTION ( 'NONE',  ( -0.4999999999999987788, 0.8660254037844392627, 0.000000000000000000 ) ) ;
#81995 = CARTESIAN_POINT ( 'NONE',  ( 154.4470374439381146, 277.6591429590598068, -9.115886381272481742 ) ) ;
#81996 = CARTESIAN_POINT ( 'NONE',  ( 82.35755591800861453, 40.39341603438295891, 1.412376108039225864 ) ) ;
#81998 = EDGE_CURVE ( 'NONE', #30330, #53652, #100264, .T. ) ;
#81997 = CARTESIAN_POINT ( 'NONE',  ( 169.4077006606329405, 286.8755356998590855, -4.641866896595598924 ) ) ;
#81999 = CARTESIAN_POINT ( 'NONE',  ( 169.2387200762215684, 267.1480446973579888, 16.80865198575004982 ) ) ;
#82000 = CARTESIAN_POINT ( 'NONE',  ( 181.7124919110368921, 257.0325072718674164, 5.021470642198736734 ) ) ;
#82001 = CARTESIAN_POINT ( 'NONE',  ( 104.0717290597573026, 221.7048013555409796, 4.594050593750051981 ) ) ;
#82002 = ORIENTED_EDGE ( 'NONE', *, *, #44455, .F. ) ;
#82003 = CARTESIAN_POINT ( 'NONE',  ( 73.99515186948657686, 54.97541550358009488, -16.60506967685200408 ) ) ;
#82004 = DIRECTION ( 'NONE',  ( 0.8660254037844378194, 0.5000000000000013323, 0.000000000000000000 ) ) ;
#82005 = CARTESIAN_POINT ( 'NONE',  ( 166.7216842753552157, 278.1553442122267370, -13.35919087224943880 ) ) ;
#82006 = VERTEX_POINT ( 'NONE', #38430 ) ;
#82007 = ORIENTED_EDGE ( 'NONE', *, *, #73429, .T. ) ;
#82008 = ORIENTED_EDGE ( 'NONE', *, *, #25303, .T. ) ;
#82009 = CARTESIAN_POINT ( 'NONE',  ( 87.02439212704567240, 45.81336919377327632, -8.633490303204487404 ) ) ;
#82010 = ADVANCED_FACE ( 'NONE', ( #77465 ), #93686, .T. ) ;
#82011 = CARTESIAN_POINT ( 'NONE',  ( 179.2777005192219235, 293.2395681535716108, -2.642785613701771563 ) ) ;
#82012 = CARTESIAN_POINT ( 'NONE',  ( 196.3341081413628899, 290.5863447708742342, 16.12390540996472410 ) ) ;
#82013 = CARTESIAN_POINT ( 'NONE',  ( 159.5050723400634638, 254.3761059724978679, -15.34938048045353298 ) ) ;
#82014 = B_SPLINE_CURVE_WITH_KNOTS ( 'NONE', 3,
 ( #77051, #32464, #25356, #9685, #70456, #62849, #86718, #55238, #62339, #40545, #70980, #55729, #1067, #79101, #63361, #16257, #17775, #54233, #48159, #69457, #1581, #39532, #78580, #8166, #54740, #94301, #31447, #39037, #85726, #71480, #85201, #7660, #38548, #93293, #2075, #9165, #46652, #40039, #69947, #24854, #17254, #93805, #32953, #86219, #23848, #63858 ),
 .UNSPECIFIED., .F., .F.,
 ( 4, 1, 2, 2, 1, 2, 2, 1, 1, 2, 2, 1, 1, 2, 2, 1, 1, 2, 2, 1, 1, 1, 2, 2, 1, 1, 1, 2, 2, 4 ),
 ( 0.000000000000000000, 0.06249999999999159006, 0.09374999999998935574, 0.1249999999999871214, 0.1874999999999826528, 0.2187499999999827915, 0.2499999999999829581, 0.3124999999999871214, 0.3437499999999888978, 0.3593749999999896749, 0.3749999999999904521, 0.4374999999999901190, 0.4687499999999881206, 0.4843749999999875100, 0.4999999999999868994, 0.5624999999999862332, 0.5937499999999877875, 0.6093749999999867883, 0.6249999999999857891, 0.6874999999999792388, 0.7187499999999759082, 0.7343749999999742428, 0.7421874999999752420, 0.7499999999999763522, 0.8124999999999775735, 0.8437499999999800160, 0.8593749999999811262, 0.8671874999999835687, 0.8749999999999859002, 1.000000000000000000 ),
 .UNSPECIFIED. ) ;
#82015 = CARTESIAN_POINT ( 'NONE',  ( 208.3379394461497895, 269.7950990654974817, 2.541397148058371691 ) ) ;
#82016 = EDGE_CURVE ( 'NONE', #8241, #49563, #69837, .T. ) ;
#82017 = EDGE_LOOP ( 'NONE', ( #76817, #97919, #3932, #59241 ) ) ;
#82018 = VERTEX_POINT ( 'NONE', #24249 ) ;
#82019 = CARTESIAN_POINT ( 'NONE',  ( 189.5534384022301424, 269.0062095459838929, -14.92796778812864922 ) ) ;
#82020 = CARTESIAN_POINT ( 'NONE',  ( 207.8446715390582540, 270.6494641423232679, -2.429516028743652800 ) ) ;
#82021 = ORIENTED_EDGE ( 'NONE', *, *, #49370, .T. ) ;
#82022 = DIRECTION ( 'NONE',  ( -0.9364604334398948238, 0.2023802897980871707, -0.2865031848039503726 ) ) ;
#82023 = DIRECTION ( 'NONE',  ( 0.4999999999999998890, -0.8660254037844385966, 0.000000000000000000 ) ) ;
#82024 = CONICAL_SURFACE ( 'NONE', #41543, 11.00000000000002842, 0.7853981633974557175 ) ;
#82025 = DIRECTION ( 'NONE',  ( -0.8660254037844387076, -0.4999999999999998890, -0.000000000000000000 ) ) ;
#82027 = CARTESIAN_POINT ( 'NONE',  ( 199.9289737974172567, 283.7008907154707344, 17.00951001457953637 ) ) ;
#82026 = CARTESIAN_POINT ( 'NONE',  ( 130.5662598870812019, 252.3149278399160664, 9.188101187500093303 ) ) ;
#82028 = CARTESIAN_POINT ( 'NONE',  ( 29.41244916810467203, 42.77587997571678358, -10.00000000000000000 ) ) ;
#82029 = VERTEX_POINT ( 'NONE', #85080 ) ;
#82031 = CARTESIAN_POINT ( 'NONE',  ( 69.55128746018320385, 199.4155109091896065, 2.679491924311254714 ) ) ;
#82030 = VECTOR ( 'NONE', #89721, 1000.000000000000114 ) ;
#82032 = CARTESIAN_POINT ( 'NONE',  ( 87.97782240006738164, 43.76496563450900368, 2.369043524150745927 ) ) ;
#82033 = EDGE_CURVE ( 'NONE', #31533, #94451, #75893, .T. ) ;
#82034 = CARTESIAN_POINT ( 'NONE',  ( 206.7893622945242385, 272.4773133715531230, -10.52881283832460291 ) ) ;
#82035 = CARTESIAN_POINT ( 'NONE',  ( 170.0332508499076312, 248.8708985649008696, -0.2654087898054893757 ) ) ;
#82036 = CARTESIAN_POINT ( 'NONE',  ( 33.96495592097634386, 201.9637435831425023, 2.679491924311251605 ) ) ;
#82037 = VECTOR ( 'NONE', #7702, 1000.000000000000114 ) ;
#82038 = CARTESIAN_POINT ( 'NONE',  ( 76.37155543872398766, 51.66608632798631362, -16.16864924473253495 ) ) ;
#82039 = CARTESIAN_POINT ( 'NONE',  ( 199.0897609194714164, 281.8722272735701040, -16.59838435980774562 ) ) ;
#82040 = CARTESIAN_POINT ( 'NONE',  ( 136.4265865026747804, 261.1199935810940360, 2.679491924311251605 ) ) ;
#82041 = EDGE_CURVE ( 'NONE', #6796, #7444, #62224, .T. ) ;
#82042 = CARTESIAN_POINT ( 'NONE',  ( 79.30680381492646802, 47.66299911123399369, 13.58578065917975408 ) ) ;
#82043 = CARTESIAN_POINT ( 'NONE',  ( 206.7925996035142759, 272.0411403573240818, 6.555066398942419603 ) ) ;
#82044 = CARTESIAN_POINT ( 'NONE',  ( 167.6018919913909428, 249.9623704280710967, 7.441045516060340148 ) ) ;
#82045 = CARTESIAN_POINT ( 'NONE',  ( 77.76918168362882966, 62.01216915286021703, 15.64204638271909609 ) ) ;
#82046 = CARTESIAN_POINT ( 'NONE',  ( 207.6837091943624785, 270.9282591014416539, -1.156610046911421552 ) ) ;
#82047 = EDGE_CURVE ( 'NONE', #49158, #31854, #85605, .T. ) ;
#82048 = ADVANCED_FACE ( 'NONE', ( #37759 ), #37272, .T. ) ;
#82049 = VECTOR ( 'NONE', #59546, 1000.000000000000114 ) ;
#82050 = CARTESIAN_POINT ( 'NONE',  ( 68.81680935467448990, 70.26118697200512031, -1.737775333008780843 ) ) ;
#82052 = CARTESIAN_POINT ( 'NONE',  ( -20.77549415122608067, 95.15121615758417306, 45.19943101769310090 ) ) ;
#82051 = CARTESIAN_POINT ( 'NONE',  ( 177.5665759502285539, 275.7863988818428993, 17.69313789786682989 ) ) ;
#82054 = EDGE_CURVE ( 'NONE', #48590, #66065, #84410, .T. ) ;
#82053 = B_SPLINE_CURVE_WITH_KNOTS ( 'NONE', 3,
 ( #88925, #64555, #9873, #19485, #50341, #11866, #42722, #10363, #33664, #5248, #82791, #43728, #13357, #89407, #98955, #19958, #97471, #50835, #67531, #44221, #81785, #91367, #99451, #45226 ),
 .UNSPECIFIED., .F., .F.,
 ( 4, 2, 2, 2, 2, 2, 2, 2, 2, 2, 2, 4 ),
 ( 0.000000000000000000, 0.1249999999999922839, 0.2499999999999845679, 0.3749999999999768518, 0.4374999999999790723, 0.4999999999999813483, 0.5624999999999835687, 0.6249999999999857891, 0.6874999999999881206, 0.7499999999999903411, 0.8749999999999951150, 1.000000000000000000 ),
 .UNSPECIFIED. ) ;
#82055 = CARTESIAN_POINT ( 'NONE',  ( 187.0083344850037008, 268.0836409071914090, -15.22627500120235133 ) ) ;
#82056 = EDGE_CURVE ( 'NONE', #57272, #53392, #6386, .T. ) ;
#82057 = CARTESIAN_POINT ( 'NONE',  ( 33.91574581199579086, 27.78052372038643369, -10.00000000000000355 ) ) ;
#82058 = CARTESIAN_POINT ( 'NONE',  ( 76.26965850597605368, 57.48574154835009864, -16.55951103678767566 ) ) ;
#82059 = LINE ( 'NONE', #27812, #84942 ) ;
#82060 = PLANE ( 'NONE',  #65665 ) ;
#82061 = AXIS2_PLACEMENT_3D ( 'NONE', #1546, #24820, #9651 ) ;
#82062 = DIRECTION ( 'NONE',  ( 0.9041295198386993803, -0.4272584830711297910, 0.000000000000000000 ) ) ;
#82063 = CARTESIAN_POINT ( 'NONE',  ( 207.2337123599961899, 271.7076764818092443, -5.443417788256701861 ) ) ;
#82064 = CARTESIAN_POINT ( 'NONE',  ( 22.80074434730262567, 171.7202760586659736, -5.415160957724236172E-17 ) ) ;
#82065 = CARTESIAN_POINT ( 'NONE',  ( 68.75998362855375490, 69.65436878770546514, 5.732468190288290799 ) ) ;
#82066 = ORIENTED_EDGE ( 'NONE', *, *, #12122, .T. ) ;
#82067 = CARTESIAN_POINT ( 'NONE',  ( 86.88781708706541451, 46.48626182808993690, 9.021352103034745440 ) ) ;
#82068 = DIRECTION ( 'NONE',  ( -0.6066398774942428629, 0.7949767663484071933, 0.000000000000000000 ) ) ;
#82069 = CARTESIAN_POINT ( 'NONE',  ( 164.3890147726454813, 245.9168695380243435, -6.010262808998044548 ) ) ;
#82070 = CARTESIAN_POINT ( 'NONE',  ( 40.25072390630947439, 24.20801979619931998, -3.090169943749474069 ) ) ;
#82071 = CARTESIAN_POINT ( 'NONE',  ( 55.49285624440017273, 202.8458772461660260, 9.188101187500095079 ) ) ;
#82072 = CARTESIAN_POINT ( 'NONE',  ( 84.34903687182406884, 231.0530062829863027, -4.648177544792955347E-16 ) ) ;
#82073 = LINE ( 'NONE', #20236, #77369 ) ;
#82074 = CARTESIAN_POINT ( 'NONE',  ( 190.3625087333586521, 300.9294583479858147, -4.271886578030237303 ) ) ;
#82075 = CARTESIAN_POINT ( 'NONE',  ( 8.859747497914600700, 17.06628583063839599, -9.188101187500006262 ) ) ;
#82076 = CARTESIAN_POINT ( 'NONE',  ( 199.6805176955043066, 267.7911124590283976, -6.556812613813658430 ) ) ;
#82077 = CARTESIAN_POINT ( 'NONE',  ( 191.0933613939813540, 299.6635844069401173, -8.689828987424775164 ) ) ;
#82078 = ORIENTED_EDGE ( 'NONE', *, *, #25902, .F. ) ;
#82079 = CARTESIAN_POINT ( 'NONE',  ( 47.49582885874516336, 78.29235751436857527, -10.00000000000000000 ) ) ;
#82080 = CARTESIAN_POINT ( 'NONE',  ( 24.22498904768565353, 14.39040679176983062, 1.333680081654574804E-15 ) ) ;
#82081 = CARTESIAN_POINT ( 'NONE',  ( 87.07068318106846050, 45.96719988987016592, -8.154473134044517124 ) ) ;
#82082 = FACE_OUTER_BOUND ( 'NONE', #67635, .T. ) ;
#82083 = DIRECTION ( 'NONE',  ( -0.1237105541964931971, 0.9923183454821323801, 0.000000000000000000 ) ) ;
#82084 = CARTESIAN_POINT ( 'NONE',  ( 92.75901190277325270, 224.3615022471902591, -10.00000000000009592 ) ) ;
#82085 = CARTESIAN_POINT ( 'NONE',  ( 39.64431452495995245, 58.26521502737223557, -10.00000000000000000 ) ) ;
#82086 = CARTESIAN_POINT ( 'NONE',  ( 38.89349527680885643, 24.58380873178789727, 6.180339887498953466 ) ) ;
#82087 = VERTEX_POINT ( 'NONE', #90536 ) ;
#82088 = CARTESIAN_POINT ( 'NONE',  ( 60.68900866710680475, 205.8458772461660544, 9.188101187500095079 ) ) ;
#82089 = VERTEX_POINT ( 'NONE', #30170 ) ;
#82090 = CARTESIAN_POINT ( 'NONE',  ( 166.0118957362736012, 265.2928580242756880, 16.55930147465089064 ) ) ;
#82091 = CARTESIAN_POINT ( 'NONE',  ( 161.5400823882263808, 251.2469044075661486, 12.89492200680558120 ) ) ;
#82092 = CARTESIAN_POINT ( 'NONE',  ( 67.31420450098354991, 66.64469210376232411, -8.500257707143351382 ) ) ;
#82093 = ORIENTED_EDGE ( 'NONE', *, *, #25154, .T. ) ;
#82094 = CARTESIAN_POINT ( 'NONE',  ( 167.8036517631731215, 285.0360000349990628, 7.673623445836456725 ) ) ;
#82095 = CARTESIAN_POINT ( 'NONE',  ( 207.0548180518391916, 272.0175305127218053, 7.721676452263806389 ) ) ;
#82096 = DIRECTION ( 'NONE',  ( -1.000000000000000000, 0.000000000000000000, 0.000000000000000000 ) ) ;
#82097 = CARTESIAN_POINT ( 'NONE',  ( 32.45774345291223995, 27.24335787977765833, -9.188101187500008038 ) ) ;
#82098 = CARTESIAN_POINT ( 'NONE',  ( 186.3038661936600704, 263.7620536213361788, 10.91854419716388769 ) ) ;
#82099 = CARTESIAN_POINT ( 'NONE',  ( 86.35226789200304154, 47.00689162210669991, -10.01921365420989751 ) ) ;
#82100 = VECTOR ( 'NONE', #631, 1000.000000000000000 ) ;
#82101 = CARTESIAN_POINT ( 'NONE',  ( 205.0302908362115772, 275.5241145114948154, 13.44798751587103425 ) ) ;
#82102 = ORIENTED_EDGE ( 'NONE', *, *, #91277, .T. ) ;
#82103 = VECTOR ( 'NONE', #53636, 1000.000000000000114 ) ;
#82104 = CARTESIAN_POINT ( 'NONE',  ( 14.05709621874952475, 23.51421378149918340, -9.188101187500004485 ) ) ;
#82105 = CARTESIAN_POINT ( 'NONE',  ( 69.00650497353377943, 64.42272793400444186, 12.49602259808233562 ) ) ;
#82106 = CARTESIAN_POINT ( 'NONE',  ( 70.69086365586154841, 70.23154535277738830, -5.847355862645180480 ) ) ;
#82107 = CARTESIAN_POINT ( 'NONE',  ( 18.95962131514559346, 16.11029122506294087, -8.090169943749478065 ) ) ;
#82108 = VERTEX_POINT ( 'NONE', #61055 ) ;
#82109 = CARTESIAN_POINT ( 'NONE',  ( 181.1411778180677175, 283.4433145892596144, 14.97450737243938157 ) ) ;
#82110 = CARTESIAN_POINT ( 'NONE',  ( 39.64431452495995245, 58.26521502737223557, -10.00000000000000000 ) ) ;
#82111 = CARTESIAN_POINT ( 'NONE',  ( 206.1408608592916494, 273.6005508061571732, -10.42739367433323494 ) ) ;
#82112 = ORIENTED_EDGE ( 'NONE', *, *, #40123, .F. ) ;
#82113 = VERTEX_POINT ( 'NONE', #28676 ) ;
#82114 = AXIS2_PLACEMENT_3D ( 'NONE', #75013, #75507, #20311 ) ;
#82116 = LINE ( 'NONE', #35461, #60447 ) ;
#82115 = CARTESIAN_POINT ( 'NONE',  ( 161.6923300915171922, 250.5876644177310482, -14.43081872899884566 ) ) ;
#82117 = CARTESIAN_POINT ( 'NONE',  ( 196.2878005184348353, 290.6665519265632724, -16.69183432842427806 ) ) ;
#82118 = ORIENTED_EDGE ( 'NONE', *, *, #863, .F. ) ;
#82119 = CARTESIAN_POINT ( 'NONE',  ( 66.44514283687411194, 68.77124511786847449, -2.157765416611612697 ) ) ;
#82120 = DIRECTION ( 'NONE',  ( -0.1963739994383708332, 0.9805290675673918876, 0.000000000000000000 ) ) ;
#82121 = CARTESIAN_POINT ( 'NONE',  ( 81.88283113365912413, 55.39261312399677450, 16.27191101227217729 ) ) ;
#82122 = CARTESIAN_POINT ( 'NONE',  ( 78.08878743907096975, 62.01730706715306951, -16.03713534414099939 ) ) ;
#82124 = ADVANCED_FACE ( 'NONE', ( #38247 ), #44860, .F. ) ;
#82123 = CARTESIAN_POINT ( 'NONE',  ( 117.4133255192225391, 250.8464784336661353, 1.353441290958777525E-15 ) ) ;
#82125 = CARTESIAN_POINT ( 'NONE',  ( 190.9501423151522772, 299.9116471280854626, 8.746938802470586083 ) ) ;
#82126 = CARTESIAN_POINT ( 'NONE',  ( 67.84273934451053378, 216.6427522451419065, -10.00000000000009592 ) ) ;
#82127 = VERTEX_POINT ( 'NONE', #13501 ) ;
#82128 = CIRCLE ( 'NONE', #85379, 70.00000000000001421 ) ;
#82129 = CARTESIAN_POINT ( 'NONE',  ( 207.5215400641004351, 271.2091442744748520, 2.886080616848571534 ) ) ;
#82130 = VERTEX_POINT ( 'NONE', #14958 ) ;
#82131 = ORIENTED_EDGE ( 'NONE', *, *, #38048, .F. ) ;
#82132 = FACE_BOUND ( 'NONE', #88581, .T. ) ;
#82133 = CARTESIAN_POINT ( 'NONE',  ( 204.8370930553071503, 274.7064833943479698, -12.16292712972826706 ) ) ;
#82134 = CARTESIAN_POINT ( 'NONE',  ( 76.25066296318219372, 205.6423013555409796, -4.594050593750043987 ) ) ;
#82135 = ORIENTED_EDGE ( 'NONE', *, *, #69136, .T. ) ;
#82136 = EDGE_CURVE ( 'NONE', #14010, #52870, #91022, .T. ) ;
#82137 = CARTESIAN_POINT ( 'NONE',  ( 22.95375591501717594, 177.3927522451418497, 10.00000000000009948 ) ) ;
#82138 = DIRECTION ( 'NONE',  ( -1.000000000000000000, 0.000000000000000000, 0.000000000000000000 ) ) ;
#82139 = CARTESIAN_POINT ( 'NONE',  ( 198.6416989287814943, 286.5894802839873137, 18.33538993684147300 ) ) ;
#82140 = CARTESIAN_POINT ( 'NONE',  ( 173.3845174282522237, 277.2994966234552408, 15.60446512967379284 ) ) ;
#82141 = ADVANCED_FACE ( 'NONE', ( #91510 ), #53460, .T. ) ;
#82142 = ORIENTED_EDGE ( 'NONE', *, *, #42846, .F. ) ;
#82143 = CARTESIAN_POINT ( 'NONE',  ( 67.16990927169524639, 66.79708245693808522, -9.067759095298590921 ) ) ;
#82144 = VECTOR ( 'NONE', #5540, 1000.000000000000227 ) ;
#82145 = CARTESIAN_POINT ( 'NONE',  ( 87.59157332177183264, 43.83901051802146043, -1.268023806040525781 ) ) ;
#82146 = CARTESIAN_POINT ( 'NONE',  ( 201.0468719883840265, 282.4235983437597497, -16.59631526626950659 ) ) ;
#82147 = CARTESIAN_POINT ( 'NONE',  ( -27.42236680055714260, 166.5217562850347406, 1.224646799147364892E-15 ) ) ;
#82148 = EDGE_LOOP ( 'NONE', ( #98581, #50563, #73186, #57152 ) ) ;
#82149 = CARTESIAN_POINT ( 'NONE',  ( 156.6812872898450735, 261.2670451491295012, 0.000000000000000000 ) ) ;
#82150 = CARTESIAN_POINT ( 'NONE',  ( 161.1093323826042933, 251.5974460702646809, -13.93502574894237078 ) ) ;
#82151 = CARTESIAN_POINT ( 'NONE',  ( 164.2618602210349934, 246.6285193662782547, 4.483609632043464188 ) ) ;
#82152 = CARTESIAN_POINT ( 'NONE',  ( 50.30020549591840506, 90.50945844122863093, 177.5919119679930134 ) ) ;
#82153 = CARTESIAN_POINT ( 'NONE',  ( 164.8849641302980444, 245.0578600525887794, 2.884140591399200648 ) ) ;
#82154 = ORIENTED_EDGE ( 'NONE', *, *, #42742, .T. ) ;
#82155 = DIRECTION ( 'NONE',  ( -0.000000000000000000, -0.000000000000000000, -1.000000000000000000 ) ) ;
#82156 = CARTESIAN_POINT ( 'NONE',  ( 128.2929432021470859, 251.0024278399160949, 9.188101187500095079 ) ) ;
#82157 = ORIENTED_EDGE ( 'NONE', *, *, #34026, .T. ) ;
#82158 = CARTESIAN_POINT ( 'NONE',  ( 85.93878220393966672, 44.20073796858249437, -6.077267220493034472 ) ) ;
#82159 = CARTESIAN_POINT ( 'NONE',  ( 86.25488010490016677, 44.66640252382467935, 6.626028542311385827 ) ) ;
#82160 = CARTESIAN_POINT ( 'NONE',  ( 205.2706556652093752, 273.1077904153184477, -10.97544480913108167 ) ) ;
#82161 = LINE ( 'NONE', #12736, #15943 ) ;
#82162 = CARTESIAN_POINT ( 'NONE',  ( 74.35132386903860890, 58.97444165883455724, 15.77412187530554810 ) ) ;
#82163 = CARTESIAN_POINT ( 'NONE',  ( 200.6117230619925635, 269.0360104864248001, 9.242361455687714056 ) ) ;
#82164 = ORIENTED_EDGE ( 'NONE', *, *, #60528, .F. ) ;
#82165 = CARTESIAN_POINT ( 'NONE',  ( 77.58957552442460326, 61.75793702469097468, 15.67560070342385892 ) ) ;
#82166 = DIRECTION ( 'NONE',  ( 1.000000000000000000, 0.000000000000000000, 0.000000000000000000 ) ) ;
#82167 = EDGE_CURVE ( 'NONE', #49046, #45423, #17724, .T. ) ;
#82168 = CARTESIAN_POINT ( 'NONE',  ( 167.6380257754661045, 249.1599301665656867, -6.117841082608373782 ) ) ;
#82169 = CARTESIAN_POINT ( 'NONE',  ( 205.9580306612148490, 273.9172219983844911, -10.82161348643986720 ) ) ;
#82170 = CARTESIAN_POINT ( 'NONE',  ( 73.72368916567589281, 69.52486454841584873, -9.771537494043835537 ) ) ;
#82171 = CARTESIAN_POINT ( 'NONE',  ( 147.1249913145849177, 275.8190353104462815, 3.637773609013635223 ) ) ;
#82172 = EDGE_CURVE ( 'NONE', #41966, #30353, #9693, .T. ) ;
#82173 = CARTESIAN_POINT ( 'NONE',  ( 165.5918197702007433, 245.8335501706607147, 2.182451016153225905E-15 ) ) ;
#82174 = VECTOR ( 'NONE', #57858, 1000.000000000000000 ) ;
#82175 = CARTESIAN_POINT ( 'NONE',  ( 195.0636388027741930, 270.1460199898987184, 12.01487925370120990 ) ) ;
#82176 = EDGE_CURVE ( 'NONE', #22854, #69571, #48514, .T. ) ;
#82177 = B_SPLINE_SURFACE_WITH_KNOTS ( 'NONE', 3, 1, ( 
 ( #49976, #97594 ),
 ( #42842, #57560 ),
 ( #27686, #3399 ),
 ( #4885, #43853 ),
 ( #81909, #81414 ),
 ( #50958, #34761 ),
 ( #65661, #89527 ),
 ( #35267, #19603 ),
 ( #82428, #74794 ),
 ( #12488, #97118 ),
 ( #96120, #96619 ),
 ( #5372, #27183 ),
 ( #80933, #4369 ),
 ( #88536, #58070 ),
 ( #66663, #20087 ),
 ( #34274, #26674 ),
 ( #43355, #74303 ),
 ( #73286, #98079 ),
 ( #28165, #3878 ),
 ( #11986, #57059 ),
 ( #11502, #73780 ),
 ( #66172, #88041 ),
 ( #59035, #42354 ),
 ( #89053, #50463 ),
 ( #90006, #20581 ),
 ( #51462, #12994 ),
 ( #36255, #18590 ),
 ( #49468, #67158 ),
 ( #80423, #10996 ),
 ( #41868, #61543 ),
 ( #53926, #22053 ) ),
 .UNSPECIFIED., .F., .F., .F.,
 ( 4, 3, 3, 3, 3, 3, 3, 3, 3, 3, 4 ),
 ( 2, 2 ),
 ( 0.000000000000000000, 0.1333490885032350692, 0.3007194338854288218, 0.4699862290245104268, 0.5844252810809298371, 0.6686540514502736787, 0.7354980260655487045, 0.8028463152565475935, 0.8633854507757110497, 0.9437142632667278042, 1.000000000000000000 ),
 ( 0.000000000000000000, 1.000000000000000000 ),
 .UNSPECIFIED. ) ;
#82178 = CARTESIAN_POINT ( 'NONE',  ( 17.67616779290014506, 25.90829794293879829, 10.00000000000000355 ) ) ;
#82179 = CARTESIAN_POINT ( 'NONE',  ( 149.0761751337341821, 272.4394858007734683, 11.56094486755886130 ) ) ;
#82180 = CARTESIAN_POINT ( 'NONE',  ( 7.864685750751951865, 30.05722773587472929, 10.00000000000000000 ) ) ;
#82181 = CARTESIAN_POINT ( 'NONE',  ( 71.82585323880603312, 69.27534975156628150, -9.342054464929514523 ) ) ;
#82182 = CARTESIAN_POINT ( 'NONE',  ( 188.0361769804965206, 281.7550819701144746, -17.70093714309158983 ) ) ;
#82183 = CARTESIAN_POINT ( 'NONE',  ( 72.26713406221064417, 71.94669707650473356, -3.758665421101202497 ) ) ;
#82184 = AXIS2_PLACEMENT_3D ( 'NONE', #43235, #51340, #67539 ) ;
#82185 =( BOUNDED_CURVE ( )  B_SPLINE_CURVE ( 2, ( #25084, #1305, #77301, #32188, #30703, #61583, #15476, #31674, #92534 ),
 .UNSPECIFIED., .F., .T. ) 
 B_SPLINE_CURVE_WITH_KNOTS ( ( 3, 2, 2, 2, 3 ),
 ( 0.4072580645161290591, 0.4086021505376344343, 0.4112903225806451846, 0.4139784946236559349, 0.4153225806451613100 ),
 .UNSPECIFIED. ) 
 CURVE ( )  GEOMETRIC_REPRESENTATION_ITEM ( )  RATIONAL_B_SPLINE_CURVE ( ( 0.9330127018922194093, 0.9330127018922207416, 1.000000000000000000, 0.8660254037844387076, 1.000000000000000000, 0.8660254037844387076, 1.000000000000000000, 0.9330127018922194093, 0.9330127018922194093 ) ) 
 REPRESENTATION_ITEM ( '' )  );
#82186 = CARTESIAN_POINT ( 'NONE',  ( 138.1351346183475357, 243.8927522451417929, -10.00000000000009059 ) ) ;
#82187 = CARTESIAN_POINT ( 'NONE',  ( 175.9837504787562636, 285.3457777721278603, -12.01839870738883143 ) ) ;
#82188 = EDGE_LOOP ( 'NONE', ( #51971, #56162, #56005, #75597 ) ) ;
#82189 = VECTOR ( 'NONE', #30735, 1000.000000000000000 ) ;
#82190 = CARTESIAN_POINT ( 'NONE',  ( 66.85524610400480583, 67.34209505064849566, -6.990925417236245387 ) ) ;
#82191 = CARTESIAN_POINT ( 'NONE',  ( 151.0388915836658725, 269.0399611886400635, -14.24896787280406585 ) ) ;
#82192 = CARTESIAN_POINT ( 'NONE',  ( -8.674473839076844328, 174.9869531367911293, 4.594050593750046652 ) ) ;
#82193 = CARTESIAN_POINT ( 'NONE',  ( 53.49034604603116350, 195.5643266524160140, 9.188101187500095079 ) ) ;
#82194 = CARTESIAN_POINT ( 'NONE',  ( 86.51006589432671490, 46.32215150632234213, 9.708631656330311444 ) ) ;
#82195 = CARTESIAN_POINT ( 'NONE',  ( 27.35777070392073185, 16.76426979415090557, 3.090169943749476733 ) ) ;
#82196 = CARTESIAN_POINT ( 'NONE',  ( 85.35998281785300890, 48.55136375776380930, 12.45655298324007632 ) ) ;
#82197 = AXIS2_PLACEMENT_3D ( 'NONE', #36339, #52049, #92579 ) ;
#82198 = CARTESIAN_POINT ( 'NONE',  ( 157.8239779013331372, 257.2878469527003062, -17.92251383114021479 ) ) ;
#82199 = CARTESIAN_POINT ( 'NONE',  ( 189.5693900039456707, 290.6981618181056888, -14.49310309556349274 ) ) ;
#82200 = CARTESIAN_POINT ( 'NONE',  ( 74.24029763082349120, 55.47955095029949035, -16.12046342301015045 ) ) ;
#82201 = CARTESIAN_POINT ( 'NONE',  ( 168.7281583638259121, 257.2268137270143029, 13.70307109309566940 ) ) ;
#82202 = CARTESIAN_POINT ( 'NONE',  ( 74.81309782283618404, 67.19796050844534818, 12.47715916803399772 ) ) ;
#82203 = CARTESIAN_POINT ( 'NONE',  ( 198.0542955016221924, 287.6068928643675804, 18.26164672886581997 ) ) ;
#82204 = CARTESIAN_POINT ( 'NONE',  ( 179.2120688271028541, 294.1024010724993332, 1.048020959340867364 ) ) ;
#82205 = CARTESIAN_POINT ( 'NONE',  ( 60.28305926085680966, 205.6115022471902591, 10.00000000000009592 ) ) ;
#82206 = FACE_OUTER_BOUND ( 'NONE', #83242, .T. ) ;
#82207 = VECTOR ( 'NONE', #52475, 1000.000000000000000 ) ;
#82208 = CARTESIAN_POINT ( 'NONE',  ( 147.6857584380539095, 274.8477581613835810, 8.112022437684441201 ) ) ;
#82209 = CARTESIAN_POINT ( 'NONE',  ( 27.67213724359008964, 174.5327760586659451, 1.948934522072303157E-15 ) ) ;
#82210 = CARTESIAN_POINT ( 'NONE',  ( 164.4201679284129227, 284.8060357136131415, 4.241341315168992487 ) ) ;
#82211 = EDGE_CURVE ( 'NONE', #34226, #27863, #27546, .T. ) ;
#82212 = CARTESIAN_POINT ( 'NONE',  ( 79.38761854802169182, 59.75627238307979638, 16.16632707334086660 ) ) ;
#82213 = CARTESIAN_POINT ( 'NONE',  ( 36.95804531498377798, 23.19860640527294748, 2.839279412974134775 ) ) ;
#82214 = DIRECTION ( 'NONE',  ( -0.5696381972391070247, 0.8218955677251095215, 0.000000000000000000 ) ) ;
#82215 = CARTESIAN_POINT ( 'NONE',  ( 179.9844968997953174, 277.0016935229651267, 16.30433957883684570 ) ) ;
#82216 = CARTESIAN_POINT ( 'NONE',  ( 175.4507454171546783, 278.7747778411292643, 15.41403683019787962 ) ) ;
#82217 = CYLINDRICAL_SURFACE ( 'NONE', #78504, 10.00000000000001066 ) ;
#82218 = CARTESIAN_POINT ( 'NONE',  ( 177.5011205626351227, 261.3373948018718238, -13.00779142369327523 ) ) ;
#82219 = CARTESIAN_POINT ( 'NONE',  ( 19.86064915544625009, 12.26216523072493914, -2.296566073217252530E-15 ) ) ;
#82220 = CARTESIAN_POINT ( 'NONE',  ( 71.47384123275857348, 72.35069954344788812, 1.100233114707620530 ) ) ;
#82221 = CARTESIAN_POINT ( 'NONE',  ( 82.43748789999787618, 54.23981479609578571, 15.60310197765542384 ) ) ;
#82222 = CARTESIAN_POINT ( 'NONE',  ( 13.06432082636536762, 189.8967562850346837, -4.648177544792955347E-16 ) ) ;
#82223 = EDGE_LOOP ( 'NONE', ( #18592, #55980, #80009, #26077 ) ) ;
#82224 = CARTESIAN_POINT ( 'NONE',  ( 85.66595420452183873, 45.56309184094170206, -8.625663387003578819 ) ) ;
#82225 = CARTESIAN_POINT ( 'NONE',  ( 27.11554978534049098, 17.78380873178787525, -6.180339887498949025 ) ) ;
#82226 = CARTESIAN_POINT ( 'NONE',  ( 75.20214548854198711, 53.53950986635392439, -16.05195360511178038 ) ) ;
#82227 = CARTESIAN_POINT ( 'NONE',  ( 206.1798448551755598, 273.5330285446045195, -10.53862763475382813 ) ) ;
#82229 = ORIENTED_EDGE ( 'NONE', *, *, #96342, .F. ) ;
#82228 = B_SPLINE_CURVE_WITH_KNOTS ( 'NONE', 3,
 ( #81014, #11576, #3956, #34839, #58147, #89127, #61625, #76364, #21652, #75876, #76834, #44436, #99158, #92580, #92101, #84972, #38824, #23122, #83485, #83991, #13564, #37332, #36842, #54015, #15517, #46419, #22145, #75369, #68734, #21169, #15024, #38325, #91087, #98675, #45430, #60618, #30243, #44929, #45915, #61124, #22646, #99657, #37825, #53531, #84482, #91573, #60124, #7432 ),
 .UNSPECIFIED., .F., .F.,
 ( 4, 2, 2, 2, 2, 2, 2, 2, 2, 2, 2, 2, 2, 2, 2, 2, 2, 2, 2, 2, 2, 2, 2, 4 ),
 ( 0.0008680554427910739442, 0.001061939928173833824, 0.001158882170865213872, 0.001255824413556593921, 0.001449708898939420804, 0.001643593384322248122, 0.002031362355087858087, 0.002419131325853468052, 0.003970207208915833320, 0.004745745150447016822, 0.005133514121212644568, 0.005327398606595498340, 0.005424340849286961655, 0.005472811970632649077, 0.005521283091978336499, 0.005569754213324024789, 0.005618225334669713078, 0.005715167577361120882, 0.005909052062743800314, 0.006102936548126478011, 0.006296821033509157443, 0.006490705518891836008, 0.006684590004274514573, 0.007072358975039798844 ),
 .UNSPECIFIED. ) ;
#82230 = CARTESIAN_POINT ( 'NONE',  ( 152.8134625983922490, 265.9663140294953791, 17.57333028169644251 ) ) ;
#82231 = LINE ( 'NONE', #83713, #77295 ) ;
#82232 = CARTESIAN_POINT ( 'NONE',  ( 66.39267195988500703, 68.17678030604481876, 4.478186808409195585 ) ) ;
#82233 = CARTESIAN_POINT ( 'NONE',  ( 155.3716771045260714, 261.5353565282119348, -18.54934131471355840 ) ) ;
#82234 = VERTEX_POINT ( 'NONE', #9891 ) ;
#82235 = ORIENTED_EDGE ( 'NONE', *, *, #31520, .T. ) ;
#82237 = CARTESIAN_POINT ( 'NONE',  ( 204.4325665793906524, 276.5594032932251594, 13.33817701435311598 ) ) ;
#82236 = CARTESIAN_POINT ( 'NONE',  ( 159.2244323577040177, 279.5560594508606300, -9.704040566180836436 ) ) ;
#82238 = CARTESIAN_POINT ( 'NONE',  ( 192.6224552386041182, 297.0151161785129261, 12.49354144254605181 ) ) ;
#82239 = ORIENTED_EDGE ( 'NONE', *, *, #9942, .T. ) ;
#82240 = CARTESIAN_POINT ( 'NONE',  ( 88.44266034405603705, 44.03949081389492903, -2.406584733330055847 ) ) ;
#82241 = CIRCLE ( 'NONE', #90336, 70.00000000000001421 ) ;
#82242 = FACE_OUTER_BOUND ( 'NONE', #46661, .T. ) ;
#82243 = CARTESIAN_POINT ( 'NONE',  ( 177.5782878460544225, 263.8519546370548028, 14.60380941168531166 ) ) ;
#82244 = EDGE_LOOP ( 'NONE', ( #4416, #36216, #70167, #47036 ) ) ;
#82245 = CARTESIAN_POINT ( 'NONE',  ( 87.62084567981032990, 45.15010746144617571, -6.151098611497959112 ) ) ;
#82246 = CARTESIAN_POINT ( 'NONE',  ( 81.25234104358975173, 49.54399800360413764, -14.03529770125688181 ) ) ;
#82247 = ADVANCED_FACE ( 'NONE', ( #15963 ), #78281, .F. ) ;
#82248 = CIRCLE ( 'NONE', #100070, 70.00000000000001421 ) ;
#82249 = CARTESIAN_POINT ( 'NONE',  ( 81.14511053440421051, 43.10620461581409302, 9.543047636977719961 ) ) ;
#82250 = EDGE_LOOP ( 'NONE', ( #25004, #79266, #3935 ) ) ;
#82251 = CARTESIAN_POINT ( 'NONE',  ( 205.7639495959071212, 274.2533802642843170, 10.79039487422292432 ) ) ;
#82252 = CARTESIAN_POINT ( 'NONE',  ( 74.00425782610878400, 61.02723150855160839, 15.19944699234505059 ) ) ;
#82253 = ORIENTED_EDGE ( 'NONE', *, *, #91376, .F. ) ;
#82254 = CARTESIAN_POINT ( 'NONE',  ( 177.8323663984979532, 279.4302167523874232, -16.28584057845160515 ) ) ;
#82255 = CARTESIAN_POINT ( 'NONE',  ( 199.3359313799735162, 277.8054090533971134, 16.38672730308284997 ) ) ;
#82256 = ORIENTED_EDGE ( 'NONE', *, *, #42360, .T. ) ;
#82257 = EDGE_CURVE ( 'NONE', #19564, #89238, #85415, .T. ) ;
#82258 = CARTESIAN_POINT ( 'NONE',  ( 149.0240550263898740, 274.5270876550541743, 9.114866661042729135 ) ) ;
#82259 = ORIENTED_EDGE ( 'NONE', *, *, #24549, .F. ) ;
#82260 = EDGE_CURVE ( 'NONE', #37254, #705, #96356, .T. ) ;
#82261 = CARTESIAN_POINT ( 'NONE',  ( 157.4876528856866287, 268.9475409797686325, 15.59749454131434732 ) ) ;
#82262 = ORIENTED_EDGE ( 'NONE', *, *, #16346, .F. ) ;
#82263 = AXIS2_PLACEMENT_3D ( 'NONE', #98020, #59478, #36190 ) ;
#82264 = CARTESIAN_POINT ( 'NONE',  ( 154.5269387696429533, 265.4077020348397014, -16.45718875575290951 ) ) ;
#82265 = FACE_OUTER_BOUND ( 'NONE', #32060, .T. ) ;
#82266 = PLANE ( 'NONE',  #62570 ) ;
#82267 = CARTESIAN_POINT ( 'NONE',  ( 19.39689925177878749, 34.96947112835012916, 10.00000000000000000 ) ) ;
#82268 = CARTESIAN_POINT ( 'NONE',  ( 192.3606619183491091, 297.4685555102766443, 10.99569063633359889 ) ) ;
#82269 = LINE ( 'NONE', #3252, #22451 ) ;
#82270 = CARTESIAN_POINT ( 'NONE',  ( 194.6737116153428246, 263.0965258421714452, 3.813308892523692872 ) ) ;
#82271 = CIRCLE ( 'NONE', #27269, 0.1418229129681557177 ) ;
#82272 = VERTEX_POINT ( 'NONE', #38758 ) ;
#82273 = CARTESIAN_POINT ( 'NONE',  ( 75.65057567447028930, 57.49826290993107847, -16.09206823455592783 ) ) ;
#82274 = CARTESIAN_POINT ( 'NONE',  ( 39.23990543832261579, 24.78380873178790011, -6.180339887498949025 ) ) ;
#82276 = CARTESIAN_POINT ( 'NONE',  ( 205.9642072045669465, 273.9065239114831911, 10.22128930895731536 ) ) ;
#82275 = CARTESIAN_POINT ( 'NONE',  ( 149.7072529793668707, 271.3464269086063041, -11.98883662638834657 ) ) ;
#82277 = CARTESIAN_POINT ( 'NONE',  ( 198.4264492142971221, 286.9623037257889564, 17.00126466006521397 ) ) ;
#82278 = CARTESIAN_POINT ( 'NONE',  ( 171.3375887344810735, 288.5721954326351124, 4.189121038472729097 ) ) ;
#82279 = DIRECTION ( 'NONE',  ( 0.5000000000000002220, -0.8660254037844387076, -0.000000000000000000 ) ) ;
#82280 = ORIENTED_EDGE ( 'NONE', *, *, #70651, .F. ) ;
#82281 = CARTESIAN_POINT ( 'NONE',  ( 71.41026323507222173, 68.20115165556771331, 9.666511346903975621 ) ) ;
#82282 = CARTESIAN_POINT ( 'NONE',  ( 86.50265851752267565, 45.17908078762290813, 8.152107817765472220 ) ) ;
#82283 = DIRECTION ( 'NONE',  ( 1.000000000000000000, 0.000000000000000000, 0.000000000000000000 ) ) ;
#82284 = CARTESIAN_POINT ( 'NONE',  ( 159.9019937409323688, 253.6886179395814622, -15.75542456264497559 ) ) ;
#82285 = CARTESIAN_POINT ( 'NONE',  ( 148.1086267770833729, 274.1153287132722198, -10.31239854325041705 ) ) ;
#82286 = ORIENTED_EDGE ( 'NONE', *, *, #39262, .T. ) ;
#82287 = CARTESIAN_POINT ( 'NONE',  ( 168.7890239821780085, 254.3732592748322361, -11.73109540831163500 ) ) ;
#82288 = CARTESIAN_POINT ( 'NONE',  ( 205.5320288733365146, 274.0930176087748578, 10.72952057639821000 ) ) ;
#82289 = CIRCLE ( 'NONE', #11101, 70.00000000000001421 ) ;
#82290 = EDGE_CURVE ( 'NONE', #82431, #39405, #31151, .T. ) ;
#82291 = CARTESIAN_POINT ( 'NONE',  ( 201.4617167010348737, 281.7050662241970826, -17.43131506460443703 ) ) ;
#82292 = CARTESIAN_POINT ( 'NONE',  ( 164.9971748156432056, 244.8635054444190757, -1.825016704039769788 ) ) ;
#82293 = EDGE_CURVE ( 'NONE', #57499, #64644, #83066, .T. ) ;
#82294 = CARTESIAN_POINT ( 'NONE',  ( 31.54184116921283376, 189.0177522451418497, -10.00000000000009592 ) ) ;
#82295 = CARTESIAN_POINT ( 'NONE',  ( 109.2943373587434195, 246.1589784336661069, -6.496448406907676862E-16 ) ) ;
#82296 = CARTESIAN_POINT ( 'NONE',  ( 181.7371966266162815, 294.7030870310439923, -2.651400403382340176 ) ) ;
#82297 = CARTESIAN_POINT ( 'NONE',  ( 165.5402849709041959, 280.7227082719551277, -11.05355863872715361 ) ) ;
#82298 = B_SPLINE_CURVE_WITH_KNOTS ( 'NONE', 3,
 ( #17501, #79847, #48405, #10413 ),
 .UNSPECIFIED., .F., .F.,
 ( 4, 4 ),
 ( 0.02996210580220542985, 0.03907057961704281379 ),
 .UNSPECIFIED. ) ;
#82299 = CARTESIAN_POINT ( 'NONE',  ( 195.8248271798537417, 291.4684452715354155, 17.35175160929494709 ) ) ;
#82300 = CARTESIAN_POINT ( 'NONE',  ( 163.1685298068643988, 248.0308115086310465, 10.61953511350444046 ) ) ;
#82301 = CARTESIAN_POINT ( 'NONE',  ( 32.38097682878547090, 183.3768266524159856, 9.188101187500098632 ) ) ;
#82302 = CARTESIAN_POINT ( 'NONE',  ( 82.54945800575664805, 40.79138297396659851, 3.187804637566770349 ) ) ;
#82303 = ORIENTED_EDGE ( 'NONE', *, *, #90573, .T. ) ;
#82304 = VERTEX_POINT ( 'NONE', #42253 ) ;
#82305 = CARTESIAN_POINT ( 'NONE',  ( 9.911560002841389050, 164.9824982072973967, 3.021315404115420679E-15 ) ) ;
#82306 = CARTESIAN_POINT ( 'NONE',  ( 74.44157817134914978, 68.05905795514840406, -11.63231436587478740 ) ) ;
#82307 = CARTESIAN_POINT ( 'NONE',  ( 29.80979036164399432, 178.0177522451417929, 5.000000000000051514 ) ) ;
#82308 = CARTESIAN_POINT ( 'NONE',  ( 146.9324727656309335, 276.1524872186338371, 3.813717745456558728 ) ) ;
#82309 = CARTESIAN_POINT ( 'NONE',  ( 81.87824099083694307, 41.25415891943595881, -5.798576102226406626 ) ) ;
#82310 = CARTESIAN_POINT ( 'NONE',  ( 161.2133744761260061, 251.4172398781588811, -14.30368667312104058 ) ) ;
#82311 = DIRECTION ( 'NONE',  ( -0.8660254037844378194, -0.5000000000000014433, -0.000000000000000000 ) ) ;
#82312 = CARTESIAN_POINT ( 'NONE',  ( 74.07465050303007104, 67.87278060087763265, -11.60964415893985624 ) ) ;
#82313 = CARTESIAN_POINT ( 'NONE',  ( 99.16399144804778132, 221.3927522451417929, -10.00000000000009059 ) ) ;
#82314 = VECTOR ( 'NONE', #74686, 1000.000000000000000 ) ;
#82315 = ORIENTED_EDGE ( 'NONE', *, *, #8906, .T. ) ;
#82316 = CARTESIAN_POINT ( 'NONE',  ( 196.8199239667486609, 267.3837811503672697, -7.829876893548646244 ) ) ;
#82317 = AXIS2_PLACEMENT_3D ( 'NONE', #73943, #43005, #65817 ) ;
#82318 = CARTESIAN_POINT ( 'NONE',  ( 202.5511585997265911, 279.8180975037686835, 17.12781264818056925 ) ) ;
#82319 = CARTESIAN_POINT ( 'NONE',  ( 163.0424334805279045, 248.2492167524936804, -9.671494865076915914 ) ) ;
#82321 = EDGE_CURVE ( 'NONE', #29501, #44538, #12033, .T. ) ;
#82320 = AXIS2_PLACEMENT_3D ( 'NONE', #19336, #96340, #65399 ) ;
#82322 = CARTESIAN_POINT ( 'NONE',  ( 14.59995888762994554, 188.4244531367911293, -4.594050593750046652 ) ) ;
#82323 = AXIS2_PLACEMENT_3D ( 'NONE', #40795, #77835, #85469 ) ;
#82324 = CARTESIAN_POINT ( 'NONE',  ( 70.65694608054928949, 68.85554525066207532, -9.031325040935593407 ) ) ;
#82325 = CARTESIAN_POINT ( 'NONE',  ( 79.41031494441635630, 46.40275987550353420, -12.75878103946227782 ) ) ;
#82326 = CARTESIAN_POINT ( 'NONE',  ( 71.47130384908417966, 59.27950280012738205, -15.75482166576947662 ) ) ;
#82327 = FACE_OUTER_BOUND ( 'NONE', #46911, .T. ) ;
#82328 = CARTESIAN_POINT ( 'NONE',  ( 51.75829523846228852, 194.5643266524159856, -9.188101187500093303 ) ) ;
#82329 = PLANE ( 'NONE',  #18241 ) ;
#82330 = LINE ( 'NONE', #50369, #2989 ) ;
#82331 = DIRECTION ( 'NONE',  ( 0.000000000000000000, 0.000000000000000000, 1.000000000000000000 ) ) ;
#82332 = CARTESIAN_POINT ( 'NONE',  ( 66.34802823334818811, 68.15327646776096060, -4.473378551362304556 ) ) ;
#82333 = VERTEX_POINT ( 'NONE', #96019 ) ;
#82334 = CARTESIAN_POINT ( 'NONE',  ( -6.833909532437232315, 176.8615022471903160, 5.000000000000046185 ) ) ;
#82335 = B_SPLINE_CURVE_WITH_KNOTS ( 'NONE', 3,
 ( #2653, #47719, #9760, #48237, #85809, #33544, #86797, #86298, #78656, #64440, #25954, #32542, #87319, #95399, #48753, #17332, #63441, #40117, #49243, #71057, #40620, #56826, #87812, #70026, #1658, #80180, #94376, #71557, #70531, #54826, #33033, #79182, #24930, #2154, #55804, #63932, #641, #94871, #31522, #62415, #39610, #25433, #93376, #56324, #1148, #17851, #79685, #23928, #47234, #78152, #93884, #8739, #32023, #62932 ),
 .UNSPECIFIED., .F., .F.,
 ( 4, 2, 2, 2, 2, 2, 2, 2, 2, 2, 2, 2, 2, 2, 2, 2, 2, 2, 2, 2, 2, 2, 2, 2, 2, 2, 4 ),
 ( 0.0003929596557535101030, 0.0008568129670863414366, 0.001088739622752727667, 0.001320666278419114006, 0.001436629606252273024, 0.001552592934085432041, 0.001668556261918591058, 0.001784519589751749858, 0.002016446245418110177, 0.002248372901084470712, 0.002712226212417150582, 0.003176079523749829586, 0.004103786146415284303, 0.005031492769080740321, 0.005495346080413547260, 0.005727272736079950730, 0.005843236063913116035, 0.005901217727829699555, 0.005959199391746281341, 0.006017181055662863126, 0.006075162719579446646, 0.006191126047412610217, 0.006423052703078795111, 0.006886906014411166635, 0.007350759325743539893, 0.007582685981409723053, 0.007814612637075906212 ),
 .UNSPECIFIED. ) ;
#82336 = DIRECTION ( 'NONE',  ( -0.6778389383370750920, -0.7352104281592222179, 0.000000000000000000 ) ) ;
#82337 = CARTESIAN_POINT ( 'NONE',  ( 132.9753269110629503, 238.3923013555409796, 4.594050593750050204 ) ) ;
#82338 = CARTESIAN_POINT ( 'NONE',  ( 26.45569963029868177, 20.98920272979927049, 7.433330006724137462 ) ) ;
#82339 = CARTESIAN_POINT ( 'NONE',  ( 207.5409781303276588, 271.1754765561682348, -7.231270017877110767 ) ) ;
#82340 = DIRECTION ( 'NONE',  ( 1.000000000000000000, 0.000000000000000000, 0.000000000000000000 ) ) ;
#82341 = FACE_OUTER_BOUND ( 'NONE', #18017, .T. ) ;
#82343 = CARTESIAN_POINT ( 'NONE',  ( 189.4247981172279367, 289.8473999775135894, 14.52074419908731961 ) ) ;
#82342 = DIRECTION ( 'NONE',  ( 0.9991767892008865948, 0.04056776950002415755, 0.000000000000000000 ) ) ;
#82344 = CARTESIAN_POINT ( 'NONE',  ( 68.43344345364462811, 64.47918733080135212, 12.19408877863543061 ) ) ;
#82345 = EDGE_LOOP ( 'NONE', ( #46048, #94314, #97902, #48044 ) ) ;
#82346 = CARTESIAN_POINT ( 'NONE',  ( 150.8757650385446993, 269.3225046528533539, 14.31332712971473953 ) ) ;
#82347 = CARTESIAN_POINT ( 'NONE',  ( 208.2570380151932170, 269.9352244543189272, -0.4063029386674604782 ) ) ;
#82348 = CARTESIAN_POINT ( 'NONE',  ( 151.3417120142295289, 269.1063531457227214, -14.26574085409202652 ) ) ;
#82349 = CARTESIAN_POINT ( 'NONE',  ( 166.7436140395748225, 253.3389855339687244, 13.27779792997078090 ) ) ;
#82350 = CARTESIAN_POINT ( 'NONE',  ( 197.2826717042014479, 273.3494898236381800, -13.53960516259263613 ) ) ;
#82352 = ORIENTED_EDGE ( 'NONE', *, *, #49866, .F. ) ;
#82351 = VECTOR ( 'NONE', #6628, 1000.000000000000114 ) ;
#82353 = CARTESIAN_POINT ( 'NONE',  ( 71.47987467218354141, 71.01764064272968824, 5.056666948270793327 ) ) ;
#82354 = CARTESIAN_POINT ( 'NONE',  ( 74.32283972735670829, 55.33658384534070507, 16.60204640374922036 ) ) ;
#82355 = CARTESIAN_POINT ( 'NONE',  ( 86.07719285220247230, 46.34390285249480002, 9.364539065597575984 ) ) ;
#82356 = CARTESIAN_POINT ( 'NONE',  ( 193.1030321335636586, 294.1827325794992021, -14.54662778306917481 ) ) ;
#82357 = CARTESIAN_POINT ( 'NONE',  ( 181.8573685214958573, 295.1748175033092139, 4.857304733903339944 ) ) ;
#82358 = CARTESIAN_POINT ( 'NONE',  ( 67.91653825465498073, 69.16631803100915477, 4.245417807664631837 ) ) ;
#82359 = DIRECTION ( 'NONE',  ( -1.110223024625156343E-15, 1.000000000000000000, 0.000000000000000000 ) ) ;
#82360 = ORIENTED_EDGE ( 'NONE', *, *, #81062, .F. ) ;
#82361 = PLANE ( 'NONE',  #128 ) ;
#82362 = CARTESIAN_POINT ( 'NONE',  ( 16.59523773630703758, 17.78052372038640172, -10.00000000000000355 ) ) ;
#82363 = CARTESIAN_POINT ( 'NONE',  ( 192.0177730709008301, 287.5582357824112023, -16.95470262859629784 ) ) ;
#82364 = ORIENTED_EDGE ( 'NONE', *, *, #73774, .T. ) ;
#82365 = DIRECTION ( 'NONE',  ( -0.8660254037844377084, -0.5000000000000014433, -0.000000000000000000 ) ) ;
#82366 = CARTESIAN_POINT ( 'NONE',  ( 86.54479369881731543, 47.18726309986306688, -10.63286291588201316 ) ) ;
#82367 = CARTESIAN_POINT ( 'NONE',  ( 159.7028767715829929, 264.1383856807740358, -17.65718168856439618 ) ) ;
#82368 = ORIENTED_EDGE ( 'NONE', *, *, #98027, .F. ) ;
#82369 = CARTESIAN_POINT ( 'NONE',  ( 191.7934382699952494, 298.4510156884799699, -8.680100145728863126 ) ) ;
#82370 = CARTESIAN_POINT ( 'NONE',  ( 204.7444193837539501, 273.0031821285110709, -9.756915323793542427 ) ) ;
#82371 = CARTESIAN_POINT ( 'NONE',  ( 164.2851776226980860, 246.0967207574460929, 5.847738044744511754 ) ) ;
#82372 = EDGE_CURVE ( 'NONE', #89979, #27077, #26581, .T. ) ;
#82373 = DIRECTION ( 'NONE',  ( -0.8321961394790272637, 0.5544813661758195567, 0.000000000000000000 ) ) ;
#82374 = ORIENTED_EDGE ( 'NONE', *, *, #61776, .F. ) ;
#82375 = CARTESIAN_POINT ( 'NONE',  ( 85.85769841670955316, 226.5024278399160949, -9.188101187500093303 ) ) ;
#82376 = CARTESIAN_POINT ( 'NONE',  ( 155.0271965705274795, 262.1320143153159847, 17.46223432386462093 ) ) ;
#82377 = CARTESIAN_POINT ( 'NONE',  ( 181.2624089752565624, 271.4720694466574287, -17.37114438570441521 ) ) ;
#82378 = CARTESIAN_POINT ( 'NONE',  ( 181.8338920363375735, 257.2967203629509072, -6.061067647267480929 ) ) ;
#82379 = ORIENTED_EDGE ( 'NONE', *, *, #96899, .T. ) ;
#82380 = VERTEX_POINT ( 'NONE', #88435 ) ;
#82381 = ADVANCED_FACE ( 'NONE', ( #34663 ), #12380, .T. ) ;
#82382 = CARTESIAN_POINT ( 'NONE',  ( 88.35351169220642475, 43.78681510747281180, 0.1754685934989754781 ) ) ;
#82383 = ORIENTED_EDGE ( 'NONE', *, *, #94225, .F. ) ;
#82384 = CARTESIAN_POINT ( 'NONE',  ( 80.95286987779635979, 48.31441995295947578, 13.44804738609444783 ) ) ;
#82385 = ORIENTED_EDGE ( 'NONE', *, *, #5103, .T. ) ;
#82386 = EDGE_CURVE ( 'NONE', #36946, #4581, #95221, .T. ) ;
#82387 = CARTESIAN_POINT ( 'NONE',  ( 75.69790233746202546, 62.18877547806692263, 15.18360658727204182 ) ) ;
#82388 = CARTESIAN_POINT ( 'NONE',  ( 155.2922060645262263, 261.6730044072216401, -16.98884022075611355 ) ) ;
#82389 = ORIENTED_EDGE ( 'NONE', *, *, #72640, .F. ) ;
#82390 = CARTESIAN_POINT ( 'NONE',  ( 164.8768953149048286, 245.0718356508067188, 2.399905317103016689 ) ) ;
#82391 = CARTESIAN_POINT ( 'NONE',  ( 82.65950105694894035, 40.87543522790844008, 3.277353565571960115 ) ) ;
#82392 = ADVANCED_FACE ( 'NONE', ( #91896 ), #70952, .F. ) ;
#82393 = AXIS2_PLACEMENT_3D ( 'NONE', #80111, #56252, #1587 ) ;
#82394 = CARTESIAN_POINT ( 'NONE',  ( 201.0732166862245549, 282.3779679885897167, -18.18766936363638820 ) ) ;
#82395 = ADVANCED_FACE ( 'NONE', ( #63449 ), #40186, .F. ) ;
#82396 = CARTESIAN_POINT ( 'NONE',  ( 148.1829914015846157, 273.9865254053503349, -9.304102644963160529 ) ) ;
#82398 = CARTESIAN_POINT ( 'NONE',  ( 157.5735440838707007, 281.7061173120971489, 2.965151850968649416 ) ) ;
#82397 = VECTOR ( 'NONE', #58934, 1000.000000000000000 ) ;
#82399 = CARTESIAN_POINT ( 'NONE',  ( 168.3667151233534014, 267.2158819435744590, -17.25990780505111744 ) ) ;
#82400 = ORIENTED_EDGE ( 'NONE', *, *, #19660, .F. ) ;
#82401 = CARTESIAN_POINT ( 'NONE',  ( 76.67677140431342764, 59.69997763987031192, 15.91096609934128026 ) ) ;
#82402 = CARTESIAN_POINT ( 'NONE',  ( 10.26703877906431472, 17.87878583063839599, -9.188101187500006262 ) ) ;
#82403 = AXIS2_PLACEMENT_3D ( 'NONE', #42385, #91034, #22587 ) ;
#82404 = ORIENTED_EDGE ( 'NONE', *, *, #81130, .T. ) ;
#82405 = CARTESIAN_POINT ( 'NONE',  ( 167.2558879808692609, 284.3031459148808722, 9.343441084002181540 ) ) ;
#82406 = VECTOR ( 'NONE', #92975, 1000.000000000000114 ) ;
#82408 = ORIENTED_EDGE ( 'NONE', *, *, #41367, .F. ) ;
#82407 = CARTESIAN_POINT ( 'NONE',  ( 168.2356071464602962, 248.8554872198452301, 6.669745218284529820 ) ) ;
#82409 = CARTESIAN_POINT ( 'NONE',  ( -3.441976700948170542, 175.4865022471903160, -10.00000000000009592 ) ) ;
#82410 = CARTESIAN_POINT ( 'NONE',  ( 37.07881409725408162, 81.27343214090025469, 59.99999999999999289 ) ) ;
#82411 = CARTESIAN_POINT ( 'NONE',  ( 188.3691292746556769, 260.5545915045569245, 2.351640140481156216 ) ) ;
#82412 = CARTESIAN_POINT ( 'NONE',  ( 160.7870188850188526, 282.4993610488249942, -6.291640665936681032 ) ) ;
#82413 = DIRECTION ( 'NONE',  ( -1.000000000000000000, 0.000000000000000000, 0.000000000000000000 ) ) ;
#82414 = CARTESIAN_POINT ( 'NONE',  ( 157.4627203480516755, 258.4629190429250798, 16.86169483958236626 ) ) ;
#82415 = CARTESIAN_POINT ( 'NONE',  ( 84.78442088202375260, 42.33400169264517388, 1.646337173112248697 ) ) ;
#82416 = CARTESIAN_POINT ( 'NONE',  ( 88.20386072652870268, 44.20680737956164563, -1.789751738150168636 ) ) ;
#82417 = VECTOR ( 'NONE', #86357, 1000.000000000000000 ) ;
#82418 = VERTEX_POINT ( 'NONE', #10256 ) ;
#82419 = CARTESIAN_POINT ( 'NONE',  ( 181.5093725072136976, 271.2422899577236421, -15.97233562208454138 ) ) ;
#82420 = CARTESIAN_POINT ( 'NONE',  ( 76.47588893644459063, 61.71057517685051153, -15.49423374570369205 ) ) ;
#82421 = ORIENTED_EDGE ( 'NONE', *, *, #54175, .T. ) ;
#82422 = CARTESIAN_POINT ( 'NONE',  ( 158.4995706392118393, 280.6444534788661258, 8.122523594373102895 ) ) ;
#82423 = DIRECTION ( 'NONE',  ( 0.8660254037844385966, 0.5000000000000002220, 7.511572993685832627E-16 ) ) ;
#82424 = CARTESIAN_POINT ( 'NONE',  ( 164.1107196200280782, 246.3988908818576249, -7.889078953360578517 ) ) ;
#82425 = CARTESIAN_POINT ( 'NONE',  ( 191.4420812244453600, 260.8157448279923187, -1.331758356259544085 ) ) ;
#82426 = CARTESIAN_POINT ( 'NONE',  ( 164.8178548836487778, 274.1146863845406187, 15.79208962134384642 ) ) ;
#82428 = CARTESIAN_POINT ( 'NONE',  ( 88.45605923504750479, 44.01628325393264163, 2.215908606781749501 ) ) ;
#82427 = CARTESIAN_POINT ( 'NONE',  ( -5.399728507075681527, 173.8149278399160949, -9.188101187500095079 ) ) ;
#82429 = AXIS2_PLACEMENT_3D ( 'NONE', #55959, #8394, #7902 ) ;
#82430 = CARTESIAN_POINT ( 'NONE',  ( 203.3947719899915683, 270.0274960689384898, 5.925299578284906055 ) ) ;
#82431 = VERTEX_POINT ( 'NONE', #72062 ) ;
#82432 = PRODUCT_DEFINITION_SHAPE ( 'NONE', 'NONE',  #57543 ) ;
#82433 = ORIENTED_EDGE ( 'NONE', *, *, #63334, .F. ) ;
#82434 = DIRECTION ( 'NONE',  ( 0.000000000000000000, -0.000000000000000000, -1.000000000000000000 ) ) ;
#82435 = CARTESIAN_POINT ( 'NONE',  ( 189.9728169475564528, 273.9113149598638870, -15.63390733120380638 ) ) ;
#82436 = B_SPLINE_CURVE_WITH_KNOTS ( 'NONE', 3,
 ( #36561, #20899, #7155, #83205 ),
 .UNSPECIFIED., .F., .F.,
 ( 4, 4 ),
 ( 0.000000000000000000, 0.003361958963760078647 ),
 .UNSPECIFIED. ) ;
#82437 = CARTESIAN_POINT ( 'NONE',  ( 85.53835401965352503, 48.98340217412621911, -12.70221784291844891 ) ) ;
#82438 = CARTESIAN_POINT ( 'NONE',  ( 175.4168235025557578, 290.8539856576853708, 2.566641252103732285 ) ) ;
#82439 = CARTESIAN_POINT ( 'NONE',  ( 153.4389798490260262, 264.8828863703868137, 16.68923469758090761 ) ) ;
#82440 = CARTESIAN_POINT ( 'NONE',  ( 71.78811623112386542, 71.82131630954249601, 4.652117579582786711 ) ) ;
#82441 = CARTESIAN_POINT ( 'NONE',  ( 193.8003511027313550, 288.1208047801705447, 17.19107869180001913 ) ) ;
#82442 = CARTESIAN_POINT ( 'NONE',  ( 11.65032017781297036, 177.5333772461660544, 9.188101187500095079 ) ) ;
#82443 = CARTESIAN_POINT ( 'NONE',  ( 103.0163473728362504, 218.0327760586659451, 1.948934522072303157E-15 ) ) ;
#82444 = CARTESIAN_POINT ( 'NONE',  ( 87.91725590613566510, 44.21674671100767284, -4.392329086374235025 ) ) ;
#82445 = CARTESIAN_POINT ( 'NONE',  ( 180.4917861999344950, 255.8997540221662916, -2.348914290984229325 ) ) ;
#82446 = CARTESIAN_POINT ( 'NONE',  ( 78.70313684180190705, 54.56738927272936479, 15.99217558139294582 ) ) ;
#82447 = CARTESIAN_POINT ( 'NONE',  ( 178.2349067178215307, 283.5087980138422381, -14.56972715175360733 ) ) ;
#82448 = EDGE_CURVE ( 'NONE', #68842, #15749, #2661, .T. ) ;
#82449 = CARTESIAN_POINT ( 'NONE',  ( 79.66253929351360341, 53.73098452899868249, -15.77044947192900537 ) ) ;
#82450 = CARTESIAN_POINT ( 'NONE',  ( 47.89168550319194395, 74.68847913791599069, -10.00000000000000000 ) ) ;
#82451 = CARTESIAN_POINT ( 'NONE',  ( 180.8580557430661315, 273.1824778245191396, 17.46595093170893520 ) ) ;
#82452 = CARTESIAN_POINT ( 'NONE',  ( 194.9757425430702824, 292.9391030023704161, -15.21392314336593365 ) ) ;
#82453 = B_SPLINE_CURVE_WITH_KNOTS ( 'NONE', 3,
 ( #4418, #89573, #36308, #75839, #97163, #66226, #27728, #59088, #59595, #5918, #50510, #12534, #52019, #21623, #6426, #20631, #51514, #42889, #43905, #74845, #90572, #83452, #20135, #36807, #67719, #98643, #5425, #29226, #58598, #89097, #43406, #74351, #4939, #28721, #60094, #66711 ),
 .UNSPECIFIED., .F., .F.,
 ( 4, 2, 2, 2, 2, 2, 2, 2, 2, 2, 2, 2, 2, 2, 2, 2, 2, 4 ),
 ( 0.0009418892082754573266, 0.001034195886821434552, 0.001126502565367411886, 0.001311115922459314947, 0.001680342636643120851, 0.002418796065010804866, 0.003895702921746029782, 0.004634156350113681488, 0.005003383064297432098, 0.005372609778481181840, 0.005418763117754132885, 0.005464916457027083063, 0.005511069796300034108, 0.005557223135572984286, 0.005741836492664717344, 0.006111063206848219888, 0.006480289921031722432, 0.006849516635215224108 ),
 .UNSPECIFIED. ) ;
#82454 = FACE_OUTER_BOUND ( 'NONE', #94686, .T. ) ;
#82455 = CARTESIAN_POINT ( 'NONE',  ( 193.6585565783151424, 265.7726264491872143, 7.804970366182538477 ) ) ;
#82456 = CARTESIAN_POINT ( 'NONE',  ( 18.55511606660780899, 34.21091486745861232, -1.111400068045478839E-16 ) ) ;
#82457 = CARTESIAN_POINT ( 'NONE',  ( 162.3075208383741312, 251.8437974874645420, -12.94720210134591376 ) ) ;
#82458 = LINE ( 'NONE', #83931, #75621 ) ;
#82459 = CARTESIAN_POINT ( 'NONE',  ( 175.7396758166374013, 265.4884659434268883, -15.79124167090947850 ) ) ;
#82460 = EDGE_CURVE ( 'NONE', #3492, #79294, #30983, .T. ) ;
#82461 = CARTESIAN_POINT ( 'NONE',  ( 75.84410613756948294, 226.8464784336661353, 1.353441290958777327E-15 ) ) ;
#82462 = CARTESIAN_POINT ( 'NONE',  ( 4.836955906052805787, 24.83396525600387861, -2.839279412974133887 ) ) ;
#82463 = CARTESIAN_POINT ( 'NONE',  ( 68.19017624660753540, 65.83665076471868360, 10.85206676099518752 ) ) ;
#82464 = AXIS2_PLACEMENT_3D ( 'NONE', #3433, #57593, #87081 ) ;
#82465 = CARTESIAN_POINT ( 'NONE',  ( 159.0966864002964769, 259.3073909472009291, -17.37488020174250636 ) ) ;
#82467 = CARTESIAN_POINT ( 'NONE',  ( 82.35782067460354483, 41.89994089823363055, -5.292397707111204497 ) ) ;
#82466 = CARTESIAN_POINT ( 'NONE',  ( 157.1135969804030310, 258.5182628004787944, 17.19660297500358226 ) ) ;
#82468 = CARTESIAN_POINT ( 'NONE',  ( 75.65669688662353565, 65.40331689797208981, 14.28920693795837593 ) ) ;
#82469 = CARTESIAN_POINT ( 'NONE',  ( 204.5540905216327303, 275.9620748824726775, -12.79967422555914958 ) ) ;
#82470 = CARTESIAN_POINT ( 'NONE',  ( 36.57256041901661803, 33.06628583063844928, -9.188101187500006262 ) ) ;
#82471 = CARTESIAN_POINT ( 'NONE',  ( 147.0456760057551833, 275.9564134551570760, -3.678503029046952033 ) ) ;
#82472 = LINE ( 'NONE', #14986, #29673 ) ;
#82473 = VERTEX_POINT ( 'NONE', #10756 ) ;
#82474 = CARTESIAN_POINT ( 'NONE',  ( 28.47099635789628280, 18.29860640527293114, -2.839279412974138328 ) ) ;
#82475 = FACE_OUTER_BOUND ( 'NONE', #32268, .T. ) ;
#82476 = CARTESIAN_POINT ( 'NONE',  ( 192.9633865298379476, 296.4246058602058156, -11.85717392250713864 ) ) ;
#82477 = DIRECTION ( 'NONE',  ( 0.000000000000000000, -0.000000000000000000, -1.000000000000000000 ) ) ;
#82478 = CARTESIAN_POINT ( 'NONE',  ( 70.96223225445140770, 61.14671028016761056, 15.00175667792790968 ) ) ;
#82479 = CARTESIAN_POINT ( 'NONE',  ( 198.5612432604688991, 286.7288335892616260, 18.30793681285053509 ) ) ;
#82480 = CARTESIAN_POINT ( 'NONE',  ( 183.8210692855788864, 257.9504670327482927, 6.873620218444065344 ) ) ;
#82481 = CARTESIAN_POINT ( 'NONE',  ( 72.58717870133969541, 71.54427304635605367, 5.456046482779852269 ) ) ;
#82482 = AXIS2_PLACEMENT_3D ( 'NONE', #11678, #58732, #65357 ) ;
#82484 =( BOUNDED_CURVE ( )  B_SPLINE_CURVE ( 2, ( #99208, #85024, #15568, #46471, #62168, #23669, #46992, #77401, #69783 ),
 .UNSPECIFIED., .F., .T. ) 
 B_SPLINE_CURVE_WITH_KNOTS ( ( 3, 2, 2, 2, 3 ),
 ( 0.4233870967741935609, 0.4247311827956989361, 0.4274193548387096864, 0.4301075268817204367, 0.4314516129032258118 ),
 .UNSPECIFIED. ) 
 CURVE ( )  GEOMETRIC_REPRESENTATION_ITEM ( )  RATIONAL_B_SPLINE_CURVE ( ( 0.9330127018922194093, 0.9330127018922194093, 1.000000000000000000, 0.8660254037844387076, 1.000000000000000000, 0.8660254037844387076, 1.000000000000000000, 0.9330127018922194093, 0.9330127018922194093 ) ) 
 REPRESENTATION_ITEM ( '' )  );
#82483 = CARTESIAN_POINT ( 'NONE',  ( 139.4522149234842061, 257.9865022471903444, -10.00000000000009415 ) ) ;
#82485 = CARTESIAN_POINT ( 'NONE',  ( 88.25688461590929990, 44.25163671709261592, -1.880183453705753127 ) ) ;
#82486 = ORIENTED_EDGE ( 'NONE', *, *, #910, .F. ) ;
#82487 = CARTESIAN_POINT ( 'NONE',  ( 84.14312167556933275, 48.98415679381830756, 0.000000000000000000 ) ) ;
#82488 = B_SPLINE_SURFACE_WITH_KNOTS ( 'NONE', 3, 1, ( 
 ( #13676, #50663 ),
 ( #43047, #12187 ),
 ( #71630, #2225 ),
 ( #45052, #75476 ),
 ( #75992, #67866 ),
 ( #21757, #77474 ),
 ( #8068, #7053 ),
 ( #53642, #6061 ),
 ( #23244, #6569 ),
 ( #30359, #45541 ),
 ( #29860, #30859 ),
 ( #84597, #15135 ),
 ( #46032, #76949 ),
 ( #37442, #7549 ),
 ( #60730, #54131 ),
 ( #61744, #38441 ),
 ( #31351, #83599 ),
 ( #98788, #92693 ),
 ( #85094, #15640 ),
 ( #84113, #46537 ),
 ( #69355, #38943 ),
 ( #61244, #91197 ),
 ( #36955, #99768 ),
 ( #52644, #29370 ),
 ( #14165, #69848 ),
 ( #461, #14665 ),
 ( #60236, #92210 ),
 ( #62234, #37934 ),
 ( #100274, #76473 ),
 ( #93186, #22765 ),
 ( #23741, #68352 ),
 ( #68847, #54635 ),
 ( #85614, #16157 ),
 ( #22255, #99277 ) ),
 .UNSPECIFIED., .T., .F., .F.,
 ( 4, 2, 2, 2, 2, 2, 2, 2, 2, 2, 2, 2, 2, 2, 2, 2, 4 ),
 ( 2, 2 ),
 ( 0.000000000000000000, 0.06250000000000000000, 0.1250000000000000000, 0.1875000000000000000, 0.2500000000000000000, 0.3125000000000000000, 0.3750000000000000000, 0.4375000000000000000, 0.5000000000000000000, 0.5625000000000000000, 0.6250000000000000000, 0.6875000000000000000, 0.7500000000000000000, 0.8125000000000000000, 0.8750000000000000000, 0.9375000000000000000, 1.000000000000000000 ),
 ( 0.000000000000000000, 1.000000000000000000 ),
 .UNSPECIFIED. ) ;
#82489 = ORIENTED_EDGE ( 'NONE', *, *, #87771, .F. ) ;
#82490 = DIRECTION ( 'NONE',  ( 0.000000000000000000, 0.000000000000000000, 1.000000000000000000 ) ) ;
#82491 = CARTESIAN_POINT ( 'NONE',  ( 81.75211762113612224, 42.34667925476468042, -8.001231807219630454 ) ) ;
#82492 = CARTESIAN_POINT ( 'NONE',  ( 184.1800646242121786, 291.9084716066498686, -10.70019971855618834 ) ) ;
#82493 = ORIENTED_EDGE ( 'NONE', *, *, #84418, .F. ) ;
#82494 = CARTESIAN_POINT ( 'NONE',  ( 88.05624235485146301, 44.55787864911079765, -5.145732200269208079 ) ) ;
#82495 = CARTESIAN_POINT ( 'NONE',  ( 194.1714003930522949, 280.7953645453140439, -17.43791269142986877 ) ) ;
#82496 = CARTESIAN_POINT ( 'NONE',  ( 88.15573124791052351, 44.39703741701313078, -4.524867680024760475 ) ) ;
#82497 = CARTESIAN_POINT ( 'NONE',  ( 153.4361244163197000, 264.8878321249116539, -17.23169627811277493 ) ) ;
#82498 = CARTESIAN_POINT ( 'NONE',  ( -78.24550368024017644, 54.29179893118896416, -10.00000000000000000 ) ) ;
#82499 = CARTESIAN_POINT ( 'NONE',  ( 32.39821438149254362, 40.74646525600392977, 2.839279412974139660 ) ) ;
#82500 = DIRECTION ( 'NONE',  ( 1.000000000000000000, 0.000000000000000000, 0.000000000000000000 ) ) ;
#82501 = ADVANCED_FACE ( 'NONE', ( #49744 ), #28785, .F. ) ;
#82502 = CARTESIAN_POINT ( 'NONE',  ( 164.6328405706842943, 274.5024593735440135, 14.72560760841240679 ) ) ;
#82503 =( BOUNDED_CURVE ( )  B_SPLINE_CURVE ( 2, ( #61939, #7253, #22950, #23445, #93398, #54851, #54334, #93906, #32043, #39632, #70553, #85306, #31547 ),
 .UNSPECIFIED., .F., .T. ) 
 B_SPLINE_CURVE_WITH_KNOTS ( ( 3, 2, 2, 2, 2, 2, 3 ),
 ( 0.1625000000000000056, 0.1650000000000000078, 0.1700000000000000122, 0.1749999999999999889, 0.1799999999999999933, 0.1849999999999999978, 0.1875000000000000000 ),
 .UNSPECIFIED. ) 
 CURVE ( )  GEOMETRIC_REPRESENTATION_ITEM ( )  RATIONAL_B_SPLINE_CURVE ( ( 0.9755282581475768211, 0.9755282581475768211, 1.000000000000000000, 0.9510565162951535312, 1.000000000000000000, 0.9510565162951535312, 1.000000000000000000, 0.9510565162951535312, 1.000000000000000000, 0.9510565162951535312, 1.000000000000000000, 0.9755282581475768211, 0.9755282581475768211 ) ) 
 REPRESENTATION_ITEM ( '' )  );
#82504 = CARTESIAN_POINT ( 'NONE',  ( 49.80235952159635815, 85.00000000000000000, 10.00000000000000000 ) ) ;
#82505 = VERTEX_POINT ( 'NONE', #23315 ) ;
#82506 = ORIENTED_EDGE ( 'NONE', *, *, #89498, .T. ) ;
#82507 = CARTESIAN_POINT ( 'NONE',  ( 182.8497346172418077, 296.2091331152387852, 0.3117783270952969032 ) ) ;
#82509 = LINE ( 'NONE', #66741, #36239 ) ;
#82508 = CARTESIAN_POINT ( 'NONE',  ( 204.9004517216375518, 275.7490024547470853, 14.55104398969427670 ) ) ;
#82510 = CARTESIAN_POINT ( 'NONE',  ( 85.94199290331987129, 48.36193870280315110, 12.04004775853120357 ) ) ;
#82511 = CYLINDRICAL_SURFACE ( 'NONE', #5302, 70.00000000000002842 ) ;
#82512 = CARTESIAN_POINT ( 'NONE',  ( 71.11649605149564479, 61.92534502158513021, -14.18178967544274371 ) ) ;
#82513 = DIRECTION ( 'NONE',  ( -0.000000000000000000, -0.000000000000000000, -1.000000000000000000 ) ) ;
#82514 = CARTESIAN_POINT ( 'NONE',  ( 171.0161179014379798, 287.7422477288193932, -4.570675186747868324 ) ) ;
#82515 = ADVANCED_FACE ( 'NONE', ( #94265 ), #15713, .F. ) ;
#82516 = CARTESIAN_POINT ( 'NONE',  ( 77.16944367370705038, 62.93815415716151307, -15.28450044950025877 ) ) ;
#82517 = DIRECTION ( 'NONE',  ( -0.4999999999999987788, 0.8660254037844392627, 0.000000000000000000 ) ) ;
#82518 = CARTESIAN_POINT ( 'NONE',  ( 107.1028179730028285, 223.4548013555409796, -4.594050593750042211 ) ) ;
#82519 = ORIENTED_EDGE ( 'NONE', *, *, #91733, .F. ) ;
#82520 = CARTESIAN_POINT ( 'NONE',  ( -0.4807448425718762741, 158.9824982072973683, 3.021315404115420679E-15 ) ) ;
#82521 = CARTESIAN_POINT ( 'NONE',  ( 179.4404154152157105, 291.3709498135804097, -10.08759257512885199 ) ) ;
#82522 = VERTEX_POINT ( 'NONE', #15209 ) ;
#82523 = ORIENTED_EDGE ( 'NONE', *, *, #36387, .T. ) ;
#82524 = CARTESIAN_POINT ( 'NONE',  ( 87.18493082415903928, 46.24780984919522808, -8.452580536463766947 ) ) ;
#82525 = CYLINDRICAL_SURFACE ( 'NONE', #68948, 17.82106496071139645 ) ;
#82526 = CARTESIAN_POINT ( 'NONE',  ( 157.2464636617698375, 258.2881309577184652, 18.14284729738657731 ) ) ;
#82527 = CARTESIAN_POINT ( 'NONE',  ( 206.2809287719926488, 273.3579460648492159, -10.70911012174624588 ) ) ;
#82528 = DIRECTION ( 'NONE',  ( -1.000000000000000000, -1.110223024625156343E-15, 0.000000000000000000 ) ) ;
#82529 = VERTEX_POINT ( 'NONE', #23815 ) ;
#82530 = VERTEX_POINT ( 'NONE', #54202 ) ;
#82531 = CARTESIAN_POINT ( 'NONE',  ( -17.42236680055705023, 149.2012482093457777, 0.000000000000000000 ) ) ;
#82532 = VERTEX_POINT ( 'NONE', #85170 ) ;
#82533 = VECTOR ( 'NONE', #30502, 1000.000000000000000 ) ;
#82534 = CARTESIAN_POINT ( 'NONE',  ( 191.7168775847123641, 264.3120571150079172, -7.888889122128393439 ) ) ;
#82535 = FACE_OUTER_BOUND ( 'NONE', #43313, .T. ) ;
#82536 = CARTESIAN_POINT ( 'NONE',  ( 83.08198603362329493, 46.51316202230789543, 11.28621070833093931 ) ) ;
#82538 = CARTESIAN_POINT ( 'NONE',  ( 69.39572770259547951, 62.82886628838792120, -13.71575758985256499 ) ) ;
#82537 = CARTESIAN_POINT ( 'NONE',  ( 141.5001777056247931, 246.3768266524160140, 9.188101187500098632 ) ) ;
#82539 = CYLINDRICAL_SURFACE ( 'NONE', #57563, 2.471954595299370006 ) ;
#82540 = ORIENTED_EDGE ( 'NONE', *, *, #43566, .F. ) ;
#82541 = CARTESIAN_POINT ( 'NONE',  ( 190.3791419447713906, 300.9006487807255326, -5.688668718458480988 ) ) ;
#82542 = CARTESIAN_POINT ( 'NONE',  ( 82.08601192207028419, 50.00142036091599351, 14.02437814591130127 ) ) ;
#82543 = CARTESIAN_POINT ( 'NONE',  ( 82.40574091212634755, 41.31496069167722851, -3.377884205285225594 ) ) ;
#82544 = CARTESIAN_POINT ( 'NONE',  ( 192.8798198427039665, 270.9848878250640496, 14.54342281811944027 ) ) ;
#82545 = CARTESIAN_POINT ( 'NONE',  ( 178.2267749612124135, 285.2995087623953623, 13.03308732619244736 ) ) ;
#82546 = FACE_OUTER_BOUND ( 'NONE', #68139, .T. ) ;
#82547 = CARTESIAN_POINT ( 'NONE',  ( 198.7849384794873231, 282.4363158398074916, -17.34911472281661204 ) ) ;
#82548 = CARTESIAN_POINT ( 'NONE',  ( 72.04273812837080015, 59.28583566120335036, 15.84548535902080246 ) ) ;
#82549 = CARTESIAN_POINT ( 'NONE',  ( 80.65449906233159538, 53.35338484752109167, 15.59324704275317863 ) ) ;
#82550 = CARTESIAN_POINT ( 'NONE',  ( 68.38943100534879704, 69.90328650375072073, -2.303593894763091399 ) ) ;
#82551 = CARTESIAN_POINT ( 'NONE',  ( 60.95981515367195414, 199.8768266524160140, 9.188101187500098632 ) ) ;
#82552 = LINE ( 'NONE', #53576, #54083 ) ;
#82553 = CARTESIAN_POINT ( 'NONE',  ( 77.78993031024410243, 61.70844822385715389, 16.06828208845740136 ) ) ;
#82554 = CARTESIAN_POINT ( 'NONE',  ( 162.8480293090835005, 248.5859346546387769, -9.753154585358942086 ) ) ;
#82555 = B_SPLINE_CURVE_WITH_KNOTS ( 'NONE', 3,
 ( #20786, #34960, #5078, #65860 ),
 .UNSPECIFIED., .F., .F.,
 ( 4, 4 ),
 ( 0.008944368131606707586, 0.01511703026669370883 ),
 .UNSPECIFIED. ) ;
#82556 = CARTESIAN_POINT ( 'NONE',  ( 196.3345161992979229, 288.9417725351840431, -17.15029287748203757 ) ) ;
#82557 = VECTOR ( 'NONE', #34697, 1000.000000000000114 ) ;
#82558 = ADVANCED_FACE ( 'NONE', ( #78040 ), #61810, .T. ) ;
#82559 = CARTESIAN_POINT ( 'NONE',  ( 57.06414817410224316, 218.1868197944957330, -17.47570218321533631 ) ) ;
#82560 = CARTESIAN_POINT ( 'NONE',  ( 50.27371054362190961, 89.86549102125590593, -10.00000000000000000 ) ) ;
#82561 = CARTESIAN_POINT ( 'NONE',  ( 174.3943357370370677, 284.3386801424128976, 13.92617907230369312 ) ) ;
#82562 = ADVANCED_FACE ( 'NONE', ( #24821 ), #16229, .T. ) ;
#82563 = DIRECTION ( 'NONE',  ( 1.000000000000000000, 0.000000000000000000, -0.000000000000000000 ) ) ;
#82564 = CARTESIAN_POINT ( 'NONE',  ( 149.9060791885465846, 273.0020498124315509, -11.57482514211843849 ) ) ;
#82565 = CARTESIAN_POINT ( 'NONE',  ( 195.9713281756800427, 291.2146981034049418, 17.52210387885178022 ) ) ;
#82566 = LINE ( 'NONE', #13129, #96456 ) ;
#82567 = CARTESIAN_POINT ( 'NONE',  ( 20.20266813594930611, 170.2202760586659736, -5.415160957724236172E-17 ) ) ;
#82568 = CARTESIAN_POINT ( 'NONE',  ( 48.66388509341562241, 192.2365022471902023, -10.00000000000009237 ) ) ;
#82569 = ORIENTED_EDGE ( 'NONE', *, *, #95988, .F. ) ;
#82570 = EDGE_CURVE ( 'NONE', #50852, #16524, #14523, .T. ) ;
#82571 = CARTESIAN_POINT ( 'NONE',  ( 196.3341081413628899, 290.5863447708742342, 16.12390540996472410 ) ) ;
#82572 = CARTESIAN_POINT ( 'NONE',  ( 199.3468182655126100, 277.7844241296513701, 15.39279173571824266 ) ) ;
#82573 = CYLINDRICAL_SURFACE ( 'NONE', #38597, 10.00000000000010658 ) ;
#82574 = CARTESIAN_POINT ( 'NONE',  ( 71.79738241951251609, 72.08784563739403950, -1.676743678701877238 ) ) ;
#82575 = CARTESIAN_POINT ( 'NONE',  ( 42.23166870106845039, 201.3149278399161233, 9.188101187500093303 ) ) ;
#82576 = CARTESIAN_POINT ( 'NONE',  ( 87.22595043061240005, 46.05622627631750987, 8.811080105847633348 ) ) ;
#82577 = CARTESIAN_POINT ( 'NONE',  ( 199.1944722252943905, 285.6320488493591938, -18.17555833707144686 ) ) ;
#82578 = CARTESIAN_POINT ( 'NONE',  ( 190.1607982559816890, 301.2788311432216233, -4.972636536415983244 ) ) ;
#82579 = CARTESIAN_POINT ( 'NONE',  ( 12.16146256644911539, 9.947547579820877672, 5.678558825948272215 ) ) ;
#82580 = CARTESIAN_POINT ( 'NONE',  ( 199.7244443182572979, 267.8419476567416950, -6.547629676957067879 ) ) ;
#82581 = CARTESIAN_POINT ( 'NONE',  ( 193.6881582770097054, 289.9360790452486754, 16.66172979718519898 ) ) ;
#82582 = CARTESIAN_POINT ( 'NONE',  ( 176.9920332807921568, 275.4403497717407276, 17.58608646401103215 ) ) ;
#82583 = DIRECTION ( 'NONE',  ( 0.4999999999999998890, -0.8660254037844385966, 0.000000000000000000 ) ) ;
#82584 = CARTESIAN_POINT ( 'NONE',  ( 67.57193167581756654, 67.79594878957911419, -6.919506841086756843 ) ) ;
#82585 = CARTESIAN_POINT ( 'NONE',  ( 163.3377027424940025, 255.8893630163459534, -14.85816214141254576 ) ) ;
#82586 = EDGE_CURVE ( 'NONE', #59744, #50323, #3327, .T. ) ;
#82587 = CARTESIAN_POINT ( 'NONE',  ( -13.76211276271269668, 162.8615022471902591, 0.000000000000000000 ) ) ;
#82588 = CARTESIAN_POINT ( 'NONE',  ( 104.9555363394041336, 224.7365022471902307, 10.00000000000009592 ) ) ;
#82589 = CARTESIAN_POINT ( 'NONE',  ( 200.1102648775588193, 284.0458494464393198, 17.54251420653697835 ) ) ;
#82590 = CARTESIAN_POINT ( 'NONE',  ( 164.9127185089346028, 270.4126442277538445, -16.66829531255166330 ) ) ;
#82591 = ORIENTED_EDGE ( 'NONE', *, *, #49742, .F. ) ;
#82592 = CARTESIAN_POINT ( 'NONE',  ( 54.35602435405059651, 208.3149278399161233, -9.188101187500095079 ) ) ;
#82593 = VERTEX_POINT ( 'NONE', #24331 ) ;
#82594 = CARTESIAN_POINT ( 'NONE',  ( -22.42236680055709641, 157.8615022471902591, 0.000000000000000000 ) ) ;
#82595 = CARTESIAN_POINT ( 'NONE',  ( 175.0296968597178306, 264.6864531019056699, -16.70299667166197466 ) ) ;
#82597 = CARTESIAN_POINT ( 'NONE',  ( -48.71813016832984289, 30.75580926756359901, 10.00000000000000000 ) ) ;
#82596 = AXIS2_PLACEMENT_3D ( 'NONE', #96164, #42888, #95686 ) ;
#82598 = ORIENTED_EDGE ( 'NONE', *, *, #38829, .F. ) ;
#82599 = DIRECTION ( 'NONE',  ( 0.8660254037844379305, 0.5000000000000011102, 0.000000000000000000 ) ) ;
#82600 = CARTESIAN_POINT ( 'NONE',  ( 79.19871682019896753, 45.77535205480253921, -13.02187134424031534 ) ) ;
#82601 = CARTESIAN_POINT ( 'NONE',  ( 155.7716105177659927, 262.8426515368366267, -17.72795275872529430 ) ) ;
#82602 = CARTESIAN_POINT ( 'NONE',  ( 33.49697393745356777, 27.84335787977765264, 9.188101187500006262 ) ) ;
#82603 = CARTESIAN_POINT ( 'NONE',  ( 189.3285837834738174, 265.1763588534336122, 10.46335708403672626 ) ) ;
#82604 = CARTESIAN_POINT ( 'NONE',  ( 196.2421909983451940, 290.7455499326673021, -17.31908925000307065 ) ) ;
#82605 = CARTESIAN_POINT ( 'NONE',  ( 157.2014865449050660, 258.3660336093062142, 16.87758714513496017 ) ) ;
#82606 = ORIENTED_EDGE ( 'NONE', *, *, #68326, .F. ) ;
#82607 = CARTESIAN_POINT ( 'NONE',  ( 17.99393647837114329, 33.49540643055186706, 3.479690158560446702E-15 ) ) ;
#82608 = CARTESIAN_POINT ( 'NONE',  ( 76.40434453536583703, 62.66765977773136598, 15.20766477907509184 ) ) ;
#82609 = CARTESIAN_POINT ( 'NONE',  ( 71.52184754477866591, 70.29122656255715640, -6.759684521044225569 ) ) ;
#82610 = CARTESIAN_POINT ( 'NONE',  ( 14.65590419365400798, 24.16454794089040448, -10.00000000000000355 ) ) ;
#82611 = ADVANCED_FACE ( 'NONE', ( #46615 ), #76542, .T. ) ;
#82612 = EDGE_CURVE ( 'NONE', #50052, #20654, #90371, .T. ) ;
#82613 = ORIENTED_EDGE ( 'NONE', *, *, #71260, .T. ) ;
#82614 = CARTESIAN_POINT ( 'NONE',  ( -2.073866539663252073, 26.60322154129610794, -10.00000000000000000 ) ) ;
#82615 = CARTESIAN_POINT ( 'NONE',  ( 166.9403103669216648, 261.3810178180994512, 16.77684693550508754 ) ) ;
#82616 = CARTESIAN_POINT ( 'NONE',  ( 206.7893622945242385, 272.4773133715531230, -10.52881283832460291 ) ) ;
#82617 = CIRCLE ( 'NONE', #27556, 60.00000000000002132 ) ;
#82618 = ORIENTED_EDGE ( 'NONE', *, *, #23026, .F. ) ;
#82619 = ADVANCED_FACE ( 'NONE', ( #69426 ), #67612, .T. ) ;
#82621 = CARTESIAN_POINT ( 'NONE',  ( -19.65312891409030271, 93.06504152958497400, 10.00000000000000888 ) ) ;
#82620 = CARTESIAN_POINT ( 'NONE',  ( 71.46351114784202707, 64.97172176451604741, 13.12417365010213643 ) ) ;
#82622 = CARTESIAN_POINT ( 'NONE',  ( 71.21786832307518011, 71.42957135316279960, -4.816066736783382929 ) ) ;
#82623 = VERTEX_POINT ( 'NONE', #48640 ) ;
#82624 = CARTESIAN_POINT ( 'NONE',  ( 65.82417520554362511, 68.94067023863627242, -2.334285861092879166 ) ) ;
#82625 = CARTESIAN_POINT ( 'NONE',  ( 159.2554912534056939, 254.8083930951974878, 16.49944922174842432 ) ) ;
#82626 = CYLINDRICAL_SURFACE ( 'NONE', #43491, 10.00000000000010658 ) ;
#82627 = CARTESIAN_POINT ( 'NONE',  ( 164.5858729372050675, 265.2716139154605344, -16.65117712114545512 ) ) ;
#82628 = CARTESIAN_POINT ( 'NONE',  ( 124.8288415870092791, 249.0024278399161517, -9.188101187500093303 ) ) ;
#82629 = EDGE_CURVE ( 'NONE', #48601, #30838, #72955, .T. ) ;
#82630 = CARTESIAN_POINT ( 'NONE',  ( 114.3374782137354799, 243.4865022471903160, 10.00000000000009415 ) ) ;
#82631 = ORIENTED_EDGE ( 'NONE', *, *, #5964, .F. ) ;
#82632 = CARTESIAN_POINT ( 'NONE',  ( 174.0587387296342854, 265.5211078058665066, 16.69357511762551383 ) ) ;
#82633 = CARTESIAN_POINT ( 'NONE',  ( 30.80155721116056355, 46.36891074996812989, -10.00000000000000000 ) ) ;
#82634 = CARTESIAN_POINT ( 'NONE',  ( 36.00834752015899198, 180.0494855054051868, -2.679491924311248496 ) ) ;
#82635 = VERTEX_POINT ( 'NONE', #87206 ) ;
#82636 = CARTESIAN_POINT ( 'NONE',  ( 160.4722622339176041, 253.9870023085891830, 15.41922939303313811 ) ) ;
#82637 = VERTEX_POINT ( 'NONE', #79575 ) ;
#82638 = ORIENTED_EDGE ( 'NONE', *, *, #18775, .T. ) ;
#82639 = EDGE_CURVE ( 'NONE', #41570, #17465, #72455, .T. ) ;
#82640 = CARTESIAN_POINT ( 'NONE',  ( 159.9628729326222754, 253.5831720864507588, 15.75051413866357386 ) ) ;
#82641 = CARTESIAN_POINT ( 'NONE',  ( 15.36455789491911794, 32.15369338429142942, 10.00000000000000000 ) ) ;
#82642 = ADVANCED_FACE ( 'NONE', ( #65325 ), #13440, .T. ) ;
#82643 = CARTESIAN_POINT ( 'NONE',  ( 68.80799682758592439, 210.5333772461660544, 9.188101187500095079 ) ) ;
#82644 = CARTESIAN_POINT ( 'NONE',  ( -30.04356256989597540, 94.99361293546084539, 12.66716928022279909 ) ) ;
#82645 = CARTESIAN_POINT ( 'NONE',  ( 176.9376637958658591, 282.2927093116995820, 15.89557571866741981 ) ) ;
#82646 = CARTESIAN_POINT ( 'NONE',  ( 154.9344967692067598, 262.2925750810547356, 17.30210568643136781 ) ) ;
#82647 = CARTESIAN_POINT ( 'NONE',  ( 175.7384777704949386, 278.2480916999407441, 15.65549428786727759 ) ) ;
#82648 = ORIENTED_EDGE ( 'NONE', *, *, #95017, .F. ) ;
#82649 = CARTESIAN_POINT ( 'NONE',  ( 73.50385191007055141, 63.43673688022664692, -14.15219903627441944 ) ) ;
#82650 = CARTESIAN_POINT ( 'NONE',  ( 87.87264940252229906, 43.95799710625667700, -0.8674386733748262746 ) ) ;
#82651 = CARTESIAN_POINT ( 'NONE',  ( 201.2949053258274148, 281.9939920013367782, -18.04004790210578335 ) ) ;
#82652 = CARTESIAN_POINT ( 'NONE',  ( 203.5629025532486196, 278.0657055720176913, -15.85226727704602823 ) ) ;
#82653 = VERTEX_POINT ( 'NONE', #29321 ) ;
#82654 = CARTESIAN_POINT ( 'NONE',  ( 72.94880756138117306, 69.80684942108813118, -8.830661643779624370 ) ) ;
#82655 = FACE_OUTER_BOUND ( 'NONE', #97460, .T. ) ;
#82656 = CARTESIAN_POINT ( 'NONE',  ( 73.99515186948657686, 54.97541550358009488, -16.60506967685200408 ) ) ;
#82657 = CARTESIAN_POINT ( 'NONE',  ( 80.38548996768443544, 54.44962404282426149, 16.25868990910755230 ) ) ;
#82658 = CARTESIAN_POINT ( 'NONE',  ( 206.0691053506789387, 273.7248349927971844, 11.70564474658248422 ) ) ;
#82659 = CARTESIAN_POINT ( 'NONE',  ( 163.7183543885751078, 247.0784873978576854, -6.786164904910574336 ) ) ;
#82660 = CARTESIAN_POINT ( 'NONE',  ( 139.7141738582018604, 239.2202760586659736, -5.415160957724236172E-17 ) ) ;
#82661 = ORIENTED_EDGE ( 'NONE', *, *, #41742, .T. ) ;
#82662 = DIRECTION ( 'NONE',  ( -0.8098206029991052990, 0.5866775868892262213, 0.000000000000000000 ) ) ;
#82663 = CARTESIAN_POINT ( 'NONE',  ( 67.27576334028319138, 67.83911610176210161, -7.634865361317446641 ) ) ;
#82664 = DIRECTION ( 'NONE',  ( 0.000000000000000000, 0.000000000000000000, 1.000000000000000000 ) ) ;
#82665 = B_SPLINE_CURVE_WITH_KNOTS ( 'NONE', 3,
 ( #62366, #99411, #45671, #61380 ),
 .UNSPECIFIED., .F., .F.,
 ( 4, 4 ),
 ( 0.01147170345886797983, 0.01992442707605523305 ),
 .UNSPECIFIED. ) ;
#82666 = CARTESIAN_POINT ( 'NONE',  ( 72.89074862266798505, 70.83676290058953384, 7.267550809142558244 ) ) ;
#82667 = CYLINDRICAL_SURFACE ( 'NONE', #56315, 17.82106496071139645 ) ;
#82668 = DIRECTION ( 'NONE',  ( -0.000000000000000000, -0.000000000000000000, -1.000000000000000000 ) ) ;
#82669 = ORIENTED_EDGE ( 'NONE', *, *, #24798, .F. ) ;
#82670 = DIRECTION ( 'NONE',  ( -0.5866775868892349921, -0.8098206029990988597, 0.000000000000000000 ) ) ;
#82671 = CARTESIAN_POINT ( 'NONE',  ( 182.2980163133740064, 275.2725943275962095, -16.61995625180471592 ) ) ;
#82672 = CARTESIAN_POINT ( 'NONE',  ( 159.9950753608005130, 276.8117990079294373, 13.35014033362692487 ) ) ;
#82673 = CARTESIAN_POINT ( 'NONE',  ( 81.07073587917510338, 51.75993004551867926, 15.01386952398517494 ) ) ;
#82674 = CARTESIAN_POINT ( 'NONE',  ( 73.72211794458776524, 69.54036169704887982, -9.751718775917950666 ) ) ;
#82675 = CARTESIAN_POINT ( 'NONE',  ( 146.8201187048455267, 276.3470901603510015, 4.112223577763169047 ) ) ;
#82676 = B_SPLINE_CURVE_WITH_KNOTS ( 'NONE', 3,
 ( #65998, #96950, #60858, #61371, #84721, #91 ),
 .UNSPECIFIED., .F., .F.,
 ( 4, 2, 4 ),
 ( 0.02038262341263210459, 0.02494425553470808188, 0.02950588765678405917 ),
 .UNSPECIFIED. ) ;
#82677 = CARTESIAN_POINT ( 'NONE',  ( 182.9080384886626973, 280.6966867911361305, 16.99481542840181092 ) ) ;
#82678 = CARTESIAN_POINT ( 'NONE',  ( 157.2777284163744582, 258.2339788142568864, -16.82360006463426316 ) ) ;
#82679 = CARTESIAN_POINT ( 'NONE',  ( 23.46864935082044923, 158.3759306620404459, 22.50000000000001776 ) ) ;
#82680 = CARTESIAN_POINT ( 'NONE',  ( 28.12636825332733537, 17.20801979619929512, -3.090169943749474069 ) ) ;
#82681 = DIRECTION ( 'NONE',  ( -0.000000000000000000, 0.000000000000000000, 1.000000000000000000 ) ) ;
#82682 = FACE_OUTER_BOUND ( 'NONE', #81949, .T. ) ;
#82683 = CARTESIAN_POINT ( 'NONE',  ( 66.52392041426838887, 68.84470833973988135, -4.415679280545959706 ) ) ;
#82684 = CARTESIAN_POINT ( 'NONE',  ( 159.9880386575927957, 253.5395837721924863, 15.85893018594752846 ) ) ;
#82685 = CARTESIAN_POINT ( 'NONE',  ( 175.4039180538638050, 286.4985578832265105, -12.71199677751706503 ) ) ;
#82686 = CARTESIAN_POINT ( 'NONE',  ( 130.2687372006388671, 246.0177522451418497, -10.00000000000009592 ) ) ;
#82687 = CARTESIAN_POINT ( 'NONE',  ( 173.8366476056167755, 284.1819771225056002, -12.13474973978462579 ) ) ;
#82688 = ORIENTED_EDGE ( 'NONE', *, *, #65463, .T. ) ;
#82689 = EDGE_CURVE ( 'NONE', #1959, #35128, #69540, .T. ) ;
#82690 = CARTESIAN_POINT ( 'NONE',  ( 66.81157939586830707, 67.57634921264273942, -6.489721810135971936 ) ) ;
#82691 = CARTESIAN_POINT ( 'NONE',  ( 151.1699610800269511, 268.8129421616204695, -14.28929860221299286 ) ) ;
#82692 = CARTESIAN_POINT ( 'NONE',  ( 15.22267496842377099, 179.5958772461660544, -9.188101187500095079 ) ) ;
#82693 = CARTESIAN_POINT ( 'NONE',  ( 178.6505616879398985, 259.2469067511012213, -10.41651906039837527 ) ) ;
#82694 = CARTESIAN_POINT ( 'NONE',  ( 22.35053764064823767, 35.83705186507754803, 3.090169943749475401 ) ) ;
#82695 = CARTESIAN_POINT ( 'NONE',  ( 85.31220642273653709, 48.47216915277315508, 12.41700016606928259 ) ) ;
#82696 = CARTESIAN_POINT ( 'NONE',  ( 204.6075833744878878, 276.2562653119390461, -13.34672481898815910 ) ) ;
#82697 = FACE_OUTER_BOUND ( 'NONE', #58782, .T. ) ;
#82698 = LINE ( 'NONE', #7631, #96038 ) ;
#82699 = CARTESIAN_POINT ( 'NONE',  ( 170.9894030905899456, 257.8110510375899480, 14.60046632396432109 ) ) ;
#82700 = CARTESIAN_POINT ( 'NONE',  ( 178.8651605570578624, 254.1428845745818990, -4.151848116954283796 ) ) ;
#82701 = EDGE_CURVE ( 'NONE', #92094, #77711, #22364, .T. ) ;
#82702 = CARTESIAN_POINT ( 'NONE',  ( 150.2950809960438221, 270.3282789176094525, 14.12607625385173193 ) ) ;
#82703 = EDGE_CURVE ( 'NONE', #43568, #33103, #68278, .T. ) ;
#82704 = CARTESIAN_POINT ( 'NONE',  ( 47.29267820409018697, 208.1115022471903160, -5.000000000000047962 ) ) ;
#82705 = CARTESIAN_POINT ( 'NONE',  ( 181.6690914948270574, 291.8339887612885946, 9.074948012314465018 ) ) ;
#82706 = CARTESIAN_POINT ( 'NONE',  ( 148.0389988358468827, 274.2359278451201590, 7.783622668412842671 ) ) ;
#82707 = CARTESIAN_POINT ( 'NONE',  ( 22.47598482088346117, 171.5327760586659451, 1.948934522072303157E-15 ) ) ;
#82708 = CARTESIAN_POINT ( 'NONE',  ( 168.0427418980721939, 286.7126107662992922, 5.006243472136755912 ) ) ;
#82709 = CARTESIAN_POINT ( 'NONE',  ( 79.13720140929677882, 60.04739137989873399, 16.13033826897202871 ) ) ;
#82710 = CARTESIAN_POINT ( 'NONE',  ( 35.85928575902275384, 36.10171378149922106, 9.188101187500008038 ) ) ;
#82711 = LINE ( 'NONE', #36045, #90271 ) ;
#82712 = CARTESIAN_POINT ( 'NONE',  ( 179.8149668105232877, 276.9306161883004052, 16.29941506102614923 ) ) ;
#82713 = CARTESIAN_POINT ( 'NONE',  ( 188.0775634319173832, 267.1413101313072502, 14.31780989748781252 ) ) ;
#82714 = DIRECTION ( 'NONE',  ( 0.000000000000000000, 0.000000000000000000, 1.000000000000000000 ) ) ;
#82715 = CARTESIAN_POINT ( 'NONE',  ( 164.1509177496182588, 281.5495894003347530, 8.939607256454412010 ) ) ;
#82716 = CARTESIAN_POINT ( 'NONE',  ( 0.000000000000000000, 0.000000000000000000, 0.000000000000000000 ) ) ;
#82717 = CARTESIAN_POINT ( 'NONE',  ( 13.45569633750675465, 25.95586893147754282, 7.433330006724141015 ) ) ;
#82718 = CARTESIAN_POINT ( 'NONE',  ( 71.95794525336515335, 72.58301972798899726, 1.600903759350515543 ) ) ;
#82719 = CARTESIAN_POINT ( 'NONE',  ( 82.69645212816358537, 54.02937911834194296, 15.50030166553341004 ) ) ;
#82720 = DIRECTION ( 'NONE',  ( -0.000000000000000000, -0.000000000000000000, 1.000000000000000000 ) ) ;
#82721 = CARTESIAN_POINT ( 'NONE',  ( 194.1493756275458793, 294.3704124857528655, 13.94613522129020744 ) ) ;
#82722 = ORIENTED_EDGE ( 'NONE', *, *, #27823, .F. ) ;
#82723 = DIRECTION ( 'NONE',  ( -0.8660254037844387076, -0.4999999999999998890, -0.000000000000000000 ) ) ;
#82724 = CARTESIAN_POINT ( 'NONE',  ( 156.9346906984713144, 276.3858077937837834, 10.77862339299636574 ) ) ;
#82725 = CARTESIAN_POINT ( 'NONE',  ( 81.38228331523285419, 42.18052851735775732, 8.075145019535051816 ) ) ;
#82726 = ORIENTED_EDGE ( 'NONE', *, *, #27951, .T. ) ;
#82727 = CARTESIAN_POINT ( 'NONE',  ( 195.7705542948037021, 290.3450269424856742, -16.49291066975641229 ) ) ;
#82728 = DIRECTION ( 'NONE',  ( -0.8660254037844387076, -0.4999999999999998890, -0.000000000000000000 ) ) ;
#82729 = CARTESIAN_POINT ( 'NONE',  ( 66.64262941566822462, 68.29515624540186991, 4.552616485263072832 ) ) ;
#82730 = CARTESIAN_POINT ( 'NONE',  ( 155.1865148098964937, 261.8560670301561686, -16.99758927948949605 ) ) ;
#82731 = ORIENTED_EDGE ( 'NONE', *, *, #65948, .F. ) ;
#82732 = ORIENTED_EDGE ( 'NONE', *, *, #26253, .F. ) ;
#82733 = EDGE_CURVE ( 'NONE', #48909, #62608, #29301, .T. ) ;
#82735 = DIRECTION ( 'NONE',  ( -1.000000000000000000, 0.000000000000000000, 0.000000000000000000 ) ) ;
#82734 = FACE_OUTER_BOUND ( 'NONE', #65378, .T. ) ;
#82736 = CARTESIAN_POINT ( 'NONE',  ( 152.6845319923753834, 266.1896283897672220, 17.20844521882669653 ) ) ;
#82737 = ORIENTED_EDGE ( 'NONE', *, *, #85698, .F. ) ;
#82738 = CARTESIAN_POINT ( 'NONE',  ( 191.3638605175971747, 299.1950661814348678, 7.382965314423603154 ) ) ;
#82739 = CARTESIAN_POINT ( 'NONE',  ( 81.45669997382150029, 55.98862135975878118, -16.04303691645969820 ) ) ;
#82740 = CARTESIAN_POINT ( 'NONE',  ( 162.2281535785777464, 260.3593638863677597, -17.46508937750856560 ) ) ;
#82741 = VERTEX_POINT ( 'NONE', #53571 ) ;
#82742 = CARTESIAN_POINT ( 'NONE',  ( 49.42830306794131445, 81.76213237698445369, 177.5919119679930134 ) ) ;
#82743 = EDGE_CURVE ( 'NONE', #62710, #47438, #22692, .T. ) ;
#82744 = ADVANCED_FACE ( 'NONE', ( #99697 ), #13599, .T. ) ;
#82745 = CARTESIAN_POINT ( 'NONE',  ( 81.29539683307429243, 43.25976067956239035, 9.624898955646088439 ) ) ;
#82746 = ORIENTED_EDGE ( 'NONE', *, *, #1249, .F. ) ;
#82747 = CARTESIAN_POINT ( 'NONE',  ( 206.1932826529868805, 273.5097535960530877, 11.72208607728249241 ) ) ;
#82748 = ADVANCED_FACE ( 'NONE', ( #15069 ), #69776, .T. ) ;
#82749 = CARTESIAN_POINT ( 'NONE',  ( -52.57320609282758994, 32.70376883311633520, 10.00000000000000000 ) ) ;
#82750 = ORIENTED_EDGE ( 'NONE', *, *, #52881, .T. ) ;
#82751 = CARTESIAN_POINT ( 'NONE',  ( 177.1951107123421139, 278.9335273702716336, -15.93379266965202312 ) ) ;
#82752 = CARTESIAN_POINT ( 'NONE',  ( 168.9995394412663927, 261.3531918911040179, -16.36193740910546168 ) ) ;
#82753 = ORIENTED_EDGE ( 'NONE', *, *, #96333, .T. ) ;
#82754 = FACE_OUTER_BOUND ( 'NONE', #16048, .T. ) ;
#82755 = CARTESIAN_POINT ( 'NONE',  ( 192.4867975473904949, 297.2500821921321972, -13.04960750009181325 ) ) ;
#82756 = ORIENTED_EDGE ( 'NONE', *, *, #21827, .F. ) ;
#82757 = VECTOR ( 'NONE', #26522, 1000.000000000000000 ) ;
#82758 = ORIENTED_EDGE ( 'NONE', *, *, #29825, .T. ) ;
#82759 = CARTESIAN_POINT ( 'NONE',  ( 155.2084098882724845, 265.7658068242191689, -16.35003261853351830 ) ) ;
#82760 = CARTESIAN_POINT ( 'NONE',  ( -19.65312891409030271, 93.06504152958497400, 59.99999999999999289 ) ) ;
#82761 = CARTESIAN_POINT ( 'NONE',  ( 188.6795480343751308, 298.6307287810504931, -4.269171661791919092 ) ) ;
#82762 = CARTESIAN_POINT ( 'NONE',  ( 190.0259678364800493, 301.5123642802043946, 4.004183174499006626 ) ) ;
#82763 = CARTESIAN_POINT ( 'NONE',  ( 157.1241657895010633, 258.9031910183524019, -16.87105681078169894 ) ) ;
#82764 = CARTESIAN_POINT ( 'NONE',  ( 146.6805974831222841, 276.5887480051095508, -0.6663123207720742514 ) ) ;
#82765 = CARTESIAN_POINT ( 'NONE',  ( 147.2405539530007559, 275.6188749492528132, 0.4306668706573002492 ) ) ;
#82766 = ORIENTED_EDGE ( 'NONE', *, *, #69580, .T. ) ;
#82767 = CARTESIAN_POINT ( 'NONE',  ( 74.73127975335565054, 57.80664375811601019, -15.99177344183713778 ) ) ;
#82768 = CARTESIAN_POINT ( 'NONE',  ( 58.10966550219799132, 178.3759306620403606, 18.47570218321542868 ) ) ;
#82769 = CARTESIAN_POINT ( 'NONE',  ( 164.9617201910520237, 244.9249146555742414, 2.745022583679548767 ) ) ;
#82770 = CARTESIAN_POINT ( 'NONE',  ( 67.11701428173226702, 66.86566084198229021, 8.934729829905201370 ) ) ;
#82771 = CARTESIAN_POINT ( 'NONE',  ( 168.2709212779534482, 286.3625079078701674, 3.948410620585521613 ) ) ;
#82772 = CARTESIAN_POINT ( 'NONE',  ( 84.74721491826518616, 41.70368105205244547, 1.055763243526395279 ) ) ;
#82773 = CARTESIAN_POINT ( 'NONE',  ( 100.3364738622893810, 237.9244531367911009, -4.594050593750046652 ) ) ;
#82774 = ORIENTED_EDGE ( 'NONE', *, *, #78927, .F. ) ;
#82775 = CARTESIAN_POINT ( 'NONE',  ( 190.1544783179600415, 301.2897775969759664, -3.447215837936876248 ) ) ;
#82776 = CARTESIAN_POINT ( 'NONE',  ( 76.79673682827939274, 53.97105271787633285, -16.03547630156775838 ) ) ;
#82777 = CARTESIAN_POINT ( 'NONE',  ( 202.5752970409983220, 279.0574324504058268, 15.43767528721618021 ) ) ;
#82778 = CARTESIAN_POINT ( 'NONE',  ( 78.94111852906270599, 46.22145796229974479, 12.82134408105561363 ) ) ;
#82779 = CARTESIAN_POINT ( 'NONE',  ( 198.7409601489106592, 286.4175548075023698, -17.25928620176719974 ) ) ;
#82780 = FACE_OUTER_BOUND ( 'NONE', #595, .T. ) ;
#82781 = VERTEX_POINT ( 'NONE', #76876 ) ;
#82782 = CARTESIAN_POINT ( 'NONE',  ( 170.5199279757401598, 255.7150289786715973, -11.87445405841454971 ) ) ;
#82783 =( BOUNDED_CURVE ( )  B_SPLINE_CURVE ( 2, ( #44367, #82921, #50973, #90022, #4382, #66189, #59556, #20594, #27702 ),
 .UNSPECIFIED., .F., .T. ) 
 B_SPLINE_CURVE_WITH_KNOTS ( ( 3, 2, 2, 2, 3 ),
 ( 0.3346774193548386900, 0.3360215053763440651, 0.3387096774193548154, 0.3413978494623655657, 0.3427419354838709964 ),
 .UNSPECIFIED. ) 
 CURVE ( )  GEOMETRIC_REPRESENTATION_ITEM ( )  RATIONAL_B_SPLINE_CURVE ( ( 0.9330127018922194093, 0.9330127018922194093, 1.000000000000000000, 0.8660254037844387076, 1.000000000000000000, 0.8660254037844387076, 1.000000000000000000, 0.9330127018922179660, 0.9330127018922194093 ) ) 
 REPRESENTATION_ITEM ( '' )  );
#82784 = CARTESIAN_POINT ( 'NONE',  ( 84.22619167544027619, 44.03813768368893022, 8.426601908164510490 ) ) ;
#82786 = EDGE_CURVE ( 'NONE', #41262, #32844, #91128, .T. ) ;
#82785 = CARTESIAN_POINT ( 'NONE',  ( 164.8329445879545290, 245.1479605429143760, -2.955380775890217304 ) ) ;
#82787 = CARTESIAN_POINT ( 'NONE',  ( 31.61400995286148330, 202.3927522451419350, 2.944929066748280225E-16 ) ) ;
#82788 = CARTESIAN_POINT ( 'NONE',  ( 119.3079296378835181, 245.8149278399160949, -9.188101187500095079 ) ) ;
#82789 = CARTESIAN_POINT ( 'NONE',  ( 199.0363797504450929, 285.9058730480928716, -17.12190301149298222 ) ) ;
#82790 = CARTESIAN_POINT ( 'NONE',  ( 164.1788121382481904, 280.3338528224191464, -11.36002433749857410 ) ) ;
#82791 = CARTESIAN_POINT ( 'NONE',  ( 84.60621859610353113, 50.62332914066485756, 13.66912872509914578 ) ) ;
#82792 = CARTESIAN_POINT ( 'NONE',  ( 172.3688428511626967, 251.1033656833274677, -4.005216378610661820 ) ) ;
#82793 = CARTESIAN_POINT ( 'NONE',  ( 38.76756708593069334, 199.3149278399161233, -9.188101187500095079 ) ) ;
#82794 = DIRECTION ( 'NONE',  ( -1.000000000000000000, 0.000000000000000000, 0.000000000000000000 ) ) ;
#82795 = ORIENTED_EDGE ( 'NONE', *, *, #88568, .T. ) ;
#82796 = CARTESIAN_POINT ( 'NONE',  ( -1.387478102835363769, 181.5530062829863596, 2.649461200531984646E-14 ) ) ;
#82797 = CARTESIAN_POINT ( 'NONE',  ( 181.8871442283018212, 266.9089101108496038, 15.94309912413098473 ) ) ;
#82798 = CARTESIAN_POINT ( 'NONE',  ( -61.64759997997268925, 36.73658404823907375, 10.00000000000000000 ) ) ;
#82799 = CARTESIAN_POINT ( 'NONE',  ( 81.75715262849954001, 41.47753617486669242, -5.100220969704232665 ) ) ;
#82800 = CARTESIAN_POINT ( 'NONE',  ( 14.38368916104982986, 8.708529653044781327, 1.583844403245360466 ) ) ;
#82801 = CARTESIAN_POINT ( 'NONE',  ( 178.6792603332878002, 287.1060177970853715, -12.25702117352004450 ) ) ;
#82802 = CARTESIAN_POINT ( 'NONE',  ( 164.2020060191955793, 250.0206628281335668, 10.23082325107943191 ) ) ;
#82803 = CARTESIAN_POINT ( 'NONE',  ( 94.76169564547690527, 215.5177522451417929, 5.000000000000051514 ) ) ;
#82804 = VERTEX_POINT ( 'NONE', #38869 ) ;
#82805 = CARTESIAN_POINT ( 'NONE',  ( 198.7498379103732304, 267.8340533398088610, -8.134651165626271663 ) ) ;
#82806 = EDGE_CURVE ( 'NONE', #14068, #63364, #99904, .T. ) ;
#82807 = CARTESIAN_POINT ( 'NONE',  ( 155.1870085809113675, 280.1431070046639320, -2.400648766995867600 ) ) ;
#82808 = CARTESIAN_POINT ( 'NONE',  ( 208.1612901671020381, 270.1010645919285480, -2.401583477149568768 ) ) ;
#82809 = CARTESIAN_POINT ( 'NONE',  ( 16.06189740016370848, 170.8923013555409796, 4.594050593750050204 ) ) ;
#82810 = CARTESIAN_POINT ( 'NONE',  ( 5.287540158160898507, 21.79103043416546726, 8.090169943749478065 ) ) ;
#82811 = CARTESIAN_POINT ( 'NONE',  ( 192.2441535563929733, 272.1090697265545373, 14.30193341551846586 ) ) ;
#82812 = CARTESIAN_POINT ( 'NONE',  ( 71.50282862545680018, 59.38978230636582367, -15.72801454580908320 ) ) ;
#82813 = CARTESIAN_POINT ( 'NONE',  ( 71.98214240380765716, 72.19672774639096247, -1.652923604091230958 ) ) ;
#82814 = CARTESIAN_POINT ( 'NONE',  ( 52.46142023538963173, 213.3464784336661637, 1.353441290958777327E-15 ) ) ;
#82815 = CARTESIAN_POINT ( 'NONE',  ( 207.6590484093196096, 270.9709728340903894, 3.402057849327809524 ) ) ;
#82816 = CARTESIAN_POINT ( 'NONE',  ( 72.49386282319787256, 57.57572440859878071, 15.80166580940836596 ) ) ;
#82817 = EDGE_CURVE ( 'NONE', #62993, #35992, #100027, .T. ) ;
#82818 = CARTESIAN_POINT ( 'NONE',  ( -19.65312891409030271, 93.06504152958497400, 59.99999999999999289 ) ) ;
#82819 = CARTESIAN_POINT ( 'NONE',  ( 164.9404048476745004, 244.9618339132846074, -2.801285734921658666 ) ) ;
#82820 = ORIENTED_EDGE ( 'NONE', *, *, #64377, .T. ) ;
#82821 = EDGE_CURVE ( 'NONE', #3950, #4092, #49120, .T. ) ;
#82822 = VECTOR ( 'NONE', #71230, 1000.000000000000000 ) ;
#82823 = CARTESIAN_POINT ( 'NONE',  ( 1.898513289055842712, 185.2365022471903444, 2.944929066748280225E-16 ) ) ;
#82824 = CARTESIAN_POINT ( 'NONE',  ( 49.10122569834318540, 93.29622288527660601, -10.00000000000000000 ) ) ;
#82825 = CARTESIAN_POINT ( 'NONE',  ( 139.7406297344813311, 260.6744531367911009, 4.594050593750047540 ) ) ;
#82826 = CARTESIAN_POINT ( 'NONE',  ( 26.50621139815081762, 30.70171378149920471, -9.188101187500004485 ) ) ;
#82827 = CARTESIAN_POINT ( 'NONE',  ( 165.0826521866380006, 244.7154542949585050, 1.746033430215258475 ) ) ;
#82828 = CARTESIAN_POINT ( 'NONE',  ( 83.44578961920555571, 51.64149152686551503, -14.89211022975658949 ) ) ;
#82829 = DIRECTION ( 'NONE',  ( -0.8660254037844387076, -0.4999999999999998890, -0.000000000000000000 ) ) ;
#82831 = CARTESIAN_POINT ( 'NONE',  ( 188.2348408267917250, 289.2768701213889244, 14.43578146676328977 ) ) ;
#82830 = CARTESIAN_POINT ( 'NONE',  ( 81.65971250072203702, 41.57115319798205633, -5.463628752668030053 ) ) ;
#82832 = CARTESIAN_POINT ( 'NONE',  ( 17.60357497223980516, 35.28838536716092023, 10.00000000000000000 ) ) ;
#82833 = VERTEX_POINT ( 'NONE', #2399 ) ;
#82834 = CARTESIAN_POINT ( 'NONE',  ( 150.6431064791187850, 269.7254810985950257, 15.11064854015152470 ) ) ;
#82835 = CARTESIAN_POINT ( 'NONE',  ( 163.4299912484447930, 247.5779470075939059, 8.687773149566549336 ) ) ;
#82836 = CARTESIAN_POINT ( 'NONE',  ( 129.4230657250939203, 233.9824982072973683, 3.021315404115420679E-15 ) ) ;
#82837 = CARTESIAN_POINT ( 'NONE',  ( 172.9592948101169725, 268.4257463397073593, -16.38380952890091891 ) ) ;
#82838 = CARTESIAN_POINT ( 'NONE',  ( 197.3002854903134562, 273.1938965430982194, -13.39091482477390116 ) ) ;
#82839 = VERTEX_POINT ( 'NONE', #56575 ) ;
#82840 = CARTESIAN_POINT ( 'NONE',  ( 68.91246633537454613, 66.80396089893802980, 9.505547287390900379 ) ) ;
#82841 = CARTESIAN_POINT ( 'NONE',  ( 171.3274490369448415, 284.4986492857913163, -11.39081580260379134 ) ) ;
#82842 = CARTESIAN_POINT ( 'NONE',  ( 71.71444459471545940, 72.49928141732988252, 0.9658765412761323166 ) ) ;
#82843 = CARTESIAN_POINT ( 'NONE',  ( 80.05961770938091604, 205.4824982072973967, 3.021315404115420679E-15 ) ) ;
#82844 = CARTESIAN_POINT ( 'NONE',  ( 196.1399273980812836, 271.0394808790050547, 12.45890580183448471 ) ) ;
#82845 = CARTESIAN_POINT ( 'NONE',  ( 185.8152975361811912, 296.8366838734828548, 5.365625994531613152 ) ) ;
#82846 = CARTESIAN_POINT ( 'NONE',  ( 22.72264919896475988, 37.02287747747012503, 10.00000000000000000 ) ) ;
#82847 = FACE_OUTER_BOUND ( 'NONE', #82250, .T. ) ;
#82848 = PLANE ( 'NONE',  #30553 ) ;
#82849 = EDGE_CURVE ( 'NONE', #22636, #51125, #58895, .T. ) ;
#82850 = DIRECTION ( 'NONE',  ( 0.5000000000000001110, -0.8660254037844384856, -0.000000000000000000 ) ) ;
#82851 = CARTESIAN_POINT ( 'NONE',  ( 13.51924585473484974, 23.50829794293879615, -10.00000000000000355 ) ) ;
#82852 = CARTESIAN_POINT ( 'NONE',  ( 82.56691085815100450, 44.30186147993075707, 9.990707220731064098 ) ) ;
#82853 = ORIENTED_EDGE ( 'NONE', *, *, #78427, .T. ) ;
#82854 = CARTESIAN_POINT ( 'NONE',  ( 166.7959447105422157, 276.3626885415273478, 15.91653206054683523 ) ) ;
#82855 = CARTESIAN_POINT ( 'NONE',  ( 86.25376498619890242, 46.94328282020536136, -10.55339115541320538 ) ) ;
#82856 = CARTESIAN_POINT ( 'NONE',  ( -76.23101443460923576, 54.01191295053621388, 10.00000000000000000 ) ) ;
#82857 = ORIENTED_EDGE ( 'NONE', *, *, #32793, .F. ) ;
#82858 = CARTESIAN_POINT ( 'NONE',  ( 163.5477118939200807, 267.5842859632946329, -17.71268400963646528 ) ) ;
#82859 = CARTESIAN_POINT ( 'NONE',  ( 185.2241444343604257, 291.3773840544799896, 11.95617939456810674 ) ) ;
#82860 = CARTESIAN_POINT ( 'NONE',  ( 163.7064929935861244, 247.0990319366274548, 6.401263337036986023 ) ) ;
#82861 = CARTESIAN_POINT ( 'NONE',  ( 19.12011368430507829, 34.47266676343468106, 10.00000000000000000 ) ) ;
#82862 = ORIENTED_EDGE ( 'NONE', *, *, #62203, .F. ) ;
#82863 = CARTESIAN_POINT ( 'NONE',  ( 75.84410613756948294, 226.8464784336661353, 1.353441290958777525E-15 ) ) ;
#82864 = CARTESIAN_POINT ( 'NONE',  ( 155.0478382459045577, 262.0962618848092802, 18.21693143622618649 ) ) ;
#82865 = CARTESIAN_POINT ( 'NONE',  ( 180.1013849714563833, 270.4519419265931788, -16.02035677620936482 ) ) ;
#82866 = CARTESIAN_POINT ( 'NONE',  ( 81.53115339417709606, 41.92267797689947884, -7.515177224797632505 ) ) ;
#82867 = VERTEX_POINT ( 'NONE', #25175 ) ;
#82868 = ADVANCED_FACE ( 'NONE', ( #8486 ), #98364, .F. ) ;
#82869 = EDGE_LOOP ( 'NONE', ( #37478, #33974, #67076, #70624, #73768 ) ) ;
#82870 = CARTESIAN_POINT ( 'NONE',  ( 207.3500332735622180, 270.8109745646875126, 1.847778963486053749 ) ) ;
#82871 = VERTEX_POINT ( 'NONE', #72816 ) ;
#82872 = CARTESIAN_POINT ( 'NONE',  ( 81.78568384109607337, 51.89477062050791289, 14.95452106162773198 ) ) ;
#82873 = ORIENTED_EDGE ( 'NONE', *, *, #8469, .T. ) ;
#82874 = CARTESIAN_POINT ( 'NONE',  ( 75.29381676803062362, 60.13143282175177973, 15.65255259757436512 ) ) ;
#82875 = ORIENTED_EDGE ( 'NONE', *, *, #52578, .T. ) ;
#82876 = CARTESIAN_POINT ( 'NONE',  ( 165.0777597283848195, 244.7239282812269039, 1.811418920707685842 ) ) ;
#82877 = CARTESIAN_POINT ( 'NONE',  ( 152.9273493951901628, 265.7690563111299298, -17.70273273795505631 ) ) ;
#82878 = CARTESIAN_POINT ( 'NONE',  ( 47.49582885874516336, 78.29235751436857527, 10.00000000000000000 ) ) ;
#82879 = CARTESIAN_POINT ( 'NONE',  ( 72.97361289423018604, 68.13649966853542139, -10.75395737491361814 ) ) ;
#82880 = CARTESIAN_POINT ( 'NONE',  ( 164.7384773709341630, 265.0745892635314362, -16.62235727310338618 ) ) ;
#82881 = ORIENTED_EDGE ( 'NONE', *, *, #97232, .T. ) ;
#82882 = CARTESIAN_POINT ( 'NONE',  ( 76.56819355343940003, 59.09054857262015759, 15.98656334013552893 ) ) ;
#82883 = CARTESIAN_POINT ( 'NONE',  ( 14.66449673273962340, 9.262165230724928477, -2.296566073217252530E-15 ) ) ;
#82884 = EDGE_CURVE ( 'NONE', #76991, #82653, #50166, .T. ) ;
#82885 = VERTEX_POINT ( 'NONE', #73788 ) ;
#82886 = CARTESIAN_POINT ( 'NONE',  ( 166.9150765994704955, 283.4538441081094788, 8.983515016175676493 ) ) ;
#82888 = VERTEX_POINT ( 'NONE', #20097 ) ;
#82887 = CARTESIAN_POINT ( 'NONE',  ( 203.2792425030030188, 271.6204427260279317, 9.522413789076535906 ) ) ;
#82889 = CARTESIAN_POINT ( 'NONE',  ( 70.98683038387876820, 61.11472152276905234, -14.49225651734632692 ) ) ;
#82890 = CARTESIAN_POINT ( 'NONE',  ( 160.0081047537594543, 253.5048282741223602, -16.11956848123596941 ) ) ;
#82891 = CARTESIAN_POINT ( 'NONE',  ( 150.1843315557205756, 276.3611790585334802, -5.337065203306020855 ) ) ;
#82892 = CARTESIAN_POINT ( 'NONE',  ( 165.4478602433182743, 246.8625711930905027, -1.873768097677063427 ) ) ;
#82893 = FACE_OUTER_BOUND ( 'NONE', #74894, .T. ) ;
#82894 = CARTESIAN_POINT ( 'NONE',  ( 168.4809247738020019, 252.9187805847961670, 12.05003015331094041 ) ) ;
#82895 = CARTESIAN_POINT ( 'NONE',  ( 88.42385336119198769, 44.01808410483894107, -2.342466917228906098 ) ) ;
#82896 = VERTEX_POINT ( 'NONE', #18596 ) ;
#82898 = CARTESIAN_POINT ( 'NONE',  ( 155.4266178972399359, 261.4401962838231839, -18.59384973550221076 ) ) ;
#82897 = B_SPLINE_CURVE_WITH_KNOTS ( 'NONE', 3,
 ( #73335, #26724, #27230, #73823, #81459, #51510, #90568, #44397, #43901, #57606, #12531, #52014, #4415, #59083, #50022, #34321, #12030, #35310, #74841, #97642, #42886, #5421, #82955, #13529, #75332, #67207, #58114, #65219, #43402, #89095, #50505, #96161, #28714, #88587, #36303, #19644, #98130, #19148, #66223, #35813, #80976, #11541, #66707, #3922, #28207, #97161 ),
 .UNSPECIFIED., .F., .F.,
 ( 4, 2, 2, 2, 2, 2, 2, 2, 2, 2, 2, 2, 2, 2, 2, 2, 2, 2, 2, 2, 2, 2, 4 ),
 ( 0.002719413596635465377, 0.003132706262424970068, 0.003339352595319770335, 0.003442675761767165915, 0.003545998928214561929, 0.003752645261109377375, 0.003959291594004193254, 0.004372584259793886596, 0.005199169591373273280, 0.006025754922952659097, 0.006852340254532045781, 0.007678925586111432465, 0.007782248752558854933, 0.007833910335782613005, 0.007885571919006371944, 0.007937233502230130883, 0.007988895085453889822, 0.008092218251901553416, 0.008505510917692367390, 0.008712157250587838561, 0.008918803583483309733, 0.009125449916378780904, 0.009332096249274252076 ),
 .UNSPECIFIED. ) ;
#82899 = CARTESIAN_POINT ( 'NONE',  ( 70.24152351796814742, 63.55507216885125388, -13.00701345941583575 ) ) ;
#82900 = EDGE_LOOP ( 'NONE', ( #71733, #37065, #97696, #56049, #81729, #17430, #9460, #76733, #21094, #28505, #2564 ) ) ;
#82902 = ADVANCED_FACE ( 'NONE', ( #26189 ), #58079, .T. ) ;
#82901 = CARTESIAN_POINT ( 'NONE',  ( 160.1345624105295542, 276.5719778673294513, 12.81990450689413308 ) ) ;
#82903 = CARTESIAN_POINT ( 'NONE',  ( 201.4015734403423323, 266.9510600575795820, -2.208871080923278107 ) ) ;
#82904 = CARTESIAN_POINT ( 'NONE',  ( 164.0871364075242980, 246.4397382041199762, -7.779248982433414561 ) ) ;
#82905 = CARTESIAN_POINT ( 'NONE',  ( 84.35687393656843369, 44.63875131664023854, -8.325067569704064141 ) ) ;
#82906 = FACE_OUTER_BOUND ( 'NONE', #84709, .T. ) ;
#82908 = CARTESIAN_POINT ( 'NONE',  ( 76.03019726450892790, 65.44783958900880805, 14.37600347258596045 ) ) ;
#82907 = CARTESIAN_POINT ( 'NONE',  ( -9.188242552867592394, 159.3768266524160140, 9.188101187500098632 ) ) ;
#82909 = CARTESIAN_POINT ( 'NONE',  ( 19.34531673258195994, 188.6427522451419350, 10.00000000000009415 ) ) ;
#82910 = ORIENTED_EDGE ( 'NONE', *, *, #39834, .T. ) ;
#82911 = ORIENTED_EDGE ( 'NONE', *, *, #62981, .F. ) ;
#82912 = CARTESIAN_POINT ( 'NONE',  ( -23.29562891409031522, 78.77562236714182120, 59.99999999999999289 ) ) ;
#82913 = CARTESIAN_POINT ( 'NONE',  ( 169.1310403812000516, 286.3093371794724931, 8.868891257890425095 ) ) ;
#82914 = CARTESIAN_POINT ( 'NONE',  ( -6.887318171848119341, 24.23892674679882475, 177.5919119679930134 ) ) ;
#82915 = CARTESIAN_POINT ( 'NONE',  ( 172.2401199401735710, 289.4450576335847813, 2.617625608981040575 ) ) ;
#82916 = CARTESIAN_POINT ( 'NONE',  ( 85.84416675550359344, 42.93383034132180143, 1.917673184544592013 ) ) ;
#82917 = CARTESIAN_POINT ( 'NONE',  ( 83.86430188519919682, 45.36457422996819133, 9.662219384362932928 ) ) ;
#82918 = CARTESIAN_POINT ( 'NONE',  ( -19.65312891409030271, 93.06504152958497400, 10.00000000000000888 ) ) ;
#82919 = CARTESIAN_POINT ( 'NONE',  ( 18.68642948779652002, 193.8464784336661637, 1.353441290958777525E-15 ) ) ;
#82920 = CARTESIAN_POINT ( 'NONE',  ( 116.5476472112030990, 238.0958772461660544, -9.188101187500095079 ) ) ;
#82921 = CARTESIAN_POINT ( 'NONE',  ( 45.26399402665309424, 185.3932355074535678, -2.679491924311248496 ) ) ;
#82922 = CARTESIAN_POINT ( 'NONE',  ( 12.00096474099108690, 32.03863464977599307, -10.00000000000000000 ) ) ;
#82923 = CARTESIAN_POINT ( 'NONE',  ( 78.71261887716285344, 54.61647413563439812, 15.99851350793635518 ) ) ;
#82924 = CARTESIAN_POINT ( 'NONE',  ( 178.3505713125701959, 283.6140345280227848, -14.62659922741302054 ) ) ;
#82925 = AXIS2_PLACEMENT_3D ( 'NONE', #96198, #72889, #74385 ) ;
#82926 = CARTESIAN_POINT ( 'NONE',  ( 80.53132723571809493, 53.42204839544174888, -15.60352693426686699 ) ) ;
#82927 = CARTESIAN_POINT ( 'NONE',  ( 193.7706395672514645, 295.0264025848412075, 15.16938698680137065 ) ) ;
#82928 = CARTESIAN_POINT ( 'NONE',  ( 207.8844858873204657, 270.5805036682629066, -6.251308616122969397 ) ) ;
#82929 = CARTESIAN_POINT ( 'NONE',  ( 194.3541845315608612, 294.0156730581561533, -14.67567721756631016 ) ) ;
#82930 = CARTESIAN_POINT ( 'NONE',  ( 84.71425524834847920, 50.25098136614051469, 13.83365903171529077 ) ) ;
#82931 = DIRECTION ( 'NONE',  ( 0.000000000000000000, 0.000000000000000000, 1.000000000000000000 ) ) ;
#82932 = ADVANCED_FACE ( 'NONE', ( #11995 ), #81920, .F. ) ;
#82933 = DIRECTION ( 'NONE',  ( -0.5372068985985170020, -0.8434505012732892437, 0.000000000000000000 ) ) ;
#82934 = CARTESIAN_POINT ( 'NONE',  ( 184.1241864019008858, 268.6134890520179397, -15.18471742826366722 ) ) ;
#82935 = CARTESIAN_POINT ( 'NONE',  ( 48.81784752633560487, 86.82484054835779830, -10.00000000000000000 ) ) ;
#82936 = EDGE_CURVE ( 'NONE', #38602, #90969, #43363, .T. ) ;
#82938 = EDGE_CURVE ( 'NONE', #22359, #55654, #3406, .T. ) ;
#82937 = CARTESIAN_POINT ( 'NONE',  ( 172.7788321272523717, 263.1548091139151779, -15.50655718291449148 ) ) ;
#82939 = EDGE_CURVE ( 'NONE', #57243, #13423, #57568, .T. ) ;
#82940 = CARTESIAN_POINT ( 'NONE',  ( 95.14032143958276322, 234.9244531367911009, -4.594050593750046652 ) ) ;
#82941 = CARTESIAN_POINT ( 'NONE',  ( 190.7779368023172708, 300.2099158256590385, 8.142228434510803581 ) ) ;
#82942 = CARTESIAN_POINT ( 'NONE',  ( 9.684647596568824568, 42.25052203202275081, 59.99999999999999289 ) ) ;
#82943 = VECTOR ( 'NONE', #30642, 1000.000000000000114 ) ;
#82945 = CARTESIAN_POINT ( 'NONE',  ( 199.9508427912207367, 284.3219765998254047, 18.49391385354404349 ) ) ;
#82944 = CARTESIAN_POINT ( 'NONE',  ( 157.8092552871339365, 257.3133472685137235, 17.04082256169242626 ) ) ;
#82946 = CYLINDRICAL_SURFACE ( 'NONE', #22206, 10.00000000000010658 ) ;
#82947 = CARTESIAN_POINT ( 'NONE',  ( 199.2383506163646132, 285.5560492466715345, -17.78808061564097898 ) ) ;
#82948 = CARTESIAN_POINT ( 'NONE',  ( 204.3209023394900328, 276.1179509721322347, -13.17759910032226678 ) ) ;
#82949 = CARTESIAN_POINT ( 'NONE',  ( 42.56377214068922399, 30.28920272979930672, -7.433330006724141015 ) ) ;
#82950 = CARTESIAN_POINT ( 'NONE',  ( 147.4824818982269790, 275.1998434563504929, -4.972419998968698351 ) ) ;
#82951 = CYLINDRICAL_SURFACE ( 'NONE', #55540, 17.82106496071139645 ) ;
#82952 = ORIENTED_EDGE ( 'NONE', *, *, #4440, .F. ) ;
#82953 = CARTESIAN_POINT ( 'NONE',  ( 25.31423016981892715, 26.56628583063841731, 9.188101187500006262 ) ) ;
#82954 = CARTESIAN_POINT ( 'NONE',  ( 192.8011239859581849, 296.7056528303708660, -11.79847971295421694 ) ) ;
#82955 = CARTESIAN_POINT ( 'NONE',  ( 191.3732078456864372, 287.7026800961180015, -15.83705375440161767 ) ) ;
#82956 = ORIENTED_EDGE ( 'NONE', *, *, #1901, .T. ) ;
#82957 = CARTESIAN_POINT ( 'NONE',  ( 70.76797951062305003, 60.86569645529516492, 14.54278018258353988 ) ) ;
#82958 = CARTESIAN_POINT ( 'NONE',  ( 75.84431516675671503, 65.82088634210550993, -14.12726274127321169 ) ) ;
#82959 = CARTESIAN_POINT ( 'NONE',  ( 175.6063544791335573, 254.0105997054014040, 8.344378697908656051 ) ) ;
#82960 = CARTESIAN_POINT ( 'NONE',  ( 172.7840071827034478, 253.8156868574323255, -8.935542012173989690 ) ) ;
#82961 = CARTESIAN_POINT ( 'NONE',  ( 1.813001633210440611, 27.74720351945397923, -10.00000000000000000 ) ) ;
#82962 = CARTESIAN_POINT ( 'NONE',  ( 136.9984762794282744, 263.2365022471902876, 2.944929066748280225E-16 ) ) ;
#82963 = CARTESIAN_POINT ( 'NONE',  ( 88.19053702688614749, 44.32527345396092500, -2.493626234014364673 ) ) ;
#82964 = ORIENTED_EDGE ( 'NONE', *, *, #77623, .T. ) ;
#82965 = CARTESIAN_POINT ( 'NONE',  ( 84.37861180241492320, 46.14357002009968056, -10.86416137306961360 ) ) ;
#82966 = ORIENTED_EDGE ( 'NONE', *, *, #64947, .T. ) ;
#82967 = CARTESIAN_POINT ( 'NONE',  ( 197.0006684375643715, 265.0764226805687827, -4.603465283812302467 ) ) ;
#82968 = DIRECTION ( 'NONE',  ( -1.000000000000000000, 0.000000000000000000, 0.000000000000000000 ) ) ;
#82969 = VERTEX_POINT ( 'NONE', #80940 ) ;
#82970 = CARTESIAN_POINT ( 'NONE',  ( 183.1488928027059444, 291.3758770271683147, -10.74625559401416375 ) ) ;
#82971 = ORIENTED_EDGE ( 'NONE', *, *, #49674, .T. ) ;
#82972 = CARTESIAN_POINT ( 'NONE',  ( -19.65312891409030271, 93.06504152958497400, 10.00000000000000888 ) ) ;
#82973 = CARTESIAN_POINT ( 'NONE',  ( 205.5156181057928677, 274.6835030222813998, 11.38452381065716068 ) ) ;
#82974 = CARTESIAN_POINT ( 'NONE',  ( 193.4272026183557216, 280.4276906386824635, -16.92506342575424583 ) ) ;
#82975 = CARTESIAN_POINT ( 'NONE',  ( 193.2107205041928353, 295.9962108501849229, -13.27437237753875721 ) ) ;
#82976 = CARTESIAN_POINT ( 'NONE',  ( 201.3053499423511425, 281.9759013948520874, -16.75960365258566398 ) ) ;
#82977 = FACE_OUTER_BOUND ( 'NONE', #68825, .T. ) ;
#82978 = CARTESIAN_POINT ( 'NONE',  ( 39.89592612264573290, 25.96004757982093025, -5.678558825948275768 ) ) ;
#82979 = CARTESIAN_POINT ( 'NONE',  ( 71.19423160720042176, 61.06544498174218916, -14.56549237402769670 ) ) ;
#82980 = CARTESIAN_POINT ( 'NONE',  ( 170.9169832065359458, 256.6048082181670225, 13.90689315385514035 ) ) ;
#82981 = CARTESIAN_POINT ( 'NONE',  ( 46.80963145949300497, 71.09457308843315104, -10.00000000000000000 ) ) ;
#82982 = ORIENTED_EDGE ( 'NONE', *, *, #48490, .T. ) ;
#82983 = ORIENTED_EDGE ( 'NONE', *, *, #24044, .F. ) ;
#82984 = CARTESIAN_POINT ( 'NONE',  ( 183.8037341582430884, 275.4624792557407318, 17.77592483611231700 ) ) ;
#82986 = CARTESIAN_POINT ( 'NONE',  ( 163.1080940025530310, 272.5857820118623636, -15.50684756597832958 ) ) ;
#82985 = CARTESIAN_POINT ( 'NONE',  ( 174.5258411212118972, 257.2153983152082333, -12.12657788165876838 ) ) ;
#82987 = PLANE ( 'NONE',  #78922 ) ;
#82988 = CARTESIAN_POINT ( 'NONE',  ( 148.7819146692434629, 276.2864599824047218, -5.482525570765545808 ) ) ;
#82989 = CARTESIAN_POINT ( 'NONE',  ( 73.46416042179349404, 61.28524521429519467, -15.02223754724939653 ) ) ;
#82990 = CARTESIAN_POINT ( 'NONE',  ( 189.8238368927809745, 301.8624653444729802, -0.3620111495846872751 ) ) ;
#82991 = CARTESIAN_POINT ( 'NONE',  ( 170.9352951703182555, 287.6820827080605341, -4.605083712371007110 ) ) ;
#82992 = CARTESIAN_POINT ( 'NONE',  ( 77.07143086693146472, 63.53409821367920784, -15.43182057973166188 ) ) ;
#82993 = CARTESIAN_POINT ( 'NONE',  ( 181.7635954225607406, 256.3719561854650237, 5.206822859736072395 ) ) ;
#82994 = CARTESIAN_POINT ( 'NONE',  ( 101.5001087246834857, 241.6589784336661637, -6.496448406907675876E-16 ) ) ;
#82995 = ORIENTED_EDGE ( 'NONE', *, *, #19434, .F. ) ;
#82996 = CARTESIAN_POINT ( 'NONE',  ( 0.9561933761060431580, 66.99251067065806353, -10.00000000000000000 ) ) ;
#82997 = CARTESIAN_POINT ( 'NONE',  ( 191.8819534272594183, 275.1740554287606528, 16.67007678262692494 ) ) ;
#82998 = EDGE_CURVE ( 'NONE', #27498, #44553, #90257, .T. ) ;
#82999 = ORIENTED_EDGE ( 'NONE', *, *, #16908, .F. ) ;
#83000 = VECTOR ( 'NONE', #76203, 1000.000000000000227 ) ;
#83001 = AXIS2_PLACEMENT_3D ( 'NONE', #26491, #32584, #25480 ) ;
#83002 = CARTESIAN_POINT ( 'NONE',  ( 87.17963343274935539, 46.25680430639528140, -9.118192349661992324 ) ) ;
#83003 = VECTOR ( 'NONE', #54875, 1000.000000000000114 ) ;
#83005 = B_SPLINE_SURFACE_WITH_KNOTS ( 'NONE', 3, 1, ( 
 ( #16465, #78284 ),
 ( #31155, #39733 ),
 ( #70665, #94011 ),
 ( #30680, #1279 ),
 ( #76771, #45848 ),
 ( #63068, #55446 ),
 ( #86433, #23053 ),
 ( #92507, #47848 ),
 ( #6871, #53462 ),
 ( #37762, #99588 ),
 ( #53951, #30172 ),
 ( #61058, #15449 ),
 ( #46348, #77271 ),
 ( #65932, #5143 ),
 ( #71193, #26946 ),
 ( #3662, #57830 ),
 ( #73551, #12761 ),
 ( #58814, #66924 ),
 ( #42133, #89303 ),
 ( #49743, #18860 ),
 ( #11758, #58328 ),
 ( #65438, #26457 ),
 ( #34540, #9374 ),
 ( #27457, #12253 ),
 ( #95899, #4135 ),
 ( #73064, #89776 ),
 ( #51221, #96887 ),
 ( #42622, #43110 ),
 ( #19858, #36024 ),
 ( #3178, #88810 ),
 ( #96383, #19376 ),
 ( #50724, #97364 ),
 ( #50235, #74055 ),
 ( #81190, #35028 ) ),
 .UNSPECIFIED., .T., .F., .F.,
 ( 4, 2, 2, 2, 2, 2, 2, 2, 2, 2, 2, 2, 2, 2, 2, 2, 4 ),
 ( 2, 2 ),
 ( 0.000000000000000000, 0.06250000000000000000, 0.1250000000000000000, 0.1875000000000000000, 0.2500000000000000000, 0.3125000000000000000, 0.3750000000000000000, 0.4375000000000000000, 0.5000000000000000000, 0.5625000000000000000, 0.6250000000000000000, 0.6875000000000000000, 0.7500000000000000000, 0.8125000000000000000, 0.8750000000000000000, 0.9375000000000000000, 1.000000000000000000 ),
 ( 0.000000000000000000, 1.000000000000000000 ),
 .UNSPECIFIED. ) ;
#83004 = DIRECTION ( 'NONE',  ( 0.8660254037844384856, 0.5000000000000002220, -5.782411586589354927E-17 ) ) ;
#83006 = CARTESIAN_POINT ( 'NONE',  ( 195.9920715006079490, 291.1787696107118677, 15.99608784761372071 ) ) ;
#83007 = CARTESIAN_POINT ( 'NONE',  ( 26.05686017436622137, 36.81751292744056769, -6.180339887498951690 ) ) ;
#83008 = CARTESIAN_POINT ( 'NONE',  ( 73.83400387536809717, 55.06300064600840471, -16.12704957102858572 ) ) ;
#83009 = VERTEX_POINT ( 'NONE', #3887 ) ;
#83010 = ORIENTED_EDGE ( 'NONE', *, *, #50238, .F. ) ;
#83011 = B_SPLINE_CURVE_WITH_KNOTS ( 'NONE', 3,
 ( #8888, #30699, #24086, #86453, #69185, #54982, #85961, #39266, #32184, #16978, #39757, #61579, #31178, #61078, #76791, #23077, #45866, #68682, #85441, #46367, #53969, #15989, #37780, #16487, #47383, #15472, #100114, #93016, #7904, #70176, #84926, #78307, #784, #31670, #77297, #7384, #38779, #69685, #62566, #290, #62068, #94032, #23570, #38273, #54462, #70685 ),
 .UNSPECIFIED., .F., .F.,
 ( 4, 2, 2, 2, 2, 2, 2, 2, 2, 2, 2, 2, 2, 2, 2, 2, 2, 2, 2, 2, 2, 2, 4 ),
 ( 0.002472027920451953277, 0.002893672058135126832, 0.003104494126976747436, 0.003209905161397578338, 0.003315316195818409240, 0.003420727230239240142, 0.003526138264660071044, 0.003736960333501726343, 0.004158604471184948470, 0.005001892746551547114, 0.005845181021918147493, 0.006688469297284747005, 0.007110113434968052398, 0.007531757572651357792, 0.007637168607072145760, 0.007689874124282577474, 0.007742579641493009188, 0.007847990675913931596, 0.007953401710334854005, 0.008375045848018541905, 0.008796689985702228071, 0.009007512054544076358, 0.009218334123385926379 ),
 .UNSPECIFIED. ) ;
#83012 = CARTESIAN_POINT ( 'NONE',  ( 41.93414601462609426, 195.0177522451418781, -10.00000000000009592 ) ) ;
#83013 = ORIENTED_EDGE ( 'NONE', *, *, #99333, .F. ) ;
#83014 = EDGE_CURVE ( 'NONE', #8310, #18075, #45355, .T. ) ;
#83015 = CARTESIAN_POINT ( 'NONE',  ( 194.6903171191896433, 266.4159511179065021, -7.916380833475905376 ) ) ;
#83016 = CARTESIAN_POINT ( 'NONE',  ( -40.67952639183666008, 27.60432558407080350, -10.00000000000000000 ) ) ;
#83017 = CARTESIAN_POINT ( 'NONE',  ( 67.31170132302078457, 68.89449653470401813, -3.954031917524302386 ) ) ;
#83019 = CARTESIAN_POINT ( 'NONE',  ( 199.8805116513159135, 284.0430704225434511, 16.91808164086238264 ) ) ;
#83018 = CARTESIAN_POINT ( 'NONE',  ( 197.9793137651938935, 285.9304194886471464, 17.71000985939274841 ) ) ;
#83020 = CARTESIAN_POINT ( 'NONE',  ( 152.6873874250818517, 266.1846826352417565, -16.66598363829485763 ) ) ;
#83021 = VERTEX_POINT ( 'NONE', #36267 ) ;
#83022 = CARTESIAN_POINT ( 'NONE',  ( 157.1886094632603772, 258.3883373689681093, 18.40926891635499985 ) ) ;
#83024 = CARTESIAN_POINT ( 'NONE',  ( 82.33638059893669947, 51.07561602432041781, 14.47696974499355704 ) ) ;
#83023 = B_SPLINE_SURFACE_WITH_KNOTS ( 'NONE', 3, 1, ( 
 ( #15437, #88796 ),
 ( #77259, #10742 ),
 ( #48234, #18847 ),
 ( #26445, #87315 ),
 ( #57321, #33540 ),
 ( #7868, #38747 ),
 ( #64438, #56824 ),
 ( #80683, #259 ),
 ( #79179, #63929 ),
 ( #88293, #11258 ),
 ( #2148, #31141 ),
 ( #92985, #71553 ),
 ( #33029, #94868 ),
 ( #25429, #56321 ),
 ( #50713, #82678 ),
 ( #27441, #4629 ),
 ( #35016, #19364 ),
 ( #51209, #97353 ),
 ( #81666, #50223 ),
 ( #21325, #35523 ),
 ( #81178, #96873 ),
 ( #44596, #59291 ),
 ( #66423, #37011 ),
 ( #90272, #51736 ),
 ( #58802, #12750 ),
 ( #74552, #11744 ),
 ( #28931, #36011 ),
 ( #83153, #66913 ),
 ( #13243, #36511 ),
 ( #59805, #90774 ),
 ( #75531, #67920 ),
 ( #98841, #42607 ),
 ( #8122, #52701 ),
 ( #30910, #15698 ) ),
 .UNSPECIFIED., .T., .F., .F.,
 ( 4, 2, 2, 2, 2, 2, 2, 2, 2, 2, 2, 2, 2, 2, 2, 2, 4 ),
 ( 2, 2 ),
 ( 0.000000000000000000, 0.06250000000000000000, 0.1250000000000000000, 0.1875000000000000000, 0.2500000000000000000, 0.3125000000000000000, 0.3750000000000000000, 0.4375000000000000000, 0.5000000000000000000, 0.5625000000000000000, 0.6250000000000000000, 0.6875000000000000000, 0.7500000000000000000, 0.8125000000000000000, 0.8750000000000000000, 0.9375000000000000000, 1.000000000000000000 ),
 ( 0.000000000000000000, 1.000000000000000000 ),
 .UNSPECIFIED. ) ;
#83025 = CARTESIAN_POINT ( 'NONE',  ( 82.16331024188988863, 41.19762905728452296, -3.464377343443369561 ) ) ;
#83026 = CARTESIAN_POINT ( 'NONE',  ( 173.2276582641987659, 251.6345432004491443, -0.2848423752525459096 ) ) ;
#83027 = CARTESIAN_POINT ( 'NONE',  ( 45.14796862286864609, 185.3262482093457209, 3.021315404115420679E-15 ) ) ;
#83028 = CYLINDRICAL_SURFACE ( 'NONE', #12791, 16.60714546451156792 ) ;
#83029 = CARTESIAN_POINT ( 'NONE',  ( 83.71913944427328147, 44.06062028468042513, 7.985639216668514173 ) ) ;
#83030 = FACE_OUTER_BOUND ( 'NONE', #58124, .T. ) ;
#83031 = CARTESIAN_POINT ( 'NONE',  ( 194.2669918475045279, 294.1666952169902629, 14.00965265288584050 ) ) ;
#83032 = CARTESIAN_POINT ( 'NONE',  ( 178.2382707639212356, 285.7843550335422833, 14.43266090959460435 ) ) ;
#83033 = CARTESIAN_POINT ( 'NONE',  ( 69.64148527851303072, 70.32813841140065847, -3.761399768473041139 ) ) ;
#83034 = CARTESIAN_POINT ( 'NONE',  ( 78.52397964811635234, 206.9548013555409796, -4.594050593750042211 ) ) ;
#83035 = CARTESIAN_POINT ( 'NONE',  ( 159.4491226731523454, 254.4730136382542582, -15.39140229921534520 ) ) ;
#83036 = DIRECTION ( 'NONE',  ( 0.000000000000000000, 1.000000000000000000, 0.000000000000000000 ) ) ;
#83037 = CARTESIAN_POINT ( 'NONE',  ( 207.6050568035884680, 271.0644890383991310, -1.456818755242089702 ) ) ;
#83038 = CARTESIAN_POINT ( 'NONE',  ( 197.1490659794403939, 288.7466081235293700, -16.65847605485208760 ) ) ;
#83039 = CARTESIAN_POINT ( 'NONE',  ( 161.1492466472929266, 251.5283125358769212, -13.33353587056634915 ) ) ;
#83040 = CYLINDRICAL_SURFACE ( 'NONE', #9321, 70.00000000000002842 ) ;
#83041 = CARTESIAN_POINT ( 'NONE',  ( -20.86454769009831978, 95.07624631637331447, 45.19946697165472216 ) ) ;
#83042 = SURFACE_STYLE_USAGE ( .BOTH. , #6994 ) ;
#83043 = CARTESIAN_POINT ( 'NONE',  ( 43.28410984748890655, 30.15404122711137447, 8.090169943749479842 ) ) ;
#83044 = CARTESIAN_POINT ( 'NONE',  ( -69.61464189717713680, 45.83092310410449244, -10.00000000000000000 ) ) ;
#83045 = CARTESIAN_POINT ( 'NONE',  ( 157.6304115535352537, 270.8650229002738001, -16.00510772102553858 ) ) ;
#83046 = CARTESIAN_POINT ( 'NONE',  ( 72.26765824385677206, 72.08528386863294202, 3.191945267484126880 ) ) ;
#83047 =( BOUNDED_CURVE ( )  B_SPLINE_CURVE ( 2, ( #48861, #64044, #9346, #32641, #42229, #87432, #57431, #56932, #3272 ),
 .UNSPECIFIED., .F., .T. ) 
 B_SPLINE_CURVE_WITH_KNOTS ( ( 3, 2, 2, 2, 3 ),
 ( 0.04435483870967742159, 0.04569892473118279674, 0.04838709677419354704, 0.05107526881720430428, 0.05241935483870967943 ),
 .UNSPECIFIED. ) 
 CURVE ( )  GEOMETRIC_REPRESENTATION_ITEM ( )  RATIONAL_B_SPLINE_CURVE ( ( 0.9330127018922194093, 0.9330127018922194093, 1.000000000000000000, 0.8660254037844387076, 1.000000000000000000, 0.8660254037844387076, 1.000000000000000000, 0.9330127018922194093, 0.9330127018922194093 ) ) 
 REPRESENTATION_ITEM ( '' )  );
#83048 = CARTESIAN_POINT ( 'NONE',  ( 27.23877744593285755, 186.5333772461660544, 9.188101187500095079 ) ) ;
#83049 = EDGE_CURVE ( 'NONE', #87772, #82029, #38237, .T. ) ;
#83050 = CARTESIAN_POINT ( 'NONE',  ( 24.34666095796415419, 37.55466486950700755, 7.012934429366973338E-14 ) ) ;
#83051 = CARTESIAN_POINT ( 'NONE',  ( 46.16810866859812990, 28.78380873178791077, -6.180339887498949025 ) ) ;
#83052 = DIRECTION ( 'NONE',  ( -0.000000000000000000, -0.000000000000000000, -1.000000000000000000 ) ) ;
#83053 = CARTESIAN_POINT ( 'NONE',  ( 71.91369179320692240, 72.15417514627694118, -1.685444156100106561 ) ) ;
#83054 = CARTESIAN_POINT ( 'NONE',  ( 52.11020483269097525, 191.7048013555409796, 4.594050593750051981 ) ) ;
#83055 = CARTESIAN_POINT ( 'NONE',  ( 20.80007953598619608, 32.98502408145592568, -5.678558825948271327 ) ) ;
#83056 = CARTESIAN_POINT ( 'NONE',  ( 151.1230807375396807, 268.8941412966845519, -14.26613110909109849 ) ) ;
#83057 = LINE ( 'NONE', #59709, #84737 ) ;
#83058 = CARTESIAN_POINT ( 'NONE',  ( 46.99896066727236388, 26.94473085651396360, 1.475505719884397138E-15 ) ) ;
#83059 = CARTESIAN_POINT ( 'NONE',  ( 178.6317619811870259, 253.9327355832967612, -4.167451725846189170 ) ) ;
#83060 = CARTESIAN_POINT ( 'NONE',  ( -19.65312891409034179, 93.06504152958504505, 0.000000000000000000 ) ) ;
#83061 = CARTESIAN_POINT ( 'NONE',  ( 176.6908210328434450, 275.1332777264201468, 16.63294263746914581 ) ) ;
#83062 = CARTESIAN_POINT ( 'NONE',  ( 72.50355919934736448, 61.03236684371051268, 14.88608095558173439 ) ) ;
#83063 = CARTESIAN_POINT ( 'NONE',  ( 149.6148422561466305, 277.4437614652936190, 3.137689077364430368 ) ) ;
#83064 = CARTESIAN_POINT ( 'NONE',  ( 163.4168112749207467, 255.7475448173238135, -14.83461233001398405 ) ) ;
#83065 = CIRCLE ( 'NONE', #94421, 0.1418229129681564116 ) ;
#83066 = B_SPLINE_CURVE_WITH_KNOTS ( 'NONE', 3,
 ( #46866, #77790, #8375, #39239, #70152, #31647, #1276, #47358, #39731, #8865, #761, #62545, #93505, #24064, #85937, #32160, #63067, #80314, #97016, #27081, #95533, #81315, #74190, #58452, #79816, #65563, #50359, #19504, #17988, #41251, #35160, #26081, #35662, #33684, #11398, #89424, #96511, #10383, #66563, #25578, #42744, #56464, #57962, #11885, #57455, #72192, #43246, #87456 ),
 .UNSPECIFIED., .F., .F.,
 ( 4, 2, 2, 2, 2, 2, 2, 2, 2, 2, 2, 2, 2, 2, 2, 2, 2, 2, 2, 2, 2, 2, 2, 4 ),
 ( 0.0005187678782849775710, 0.001523663581573160260, 0.002026111433217250846, 0.002151723396128240803, 0.002277335359039230761, 0.002402947321950220285, 0.002528559284861210243, 0.002779783210683136382, 0.003031007136505062087, 0.003533454988148913931, 0.004538350691436559073, 0.005543246394724203781, 0.006045694246368027436, 0.006296918172189937962, 0.006548142098011849356, 0.006610948079467326988, 0.006673754060922803752, 0.006736560042378281384, 0.006799366023833759015, 0.007050589949655808319, 0.007301813875477857624, 0.007553037801299906061, 0.008055485652944047170, 0.008557933504588185677 ),
 .UNSPECIFIED. ) ;
#83067 = CARTESIAN_POINT ( 'NONE',  ( 82.14913611300819696, 41.13495720016906887, 3.242338130973200894 ) ) ;
#83068 = CARTESIAN_POINT ( 'NONE',  ( 87.70552531824185394, 45.34611373530315603, -6.437115693456841647 ) ) ;
#83069 = CARTESIAN_POINT ( 'NONE',  ( 95.28491933047786233, 232.4865022471902876, -10.00000000000009415 ) ) ;
#83070 = CARTESIAN_POINT ( 'NONE',  ( 200.4592688079413847, 283.4413569069752725, 18.39277739746426832 ) ) ;
#83071 = CARTESIAN_POINT ( 'NONE',  ( 165.0635501472802957, 269.5554238516661485, -16.29592778247673479 ) ) ;
#83072 = ORIENTED_EDGE ( 'NONE', *, *, #99333, .T. ) ;
#83073 = AXIS2_PLACEMENT_3D ( 'NONE', #85965, #46371, #9913 ) ;
#83074 = CARTESIAN_POINT ( 'NONE',  ( 51.75794814269728050, 206.8149278399160949, -9.188101187500095079 ) ) ;
#83075 = ORIENTED_EDGE ( 'NONE', *, *, #53591, .T. ) ;
#83076 = CYLINDRICAL_SURFACE ( 'NONE', #28725, 17.82106496071139645 ) ;
#83077 = CARTESIAN_POINT ( 'NONE',  ( 162.6012440678564133, 250.5872267631778527, 12.68799555347811392 ) ) ;
#83078 = CARTESIAN_POINT ( 'NONE',  ( 23.64814127513158937, 118.0650415295850451, 60.00000000000000000 ) ) ;
#83079 = VERTEX_POINT ( 'NONE', #91013 ) ;
#83081 = DIRECTION ( 'NONE',  ( 0.4999999999999998890, -0.8660254037844385966, 0.000000000000000000 ) ) ;
#83080 = VECTOR ( 'NONE', #72978, 1000.000000000000114 ) ;
#83082 = CARTESIAN_POINT ( 'NONE',  ( 79.08035272007656147, 46.14455083862815599, -12.71395590097782602 ) ) ;
#83083 = DIRECTION ( 'NONE',  ( -0.000000000000000000, -0.000000000000000000, -1.000000000000000000 ) ) ;
#83084 = CARTESIAN_POINT ( 'NONE',  ( 176.6079174955794429, 274.4222495781426687, -16.64941559833394180 ) ) ;
#83085 = DIRECTION ( 'NONE',  ( -0.000000000000000000, -0.000000000000000000, 1.000000000000000000 ) ) ;
#83086 = CARTESIAN_POINT ( 'NONE',  ( 157.1517242151937523, 258.4522244926691883, 18.42395718741238042 ) ) ;
#83087 = VERTEX_POINT ( 'NONE', #36760 ) ;
#83088 = CARTESIAN_POINT ( 'NONE',  ( 18.13223351794271565, 28.65586893147756342, -7.433330006724137462 ) ) ;
#83089 = CARTESIAN_POINT ( 'NONE',  ( 23.82048379914786906, 32.49103043416550207, -8.090169943749479842 ) ) ;
#83090 = CARTESIAN_POINT ( 'NONE',  ( 71.93104225996606260, 70.29527910854686468, -7.202640768569800400 ) ) ;
#83091 = CARTESIAN_POINT ( 'NONE',  ( 75.32522729562204233, 66.75955131866579961, -12.97495178021951290 ) ) ;
#83092 = ORIENTED_EDGE ( 'NONE', *, *, #37215, .T. ) ;
#83093 = DIRECTION ( 'NONE',  ( 0.4999999999999998890, -0.8660254037844385966, 0.000000000000000000 ) ) ;
#83094 = CARTESIAN_POINT ( 'NONE',  ( 167.2310611304565953, 261.7083964245842935, 16.31600354341965087 ) ) ;
#83095 = CARTESIAN_POINT ( 'NONE',  ( 159.3451320108506764, 254.6531307488737355, -16.72997986213134425 ) ) ;
#83096 = VERTEX_POINT ( 'NONE', #98090 ) ;
#83098 = DIRECTION ( 'NONE',  ( 0.000000000000000000, 0.000000000000000000, 1.000000000000000000 ) ) ;
#83097 = CARTESIAN_POINT ( 'NONE',  ( -18.30488606758875392, 59.85806527642789376, -10.00000000000000000 ) ) ;
#83099 = CARTESIAN_POINT ( 'NONE',  ( 207.6875671281972870, 270.9215769640275653, -2.211577121115235300 ) ) ;
#83100 = CARTESIAN_POINT ( 'NONE',  ( 65.83617023856123751, 68.96008090994861561, -2.256815018066093970 ) ) ;
#83101 = CARTESIAN_POINT ( 'NONE',  ( 188.6852239700973541, 295.1919775169639593, -11.19696146816310112 ) ) ;
#83102 = LINE ( 'NONE', #4570, #43429 ) ;
#83103 = CARTESIAN_POINT ( 'NONE',  ( 164.4977080725190319, 265.4334248489062702, -16.72650950839127049 ) ) ;
#83104 = CARTESIAN_POINT ( 'NONE',  ( 119.6326891643026613, 246.0024278399160949, -9.188101187500093303 ) ) ;
#83105 = DIRECTION ( 'NONE',  ( -0.3958915996110536351, -0.9182972510888840478, 0.000000000000000000 ) ) ;
#83106 = ORIENTED_EDGE ( 'NONE', *, *, #9716, .T. ) ;
#83107 = CARTESIAN_POINT ( 'NONE',  ( 174.1098532474522642, 265.5656642385555983, 16.65038209508332301 ) ) ;
#83108 = CARTESIAN_POINT ( 'NONE',  ( 182.5686778644665083, 296.6873302901632314, 1.787712280751329708 ) ) ;
#83109 = EDGE_CURVE ( 'NONE', #60766, #97433, #92018, .T. ) ;
#83110 = ORIENTED_EDGE ( 'NONE', *, *, #21544, .T. ) ;
#83111 = PLANE ( 'NONE',  #13743 ) ;
#83112 = EDGE_LOOP ( 'NONE', ( #46649, #10660, #41510, #81337 ) ) ;
#83113 = ORIENTED_EDGE ( 'NONE', *, *, #57821, .T. ) ;
#83114 = CARTESIAN_POINT ( 'NONE',  ( 76.26946404230704957, 64.97317754398874001, 14.67006731301515998 ) ) ;
#83115 = CARTESIAN_POINT ( 'NONE',  ( 195.0452099689448460, 291.6879811394439912, -15.84229188559630686 ) ) ;
#83116 = CARTESIAN_POINT ( 'NONE',  ( 72.82007368749162879, 224.3967562850346837, -4.648177544792955347E-16 ) ) ;
#83117 = CARTESIAN_POINT ( 'NONE',  ( 87.83451486366641348, 43.48610523111371862, -0.3240457279886222453 ) ) ;
#83118 = CARTESIAN_POINT ( 'NONE',  ( 81.32935958276657118, 56.15914934284622717, 16.09084449101850467 ) ) ;
#83119 = CARTESIAN_POINT ( 'NONE',  ( 155.6518451030846961, 261.0500913200531841, 17.91778754207898317 ) ) ;
#83120 = CARTESIAN_POINT ( 'NONE',  ( 72.82007368749162879, 224.3967562850346837, -4.648177544792955347E-16 ) ) ;
#83121 = ORIENTED_EDGE ( 'NONE', *, *, #42236, .T. ) ;
#83122 = ADVANCED_FACE ( 'NONE', ( #74803 ), #52460, .T. ) ;
#83123 = CARTESIAN_POINT ( 'NONE',  ( 152.6621968174709991, 266.2283140474973493, -17.02835521334403168 ) ) ;
#83124 = CARTESIAN_POINT ( 'NONE',  ( 85.69563749947228359, 42.25122789774620458, -8.045052972278457832E-08 ) ) ;
#83125 = EDGE_LOOP ( 'NONE', ( #63146, #78082, #45909, #12969 ) ) ;
#83126 = CARTESIAN_POINT ( 'NONE',  ( 165.3929592122126451, 286.2279243276498732, 4.432946431554212197 ) ) ;
#83127 = EDGE_CURVE ( 'NONE', #3988, #86151, #21099, .T. ) ;
#83128 = CARTESIAN_POINT ( 'NONE',  ( 76.06231244383691603, 51.24788304498655833, -15.62831804942144842 ) ) ;
#83129 = CARTESIAN_POINT ( 'NONE',  ( 174.0121777967311516, 253.3006934959134355, -7.652886187659225570 ) ) ;
#83130 = CARTESIAN_POINT ( 'NONE',  ( 205.7829192689729325, 274.2205238267313234, 11.21202327925415254 ) ) ;
#83131 = CARTESIAN_POINT ( 'NONE',  ( 196.4170778717353585, 290.4426369823788718, -17.78762421190030452 ) ) ;
#83132 = CARTESIAN_POINT ( 'NONE',  ( 195.6729656511292035, 279.4309229103643020, 16.33979319762304883 ) ) ;
#83133 = CARTESIAN_POINT ( 'NONE',  ( 164.4915767550571957, 245.7392269735623529, -6.407198159945809657 ) ) ;
#83134 = CARTESIAN_POINT ( 'NONE',  ( 136.0871718362070339, 255.5024278399161233, 9.188101187500095079 ) ) ;
#83135 = ORIENTED_EDGE ( 'NONE', *, *, #2405, .F. ) ;
#83136 = CARTESIAN_POINT ( 'NONE',  ( 28.46864935082048831, 149.7156766241961350, -22.49999999999984013 ) ) ;
#83137 = CARTESIAN_POINT ( 'NONE',  ( 85.15564232274995504, 43.25524388620375760, 4.736941226824257001 ) ) ;
#83138 = CARTESIAN_POINT ( 'NONE',  ( 155.7413558407242533, 261.8087528638905610, -16.98101007095269210 ) ) ;
#83139 = CARTESIAN_POINT ( 'NONE',  ( 79.45319113830514368, 59.16108313430871135, -16.22659794754331131 ) ) ;
#83140 = AXIS2_PLACEMENT_3D ( 'NONE', #73250, #83363, #81384 ) ;
#83141 = DIRECTION ( 'NONE',  ( -0.9599109957006544125, -0.2803049773603353279, 0.000000000000000000 ) ) ;
#83142 = ORIENTED_EDGE ( 'NONE', *, *, #10456, .T. ) ;
#83143 = CARTESIAN_POINT ( 'NONE',  ( 77.15418484582102110, 58.25238759143534395, 16.13560698115002978 ) ) ;
#83144 = CARTESIAN_POINT ( 'NONE',  ( 185.5970932491234748, 277.7727884765715771, -17.11431047842418707 ) ) ;
#83145 = AXIS2_PLACEMENT_3D ( 'NONE', #40755, #34183, #71705 ) ;
#83146 = CARTESIAN_POINT ( 'NONE',  ( 72.61844844480206973, 71.38675611224468298, -5.879003452896631288 ) ) ;
#83147 = CARTESIAN_POINT ( 'NONE',  ( 80.40171677142443230, 49.09739724853191944, 14.02116035787424231 ) ) ;
#83148 = CARTESIAN_POINT ( 'NONE',  ( 199.7212432965426103, 266.8524737126543869, 0.8277979432595076181 ) ) ;
#83149 = CARTESIAN_POINT ( 'NONE',  ( 195.1484500613037483, 263.5738921410981561, 0.8534460714690799144 ) ) ;
#83150 = VECTOR ( 'NONE', #6648, 1000.000000000000114 ) ;
#83151 = CARTESIAN_POINT ( 'NONE',  ( 190.5541309856500050, 300.5975588711562523, -4.167177996129430184 ) ) ;
#83152 = CARTESIAN_POINT ( 'NONE',  ( 182.9775332447387655, 280.7556200032468610, 17.06854547713099990 ) ) ;
#83153 = CARTESIAN_POINT ( 'NONE',  ( 204.8878784573704195, 275.7707799872745795, -14.13380496213581594 ) ) ;
#83154 = CARTESIAN_POINT ( 'NONE',  ( 195.4470299022805762, 270.3734295143469808, 12.00835009477670390 ) ) ;
#83155 = EDGE_CURVE ( 'NONE', #22415, #67005, #8038, .T. ) ;
#83156 = EDGE_CURVE ( 'NONE', #19346, #47682, #7353, .T. ) ;
#83157 = CARTESIAN_POINT ( 'NONE',  ( 21.47138989493050332, 31.13478043621388736, 8.090169943749478065 ) ) ;
#83158 = CARTESIAN_POINT ( 'NONE',  ( 190.1519139143167081, 301.2942192743771557, 4.481136594690903863 ) ) ;
#83159 = DIRECTION ( 'NONE',  ( 0.8660254037844385966, 0.5000000000000002220, 7.511572993685832627E-16 ) ) ;
#83160 = CARTESIAN_POINT ( 'NONE',  ( 71.51226778736909750, 69.30015625669656743, -9.074508208858107494 ) ) ;
#83161 = CARTESIAN_POINT ( 'NONE',  ( 197.9552487813401456, 287.7784468162186613, 17.26493623863614602 ) ) ;
#83162 = CARTESIAN_POINT ( 'NONE',  ( 72.25843749594145038, 71.93659321963055220, -3.779133617516833521 ) ) ;
#83163 = CARTESIAN_POINT ( 'NONE',  ( -6.265406815095104776, 161.0643266524160140, 9.188101187500095079 ) ) ;
#83164 = CARTESIAN_POINT ( 'NONE',  ( 173.5307509579417342, 284.0411775505230594, -12.16872317665307079 ) ) ;
#83165 = ORIENTED_EDGE ( 'NONE', *, *, #18180, .T. ) ;
#83166 = ADVANCED_FACE ( 'NONE', ( #23040 ), #6859, .T. ) ;
#83167 = CARTESIAN_POINT ( 'NONE',  ( 66.47301154247004717, 67.89115917382773091, -6.669687514284739827 ) ) ;
#83168 = CARTESIAN_POINT ( 'NONE',  ( -19.65312891409030271, 93.06504152958497400, 59.99999999999999289 ) ) ;
#83169 = CARTESIAN_POINT ( 'NONE',  ( 151.0013883899287066, 269.1049186256390726, -14.25461351222133466 ) ) ;
#83170 = CARTESIAN_POINT ( 'NONE',  ( 1.284818304444202530, 180.7369531367911293, -4.594050593750048428 ) ) ;
#83171 = CARTESIAN_POINT ( 'NONE',  ( 181.6464193077049458, 276.3867670284828932, -17.07225131682299946 ) ) ;
#83172 = CARTESIAN_POINT ( 'NONE',  ( 18.29780494541646974, 34.65659080271451842, -1.878358725466461243E-16 ) ) ;
#83173 = CARTESIAN_POINT ( 'NONE',  ( -52.24036053731629892, 86.53868222403792743, -10.00000000000000000 ) ) ;
#83174 = CARTESIAN_POINT ( 'NONE',  ( 170.2422670303552081, 270.8252190829385881, -17.42252638875442017 ) ) ;
#83175 = CARTESIAN_POINT ( 'NONE',  ( 71.68807920414248258, 72.06984970416017688, -3.563505611461031286 ) ) ;
#83176 = CARTESIAN_POINT ( 'NONE',  ( 81.74119788692269140, 59.14441083166271795, 0.000000000000000000 ) ) ;
#83177 = ADVANCED_FACE ( 'NONE', ( #60048 ), #92494, .F. ) ;
#83179 = CARTESIAN_POINT ( 'NONE',  ( 73.11106055086588640, 213.0177522451418497, -10.00000000000009592 ) ) ;
#83178 = CARTESIAN_POINT ( 'NONE',  ( 196.3462811589356249, 269.2578400835121215, -10.58958620393924477 ) ) ;
#83180 = ADVANCED_FACE ( 'NONE', ( #53936 ), #83023, .F. ) ;
#83181 = CARTESIAN_POINT ( 'NONE',  ( 177.0233654624311725, 254.4087770924622873, -3.874647819833805240 ) ) ;
#83182 = CARTESIAN_POINT ( 'NONE',  ( 197.9679655381963244, 287.7564207472362341, 17.61949439995294497 ) ) ;
#83183 = CARTESIAN_POINT ( 'NONE',  ( 180.8886826254641846, 294.5332475160486183, 1.019920492680034263 ) ) ;
#83184 = CARTESIAN_POINT ( 'NONE',  ( 45.92147131476482969, 203.9865022471903444, -10.00000000000009415 ) ) ;
#83185 = CARTESIAN_POINT ( 'NONE',  ( 110.0000000000000000, 0.000000000000000000, -59.99999999999999289 ) ) ;
#83186 = CARTESIAN_POINT ( 'NONE',  ( 190.5893431400089923, 300.5365696307625853, -0.3099240395267599535 ) ) ;
#83187 = CARTESIAN_POINT ( 'NONE',  ( 23.53136650780448491, 175.2048013555409796, 4.594050593750051981 ) ) ;
#83188 = CARTESIAN_POINT ( 'NONE',  ( 164.6285367961174870, 284.7931077284160892, 4.211549190166783418 ) ) ;
#83189 = DIRECTION ( 'NONE',  ( 0.000000000000000000, 0.000000000000000000, 1.000000000000000000 ) ) ;
#83190 = CARTESIAN_POINT ( 'NONE',  ( 35.63920408047906818, 43.68290643055190969, 3.479690158560446702E-15 ) ) ;
#83191 = DIRECTION ( 'NONE',  ( -0.000000000000000000, -0.000000000000000000, 1.000000000000000000 ) ) ;
#83192 = CARTESIAN_POINT ( 'NONE',  ( 189.1023583995641104, 268.2289247844391866, 13.73749984714365091 ) ) ;
#83193 = CARTESIAN_POINT ( 'NONE',  ( 67.16990927169524639, 66.79708245693808522, -9.067759095298590921 ) ) ;
#83194 = CARTESIAN_POINT ( 'NONE',  ( 164.1193093486783710, 281.5602788190849424, 8.891021254689583486 ) ) ;
#83195 = CARTESIAN_POINT ( 'NONE',  ( 18.76490627030545610, 13.76004757982088655, 5.678558825948272215 ) ) ;
#83196 = CARTESIAN_POINT ( 'NONE',  ( 6.430760413625676186, 27.21091486745858390, -1.111400068045478839E-16 ) ) ;
#83197 = CARTESIAN_POINT ( 'NONE',  ( 82.78422215508307147, 53.78621188977052725, 15.78456841880229433 ) ) ;
#83198 = CARTESIAN_POINT ( 'NONE',  ( 71.39729339694994792, 59.37714758514961488, 15.21381503262609414 ) ) ;
#83199 = CARTESIAN_POINT ( 'NONE',  ( 193.7901930790854976, 294.9925349088783264, 14.24765323155741115 ) ) ;
#83200 = VERTEX_POINT ( 'NONE', #77529 ) ;
#83201 = CARTESIAN_POINT ( 'NONE',  ( 185.0212309258022856, 290.7568242972342887, 12.15772952871526336 ) ) ;
#83202 = DIRECTION ( 'NONE',  ( -0.8756465943326185997, -0.4829524219151267728, 0.000000000000000000 ) ) ;
#83203 = CARTESIAN_POINT ( 'NONE',  ( 81.58052743141770691, 41.99578084072658157, 7.590836836702154145 ) ) ;
#83204 = ORIENTED_EDGE ( 'NONE', *, *, #88763, .F. ) ;
#83205 = CARTESIAN_POINT ( 'NONE',  ( 158.2129804214947058, 265.2348010298870236, 17.61986633405762603 ) ) ;
#83206 = DIRECTION ( 'NONE',  ( -0.000000000000000000, 0.000000000000000000, -1.000000000000000000 ) ) ;
#83207 = CARTESIAN_POINT ( 'NONE',  ( 26.39215011307057424, 23.43677371833802425, -10.00000000000000355 ) ) ;
#83208 = CARTESIAN_POINT ( 'NONE',  ( 203.3205561747472814, 278.4854618126124706, -15.14439614831292147 ) ) ;
#83209 = COLOUR_RGB ( '',0.7921568627450980005, 0.8196078431372548767, 0.9333333333333333481 ) ;
#83210 = ORIENTED_EDGE ( 'NONE', *, *, #61054, .T. ) ;
#83211 = ORIENTED_EDGE ( 'NONE', *, *, #55878, .F. ) ;
#83213 = DIRECTION ( 'NONE',  ( -0.8660254037844387076, -0.4999999999999998890, -0.000000000000000000 ) ) ;
#83212 = CARTESIAN_POINT ( 'NONE',  ( 186.9124060917193333, 272.1944072449207965, -16.74496829271420850 ) ) ;
#83214 = ORIENTED_EDGE ( 'NONE', *, *, #24624, .T. ) ;
#83215 = CARTESIAN_POINT ( 'NONE',  ( 191.0170959869219303, 299.7956799668270946, 7.353346939903929069 ) ) ;
#83216 = FACE_OUTER_BOUND ( 'NONE', #12686, .T. ) ;
#83217 = CARTESIAN_POINT ( 'NONE',  ( 80.65095556854913639, 57.57228308630149627, 16.58706730796347628 ) ) ;
#83218 = CARTESIAN_POINT ( 'NONE',  ( 73.05863210132505969, 69.60576123971951290, -9.808587366596233537 ) ) ;
#83219 = ORIENTED_EDGE ( 'NONE', *, *, #10174, .T. ) ;
#83220 = DIRECTION ( 'NONE',  ( -0.000000000000000000, 0.000000000000000000, 1.000000000000000000 ) ) ;
#83221 = EDGE_CURVE ( 'NONE', #18761, #54490, #53215, .T. ) ;
#83222 = ORIENTED_EDGE ( 'NONE', *, *, #54183, .F. ) ;
#83223 = CARTESIAN_POINT ( 'NONE',  ( 164.4573439719129340, 245.7985198932525748, 1.541132361166968501 ) ) ;
#83224 = CARTESIAN_POINT ( 'NONE',  ( 74.76978274660817192, 64.43581441273093446, 14.05910472376388398 ) ) ;
#83225 = VERTEX_POINT ( 'NONE', #15193 ) ;
#83226 = CARTESIAN_POINT ( 'NONE',  ( 149.0802055316563326, 272.4325049467973940, 12.84384348890831085 ) ) ;
#83227 = CARTESIAN_POINT ( 'NONE',  ( 172.3329631802389201, 263.6870992125010389, -15.46481966459473689 ) ) ;
#83228 = EDGE_CURVE ( 'NONE', #49659, #80879, #31093, .T. ) ;
#83229 = ORIENTED_EDGE ( 'NONE', *, *, #35895, .F. ) ;
#83230 = CARTESIAN_POINT ( 'NONE',  ( -22.42236680055709641, 157.8615022471902591, 0.000000000000000000 ) ) ;
#83231 = CARTESIAN_POINT ( 'NONE',  ( 82.93017357788667709, 175.3855496052738374, 36.50000000000000000 ) ) ;
#83232 = EDGE_LOOP ( 'NONE', ( #60363, #24852, #68871, #52783, #81504, #97656 ) ) ;
#83233 = ORIENTED_EDGE ( 'NONE', *, *, #91858, .F. ) ;
#83234 = CARTESIAN_POINT ( 'NONE',  ( 153.8480465357228013, 265.0660884932569843, -16.61306390558784685 ) ) ;
#83235 = CARTESIAN_POINT ( 'NONE',  ( 147.5492216329511166, 275.0842468449245644, 4.751613690710122739 ) ) ;
#83236 = CARTESIAN_POINT ( 'NONE',  ( 82.47797010013799479, 53.85630837337446764, 15.85289899457425022 ) ) ;
#83237 = CARTESIAN_POINT ( 'NONE',  ( 83.90596095485256001, 41.21795184261720379, -1.108148245180562033E-06 ) ) ;
#83238 = CARTESIAN_POINT ( 'NONE',  ( 153.1745822862813498, 265.3408363824576668, 16.18092354043443493 ) ) ;
#83239 = ADVANCED_FACE ( 'NONE', ( #8615 ), #29914, .F. ) ;
#83240 = CARTESIAN_POINT ( 'NONE',  ( 191.5641729352803395, 298.8481148966207570, 9.839145202254165667 ) ) ;
#83241 = CARTESIAN_POINT ( 'NONE',  ( 191.6823192895500370, 298.6434794082964572, -8.424208857102787107 ) ) ;
#83242 = EDGE_LOOP ( 'NONE', ( #90224, #84156, #53857, #13373 ) ) ;
#83243 = CARTESIAN_POINT ( 'NONE',  ( 87.35668359673078953, 44.84080960044052233, -6.701380392922977158 ) ) ;
#83244 = CARTESIAN_POINT ( 'NONE',  ( 206.4943150373521803, 272.9883502116088039, 11.34100825923693101 ) ) ;
#83246 = CARTESIAN_POINT ( 'NONE',  ( 49.83874514172083536, 101.4840343560033915, 10.00000000000000000 ) ) ;
#83245 = CARTESIAN_POINT ( 'NONE',  ( 196.7491951525289835, 289.8673929779723721, -16.35352603081977207 ) ) ;
#83247 = CARTESIAN_POINT ( 'NONE',  ( -46.96828164281857454, 74.13349478725223207, -10.00000000000000000 ) ) ;
#83248 = CARTESIAN_POINT ( 'NONE',  ( 169.1455093422647167, 286.8367317026995238, 4.082882422040602144 ) ) ;
#83249 = CARTESIAN_POINT ( 'NONE',  ( 177.0647803954294375, 289.2179056399639876, -8.988518407010369415 ) ) ;
#83250 = ORIENTED_EDGE ( 'NONE', *, *, #24339, .T. ) ;
#83251 = CARTESIAN_POINT ( 'NONE',  ( 190.6733132232214984, 300.3911291803227641, -3.379496780928331390 ) ) ;
#83252 = CARTESIAN_POINT ( 'NONE',  ( 79.75798450490407276, 52.95241734746561946, -15.59895281915799004 ) ) ;
#83253 = CARTESIAN_POINT ( 'NONE',  ( 84.83954103072970554, 42.64226960066435623, 4.998593534305094899 ) ) ;
#83254 = ADVANCED_FACE ( 'NONE', ( #45596 ), #23298, .F. ) ;
#83255 = CARTESIAN_POINT ( 'NONE',  ( 79.70677143370977547, 46.01134058545614636, 12.98241517805147538 ) ) ;
#83256 = B_SPLINE_CURVE_WITH_KNOTS ( 'NONE', 3,
 ( #38055, #82740, #75106, #91818 ),
 .UNSPECIFIED., .F., .F.,
 ( 4, 4 ),
 ( 0.005284111372439467477, 0.01027133156736889999 ),
 .UNSPECIFIED. ) ;
#83257 = EDGE_CURVE ( 'NONE', #95321, #69469, #80958, .T. ) ;
#83258 = CARTESIAN_POINT ( 'NONE',  ( 191.8935548119142425, 297.8494204854303007, -9.596788447830101987 ) ) ;
#83259 = FACE_OUTER_BOUND ( 'NONE', #8835, .T. ) ;
#83260 = ORIENTED_EDGE ( 'NONE', *, *, #18696, .F. ) ;
#83261 = CARTESIAN_POINT ( 'NONE',  ( 163.2742264920156572, 247.8477394797576778, -9.850275379362519956 ) ) ;
#83262 = CARTESIAN_POINT ( 'NONE',  ( -19.65312891409030271, 93.06504152958497400, 60.00000000000000000 ) ) ;
#83263 = B_SPLINE_CURVE_WITH_KNOTS ( 'NONE', 3,
 ( #87129, #65248, #10563, #3477, #34352, #34835, #25249, #26755, #63755, #41439, #78987, #72379, #55628, #94688, #57638, #9574, #19181, #65737, #50053, #11571, #71874, #86613, #71372, #64764, #17662, #2988, #48560, #17146, #40437, #87633, #49061, #25773, #79501, #10062, #2472, #33353, #18161, #79995, #20165, #27756, #59624, #12563, #82507, #58143, #67746, #89123, #66253, #60120, #90600, #21648 ),
 .UNSPECIFIED., .F., .F.,
 ( 4, 2, 2, 2, 2, 2, 2, 2, 2, 2, 2, 2, 2, 2, 2, 2, 2, 2, 2, 2, 2, 2, 2, 2, 4 ),
 ( 0.0008342906553197565857, 0.001033266195178259104, 0.001132753965107476807, 0.001232241735036694727, 0.001431217274895130349, 0.001630192814753566189, 0.002028143894470437868, 0.002426094974187309114, 0.003221997133621052039, 0.004017899293054795831, 0.004813801452488538322, 0.005211752532205410002, 0.005410728072063810713, 0.005510215841993010635, 0.005609703611922210557, 0.005659447496886774523, 0.005709191381851337621, 0.005808679151780464685, 0.006007654691638748302, 0.006206630231497031920, 0.006405605771355314670, 0.006604581311213598288, 0.006803556851071881906, 0.007002532390930164656, 0.007201507930788447406 ),
 .UNSPECIFIED. ) ;
#83264 = CARTESIAN_POINT ( 'NONE',  ( 207.6900289502458179, 270.9173129631602706, 7.178327969100043227 ) ) ;
#83265 = CARTESIAN_POINT ( 'NONE',  ( 52.25428207639071587, 187.6427522451417644, 1.119607411625061291E-15 ) ) ;
#83266 = CARTESIAN_POINT ( 'NONE',  ( 116.7098534265301737, 244.3149278399160949, -9.188101187500095079 ) ) ;
#83267 = CARTESIAN_POINT ( 'NONE',  ( 172.7371573690596449, 271.6299009131761864, 17.79590902495428040 ) ) ;
#83268 = CARTESIAN_POINT ( 'NONE',  ( 20.67738335769525904, 35.85097175740956033, 177.5919119679930134 ) ) ;
#83269 = CARTESIAN_POINT ( 'NONE',  ( 195.7578697689113199, 291.5844189092309193, 17.18796537138345215 ) ) ;
#83270 = CARTESIAN_POINT ( 'NONE',  ( 174.2336437131566527, 252.7393380672576200, -3.889790898222944104 ) ) ;
#83271 = CARTESIAN_POINT ( 'NONE',  ( 36.95476026646328194, 182.9548013555409796, -4.594050593750042211 ) ) ;
#83272 = CARTESIAN_POINT ( 'NONE',  ( 41.71240375114938814, 62.05720181600818108, -10.00000000000000000 ) ) ;
#83273 = ORIENTED_EDGE ( 'NONE', *, *, #10268, .F. ) ;
#83274 = CARTESIAN_POINT ( 'NONE',  ( -13.11024591527723615, 15.00000000000000000, -32.50000000000017053 ) ) ;
#83275 = CARTESIAN_POINT ( 'NONE',  ( 74.23941942568015406, 67.87611062571697573, -11.69065606785908251 ) ) ;
#83276 = EDGE_CURVE ( 'NONE', #77883, #26521, #7609, .T. ) ;
#83277 = B_SPLINE_CURVE_WITH_KNOTS ( 'NONE', 3,
 ( #17751, #10146, #25332, #79078, #64337, #95298, #47126, #78049, #23823, #56218, #9140, #87216, #86693, #8639, #55703, #49145, #9660, #40520, #79585, #39505, #70953, #16734, #25856, #32438, #41014, #71953, #2556, #71454, #63335, #47625, #31921, #2045, #69923, #94274, #70432, #62825, #24830, #24340, #56732, #32930 ),
 .UNSPECIFIED., .F., .F.,
 ( 4, 2, 2, 2, 2, 2, 2, 2, 2, 2, 2, 2, 2, 2, 2, 2, 2, 2, 2, 4 ),
 ( 0.0009087385142839295420, 0.001001542006469175903, 0.001094345498654422048, 0.001279952483024912602, 0.001651166451765993456, 0.002393594389248154299, 0.003878450264212475983, 0.004620878201694636825, 0.004992092170435751507, 0.005177699154806264178, 0.005270502646991520948, 0.005363306139176776850, 0.005409707885269485900, 0.005456109631362194082, 0.005548913123547547996, 0.005734520107918297457, 0.006105734076659791176, 0.006476948045401284028, 0.006662555029771971907, 0.006848162014142659786 ),
 .UNSPECIFIED. ) ;
#83278 = LINE ( 'NONE', #44230, #31923 ) ;
#83279 = CARTESIAN_POINT ( 'NONE',  ( 190.8907028847385448, 300.0145992415348815, -5.421341690443150618 ) ) ;
#83280 = CARTESIAN_POINT ( 'NONE',  ( 81.89040035157415787, 41.13959363232161337, -5.507854768277897328 ) ) ;
#83281 = VECTOR ( 'NONE', #97246, 1000.000000000000000 ) ;
#83282 = CARTESIAN_POINT ( 'NONE',  ( -72.81784413424506397, 47.52919789448971244, 177.5919119679930134 ) ) ;
#83283 = DIRECTION ( 'NONE',  ( -0.000000000000000000, -0.000000000000000000, 1.000000000000000000 ) ) ;
#83284 = CARTESIAN_POINT ( 'NONE',  ( 6.117390533544194930, 29.33055864014943026, -10.00000000000000000 ) ) ;
#83285 = EDGE_CURVE ( 'NONE', #29236, #70733, #77736, .T. ) ;
#83286 = CARTESIAN_POINT ( 'NONE',  ( 95.62772104926125394, 236.0177522451419350, 5.000000000000046185 ) ) ;
#83287 = B_SPLINE_SURFACE_WITH_KNOTS ( 'NONE', 3, 1, ( 
 ( #66244, #88606 ),
 ( #97181, #20157 ),
 ( #51025, #12554 ),
 ( #50044, #59106 ),
 ( #90078, #20647 ),
 ( #51535, #82497 ),
 ( #13062, #72371 ),
 ( #2977, #33869 ),
 ( #57125, #88108 ),
 ( #49537, #80491 ),
 ( #90592, #68719 ),
 ( #67736, #6922 ),
 ( #82976, #22630 ),
 ( #61610, #45416 ),
 ( #92564, #45899 ),
 ( #37317, #67228 ),
 ( #29243, #52036 ),
 ( #91559, #52521 ),
 ( #76348, #13550 ),
 ( #61109, #30225 ),
 ( #76821, #91075 ),
 ( #98659, #99643 ),
 ( #37809, #83470 ),
 ( #14034, #36827 ),
 ( #44914, #75859 ),
 ( #22128, #60109 ),
 ( #7416, #21638 ),
 ( #15009, #6440 ),
 ( #44424, #83974 ),
 ( #68218, #99143 ),
 ( #75353, #29730 ),
 ( #92082, #60604 ),
 ( #59612, #36326 ),
 ( #21157, #53516 ) ),
 .UNSPECIFIED., .T., .F., .F.,
 ( 4, 2, 2, 2, 2, 2, 2, 2, 2, 2, 2, 2, 2, 2, 2, 2, 4 ),
 ( 2, 2 ),
 ( 0.000000000000000000, 0.06250000000000000000, 0.1250000000000000000, 0.1875000000000000000, 0.2500000000000000000, 0.3125000000000000000, 0.3750000000000000000, 0.4375000000000000000, 0.5000000000000000000, 0.5625000000000000000, 0.6250000000000000000, 0.6875000000000000000, 0.7500000000000000000, 0.8125000000000000000, 0.8750000000000000000, 0.9375000000000000000, 1.000000000000000000 ),
 ( 0.000000000000000000, 1.000000000000000000 ),
 .UNSPECIFIED. ) ;
#83288 = ORIENTED_EDGE ( 'NONE', *, *, #38385, .F. ) ;
#83289 = CARTESIAN_POINT ( 'NONE',  ( 79.16072033191956336, 59.43364827697804742, -16.53552069436850402 ) ) ;
#83290 = AXIS2_PLACEMENT_3D ( 'NONE', #43930, #29252, #73858 ) ;
#83291 = EDGE_CURVE ( 'NONE', #31851, #21922, #39482, .T. ) ;
#83292 = CARTESIAN_POINT ( 'NONE',  ( 163.4222916751007801, 247.5912830598222172, -10.52132777929285012 ) ) ;
#83293 = ADVANCED_FACE ( 'NONE', ( #62289 ), #52232, .F. ) ;
#83294 = CARTESIAN_POINT ( 'NONE',  ( 15.54743449484293372, 179.7833772461660544, -9.188101187500095079 ) ) ;
#83295 = CARTESIAN_POINT ( 'NONE',  ( 9.265696904164599346, 17.30066082961419838, -10.00000000000000533 ) ) ;
#83296 = CARTESIAN_POINT ( 'NONE',  ( 195.6045292168243463, 273.5821757523950168, 14.58780494107374359 ) ) ;
#83297 = CARTESIAN_POINT ( 'NONE',  ( 71.60869501579809082, 58.97949029833907986, -15.86055346694359436 ) ) ;
#83298 = B_SPLINE_CURVE_WITH_KNOTS ( 'NONE', 3,
 ( #16782, #95354, #88251, #9713, #2101, #32981, #17802, #56274, #63886, #40066, #18799, #94822, #25386, #32496, #49681, #64390 ),
 .UNSPECIFIED., .F., .F.,
 ( 4, 1, 2, 2, 2, 1, 2, 2, 4 ),
 ( 0.000000000000000000, 0.1250000000000022760, 0.1875000000000034972, 0.2500000000000047184, 0.5000000000000039968, 0.6250000000000035527, 0.6875000000000034417, 0.7500000000000032196, 1.000000000000000000 ),
 .UNSPECIFIED. ) ;
#83299 = CARTESIAN_POINT ( 'NONE',  ( -27.42236680055714260, 166.5217562850347406, 1.224646799147364892E-15 ) ) ;
#83301 = EDGE_CURVE ( 'NONE', #57995, #26530, #68482, .T. ) ;
#83300 = B_SPLINE_CURVE_WITH_KNOTS ( 'NONE', 3,
 ( #79912, #71788, #33266, #50458, #2386, #19597, #41352, #34756, #2900, #65656, #3873, #10475, #64678, #18081, #25681, #64169, #66167, #72805, #49463, #50953, #72294, #41863, #95117, #95628, #42837, #87548, #96614, #26176, #58065, #11981, #57054, #42349, #89048, #80418, #81408, #88036, #3394, #18584, #4364, #80928, #65163, #26669, #57554, #35260, #88531, #82903, #76273, #14460 ),
 .UNSPECIFIED., .F., .F.,
 ( 4, 2, 2, 2, 2, 2, 2, 2, 2, 2, 2, 2, 2, 2, 2, 2, 2, 2, 2, 2, 2, 2, 2, 4 ),
 ( 0.0008776508359081067320, 0.0009741453280959741544, 0.001070639820283841468, 0.001167134312471708891, 0.001263628804659576313, 0.001456617789035311375, 0.001649606773411046220, 0.002421562710914172082, 0.003965474585920503170, 0.004737430523423668931, 0.005123408492175214948, 0.005316397476551025687, 0.005412891968738894194, 0.005461139214832867045, 0.005509386460926840763, 0.005557633707020814481, 0.005605880953114787332, 0.005702375445302676656, 0.005895364429678470915, 0.006088353414054266041, 0.006281342398430060300, 0.006474331382805854559, 0.006667320367181648819, 0.007053298335933237337 ),
 .UNSPECIFIED. ) ;
#83303 = CARTESIAN_POINT ( 'NONE',  ( 44.28847903505648986, 202.5024278399160949, -9.188101187500093303 ) ) ;
#83302 = CARTESIAN_POINT ( 'NONE',  ( 174.2608556768636561, 287.0962246304461587, 10.28298298902735830 ) ) ;
#83304 = DIRECTION ( 'NONE',  ( -0.4831861483251571610, -0.8755176446347036068, 0.000000000000000000 ) ) ;
#83305 = CARTESIAN_POINT ( 'NONE',  ( 72.83288601605435986, 57.14714021852967818, 15.89844244041831089 ) ) ;
#83306 = CARTESIAN_POINT ( 'NONE',  ( -36.52772323645827868, 26.41323893245353105, -10.00000000000000000 ) ) ;
#83307 = CARTESIAN_POINT ( 'NONE',  ( 66.08643694688238668, 68.49314833729727070, -4.715610728220657855 ) ) ;
#83308 = ORIENTED_EDGE ( 'NONE', *, *, #1628, .F. ) ;
#83309 = CARTESIAN_POINT ( 'NONE',  ( 5.218277336896219865, 180.4865022471902876, 10.00000000000009237 ) ) ;
#83310 = CARTESIAN_POINT ( 'NONE',  ( 163.7323023463233937, 247.0543288263758086, -6.244751637846886361 ) ) ;
#83311 = CARTESIAN_POINT ( 'NONE',  ( 134.5444773117747275, 257.6744531367911577, 4.594050593750047540 ) ) ;
#83312 = CARTESIAN_POINT ( 'NONE',  ( 30.20304716546516133, 19.29860640527293469, -2.839279412974138328 ) ) ;
#83313 = CARTESIAN_POINT ( 'NONE',  ( 165.0596455280890211, 244.7553029964778943, 1.410246537223424079 ) ) ;
#83314 = CARTESIAN_POINT ( 'NONE',  ( 83.76909922093737748, 51.72725043056325234, -14.84865573977556075 ) ) ;
#83315 = CARTESIAN_POINT ( 'NONE',  ( 64.45080651302146180, 218.0177522451419065, 5.000000000000046185 ) ) ;
#83317 = CARTESIAN_POINT ( 'NONE',  ( 189.5697419595462918, 289.6068222778108066, 15.26551028775433494 ) ) ;
#83316 = CARTESIAN_POINT ( 'NONE',  ( 88.44572534255364360, 43.94768732639446540, 1.766277459783989867 ) ) ;
#83318 = CARTESIAN_POINT ( 'NONE',  ( 68.46226156283634623, 64.36458740167765313, 12.29825945318413005 ) ) ;
#83319 = VERTEX_POINT ( 'NONE', #623 ) ;
#83320 = FACE_OUTER_BOUND ( 'NONE', #49060, .T. ) ;
#83321 = CARTESIAN_POINT ( 'NONE',  ( -13.82959147685579104, 104.2312461070085021, 43.93259070532315036 ) ) ;
#83322 = CARTESIAN_POINT ( 'NONE',  ( 151.5039520077037309, 268.6434754965026173, -14.46698723261350317 ) ) ;
#83323 = FACE_OUTER_BOUND ( 'NONE', #53314, .T. ) ;
#83324 = CARTESIAN_POINT ( 'NONE',  ( 7.127696690345725727, 16.06628583063839244, -9.188101187500006262 ) ) ;
#83325 = VERTEX_POINT ( 'NONE', #23911 ) ;
#83326 = CARTESIAN_POINT ( 'NONE',  ( 72.23865006290039048, 71.95475215217994958, 3.607730569270007237 ) ) ;
#83327 = CIRCLE ( 'NONE', #97909, 17.82106496071138224 ) ;
#83328 = CARTESIAN_POINT ( 'NONE',  ( 83.47336872178040323, 41.48982131955913388, -3.853860643902951022 ) ) ;
#83329 = CARTESIAN_POINT ( 'NONE',  ( 71.67183227515569399, 72.09799021063221858, 0.6624418287695852392 ) ) ;
#83330 = LINE ( 'NONE', #53863, #34436 ) ;
#83331 = CARTESIAN_POINT ( 'NONE',  ( 196.1377568310088293, 271.0462798384791654, 12.65795514811142297 ) ) ;
#83332 = CARTESIAN_POINT ( 'NONE',  ( 184.7485916865611557, 296.0552073707631848, 4.660200707592978553 ) ) ;
#83333 = CARTESIAN_POINT ( 'NONE',  ( 208.3790849386676598, 269.7238329819538762, -1.525282248498321946 ) ) ;
#83334 = CARTESIAN_POINT ( 'NONE',  ( 72.91946395511783408, 57.64528416996791549, -16.31297782416237752 ) ) ;
#83335 = DIRECTION ( 'NONE',  ( -0.000000000000000000, 0.000000000000000000, -1.000000000000000000 ) ) ;
#83336 = CARTESIAN_POINT ( 'NONE',  ( 15.82880751958831667, 10.10801979619927415, 3.090169943749476733 ) ) ;
#83337 = CARTESIAN_POINT ( 'NONE',  ( 79.99999999999998579, 9.999999999999985789, 2.622423327744133559 ) ) ;
#83338 = EDGE_LOOP ( 'NONE', ( #80031, #80924, #95692, #36966 ) ) ;
#83339 = CARTESIAN_POINT ( 'NONE',  ( 167.4841441875519763, 281.4071184892553106, 13.00054054298708905 ) ) ;
#83340 = CARTESIAN_POINT ( 'NONE',  ( 32.30839531297598910, 123.0650415295850593, 203.6502102582797420 ) ) ;
#83341 = CARTESIAN_POINT ( 'NONE',  ( 191.2827847134780654, 298.6246597018299553, 8.274781095337747416 ) ) ;
#83342 = ORIENTED_EDGE ( 'NONE', *, *, #94957, .F. ) ;
#83343 = DIRECTION ( 'NONE',  ( 0.8660254037844382635, 0.5000000000000005551, 0.000000000000000000 ) ) ;
#83344 = CARTESIAN_POINT ( 'NONE',  ( 173.0842903984389807, 255.2088337646690661, -11.69841797509658399 ) ) ;
#83345 = B_SPLINE_CURVE_WITH_KNOTS ( 'NONE', 3,
 ( #29726, #43918, #60600, #15005 ),
 .UNSPECIFIED., .F., .F.,
 ( 4, 4 ),
 ( 0.04023740652969061415, 0.04865954048918677555 ),
 .UNSPECIFIED. ) ;
#83346 = CARTESIAN_POINT ( 'NONE',  ( 164.1259971043086239, 246.3724295028720519, 5.761669507629934905 ) ) ;
#83347 = DIRECTION ( 'NONE',  ( -0.03304531753666253152, -0.9994538543569188027, 0.000000000000000000 ) ) ;
#83348 = FACE_OUTER_BOUND ( 'NONE', #69632, .T. ) ;
#83349 = ORIENTED_EDGE ( 'NONE', *, *, #37774, .T. ) ;
#83350 = CARTESIAN_POINT ( 'NONE',  ( 96.60225995211651195, 217.3923013555410080, 4.594050593750050204 ) ) ;
#83351 = CARTESIAN_POINT ( 'NONE',  ( 176.6943099527350682, 256.7931168052207340, -11.17617521364210731 ) ) ;
#83352 = CARTESIAN_POINT ( 'NONE',  ( 73.17137018064387632, 69.60265530810194434, -9.888782888319330056 ) ) ;
#83353 = CARTESIAN_POINT ( 'NONE',  ( 67.09339416431679126, 69.57934519908948801, 2.872329545031587994 ) ) ;
#83354 = CARTESIAN_POINT ( 'NONE',  ( 81.42800912266413604, 42.13481243118283714, -7.961906169233770925 ) ) ;
#83355 = ORIENTED_EDGE ( 'NONE', *, *, #23835, .T. ) ;
#83356 = EDGE_LOOP ( 'NONE', ( #52066, #20574, #77983, #3222 ) ) ;
#83357 = VERTEX_POINT ( 'NONE', #30520 ) ;
#83358 = CARTESIAN_POINT ( 'NONE',  ( -38.35373792487678202, 26.90998726756845727, -10.00000000000000000 ) ) ;
#83359 = ORIENTED_EDGE ( 'NONE', *, *, #34570, .F. ) ;
#83360 = CARTESIAN_POINT ( 'NONE',  ( -17.42236680055705023, 149.2012482093457777, 0.000000000000000000 ) ) ;
#83361 = CARTESIAN_POINT ( 'NONE',  ( 87.86298961015023679, 44.89260222163544256, 6.207647304897665919 ) ) ;
#83362 = ORIENTED_EDGE ( 'NONE', *, *, #91115, .F. ) ;
#83363 = DIRECTION ( 'NONE',  ( -1.082076799516502080E-16, 0.000000000000000000, -1.000000000000000000 ) ) ;
#83364 =( BOUNDED_CURVE ( )  B_SPLINE_CURVE ( 2, ( #1585, #1071, #79104, #78077, #63365, #47646, #46140, #78583, #16758 ),
 .UNSPECIFIED., .F., .T. ) 
 B_SPLINE_CURVE_WITH_KNOTS ( ( 3, 2, 2, 2, 3 ),
 ( 0.2540322580645161255, 0.2553763440860215006, 0.2580645161290322509, 0.2607526881720430012, 0.2620967741935483764 ),
 .UNSPECIFIED. ) 
 CURVE ( )  GEOMETRIC_REPRESENTATION_ITEM ( )  RATIONAL_B_SPLINE_CURVE ( ( 0.9330127018922194093, 0.9330127018922194093, 1.000000000000000000, 0.8660254037844387076, 1.000000000000000000, 0.8660254037844387076, 1.000000000000000000, 0.9330127018922194093, 0.9330127018922194093 ) ) 
 REPRESENTATION_ITEM ( '' )  );
#83365 = CYLINDRICAL_SURFACE ( 'NONE', #89991, 70.00000000000002842 ) ;
#83366 = CARTESIAN_POINT ( 'NONE',  ( -23.39891821046326825, 99.75293890535058949, 45.19937630303414977 ) ) ;
#83368 = EDGE_CURVE ( 'NONE', #99756, #32094, #86672, .T. ) ;
#83367 = VECTOR ( 'NONE', #26959, 1000.000000000000000 ) ;
#83369 = CARTESIAN_POINT ( 'NONE',  ( 82.85943510349244434, 53.46362409593341170, -15.31598598672309031 ) ) ;
#83370 = CARTESIAN_POINT ( 'NONE',  ( 165.0565896242556505, 264.4795236785039947, -17.06046605472587530 ) ) ;
#83371 = EDGE_LOOP ( 'NONE', ( #35476, #64748, #92826, #66338 ) ) ;
#83372 = DIRECTION ( 'NONE',  ( 0.8660254037844379305, 0.5000000000000014433, 0.000000000000000000 ) ) ;
#83373 = CARTESIAN_POINT ( 'NONE',  ( 18.12859834787737157, 11.26216523072493736, -2.296566073217252530E-15 ) ) ;
#83374 = ORIENTED_EDGE ( 'NONE', *, *, #18453, .T. ) ;
#83375 = CARTESIAN_POINT ( 'NONE',  ( 164.1511151698870492, 281.6580413806572096, 8.784358064721770276 ) ) ;
#83377 = ORIENTED_EDGE ( 'NONE', *, *, #13487, .F. ) ;
#83376 = CARTESIAN_POINT ( 'NONE',  ( 11.55108809852201190, 184.1427522451419634, 10.00000000000009415 ) ) ;
#83378 = CARTESIAN_POINT ( 'NONE',  ( 162.6264071486809542, 248.9697954965390920, 10.36322805486644683 ) ) ;
#83379 = CARTESIAN_POINT ( 'NONE',  ( 188.1606188679294576, 260.7699807044755289, 2.827598859516843532 ) ) ;
#83380 = CARTESIAN_POINT ( 'NONE',  ( 161.3495717744529259, 281.4625470895858257, -6.539439586222937528 ) ) ;
#83381 = ADVANCED_FACE ( 'NONE', ( #55298 ), #79167, .T. ) ;
#83382 = CARTESIAN_POINT ( 'NONE',  ( 77.17818405207798094, 49.57096083066192449, -15.48190036198286101 ) ) ;
#83383 = FACE_OUTER_BOUND ( 'NONE', #40061, .T. ) ;
#83384 = EDGE_CURVE ( 'NONE', #33261, #9722, #82617, .T. ) ;
#83385 = LINE ( 'NONE', #76739, #58046 ) ;
#83386 = CARTESIAN_POINT ( 'NONE',  ( 157.3305006125302441, 282.1378183958786963, 1.589776369934247979 ) ) ;
#83387 = ORIENTED_EDGE ( 'NONE', *, *, #42975, .T. ) ;
#83388 = CARTESIAN_POINT ( 'NONE',  ( 194.5115483076113208, 293.7431110027661703, -15.44127576492984666 ) ) ;
#83389 = CARTESIAN_POINT ( 'NONE',  ( 193.9664686127508730, 294.0370461807386278, -14.11319465475718182 ) ) ;
#83390 = CARTESIAN_POINT ( 'NONE',  ( -6.130263895410292818, 177.2677522451419350, -5.000000000000047962 ) ) ;
#83391 = CARTESIAN_POINT ( 'NONE',  ( 82.47021907082941539, 53.30441442868470858, -15.33472904691311456 ) ) ;
#83392 = CARTESIAN_POINT ( 'NONE',  ( 171.6998185013865736, 280.1550421627382548, -15.19015613463140646 ) ) ;
#83393 = CARTESIAN_POINT ( 'NONE',  ( 164.0970344217799948, 246.4225943405349710, -8.491506243827155131 ) ) ;
#83394 = CARTESIAN_POINT ( 'NONE',  ( 72.06470348997973474, 72.25603645428110156, 1.367373202405273602 ) ) ;
#83395 = CARTESIAN_POINT ( 'NONE',  ( 161.2114343358352926, 273.1184554557211754, 15.88516176658350254 ) ) ;
#83397 = CARTESIAN_POINT ( 'NONE',  ( 76.20055470335280745, 65.09253202017347917, 14.18943646504599343 ) ) ;
#83396 = CARTESIAN_POINT ( 'NONE',  ( 2.070087696330116689, 165.8768266524159856, -9.188101187500091527 ) ) ;
#83398 = CIRCLE ( 'NONE', #34762, 70.00000000000001421 ) ;
#83399 = CARTESIAN_POINT ( 'NONE',  ( 189.0928626679413185, 297.0040558712296956, 8.255658072684374460 ) ) ;
#83400 = ORIENTED_EDGE ( 'NONE', *, *, #90708, .F. ) ;
#83401 = ORIENTED_EDGE ( 'NONE', *, *, #69637, .T. ) ;
#83402 = DIRECTION ( 'NONE',  ( 0.000000000000000000, 0.000000000000000000, 1.000000000000000000 ) ) ;
#83403 = DIRECTION ( 'NONE',  ( -0.5000000000000014433, 0.8660254037844378194, -0.000000000000000000 ) ) ;
#83404 = CARTESIAN_POINT ( 'NONE',  ( 175.1581344279587711, 291.8196898309956850, 3.447612312626186615 ) ) ;
#83405 = DIRECTION ( 'NONE',  ( 0.4999999999999992784, -0.8660254037844390407, 0.000000000000000000 ) ) ;
#83406 = CARTESIAN_POINT ( 'NONE',  ( 162.4759493558299539, 249.2303960381514969, -10.61385178995842615 ) ) ;
#83407 = CARTESIAN_POINT ( 'NONE',  ( 69.01996124760182738, 67.49486141842439224, 9.543146168910283222 ) ) ;
#83408 = CARTESIAN_POINT ( 'NONE',  ( 150.1431628338321786, 276.5498008164989869, 3.614034262083622551 ) ) ;
#83409 = EDGE_CURVE ( 'NONE', #4740, #50075, #70947, .T. ) ;
#83410 = CARTESIAN_POINT ( 'NONE',  ( 22.82720022358212120, 193.1744531367911293, 4.594050593750047540 ) ) ;
#83411 = CARTESIAN_POINT ( 'NONE',  ( 123.3136442261515526, 235.8768266524159856, 9.188101187500098632 ) ) ;
#83412 = CARTESIAN_POINT ( 'NONE',  ( -17.42236680055705023, 149.2012482093457777, 0.000000000000000000 ) ) ;
#83413 = CARTESIAN_POINT ( 'NONE',  ( 65.82138188502713660, 68.94138306836742913, 2.321386409612693047 ) ) ;
#83414 = B_SPLINE_CURVE_WITH_KNOTS ( 'NONE', 3,
 ( #95423, #42147, #73079, #64463 ),
 .UNSPECIFIED., .F., .F.,
 ( 4, 4 ),
 ( 0.01188302911889913341, 0.01804894381992137864 ),
 .UNSPECIFIED. ) ;
#83415 = CARTESIAN_POINT ( 'NONE',  ( 206.4458344621057506, 272.2190885279491681, -7.771912452422065520 ) ) ;
#83416 = EDGE_CURVE ( 'NONE', #88529, #19194, #2038, .T. ) ;
#83417 = CARTESIAN_POINT ( 'NONE',  ( 176.3489251979494554, 282.1873958766605028, -14.22545077220611276 ) ) ;
#83418 = CARTESIAN_POINT ( 'NONE',  ( 81.37890540328889699, 53.11183844281263333, -15.40672322402467387 ) ) ;
#83419 = CARTESIAN_POINT ( 'NONE',  ( 168.8785100482814698, 272.6966330010931756, 17.41127854651366391 ) ) ;
#83420 = CARTESIAN_POINT ( 'NONE',  ( 184.3506428846281722, 274.4990011916261778, 17.60835909835985547 ) ) ;
#83421 = DIRECTION ( 'NONE',  ( -0.000000000000000000, -0.000000000000000000, -1.000000000000000000 ) ) ;
#83422 = DIRECTION ( 'NONE',  ( -0.9834470158338919354, -0.1811959355157079787, 0.000000000000000000 ) ) ;
#83423 = ADVANCED_FACE ( 'NONE', ( #11732 ), #74030, .F. ) ;
#83424 = CARTESIAN_POINT ( 'NONE',  ( 84.76921427251618013, 50.44646837537948159, 13.50760817970367533 ) ) ;
#83425 = CARTESIAN_POINT ( 'NONE',  ( 186.7645341827467291, 298.9987601547266536, -0.6044513963858351158 ) ) ;
#83426 = LINE ( 'NONE', #74325, #51323 ) ;
#83427 = CARTESIAN_POINT ( 'NONE',  ( 162.2966749516206733, 251.8041562247694287, -12.92595150436406293 ) ) ;
#83428 = AXIS2_PLACEMENT_3D ( 'NONE', #46590, #61793, #9631 ) ;
#83429 = CARTESIAN_POINT ( 'NONE',  ( 48.38981961164312651, 109.5014996615669105, 177.5919119679930134 ) ) ;
#83430 = CARTESIAN_POINT ( 'NONE',  ( 81.87577037490221699, 41.13764054769151102, -5.524405591390634029 ) ) ;
#83431 = CARTESIAN_POINT ( 'NONE',  ( 98.68587325814904432, 227.7833772461660544, -9.188101187500095079 ) ) ;
#83432 = CARTESIAN_POINT ( 'NONE',  ( 6.414422030351863313, 19.10171378149916421, 9.188101187500008038 ) ) ;
#83433 = CARTESIAN_POINT ( 'NONE',  ( 164.6115012019945425, 276.7995639496792819, -15.09699049157054418 ) ) ;
#83434 = CARTESIAN_POINT ( 'NONE',  ( -22.42236680055709641, 157.8615022471902591, 0.000000000000000000 ) ) ;
#83436 = CARTESIAN_POINT ( 'NONE',  ( 199.7779437056017571, 284.6214466006996417, 18.28733359541573478 ) ) ;
#83435 = FACE_OUTER_BOUND ( 'NONE', #88718, .T. ) ;
#83437 = CARTESIAN_POINT ( 'NONE',  ( 194.5725374088679871, 291.6374747806817140, -16.23208319182986870 ) ) ;
#83438 = CARTESIAN_POINT ( 'NONE',  ( 150.6386650955079176, 269.7331738006648720, -15.06054658539322766 ) ) ;
#83439 = CARTESIAN_POINT ( 'NONE',  ( 168.2820353728258738, 287.7095463320123940, -5.019694092131335772 ) ) ;
#83440 = CARTESIAN_POINT ( 'NONE',  ( 37.97865540203802937, 30.43085787977766188, -9.188101187500008038 ) ) ;
#83441 = CARTESIAN_POINT ( 'NONE',  ( 192.8011239859581849, 296.7056528303708660, -11.79847971295421694 ) ) ;
#83442 = DIRECTION ( 'NONE',  ( -0.8660254037844379305, -0.5000000000000014433, -0.000000000000000000 ) ) ;
#83443 = ORIENTED_EDGE ( 'NONE', *, *, #50687, .F. ) ;
#83444 = CARTESIAN_POINT ( 'NONE',  ( 24.72364882272980324, 19.98920272979926693, 7.433330006724137462 ) ) ;
#83445 = CARTESIAN_POINT ( 'NONE',  ( 14.97590445773717782, 13.81029122506293305, 8.090169943749479842 ) ) ;
#83446 = CARTESIAN_POINT ( 'NONE',  ( 192.4172326059820648, 297.3705722050773943, -12.52563289807247848 ) ) ;
#83447 = CARTESIAN_POINT ( 'NONE',  ( 149.3141802193904368, 272.0272488999566463, -11.40332369054239336 ) ) ;
#83448 = VERTEX_POINT ( 'NONE', #12738 ) ;
#83449 = B_SPLINE_CURVE_WITH_KNOTS ( 'NONE', 3,
 ( #73104, #43659, #80225, #74089 ),
 .UNSPECIFIED., .F., .F.,
 ( 4, 4 ),
 ( 0.01057430845927626734, 0.01607705855292669225 ),
 .UNSPECIFIED. ) ;
#83450 = CARTESIAN_POINT ( 'NONE',  ( 70.33238309585017589, 61.19012738999462897, 14.82922649093364598 ) ) ;
#83451 = CARTESIAN_POINT ( 'NONE',  ( 75.92541454099094267, 65.74968322642241958, -14.18997729123868901 ) ) ;
#83453 = EDGE_CURVE ( 'NONE', #88645, #46305, #5608, .T. ) ;
#83452 = CARTESIAN_POINT ( 'NONE',  ( 157.5046580301597032, 268.7583167102267794, 15.65051971689831589 ) ) ;
#83454 = CARTESIAN_POINT ( 'NONE',  ( 173.1833192663806926, 253.4864516599578792, -9.233729552024655618 ) ) ;
#83455 = CARTESIAN_POINT ( 'NONE',  ( 138.6583583033484786, 260.8615022471902876, 5.000000000000046185 ) ) ;
#83456 = ORIENTED_EDGE ( 'NONE', *, *, #28685, .T. ) ;
#83457 = LINE ( 'NONE', #82487, #37484 ) ;
#83458 = ORIENTED_EDGE ( 'NONE', *, *, #53579, .F. ) ;
#83459 = CARTESIAN_POINT ( 'NONE',  ( 163.1691520398773321, 248.0297337694385931, 11.21816141384514331 ) ) ;
#83460 = CARTESIAN_POINT ( 'NONE',  ( 83.82679190265474745, 41.76113697558885463, 1.428417452354569850 ) ) ;
#83461 = EDGE_CURVE ( 'NONE', #81157, #93052, #74540, .T. ) ;
#83462 = ORIENTED_EDGE ( 'NONE', *, *, #1452, .T. ) ;
#83463 = CARTESIAN_POINT ( 'NONE',  ( 184.7176300103652125, 293.6802179342421937, -10.75420723427517977 ) ) ;
#83464 = ORIENTED_EDGE ( 'NONE', *, *, #81668, .F. ) ;
#83465 = DIRECTION ( 'NONE',  ( -0.8660254037844387076, -0.4999999999999998890, -0.000000000000000000 ) ) ;
#83466 = LINE ( 'NONE', #46917, #81558 ) ;
#83467 = CARTESIAN_POINT ( 'NONE',  ( 190.8725948953614591, 278.0229128820462279, -17.51817159285709025 ) ) ;
#83468 = DIRECTION ( 'NONE',  ( 0.4999999999999998890, -0.8660254037844385966, 0.000000000000000000 ) ) ;
#83469 = B_SPLINE_CURVE_WITH_KNOTS ( 'NONE', 3,
 ( #83924, #91512, #60062, #75304 ),
 .UNSPECIFIED., .F., .F.,
 ( 4, 4 ),
 ( 0.01804370536616622250, 0.02702473640048589851 ),
 .UNSPECIFIED. ) ;
#83470 = CARTESIAN_POINT ( 'NONE',  ( 152.6692142062575499, 266.2161595735824449, -16.77985299603479419 ) ) ;
#83471 = VECTOR ( 'NONE', #64041, 1000.000000000000000 ) ;
#83472 = CARTESIAN_POINT ( 'NONE',  ( 35.38177548881301249, 32.37878583063844218, 9.188101187500006262 ) ) ;
#83473 = CARTESIAN_POINT ( 'NONE',  ( -13.11024591527734628, 6.000000000000000000, 25.00000000000000000 ) ) ;
#83474 = CARTESIAN_POINT ( 'NONE',  ( 178.1281481821618797, 292.9991590599575488, -6.064681374715556572 ) ) ;
#83476 = VECTOR ( 'NONE', #28390, 999.9999999999998863 ) ;
#83475 = CARTESIAN_POINT ( 'NONE',  ( 87.63119364650854948, 45.29408460765224476, 6.394950601605615681 ) ) ;
#83477 = ORIENTED_EDGE ( 'NONE', *, *, #94948, .T. ) ;
#83478 = ORIENTED_EDGE ( 'NONE', *, *, #3177, .F. ) ;
#83479 = CARTESIAN_POINT ( 'NONE',  ( -0.4668637173180778532, 25.74574839753307387, 10.00000000000000000 ) ) ;
#83480 = PLANE ( 'NONE',  #91320 ) ;
#83481 = CARTESIAN_POINT ( 'NONE',  ( 79.79337866746672603, 57.38101010784296108, 16.24820852827756923 ) ) ;
#83483 = CARTESIAN_POINT ( 'NONE',  ( 165.9617581993362023, 274.1071786095166090, -15.17248422297432420 ) ) ;
#83482 = LINE ( 'NONE', #76831, #26092 ) ;
#83484 = CARTESIAN_POINT ( 'NONE',  ( 206.1569797555946195, 273.5726320587986038, -9.753408447412784454 ) ) ;
#83485 = CARTESIAN_POINT ( 'NONE',  ( 198.3132153568068929, 273.7169797895816714, -13.42874499935994237 ) ) ;
#83486 = CARTESIAN_POINT ( 'NONE',  ( 75.86996176085413879, 60.47672722295040870, -15.68272062288790814 ) ) ;
#83487 = CARTESIAN_POINT ( 'NONE',  ( 147.6618183892331331, 274.8892235422768522, 8.990680574201936892 ) ) ;
#83488 = CARTESIAN_POINT ( 'NONE',  ( 170.5177250007984640, 288.6921495108791760, -4.130607863702036475 ) ) ;
#83489 = CARTESIAN_POINT ( 'NONE',  ( 76.98305832116996328, 63.37377475765585899, -15.46912589935254623 ) ) ;
#83490 = CARTESIAN_POINT ( 'NONE',  ( 186.6577945393187008, 286.8565254842017112, -15.55016485953022176 ) ) ;
#83491 = CARTESIAN_POINT ( 'NONE',  ( 121.2028808523094767, 228.5327760586659451, 1.948934522072303157E-15 ) ) ;
#83492 = EDGE_LOOP ( 'NONE', ( #24951, #46509, #84722, #91110 ) ) ;
#83493 = CARTESIAN_POINT ( 'NONE',  ( 183.5821904726393825, 260.0513847542609938, -9.557056484130177054 ) ) ;
#83494 = CARTESIAN_POINT ( 'NONE',  ( 27.74993340135631215, 36.99752408145592852, 5.678558825948277544 ) ) ;
#83495 = CARTESIAN_POINT ( 'NONE',  ( 191.9642392354410561, 293.3079686636485803, -14.67799312013193003 ) ) ;
#83496 = ORIENTED_EDGE ( 'NONE', *, *, #93701, .T. ) ;
#83497 = AXIS2_PLACEMENT_3D ( 'NONE', #50960, #66174, #88042 ) ;
#83498 = VECTOR ( 'NONE', #67809, 1000.000000000000000 ) ;
#83499 = CARTESIAN_POINT ( 'NONE',  ( 74.21864607481936105, 68.58553829006309854, -11.54532566021463502 ) ) ;
#83500 = CARTESIAN_POINT ( 'NONE',  ( 164.9359911487327963, 246.1719262986664489, -2.773572180244460839 ) ) ;
#83501 = CARTESIAN_POINT ( 'NONE',  ( 195.8449251089225811, 291.4336346372613775, 16.14492769602857081 ) ) ;
#83502 = CARTESIAN_POINT ( 'NONE',  ( 67.33987171904671243, 68.55273472465368911, 6.369544805306559532 ) ) ;
#83503 = ADVANCED_FACE ( 'NONE', ( #97832 ), #75030, .T. ) ;
#83504 = CARTESIAN_POINT ( 'NONE',  ( 22.33482336197099016, 13.86426979415089455, -3.090169943749474069 ) ) ;
#83505 = ORIENTED_EDGE ( 'NONE', *, *, #58915, .T. ) ;
#83506 = AXIS2_PLACEMENT_3D ( 'NONE', #31034, #76173, #38629 ) ;
#83507 = CARTESIAN_POINT ( 'NONE',  ( 148.7194274992590408, 273.0573908291643761, 9.629271269182392956 ) ) ;
#83508 = EDGE_CURVE ( 'NONE', #44920, #50293, #24996, .T. ) ;
#83509 = ORIENTED_EDGE ( 'NONE', *, *, #51571, .F. ) ;
#83510 = DIRECTION ( 'NONE',  ( -0.8660254037844377084, -0.5000000000000014433, -0.000000000000000000 ) ) ;
#83511 = ORIENTED_EDGE ( 'NONE', *, *, #25003, .F. ) ;
#83513 = CARTESIAN_POINT ( 'NONE',  ( 206.5318754762992910, 272.9232936229979032, 10.63244694018452741 ) ) ;
#83512 = PRODUCT_DEFINITION_FORMATION_WITH_SPECIFIED_SOURCE ( 'ANY', '', #13637, .NOT_KNOWN. ) ;
#83514 = CARTESIAN_POINT ( 'NONE',  ( 195.9012476844455364, 265.0396910272671676, 3.914111099667014759 ) ) ;
#83515 = CARTESIAN_POINT ( 'NONE',  ( 158.4641270891539193, 263.4220271406156826, 17.63380002636472810 ) ) ;
#83516 = CARTESIAN_POINT ( 'NONE',  ( 67.08658855976769075, 68.82903281458501965, -3.711205762594173230 ) ) ;
#83518 = CARTESIAN_POINT ( 'NONE',  ( 69.95954962829708279, 62.80909189523259073, -13.34258826528541952 ) ) ;
#83517 = CYLINDRICAL_SURFACE ( 'NONE', #77588, 10.00000000000010658 ) ;
#83519 = CARTESIAN_POINT ( 'NONE',  ( 201.2949053258274148, 281.9939920013367782, -18.04004790210578335 ) ) ;
#83520 = ORIENTED_EDGE ( 'NONE', *, *, #96045, .T. ) ;
#83521 = CARTESIAN_POINT ( 'NONE',  ( 146.8358616138309571, 276.3198226421291679, 4.054088818585255716 ) ) ;
#83522 = CARTESIAN_POINT ( 'NONE',  ( 52.15148940044955594, 212.4637435831425307, 2.679491924311251605 ) ) ;
#83523 = CARTESIAN_POINT ( 'NONE',  ( 82.02651322757263586, 41.09817291294280750, -3.386295274050155069 ) ) ;
#83524 = CARTESIAN_POINT ( 'NONE',  ( 192.8922468175501876, 270.9615889258991501, 14.61616359823144506 ) ) ;
#83525 = CARTESIAN_POINT ( 'NONE',  ( 189.2695117162384122, 270.1846877967625460, -14.08055865318978839 ) ) ;
#83526 = CARTESIAN_POINT ( 'NONE',  ( 154.6982851380984130, 273.6571292083216349, -13.42362762759460892 ) ) ;
#83527 = CARTESIAN_POINT ( 'NONE',  ( 82.54609081338128362, 42.37776545139765716, 6.143319459098965041 ) ) ;
#83528 = CARTESIAN_POINT ( 'NONE',  ( 59.27500801855438795, 193.4824982072973683, 3.021315404115420679E-15 ) ) ;
#83529 = CARTESIAN_POINT ( 'NONE',  ( 155.4917600441137324, 261.3273667757233056, 17.14261720787171939 ) ) ;
#83530 = CARTESIAN_POINT ( 'NONE',  ( 191.4336085427262333, 282.7786862010840423, -17.53248462874352498 ) ) ;
#83531 = EDGE_CURVE ( 'NONE', #19194, #92966, #93948, .T. ) ;
#83532 = CARTESIAN_POINT ( 'NONE',  ( 71.45285423991207097, 70.68761458493762007, -5.807058293593552634 ) ) ;
#83533 = CARTESIAN_POINT ( 'NONE',  ( 73.95019621043853419, 207.3768266524160140, 9.188101187500098632 ) ) ;
#83534 = CARTESIAN_POINT ( 'NONE',  ( 206.7680519836501958, 272.5142239127119979, -10.57935479673322021 ) ) ;
#83535 = CARTESIAN_POINT ( 'NONE',  ( -19.83262083840140022, 133.3759306620404459, 30.52142883766498827 ) ) ;
#83536 = LINE ( 'NONE', #22195, #36510 ) ;
#83537 = CARTESIAN_POINT ( 'NONE',  ( 60.86586985908987657, 190.3595308348468791, 0.000000000000000000 ) ) ;
#83538 = B_SPLINE_CURVE_WITH_KNOTS ( 'NONE', 3,
 ( #96659, #27229, #97160, #49029, #3921, #25739, #34320, #71844, #65218, #20129, #56618, #50504, #2442, #73334, #66222, #11540, #19643, #64732, #19147, #50021, #88087, #34803, #58594, #18128 ),
 .UNSPECIFIED., .F., .F.,
 ( 4, 2, 2, 2, 2, 2, 2, 2, 2, 2, 2, 4 ),
 ( 0.005192606658219600137, 0.005519221611633958260, 0.005845836565048317252, 0.006172451518462674508, 0.006499066471877033499, 0.007152296378705787910, 0.007805526285534543189, 0.008458756192363282855, 0.009111986099192019919, 0.009765216006020758718, 0.01009183095943514720, 0.01041844591284953395 ),
 .UNSPECIFIED. ) ;
#83539 = VECTOR ( 'NONE', #36133, 1000.000000000000000 ) ;
#83540 = CARTESIAN_POINT ( 'NONE',  ( 207.1572261440131797, 271.8401544939704877, -5.633070628900782140 ) ) ;
#83541 = CARTESIAN_POINT ( 'NONE',  ( 66.91132889924701033, 69.20890817986715149, 0.7224412942219599065 ) ) ;
#83543 = CARTESIAN_POINT ( 'NONE',  ( -20.78307953964266019, 95.12990406498558116, 45.19945594742419104 ) ) ;
#83542 = CARTESIAN_POINT ( 'NONE',  ( 73.54295707248225256, 69.21941320345065662, -10.00962305751349035 ) ) ;
#83544 =( NAMED_UNIT ( * ) SI_UNIT ( $, .STERADIAN. ) SOLID_ANGLE_UNIT ( ) );
#83545 = LINE ( 'NONE', #14108, #73431 ) ;
#83546 = CARTESIAN_POINT ( 'NONE',  ( 149.7503540259411068, 272.3885311082809153, -11.42439314646132509 ) ) ;
#83547 = DIRECTION ( 'NONE',  ( -0.9140770918436990078, -0.4055404667435369426, 0.000000000000000000 ) ) ;
#83548 = VECTOR ( 'NONE', #57529, 1000.000000000000114 ) ;
#83549 = CARTESIAN_POINT ( 'NONE',  ( 71.96027346690365789, 72.28811235517684963, 3.313491923126963279 ) ) ;
#83550 = CARTESIAN_POINT ( 'NONE',  ( 26.10194555558328133, 192.0024278399160949, -9.188101187500093303 ) ) ;
#83551 = CARTESIAN_POINT ( 'NONE',  ( 196.3519702320103590, 290.5554067223432639, 17.39042812051341969 ) ) ;
#83552 = LINE ( 'NONE', #67305, #99389 ) ;
#83553 = CARTESIAN_POINT ( 'NONE',  ( 80.32319512552398066, 50.51006391666574302, -14.68283735665326084 ) ) ;
#83554 = CARTESIAN_POINT ( 'NONE',  ( 71.84099513407564075, 72.54812194311107021, -1.276242074083207001 ) ) ;
#83555 = CARTESIAN_POINT ( 'NONE',  ( 55.14129374593650113, 193.4548013555410080, -4.594050593750042211 ) ) ;
#83556 = ADVANCED_FACE ( 'NONE', ( #13710 ), #20831, .T. ) ;
#83557 = CARTESIAN_POINT ( 'NONE',  ( 18.31869600479030424, 33.68290643055186706, 3.479690158560446702E-15 ) ) ;
#83558 = CARTESIAN_POINT ( 'NONE',  ( 199.1867231605587278, 285.6454706231928071, -17.41989184023605475 ) ) ;
#83559 = CARTESIAN_POINT ( 'NONE',  ( 196.7823306783968746, 289.8100005636337073, -17.85370042640856170 ) ) ;
#83560 = CARTESIAN_POINT ( 'NONE',  ( 36.03373902044236132, 43.73705186507757503, -3.090169943749475845 ) ) ;
#83561 = DIRECTION ( 'NONE',  ( -0.7646402761590023189, -0.6444573283588950208, 0.000000000000000000 ) ) ;
#83562 = CARTESIAN_POINT ( 'NONE',  ( 159.4072785079408732, 255.6537108709859183, -16.22214289272363175 ) ) ;
#83563 = CARTESIAN_POINT ( 'NONE',  ( 175.5651479323515787, 291.1351013291215395, 2.181378784527221448 ) ) ;
#83564 = AXIS2_PLACEMENT_3D ( 'NONE', #95848, #85761, #1101 ) ;
#83565 = VERTEX_POINT ( 'NONE', #36500 ) ;
#83566 = CARTESIAN_POINT ( 'NONE',  ( 72.36041625537609434, 60.48984345533310858, 15.04059213219202640 ) ) ;
#83567 = CARTESIAN_POINT ( 'NONE',  ( 153.0305350670531936, 277.3750776671890890, 8.290292975357761662 ) ) ;
#83568 = CARTESIAN_POINT ( 'NONE',  ( 163.3837300346235395, 255.8040548010872612, -14.83920063947459056 ) ) ;
#83569 = VECTOR ( 'NONE', #11143, 1000.000000000000114 ) ;
#83570 = PLANE ( 'NONE',  #9605 ) ;
#83571 = CARTESIAN_POINT ( 'NONE',  ( 97.88299554183124940, 213.9865022471901455, 1.119607411625061291E-15 ) ) ;
#83572 = CARTESIAN_POINT ( 'NONE',  ( 161.1990332043106946, 251.4420796895884394, 14.26998817770995487 ) ) ;
#83573 = CARTESIAN_POINT ( 'NONE',  ( 164.8753104327445271, 270.4778681372466735, -17.27537531252914249 ) ) ;
#83574 = EDGE_LOOP ( 'NONE', ( #51385, #6949, #27371, #38001 ) ) ;
#83575 = CARTESIAN_POINT ( 'NONE',  ( 64.58612298413676456, 208.0958772461660544, -9.188101187500095079 ) ) ;
#83576 = VERTEX_POINT ( 'NONE', #67403 ) ;
#83577 = CARTESIAN_POINT ( 'NONE',  ( 178.5460542442402527, 263.4982612806743987, 15.38449660858491441 ) ) ;
#83578 = CARTESIAN_POINT ( 'NONE',  ( 161.5959287003499583, 251.1472748658742944, 12.79373419553940749 ) ) ;
#83579 = DIRECTION ( 'NONE',  ( 0.4999999999999998890, -0.8660254037844385966, 0.000000000000000000 ) ) ;
#83580 = ORIENTED_EDGE ( 'NONE', *, *, #66203, .T. ) ;
#83581 = DIRECTION ( 'NONE',  ( -1.000000000000000000, -0.000000000000000000, -0.000000000000000000 ) ) ;
#83582 = CARTESIAN_POINT ( 'NONE',  ( 79.38657480761875718, 46.22199533766026747, -13.24841598642484364 ) ) ;
#83583 = CARTESIAN_POINT ( 'NONE',  ( 69.61542750552385428, 62.56132062511080250, -13.94275833699888345 ) ) ;
#83584 = CARTESIAN_POINT ( 'NONE',  ( 19.31801425620940194, 115.5650415295850451, 60.00000000000000000 ) ) ;
#83585 = CARTESIAN_POINT ( 'NONE',  ( 204.7462429809936282, 276.0160998285135179, 13.10238900943261342 ) ) ;
#83586 = ORIENTED_EDGE ( 'NONE', *, *, #4642, .F. ) ;
#83587 = CARTESIAN_POINT ( 'NONE',  ( 18.74326920199815305, 31.79752408145591858, -5.678558825948271327 ) ) ;
#83588 = CARTESIAN_POINT ( 'NONE',  ( 75.26690622274593068, 56.07482427453010843, 16.14689877337623969 ) ) ;
#83589 = CARTESIAN_POINT ( 'NONE',  ( 72.67905965592419193, 70.26320000030698054, -8.002569769838684621 ) ) ;
#83590 = CARTESIAN_POINT ( 'NONE',  ( 201.1893450866852504, 280.1768276987904756, -16.82388990131531870 ) ) ;
#83591 = ORIENTED_EDGE ( 'NONE', *, *, #72157, .T. ) ;
#83592 = CARTESIAN_POINT ( 'NONE',  ( 180.8586690819065552, 283.2892246925316044, 14.99098275897606314 ) ) ;
#83593 = CARTESIAN_POINT ( 'NONE',  ( 159.5050723400634638, 254.3761059724978679, -15.34938048045353298 ) ) ;
#83594 = ORIENTED_EDGE ( 'NONE', *, *, #62756, .T. ) ;
#83595 = ORIENTED_EDGE ( 'NONE', *, *, #45378, .T. ) ;
#83597 = CARTESIAN_POINT ( 'NONE',  ( -19.65312891409030271, 93.06504152958497400, 177.5919119679930134 ) ) ;
#83596 = DIRECTION ( 'NONE',  ( 0.000000000000000000, 0.000000000000000000, 1.000000000000000000 ) ) ;
#83598 = CARTESIAN_POINT ( 'NONE',  ( 207.5959034698703078, 271.0803430774575418, -1.830000129038042544 ) ) ;
#83599 = CARTESIAN_POINT ( 'NONE',  ( 163.8990931530087494, 246.7654386749614162, 5.873176884778091633 ) ) ;
#83600 = CARTESIAN_POINT ( 'NONE',  ( 198.6562788533279615, 286.5642271139020636, 17.47134757795404525 ) ) ;
#83601 = CARTESIAN_POINT ( 'NONE',  ( 81.40581815559377787, 55.82057330830384956, 16.38440887150438385 ) ) ;
#83602 = CARTESIAN_POINT ( 'NONE',  ( 177.8194257969418288, 292.8449071177858514, 6.006967295066290013 ) ) ;
#83603 = B_SPLINE_CURVE_WITH_KNOTS ( 'NONE', 3,
 ( #98197, #51579, #59146, #66777, #22175, #27788, #74411, #59659, #60152, #21194, #75393, #68266, #43960, #21681, #51065, #4481, #5976, #52560, #29774, #36872, #82536, #35375, #75903, #67778, #98703, #29287, #42952, #60647, #6483, #4996, #91603, #66286, #97219, #58661, #89633, #20195, #12600, #97702, #43467, #28270, #69264, #92128, #22681, #61659, #7462, #24663 ),
 .UNSPECIFIED., .F., .F.,
 ( 4, 1, 2, 2, 1, 2, 2, 1, 1, 2, 2, 1, 1, 2, 2, 1, 1, 2, 2, 1, 1, 1, 2, 2, 1, 1, 1, 2, 2, 4 ),
 ( 0.000000000000000000, 0.06250000000000537070, 0.09375000000000875688, 0.1250000000000121292, 0.1875000000000191791, 0.2187500000000226763, 0.2500000000000262013, 0.3125000000000315303, 0.3437500000000344724, 0.3593750000000353051, 0.3750000000000361933, 0.4375000000000394684, 0.4687500000000424105, 0.4843750000000436318, 0.5000000000000448530, 0.5625000000000469624, 0.5937500000000474065, 0.6093750000000467404, 0.6250000000000460743, 0.6875000000000431877, 0.7187500000000411893, 0.7343750000000400791, 0.7421875000000380806, 0.7500000000000360822, 0.8125000000000286438, 0.8437500000000239808, 0.8593750000000223155, 0.8671875000000223155, 0.8750000000000223155, 1.000000000000000000 ),
 .UNSPECIFIED. ) ;
#83604 = CARTESIAN_POINT ( 'NONE',  ( 127.2647115830355347, 244.2833772461660544, -9.188101187500095079 ) ) ;
#83605 = DIRECTION ( 'NONE',  ( -0.8660254037844359321, -0.5000000000000051070, -0.000000000000000000 ) ) ;
#83606 = CARTESIAN_POINT ( 'NONE',  ( 73.95019621043853419, 207.3768266524160140, 9.188101187500098632 ) ) ;
#83607 = VERTEX_POINT ( 'NONE', #50214 ) ;
#83608 = CARTESIAN_POINT ( 'NONE',  ( 170.2399125551612258, 264.0282869839934961, 16.04968556189760776 ) ) ;
#83609 = CARTESIAN_POINT ( 'NONE',  ( 79.67912095024387042, 45.93721481267125029, 12.94223426716299663 ) ) ;
#83610 = VECTOR ( 'NONE', #31740, 1000.000000000000227 ) ;
#83611 = ORIENTED_EDGE ( 'NONE', *, *, #23362, .F. ) ;
#83612 = LINE ( 'NONE', #14180, #44602 ) ;
#83613 = AXIS2_PLACEMENT_3D ( 'NONE', #67767, #84498, #53546 ) ;
#83614 = ORIENTED_EDGE ( 'NONE', *, *, #9846, .T. ) ;
#83615 = VERTEX_POINT ( 'NONE', #82163 ) ;
#83616 = CARTESIAN_POINT ( 'NONE',  ( 76.26477717271305323, 65.12336802401900115, 14.59904178568168120 ) ) ;
#83617 = CARTESIAN_POINT ( 'NONE',  ( 66.97405472610564914, 68.05443638886698920, 6.913098729884842975 ) ) ;
#83618 = CARTESIAN_POINT ( 'NONE',  ( 197.4340835798049625, 286.5481627907838060, 16.91565206045372705 ) ) ;
#83620 = B_SPLINE_SURFACE_WITH_KNOTS ( 'NONE', 3, 1, ( 
 ( #31015, #91871 ),
 ( #45219, #45706 ),
 ( #61413, #38613 ),
 ( #22426, #76158 ),
 ( #15301, #91361 ),
 ( #30021, #62402 ),
 ( #93358, #14819 ),
 ( #37121, #7216 ),
 ( #84273, #626 ),
 ( #68028, #61905 ),
 ( #68523, #30525 ),
 ( #54814, #92855 ),
 ( #29533, #99444 ),
 ( #31507, #85791 ),
 ( #46200, #69011 ),
 ( #22913, #7722 ),
 ( #76631, #16323 ),
 ( #69518, #53800 ),
 ( #60906, #38100 ),
 ( #77117, #6226 ),
 ( #46717, #132 ),
 ( #99942, #54299 ),
 ( #77645, #23409 ),
 ( #85267, #98950 ),
 ( #15813, #8230 ),
 ( #39098, #70011 ),
 ( #60405, #21925 ),
 ( #17319, #87800 ),
 ( #79673, #56311 ),
 ( #47216, #88285 ),
 ( #78138, #1132 ) ),
 .UNSPECIFIED., .F., .F., .F.,
 ( 4, 3, 3, 3, 3, 3, 3, 3, 3, 3, 4 ),
 ( 2, 2 ),
 ( 0.000000000000000000, 0.1333490885032316831, 0.3007194338854232707, 0.4699862290244899432, 0.5844252810809152932, 0.6686540514502595789, 0.7354980260655316071, 0.8028463152565562533, 0.8633854507756971719, 0.9437142632666813968, 1.000000000000000000 ),
 ( 0.000000000000000000, 1.000000000000000000 ),
 .UNSPECIFIED. ) ;
#83619 = CARTESIAN_POINT ( 'NONE',  ( 147.1731211915891322, 275.7356719181125868, 0.5879280619134324981 ) ) ;
#83621 = CARTESIAN_POINT ( 'NONE',  ( 81.22638650634890212, 56.17890105291410663, 16.10240317970520962 ) ) ;
#83622 = CARTESIAN_POINT ( 'NONE',  ( 194.5051734451974426, 293.7541525883582381, 14.61790433731063921 ) ) ;
#83623 = EDGE_CURVE ( 'NONE', #22484, #99081, #4111, .T. ) ;
#83624 = CIRCLE ( 'NONE', #73905, 1.449999999999993072 ) ;
#83625 = CARTESIAN_POINT ( 'NONE',  ( 70.86180917824351866, 65.18287531716292449, 12.13021261807535822 ) ) ;
#83626 = CARTESIAN_POINT ( 'NONE',  ( 87.36072329576109041, 44.92403384853251680, 6.858028155142561033 ) ) ;
#83627 = EDGE_LOOP ( 'NONE', ( #85781, #16425, #33246, #43834 ) ) ;
#83628 = EDGE_CURVE ( 'NONE', #66038, #62710, #97143, .T. ) ;
#83629 = CARTESIAN_POINT ( 'NONE',  ( 24.24684063885245422, 16.12755873383626337, -6.180339887498949025 ) ) ;
#83631 = ADVANCED_FACE ( 'NONE', ( #26925 ), #88783, .T. ) ;
#83630 = CARTESIAN_POINT ( 'NONE',  ( 162.0336139374437323, 249.9965434567837974, -13.69905126395175365 ) ) ;
#83632 = ORIENTED_EDGE ( 'NONE', *, *, #74008, .T. ) ;
#83633 = CARTESIAN_POINT ( 'NONE',  ( 76.04471674989768815, 51.35811929192740166, -16.14395075012120273 ) ) ;
#83634 = EDGE_CURVE ( 'NONE', #22359, #34967, #96863, .T. ) ;
#83635 = CARTESIAN_POINT ( 'NONE',  ( 15.11407551230992219, 32.30945333909093620, 10.00000000000000000 ) ) ;
#83636 = CARTESIAN_POINT ( 'NONE',  ( 147.4298066744680398, 275.2910796202013444, -3.046391898894023953 ) ) ;
#83638 = AXIS2_PLACEMENT_3D ( 'NONE', #55329, #93385, #92880 ) ;
#83637 = CARTESIAN_POINT ( 'NONE',  ( 173.4505375608857491, 284.9503170016366198, -13.05978560202663452 ) ) ;
#83639 = CARTESIAN_POINT ( 'NONE',  ( 196.3432621239062712, 279.8021363881798038, 16.39655255723854665 ) ) ;
#83640 = LINE ( 'NONE', #75510, #41572 ) ;
#83641 = CARTESIAN_POINT ( 'NONE',  ( 141.2025682470151366, 243.1423013555409796, -4.594050593750043987 ) ) ;
#83642 = ORIENTED_EDGE ( 'NONE', *, *, #59037, .F. ) ;
#83643 = AXIS2_PLACEMENT_3D ( 'NONE', #25929, #24904, #25406 ) ;
#83644 = CARTESIAN_POINT ( 'NONE',  ( 87.74187345177139719, 44.20045605528624577, 4.652363546664123994 ) ) ;
#83645 = CARTESIAN_POINT ( 'NONE',  ( 73.36397865156375531, 67.21426321682912430, -12.28381576122694341 ) ) ;
#83646 = CARTESIAN_POINT ( 'NONE',  ( 87.83899792242847582, 44.00541668311377208, -1.848955303085624058 ) ) ;
#83647 = VECTOR ( 'NONE', #22889, 1000.000000000000000 ) ;
#83648 = CARTESIAN_POINT ( 'NONE',  ( 72.85283338774588913, 70.95119525769652569, 7.785565881738510718 ) ) ;
#83649 = CARTESIAN_POINT ( 'NONE',  ( 71.52047308030192596, 67.22020565769358313, -10.76659510055284841 ) ) ;
#83650 = ORIENTED_EDGE ( 'NONE', *, *, #77163, .T. ) ;
#83651 = CARTESIAN_POINT ( 'NONE',  ( 199.5713953663193934, 266.2439827736556026, 4.749567076163869750 ) ) ;
#83652 =( BOUNDED_CURVE ( )  B_SPLINE_CURVE ( 2, ( #99675, #84014, #83504, #52551, #84991, #14067, #37350, #30259, #60143, #6957, #52065, #98693, #15044 ),
 .UNSPECIFIED., .F., .T. ) 
 B_SPLINE_CURVE_WITH_KNOTS ( ( 3, 2, 2, 2, 2, 2, 3 ),
 ( 0.2874999999999999778, 0.2899999999999999800, 0.2949999999999999845, 0.2999999999999999889, 0.3049999999999999933, 0.3099999999999999978, 0.3125000000000000000 ),
 .UNSPECIFIED. ) 
 CURVE ( )  GEOMETRIC_REPRESENTATION_ITEM ( )  RATIONAL_B_SPLINE_CURVE ( ( 0.9755282581475768211, 0.9755282581475768211, 1.000000000000000000, 0.9510565162951535312, 1.000000000000000000, 0.9510565162951535312, 1.000000000000000000, 0.9510565162951535312, 1.000000000000000000, 0.9510565162951535312, 1.000000000000000000, 0.9755282581475768211, 0.9755282581475768211 ) ) 
 REPRESENTATION_ITEM ( '' )  );
#83653 = CARTESIAN_POINT ( 'NONE',  ( 181.5127903015804236, 292.0923642003480154, 10.55878241066769441 ) ) ;
#83654 = CARTESIAN_POINT ( 'NONE',  ( 86.54822389131679472, 42.74345947012793090, -2.172736160200603931E-06 ) ) ;
#83655 = CARTESIAN_POINT ( 'NONE',  ( 80.64045924028067702, 49.96054635152264467, 14.37335726122271318 ) ) ;
#83656 = CARTESIAN_POINT ( 'NONE',  ( 198.7494054154245191, 266.3724082695370043, 0.8279625511378244651 ) ) ;
#83657 = CARTESIAN_POINT ( 'NONE',  ( 198.5172889092661990, 266.1891015951424606, 0.5731995804530348737 ) ) ;
#83658 = CARTESIAN_POINT ( 'NONE',  ( 190.9586609929293104, 299.8968923453624598, -4.970176667899034229 ) ) ;
#83659 = CARTESIAN_POINT ( 'NONE',  ( 186.5691198594528259, 282.5508937948688981, 16.19376103776746945 ) ) ;
#83660 = B_SPLINE_CURVE_WITH_KNOTS ( 'NONE', 3,
 ( #371, #60646, #91114, #91602, #5974, #100192 ),
 .UNSPECIFIED., .F., .F.,
 ( 4, 2, 4 ),
 ( 0.02174174018087433186, 0.02633378460584469630, 0.03092582903081506074 ),
 .UNSPECIFIED. ) ;
#83661 = CARTESIAN_POINT ( 'NONE',  ( 158.1587942607527850, 261.9516103332310308, -17.82285333032626795 ) ) ;
#83662 = CARTESIAN_POINT ( 'NONE',  ( 168.9677593865781944, 262.6396129170871632, -17.12250179939312389 ) ) ;
#83663 = CARTESIAN_POINT ( 'NONE',  ( 24.23155096423127475, 19.15404122711133894, 8.090169943749479842 ) ) ;
#83664 = LINE ( 'NONE', #52704, #96949 ) ;
#83665 = CARTESIAN_POINT ( 'NONE',  ( 205.0150392401225758, 274.4627107821886511, 11.80085037109421719 ) ) ;
#83666 = CARTESIAN_POINT ( 'NONE',  ( 18.00728827979274627, 29.13478043621388380, 8.090169943749478065 ) ) ;
#83667 = CARTESIAN_POINT ( 'NONE',  ( 198.3523905153085423, 287.0905771551796306, 18.52598547438866206 ) ) ;
#83668 = CARTESIAN_POINT ( 'NONE',  ( 72.19186707540899306, 71.87388231314805864, -3.875259471157315172 ) ) ;
#83669 = CARTESIAN_POINT ( 'NONE',  ( 141.4548986661878303, 259.1427522451419350, 10.00000000000009237 ) ) ;
#83670 = CARTESIAN_POINT ( 'NONE',  ( 182.3178896938217122, 278.5243308997074791, 17.63982057706049389 ) ) ;
#83671 = VERTEX_POINT ( 'NONE', #19830 ) ;
#83672 = CARTESIAN_POINT ( 'NONE',  ( 66.98956810429928055, 67.69424080958161483, -6.459028911160978659 ) ) ;
#83673 = CARTESIAN_POINT ( 'NONE',  ( 72.76037481019557163, 70.79492043649186428, -7.951079947203121279 ) ) ;
#83674 = CARTESIAN_POINT ( 'NONE',  ( 202.4863134139235967, 273.9910293909178449, -13.09725697524322996 ) ) ;
#83675 = CARTESIAN_POINT ( 'NONE',  ( 199.1526122334580862, 285.7045524820243259, -17.32174362185583050 ) ) ;
#83676 = CARTESIAN_POINT ( 'NONE',  ( 8.727484440040480962, 175.8458772461660828, 9.188101187500095079 ) ) ;
#83678 = ADVANCED_FACE ( 'NONE', ( #43087 ), #4618, .T. ) ;
#83677 = CIRCLE ( 'NONE', #31850, 70.00000000000001421 ) ;
#83679 = CARTESIAN_POINT ( 'NONE',  ( 25.04820903906726315, 30.16454794089042224, -10.00000000000000355 ) ) ;
#83680 = CARTESIAN_POINT ( 'NONE',  ( 85.54106661513783649, 48.65811287445264810, 12.45824154186499833 ) ) ;
#83681 = CARTESIAN_POINT ( 'NONE',  ( 170.1129511229850948, 270.7127029815443393, -17.04003866544655921 ) ) ;
#83683 = VECTOR ( 'NONE', #19187, 999.9999999999998863 ) ;
#83682 = CARTESIAN_POINT ( 'NONE',  ( 72.10970998683657740, 71.81466167570245318, -3.920937378582701083 ) ) ;
#83684 = CYLINDRICAL_SURFACE ( 'NONE', #15117, 17.82106496071139645 ) ;
#83685 = DIRECTION ( 'NONE',  ( 0.8660254037844385966, 0.5000000000000003331, 3.252519625699449945E-16 ) ) ;
#83686 = CARTESIAN_POINT ( 'NONE',  ( 198.6455782124543248, 286.5827611675690605, 17.19551065434971093 ) ) ;
#83687 = EDGE_CURVE ( 'NONE', #78482, #50533, #89759, .T. ) ;
#83688 = CARTESIAN_POINT ( 'NONE',  ( 49.38557292990258674, 205.9865022471902876, 10.00000000000009237 ) ) ;
#83689 = CARTESIAN_POINT ( 'NONE',  ( -22.42236680055709641, 157.8615022471902591, 0.000000000000000000 ) ) ;
#83690 = CARTESIAN_POINT ( 'NONE',  ( 190.6084209867335915, 300.5035258309363826, -0.5505750481748228342 ) ) ;
#83691 = CARTESIAN_POINT ( 'NONE',  ( 15.76359375002403596, 192.1589784336661637, -6.496448406907675876E-16 ) ) ;
#83692 = DIRECTION ( 'NONE',  ( -0.6201213960746242426, 0.7845058662180030007, 0.000000000000000000 ) ) ;
#83693 = EDGE_CURVE ( 'NONE', #98005, #7924, #91737, .T. ) ;
#83694 = CARTESIAN_POINT ( 'NONE',  ( 78.88646228610093658, 60.09280412644832836, 16.11190982779557146 ) ) ;
#83695 = DIRECTION ( 'NONE',  ( -1.000000000000000000, 0.000000000000000000, 0.000000000000000000 ) ) ;
#83696 = CARTESIAN_POINT ( 'NONE',  ( 136.2587462434812267, 256.1427522451419350, 10.00000000000009415 ) ) ;
#83697 = CARTESIAN_POINT ( 'NONE',  ( -38.02969130575858969, 25.52022711230254615, 177.5919119679930134 ) ) ;
#83698 = CARTESIAN_POINT ( 'NONE',  ( 189.1862045837368385, 268.2028127389427254, 13.82493371562940432 ) ) ;
#83699 = CYLINDRICAL_SURFACE ( 'NONE', #8914, 10.00000000000010658 ) ;
#83700 = CARTESIAN_POINT ( 'NONE',  ( 164.1989670955858571, 281.5052563180250900, 9.464287345521309902 ) ) ;
#83701 = CARTESIAN_POINT ( 'NONE',  ( 12.93608109523609073, 25.65586893147755276, -7.433330006724137462 ) ) ;
#83702 = CARTESIAN_POINT ( 'NONE',  ( 148.3280470635002928, 273.7352816289870248, 9.058704604771318003 ) ) ;
#83703 = CARTESIAN_POINT ( 'NONE',  ( 71.94031269653281413, 59.11929964053626918, 15.87436981764813559 ) ) ;
#83704 = CARTESIAN_POINT ( 'NONE',  ( 187.0083344850037008, 268.0836409071914090, -15.22627500120235133 ) ) ;
#83705 = VERTEX_POINT ( 'NONE', #53200 ) ;
#83706 = CIRCLE ( 'NONE', #57768, 17.82106496071138935 ) ;
#83707 = CARTESIAN_POINT ( 'NONE',  ( 86.56379725475841269, 45.50107930069437856, -7.807079406273517819 ) ) ;
#83708 = DIRECTION ( 'NONE',  ( 0.000000000000000000, 0.000000000000000000, 1.000000000000000000 ) ) ;
#83709 = CARTESIAN_POINT ( 'NONE',  ( 75.35001427908503047, 53.53583770442167378, -16.04486494172472888 ) ) ;
#83710 = CARTESIAN_POINT ( 'NONE',  ( 81.61450380106850844, 42.00667554686729233, 7.576096789987255775 ) ) ;
#83711 = ORIENTED_EDGE ( 'NONE', *, *, #90057, .F. ) ;
#83712 = DIRECTION ( 'NONE',  ( 0.8660254037844382635, 0.5000000000000005551, 0.000000000000000000 ) ) ;
#83713 = CARTESIAN_POINT ( 'NONE',  ( -17.42236680055705023, 149.2012482093457777, 0.000000000000000000 ) ) ;
#83714 = CARTESIAN_POINT ( 'NONE',  ( 77.22942826013965600, 63.41635481091116588, 15.12246632917587519 ) ) ;
#83715 = CARTESIAN_POINT ( 'NONE',  ( 154.9903553346911735, 262.1958252075976361, -18.39016733948542637 ) ) ;
#83716 = ORIENTED_EDGE ( 'NONE', *, *, #29214, .F. ) ;
#83717 = ORIENTED_EDGE ( 'NONE', *, *, #17831, .T. ) ;
#83718 = AXIS2_PLACEMENT_3D ( 'NONE', #22596, #69186, #60079 ) ;
#83720 = DIRECTION ( 'NONE',  ( 0.000000000000000000, 0.000000000000000000, 1.000000000000000000 ) ) ;
#83719 = CARTESIAN_POINT ( 'NONE',  ( 190.6688270659779221, 284.0946164064107506, -17.60360843008351495 ) ) ;
#83721 = ORIENTED_EDGE ( 'NONE', *, *, #94341, .F. ) ;
#83722 = CARTESIAN_POINT ( 'NONE',  ( 153.2513309553138470, 265.2079037882803618, -16.24091495603130397 ) ) ;
#83723 = CARTESIAN_POINT ( 'NONE',  ( 70.20579083185378977, 65.41824112225215515, 12.26219425119750639 ) ) ;
#83724 = CARTESIAN_POINT ( 'NONE',  ( 80.12177396824181130, 57.42895151072963955, -16.59339316893575145 ) ) ;
#83725 = CARTESIAN_POINT ( 'NONE',  ( 47.05812965368398437, 204.6427522451419350, -10.00000000000009592 ) ) ;
#83726 = ORIENTED_EDGE ( 'NONE', *, *, #74556, .F. ) ;
#83727 = FACE_OUTER_BOUND ( 'NONE', #55353, .T. ) ;
#83728 = ORIENTED_EDGE ( 'NONE', *, *, #74265, .T. ) ;
#83729 = CARTESIAN_POINT ( 'NONE',  ( 165.0538309624641613, 244.7653741195639157, 2.311334310144196547 ) ) ;
#83730 = CARTESIAN_POINT ( 'NONE',  ( 74.55249937888110878, 63.44298656893680999, 14.44720752827713284 ) ) ;
#83731 = VERTEX_POINT ( 'NONE', #60773 ) ;
#83732 = EDGE_CURVE ( 'NONE', #44175, #2508, #69663, .T. ) ;
#83733 = CARTESIAN_POINT ( 'NONE',  ( 190.4841013044967042, 300.7188538369516095, 4.682298117523464143 ) ) ;
#83734 = DIRECTION ( 'NONE',  ( 1.000000000000000000, 0.000000000000000000, 0.000000000000000000 ) ) ;
#83735 = ORIENTED_EDGE ( 'NONE', *, *, #52335, .F. ) ;
#83736 = LINE ( 'NONE', #76124, #51414 ) ;
#83737 = CARTESIAN_POINT ( 'NONE',  ( 25.50001727096127979, 173.9824982072973967, 3.021315404115420679E-15 ) ) ;
#83738 = CARTESIAN_POINT ( 'NONE',  ( 23.64814127513158937, 118.0650415295850451, 60.00000000000000000 ) ) ;
#83739 = CARTESIAN_POINT ( 'NONE',  ( 79.48876273271771709, 46.38894273206648222, -12.71961528548989406 ) ) ;
#83740 = VERTEX_POINT ( 'NONE', #99321 ) ;
#83741 = VERTEX_POINT ( 'NONE', #76990 ) ;
#83742 = CARTESIAN_POINT ( 'NONE',  ( 155.5487322651507043, 265.9491453245429398, -16.30937882781046611 ) ) ;
#83743 = CARTESIAN_POINT ( 'NONE',  ( 147.3984236761635884, 275.3454365677582700, 5.108566646342994844 ) ) ;
#83744 = CARTESIAN_POINT ( 'NONE',  ( 190.3049670482083684, 301.0291234702190764, 0.2225066852051815758 ) ) ;
#83745 = CARTESIAN_POINT ( 'NONE',  ( 190.0707697440390689, 301.4347651000360884, 4.271360729158901748 ) ) ;
#83746 = CARTESIAN_POINT ( 'NONE',  ( 192.6797324865049745, 296.9159090750308110, 12.42053959885222625 ) ) ;
#83747 = EDGE_CURVE ( 'NONE', #98547, #26987, #22300, .T. ) ;
#83748 = FACE_OUTER_BOUND ( 'NONE', #11116, .T. ) ;
#83749 = EDGE_CURVE ( 'NONE', #11268, #28252, #29203, .T. ) ;
#83750 = CARTESIAN_POINT ( 'NONE',  ( -19.65312891409030271, 93.06504152958497400, 10.00000000000000888 ) ) ;
#83751 = LINE ( 'NONE', #35617, #2764 ) ;
#83752 = VECTOR ( 'NONE', #45579, 999.9999999999998863 ) ;
#83753 = CARTESIAN_POINT ( 'NONE',  ( 71.23563381243731385, 70.03978810160823798, 6.894242474657360731 ) ) ;
#83754 = CARTESIAN_POINT ( 'NONE',  ( 85.81045474425822306, 231.8967562850347122, -4.648177544792955347E-16 ) ) ;
#83755 = CARTESIAN_POINT ( 'NONE',  ( 66.97555164495814495, 67.03582895754806259, 8.583456203666562701 ) ) ;
#83756 = CARTESIAN_POINT ( 'NONE',  ( 25.98835327777827686, 41.64452202306098627, -10.00000000000000000 ) ) ;
#83757 = CARTESIAN_POINT ( 'NONE',  ( 78.33682591320163624, 47.43237704492500484, 14.30218028890826076 ) ) ;
#83758 = VECTOR ( 'NONE', #49513, 1000.000000000000000 ) ;
#83759 = ORIENTED_EDGE ( 'NONE', *, *, #66712, .T. ) ;
#83760 = CARTESIAN_POINT ( 'NONE',  ( 48.48788556946983874, 102.1758113618167982, -10.00000000000000000 ) ) ;
#83761 = CARTESIAN_POINT ( 'NONE',  ( 72.24611734329810986, 70.10459536098181843, 7.832089211065604850 ) ) ;
#83762 = CARTESIAN_POINT ( 'NONE',  ( 149.4596969528118393, 273.7752065243203106, 10.43958276706939614 ) ) ;
#83763 = CARTESIAN_POINT ( 'NONE',  ( 79.49710624387913072, 46.36387489428066999, 12.69932268971443357 ) ) ;
#83764 = CARTESIAN_POINT ( 'NONE',  ( 192.0122163493551284, 297.6569496777016752, -9.909203487807042521 ) ) ;
#83765 = CARTESIAN_POINT ( 'NONE',  ( 83.53204454370724363, 52.39401912150449903, -15.17729711222451883 ) ) ;
#83766 = CARTESIAN_POINT ( 'NONE',  ( 169.3013571053814132, 285.1638214189113114, -7.896588100169458890 ) ) ;
#83767 = ORIENTED_EDGE ( 'NONE', *, *, #35077, .T. ) ;
#83768 = CARTESIAN_POINT ( 'NONE',  ( 170.0174658539383188, 255.2014620101463720, -11.63331499112131873 ) ) ;
#83769 = PRESENTATION_LAYER_ASSIGNMENT (  '', '', ( #98349 ) ) ;
#83770 = CARTESIAN_POINT ( 'NONE',  ( 159.2536436069973718, 254.8115933126508992, -15.76697951715411250 ) ) ;
#83771 = FACE_OUTER_BOUND ( 'NONE', #35830, .T. ) ;
#83772 = CARTESIAN_POINT ( 'NONE',  ( 39.26390101962404344, 200.1427522451419350, -10.00000000000009415 ) ) ;
#83773 = CARTESIAN_POINT ( 'NONE',  ( 110.0524566828198232, 234.3458772461660544, 9.188101187500095079 ) ) ;
#83774 = LINE ( 'NONE', #98953, #98012 ) ;
#83775 = CARTESIAN_POINT ( 'NONE',  ( 24.19030146973739193, 38.49624447322263876, -10.00000000000000000 ) ) ;
#83776 = CARTESIAN_POINT ( 'NONE',  ( 195.8449251089225811, 291.4336346372613775, 16.14492769602857081 ) ) ;
#83777 = CARTESIAN_POINT ( 'NONE',  ( 175.4589951177797218, 253.5542521767871165, -4.185393656649594618 ) ) ;
#83778 = CARTESIAN_POINT ( 'NONE',  ( 34.70824655357364463, 190.8458772461660544, 9.188101187500095079 ) ) ;
#83779 = LINE ( 'NONE', #37620, #33345 ) ;
#83780 = CIRCLE ( 'NONE', #43305, 10.99999999999989164 ) ;
#83781 = VERTEX_POINT ( 'NONE', #23286 ) ;
#83782 = CARTESIAN_POINT ( 'NONE',  ( 191.1855593189403635, 298.9439214236015232, 7.483141010870764553 ) ) ;
#83783 = CARTESIAN_POINT ( 'NONE',  ( 181.3202242451768598, 267.7749618620028969, 14.98405922250201705 ) ) ;
#83784 = CARTESIAN_POINT ( 'NONE',  ( 73.32799597867342811, 60.88228677579900960, 15.59493297680661250 ) ) ;
#83785 = LINE ( 'NONE', #45235, #85602 ) ;
#83786 = CARTESIAN_POINT ( 'NONE',  ( 81.65911681526914379, 41.55393351364236310, -5.423798156015772420 ) ) ;
#83787 = DIRECTION ( 'NONE',  ( -0.4472135954999574281, -0.7745966692414834043, 0.4472135954999583718 ) ) ;
#83788 = CARTESIAN_POINT ( 'NONE',  ( 182.2306686641913132, 262.8049073495537300, 12.70932774860379411 ) ) ;
#83789 = CIRCLE ( 'NONE', #46563, 70.00000000000001421 ) ;
#83790 = CARTESIAN_POINT ( 'NONE',  ( 98.22579726061456995, 237.5177522451419350, 5.000000000000046185 ) ) ;
#83791 = ORIENTED_EDGE ( 'NONE', *, *, #63015, .F. ) ;
#83792 = CARTESIAN_POINT ( 'NONE',  ( 198.5886434392601529, 267.8836247115091851, -8.069141051336366388 ) ) ;
#83793 = B_SPLINE_CURVE_WITH_KNOTS ( 'NONE', 3,
 ( #90586, #59605, #99637, #45892, #75346, #83967, #43916, #14027, #6434, #53509, #21151, #76815, #67729, #29237, #74855, #5437, #44908, #30219, #75849, #82970, #38302, #37312, #82492, #76342, #84463, #68712, #68212, #60103, #5927, #13544, #36318, #22122, #91069, #99137, #6916, #29724, #53014, #69211, #21632, #37803, #52514, #14531, #83463, #45410 ),
 .UNSPECIFIED., .F., .F.,
 ( 4, 2, 2, 2, 2, 2, 2, 2, 2, 2, 2, 2, 2, 2, 2, 2, 2, 2, 2, 2, 2, 4 ),
 ( 0.002160350574709204823, 0.002597591355362379503, 0.002816211745688940171, 0.003034832136015500406, 0.003144142331178779223, 0.003253452526342058039, 0.003362762721505337289, 0.003472072916668616106, 0.003909313697321794255, 0.004783795258628099380, 0.005658276819934403637, 0.006532758381240707894, 0.006969999161893860457, 0.007407239942547013019, 0.007516550137710215941, 0.007571205235291765361, 0.007625860332873313913, 0.007735170528036391935, 0.007844480723199469957, 0.008281721503852156746, 0.008718962284504843535, 0.009156203065157532059 ),
 .UNSPECIFIED. ) ;
#83794 = CARTESIAN_POINT ( 'NONE',  ( 156.8729383767137904, 280.5345233313491349, -1.585272415347215080 ) ) ;
#83795 = CARTESIAN_POINT ( 'NONE',  ( 154.7326666781059714, 263.9299083186784287, 17.15468183873104735 ) ) ;
#83796 = ADVANCED_FACE ( 'NONE', ( #85141 ), #46581, .T. ) ;
#83797 = CARTESIAN_POINT ( 'NONE',  ( 16.84647260051960060, 180.5333772461660544, 9.188101187500095079 ) ) ;
#83798 = CARTESIAN_POINT ( 'NONE',  ( 15.82204613103260904, 8.944730856513908535, 1.475505719884397138E-15 ) ) ;
#83799 = CARTESIAN_POINT ( 'NONE',  ( 196.1666432693615718, 273.5625105224574440, 15.08246463373486002 ) ) ;
#83800 = CARTESIAN_POINT ( 'NONE',  ( 71.93836645383190387, 59.32121692304542648, -15.31782635615035026 ) ) ;
#83801 = CYLINDRICAL_SURFACE ( 'NONE', #2220, 16.60714546451156792 ) ;
#83803 = CARTESIAN_POINT ( 'NONE',  ( 63.96340690334295687, 216.9244531367911293, -4.594050593750046652 ) ) ;
#83802 = CARTESIAN_POINT ( 'NONE',  ( 174.5805834809822557, 286.5546214993515832, 10.25926391534427751 ) ) ;
#83804 = EDGE_CURVE ( 'NONE', #45170, #86137, #74176, .T. ) ;
#83805 = CARTESIAN_POINT ( 'NONE',  ( 208.1876422586379647, 270.0554214305024630, 3.377638779759113863 ) ) ;
#83806 = CARTESIAN_POINT ( 'NONE',  ( 72.75281560095611155, 57.10416661572288177, 16.38170419688453805 ) ) ;
#83807 = CARTESIAN_POINT ( 'NONE',  ( -54.21831688459418785, 33.63902229265146104, -10.00000000000000000 ) ) ;
#83808 = CARTESIAN_POINT ( 'NONE',  ( 66.38349642218635438, 68.19267280352575256, -4.414189003008335277 ) ) ;
#83809 = ORIENTED_EDGE ( 'NONE', *, *, #79482, .T. ) ;
#83810 = CARTESIAN_POINT ( 'NONE',  ( 19.21902136474470524, 175.2365022471902023, 10.00000000000009592 ) ) ;
#83811 = CARTESIAN_POINT ( 'NONE',  ( 163.8455942243524248, 246.8581015375447691, -7.178103170949780676 ) ) ;
#83812 = CARTESIAN_POINT ( 'NONE',  ( 139.7141738582018604, 239.2202760586659736, -5.415160957724236172E-17 ) ) ;
#83813 = CARTESIAN_POINT ( 'NONE',  ( 20.70865909420142259, 30.14336893147755703, 7.433330006724141015 ) ) ;
#83815 = EDGE_CURVE ( 'NONE', #91193, #67048, #81034, .T. ) ;
#83814 = CARTESIAN_POINT ( 'NONE',  ( 207.0452084649157314, 272.0341748055130324, -8.323635130805319804 ) ) ;
#83816 = CARTESIAN_POINT ( 'NONE',  ( 38.04107491472452551, 53.42442038713602415, -10.00000000000000000 ) ) ;
#83817 = CARTESIAN_POINT ( 'NONE',  ( 75.27993480048328934, 53.55678813946182260, -16.04991370599387679 ) ) ;
#83819 = CARTESIAN_POINT ( 'NONE',  ( 167.0546803224166297, 282.1702852132879684, 12.27869116404093752 ) ) ;
#83818 = CARTESIAN_POINT ( 'NONE',  ( 88.26049611827410502, 43.94792280741878443, 2.484900765466354855 ) ) ;
#83820 = CARTESIAN_POINT ( 'NONE',  ( 68.50372518212984119, 64.31961559923436766, 12.35208758802623130 ) ) ;
#83821 = VERTEX_POINT ( 'NONE', #63295 ) ;
#83822 = PLANE ( 'NONE',  #50373 ) ;
#83823 = AXIS2_PLACEMENT_3D ( 'NONE', #38837, #353, #62126 ) ;
#83824 = CARTESIAN_POINT ( 'NONE',  ( 180.9536487871291968, 287.8037316094353741, 14.06327251346537288 ) ) ;
#83825 = CARTESIAN_POINT ( 'NONE',  ( 156.6568488211063936, 280.3666888851813610, -5.413563403562074328 ) ) ;
#83826 = CARTESIAN_POINT ( 'NONE',  ( 197.0727265385168607, 273.0519042339707312, -13.37462020030573484 ) ) ;
#83827 = VERTEX_POINT ( 'NONE', #10105 ) ;
#83828 = CARTESIAN_POINT ( 'NONE',  ( 160.1202562673349803, 253.3105761544636039, 14.69629115143539266 ) ) ;
#83829 = VECTOR ( 'NONE', #87998, 1000.000000000000000 ) ;
#83830 = CARTESIAN_POINT ( 'NONE',  ( 170.7822565925250160, 283.8216418346244723, -11.11151730791865511 ) ) ;
#83831 = B_SPLINE_SURFACE_WITH_KNOTS ( 'NONE', 3, 1, ( 
 ( #1133, #41105 ),
 ( #17320, #16324 ),
 ( #25419, #47217 ),
 ( #9227, #62920 ),
 ( #2644, #25943 ),
 ( #2139, #48225 ),
 ( #71046, #32532 ),
 ( #87308, #63426 ),
 ( #56818, #24919 ),
 ( #55793, #33022 ),
 ( #40611, #56312 ),
 ( #63920, #17841 ),
 ( #48742, #79674 ),
 ( #87801, #97347 ),
 ( #27913, #57316 ),
 ( #73535, #65422 ),
 ( #97838, #66909 ),
 ( #59287, #41611 ),
 ( #82169, #96365 ),
 ( #12744, #36004 ),
 ( #88286, #96868 ),
 ( #95879, #80676 ),
 ( #28407, #18840 ),
 ( #49720, #50218 ),
 ( #81172, #11737 ),
 ( #11252, #42115 ),
 ( #26931, #42601 ),
 ( #35011, #65911 ),
 ( #58310, #73049 ),
 ( #3642, #89764 ),
 ( #81660, #26437 ),
 ( #4116, #80170 ),
 ( #34523, #57810 ),
 ( #88789, #49236 ) ),
 .UNSPECIFIED., .T., .F., .F.,
 ( 4, 2, 2, 2, 2, 2, 2, 2, 2, 2, 2, 2, 2, 2, 2, 2, 4 ),
 ( 2, 2 ),
 ( 0.000000000000000000, 0.06250000000000000000, 0.1250000000000000000, 0.1875000000000000000, 0.2500000000000000000, 0.3125000000000000000, 0.3750000000000000000, 0.4375000000000000000, 0.5000000000000000000, 0.5625000000000000000, 0.6250000000000000000, 0.6875000000000000000, 0.7500000000000000000, 0.8125000000000000000, 0.8750000000000000000, 0.9375000000000000000, 1.000000000000000000 ),
 ( 0.000000000000000000, 1.000000000000000000 ),
 .UNSPECIFIED. ) ;
#83832 = EDGE_CURVE ( 'NONE', #34316, #1591, #49103, .T. ) ;
#83833 = CARTESIAN_POINT ( 'NONE',  ( 200.6945232828033738, 282.6247322300178553, -16.66035973746479826 ) ) ;
#83834 = FACE_OUTER_BOUND ( 'NONE', #23765, .T. ) ;
#83835 = CARTESIAN_POINT ( 'NONE',  ( 32.33569778934854355, 196.1427522451419065, 10.00000000000009415 ) ) ;
#83836 = CARTESIAN_POINT ( 'NONE',  ( 208.2874212803407090, 269.8825990953837390, -1.143705256421198690 ) ) ;
#83837 = CARTESIAN_POINT ( 'NONE',  ( 201.4617167010348737, 281.7050662241970826, -17.43131506460443703 ) ) ;
#83838 = COLOUR_RGB ( '',0.7921568627450980005, 0.8196078431372548767, 0.9333333333333333481 ) ;
#83839 = ORIENTED_EDGE ( 'NONE', *, *, #59767, .F. ) ;
#83840 = FACE_OUTER_BOUND ( 'NONE', #6055, .T. ) ;
#83841 = CARTESIAN_POINT ( 'NONE',  ( 14.86318692873816083, 16.78052372038639106, -10.00000000000000355 ) ) ;
#83842 = CARTESIAN_POINT ( 'NONE',  ( 82.71715233927223210, 44.61979091911242534, 10.25119714958372796 ) ) ;
#83843 = ORIENTED_EDGE ( 'NONE', *, *, #31600, .T. ) ;
#83844 = CARTESIAN_POINT ( 'NONE',  ( 148.9275518150011806, 272.6969089400084272, 12.34519124974546500 ) ) ;
#83845 = PLANE ( 'NONE',  #88850 ) ;
#83846 = CARTESIAN_POINT ( 'NONE',  ( 189.0627537881084379, 297.0799250450181148, 8.091751816178462064 ) ) ;
#83847 = EDGE_LOOP ( 'NONE', ( #7670, #36738, #1198, #43161 ) ) ;
#83848 = CARTESIAN_POINT ( 'NONE',  ( -30.18034446749236821, 25.12100238203590763, -10.00000000000000000 ) ) ;
#83849 = CARTESIAN_POINT ( 'NONE',  ( 79.19548930461118630, 59.90515312544784621, -16.13566294680261848 ) ) ;
#83850 = AXIS2_PLACEMENT_3D ( 'NONE', #47047, #954, #22755 ) ;
#83851 = CARTESIAN_POINT ( 'NONE',  ( 164.1224127655298730, 246.3786377597482158, 7.356982420601481998 ) ) ;
#83852 = CARTESIAN_POINT ( 'NONE',  ( 69.82384421004434216, 62.57021116271138794, 13.43531312277882250 ) ) ;
#83853 = ORIENTED_EDGE ( 'NONE', *, *, #76724, .F. ) ;
#83854 = CARTESIAN_POINT ( 'NONE',  ( 97.65764163903753570, 221.0643266524160424, 9.188101187500095079 ) ) ;
#83855 = CARTESIAN_POINT ( 'NONE',  ( 203.1289230791707325, 278.8173800705629901, 16.48573034889792766 ) ) ;
#83856 = CARTESIAN_POINT ( 'NONE',  ( 170.7953178271928039, 255.2457615276028093, -12.92277808742838374 ) ) ;
#83857 = CARTESIAN_POINT ( 'NONE',  ( 180.9057600473689149, 270.9297146850697686, -15.98331193678458106 ) ) ;
#83858 = CARTESIAN_POINT ( 'NONE',  ( 81.39901424530387430, 42.08420399104508647, -7.907947396089951120 ) ) ;
#83859 = B_SPLINE_SURFACE_WITH_KNOTS ( 'NONE', 3, 1, ( 
 ( #15763, #78595 ),
 ( #40054, #46669 ),
 ( #23865, #39051 ),
 ( #578, #31462 ),
 ( #62353, #54757 ),
 ( #85743, #33481 ),
 ( #96314, #81127 ),
 ( #17790, #88737 ),
 ( #34001, #25373 ),
 ( #10188, #64886 ),
 ( #86736, #24870 ),
 ( #17272, #79119 ),
 ( #73003, #40560 ),
 ( #50174, #55744 ),
 ( #9700, #87752 ),
 ( #72507, #2595 ),
 ( #48690, #94316 ),
 ( #71990, #48175 ),
 ( #87257, #63377 ),
 ( #49669, #80123 ),
 ( #88238, #71496 ),
 ( #56264, #95832 ),
 ( #57761, #95341 ),
 ( #63874, #1598 ),
 ( #42071, #3115 ),
 ( #42553, #11694 ),
 ( #18789, #49187 ),
 ( #26385, #64379 ),
 ( #94811, #79625 ),
 ( #56770, #10685 ),
 ( #41054, #2089 ) ),
 .UNSPECIFIED., .F., .F., .F.,
 ( 4, 3, 3, 3, 3, 3, 3, 3, 3, 3, 4 ),
 ( 2, 2 ),
 ( 0.000000000000000000, 0.1122669598086822457, 0.2243161639709664035, 0.3396355846219253349, 0.4553962076585191809, 0.5677860799922548329, 0.6749047109689760848, 0.7773884377078600361, 0.8775581155834486502, 0.9782364162378277550, 1.000000000000000000 ),
 ( 0.000000000000000000, 1.000000000000000000 ),
 .UNSPECIFIED. ) ;
#83860 = ORIENTED_EDGE ( 'NONE', *, *, #13294, .T. ) ;
#83861 = EDGE_CURVE ( 'NONE', #85923, #63494, #3031, .T. ) ;
#83862 = ORIENTED_EDGE ( 'NONE', *, *, #77991, .T. ) ;
#83863 = VERTEX_POINT ( 'NONE', #1005 ) ;
#83864 = CARTESIAN_POINT ( 'NONE',  ( 80.96741822347986783, 48.36393785198333717, 13.47256384055967615 ) ) ;
#83865 = VERTEX_POINT ( 'NONE', #40968 ) ;
#83866 = CARTESIAN_POINT ( 'NONE',  ( 70.61809369003644576, 71.23760416348828528, 2.495634273706798023 ) ) ;
#83867 = DIRECTION ( 'NONE',  ( -0.000000000000000000, -0.000000000000000000, -1.000000000000000000 ) ) ;
#83868 = EDGE_LOOP ( 'NONE', ( #25266, #97299, #97188, #88777 ) ) ;
#83869 = ADVANCED_FACE ( 'NONE', ( #24788 ), #32398, .T. ) ;
#83870 = CARTESIAN_POINT ( 'NONE',  ( 164.4578252119609090, 245.7976863610386999, -6.211333091911165560 ) ) ;
#83871 = VECTOR ( 'NONE', #56947, 999.9999999999998863 ) ;
#83872 = CARTESIAN_POINT ( 'NONE',  ( 170.6484802770005729, 282.9697387111801845, 11.87827476712554997 ) ) ;
#83873 = CARTESIAN_POINT ( 'NONE',  ( 142.4134467818605572, 241.4824982072973967, 3.021315404115420679E-15 ) ) ;
#83874 = CARTESIAN_POINT ( 'NONE',  ( 82.84778848911861360, 53.43038316853105840, -15.30831281788561604 ) ) ;
#83875 = EDGE_CURVE ( 'NONE', #76591, #10673, #51841, .T. ) ;
#83876 = ORIENTED_EDGE ( 'NONE', *, *, #84448, .F. ) ;
#83877 = CARTESIAN_POINT ( 'NONE',  ( 66.33533107015807673, 68.87447202099198762, 0.1160252125227696635 ) ) ;
#83878 = CARTESIAN_POINT ( 'NONE',  ( 11.06573324809563807, 29.49540643055186351, 3.479690158560446702E-15 ) ) ;
#83879 = CARTESIAN_POINT ( 'NONE',  ( 164.4771589409865555, 281.7954605369791921, 8.842136975255975528 ) ) ;
#83880 = CARTESIAN_POINT ( 'NONE',  ( 80.50883317518791671, 57.72730120993126235, 16.59589928958306615 ) ) ;
#83882 = VERTEX_POINT ( 'NONE', #57183 ) ;
#83881 = DIRECTION ( 'NONE',  ( 0.000000000000000000, 0.000000000000000000, 1.000000000000000000 ) ) ;
#83883 = EDGE_CURVE ( 'NONE', #87907, #38349, #48609, .T. ) ;
#83884 = CARTESIAN_POINT ( 'NONE',  ( 53.17212233558426959, 213.0530062829863311, -4.648177544792955347E-16 ) ) ;
#83885 = CARTESIAN_POINT ( 'NONE',  ( 185.1676822857243963, 258.5668278037668983, 2.933763201912603424 ) ) ;
#83886 = CARTESIAN_POINT ( 'NONE',  ( 160.6907952011062264, 281.0816080609710639, -6.606445984059675425 ) ) ;
#83887 = CARTESIAN_POINT ( 'NONE',  ( 165.8568044060308182, 246.3531759204054481, -2.743205800353976542 ) ) ;
#83888 = CARTESIAN_POINT ( 'NONE',  ( 192.7705046643033313, 292.1170781437433561, -14.65601932715136435 ) ) ;
#83889 = CARTESIAN_POINT ( 'NONE',  ( 171.3768758103641972, 255.5877274061340643, 11.19587476605279441 ) ) ;
#83890 = CARTESIAN_POINT ( 'NONE',  ( 193.5872375690405534, 263.2763237561280221, -0.7636422199292929314 ) ) ;
#83891 = ORIENTED_EDGE ( 'NONE', *, *, #33756, .T. ) ;
#83892 = CARTESIAN_POINT ( 'NONE',  ( 155.7133958608191620, 260.9434822804128657, -18.28034026974484405 ) ) ;
#83893 = VECTOR ( 'NONE', #95403, 1000.000000000000114 ) ;
#83894 = DIRECTION ( 'NONE',  ( -0.000000000000000000, 1.000000000000000000, -0.000000000000000000 ) ) ;
#83895 = CARTESIAN_POINT ( 'NONE',  ( 6.860117161356369841, 164.7677522451418213, -5.000000000000041744 ) ) ;
#83896 = CARTESIAN_POINT ( 'NONE',  ( 82.86724755478759619, 53.49721348986128788, -15.32433688253754589 ) ) ;
#83897 = CARTESIAN_POINT ( 'NONE',  ( 173.7861983198416453, 280.7065551239853107, -14.21705231541378467 ) ) ;
#83898 = CARTESIAN_POINT ( 'NONE',  ( 163.9733507041129883, 246.6368208236034718, -8.809407376596537276 ) ) ;
#83899 = CARTESIAN_POINT ( 'NONE',  ( 87.10342204727412252, 44.68451332791826758, -5.678729796000945740 ) ) ;
#83900 = VECTOR ( 'NONE', #14934, 1000.000000000000000 ) ;
#83901 = CARTESIAN_POINT ( 'NONE',  ( 72.49654942766741783, 70.83148394934322312, 7.643478247317291974 ) ) ;
#83903 = CARTESIAN_POINT ( 'NONE',  ( -6.583630525541995127, 178.5530062829863027, -4.648177544792955347E-16 ) ) ;
#83902 = CARTESIAN_POINT ( 'NONE',  ( -2.963858511049441979, 169.0958772461660544, -9.188101187500095079 ) ) ;
#83904 = CARTESIAN_POINT ( 'NONE',  ( 185.0534184758703873, 295.4269076067080846, 8.465056994707534699 ) ) ;
#83905 = EDGE_LOOP ( 'NONE', ( #49079, #31738, #18978, #64564 ) ) ;
#83906 = AXIS2_PLACEMENT_3D ( 'NONE', #43693, #13321, #28492 ) ;
#83907 = ORIENTED_EDGE ( 'NONE', *, *, #62585, .T. ) ;
#83908 = CARTESIAN_POINT ( 'NONE',  ( -27.42236680055714260, 166.5217562850347406, 1.224646799147364892E-15 ) ) ;
#83909 = DIRECTION ( 'NONE',  ( -0.8660254037844375974, -0.5000000000000016653, 0.000000000000000000 ) ) ;
#83910 = CARTESIAN_POINT ( 'NONE',  ( 86.19494322620172966, 45.94452022226197130, -8.806296680070143879 ) ) ;
#83911 = CARTESIAN_POINT ( 'NONE',  ( 86.50609478078892778, 43.48068990056189165, 2.985191827711138224 ) ) ;
#83912 = CARTESIAN_POINT ( 'NONE',  ( 162.4934061880776426, 249.2001599177594073, -11.48506854272206290 ) ) ;
#83913 = VECTOR ( 'NONE', #31979, 1000.000000000000227 ) ;
#83914 = CARTESIAN_POINT ( 'NONE',  ( -24.63924516542738274, 141.7012482093459198, 1.732050807568909834 ) ) ;
#83915 = CARTESIAN_POINT ( 'NONE',  ( 153.3856580278162198, 278.7073591447287413, 3.760990798762666731 ) ) ;
#83916 = CARTESIAN_POINT ( 'NONE',  ( 17.63104780087548562, 190.1744531367911293, 4.594050593750047540 ) ) ;
#83917 = CARTESIAN_POINT ( 'NONE',  ( 127.4544149619371609, 235.2048013555409796, 4.594050593750051981 ) ) ;
#83918 = CARTESIAN_POINT ( 'NONE',  ( 2.487887237287232711, 134.7156766241960497, -21.50000000000001421 ) ) ;
#83919 = CARTESIAN_POINT ( 'NONE',  ( -29.91485116994501325, 25.08783183303773967, 10.00000000000000000 ) ) ;
#83920 = CARTESIAN_POINT ( 'NONE',  ( 78.45979614097025490, 53.37690925373113515, 15.81233777137573071 ) ) ;
#83921 = AXIS2_PLACEMENT_3D ( 'NONE', #55908, #36116, #3266 ) ;
#83922 = CARTESIAN_POINT ( 'NONE',  ( 51.80235952159636525, 85.00000000000000000, 59.99999999999999289 ) ) ;
#83923 = CARTESIAN_POINT ( 'NONE',  ( 82.47813483566071113, 52.69574577809284932, -15.09840053849920949 ) ) ;
#83924 = CARTESIAN_POINT ( 'NONE',  ( 190.7982574810033611, 262.8194055429554510, 8.405793748174573921 ) ) ;
#83925 = CARTESIAN_POINT ( 'NONE',  ( 207.8984236726843164, 270.5563627158673512, -6.084369154771423815 ) ) ;
#83926 = DIRECTION ( 'NONE',  ( 1.000000000000000000, 1.962715704248044129E-13, 0.000000000000000000 ) ) ;
#83927 = CARTESIAN_POINT ( 'NONE',  ( 167.8450657302246896, 278.1957396450247302, 14.42841292292709809 ) ) ;
#83928 = CARTESIAN_POINT ( 'NONE',  ( -1.387478102835363769, 181.5530062829863596, 2.649461200531984646E-14 ) ) ;
#83929 = CARTESIAN_POINT ( 'NONE',  ( 70.78897776588866009, 71.07630443005777465, 3.566669968915905820 ) ) ;
#83930 = CARTESIAN_POINT ( 'NONE',  ( 184.2244543100441376, 268.3421717558753699, -15.77288757490104665 ) ) ;
#83931 = CARTESIAN_POINT ( 'NONE',  ( -47.78078991586325230, 28.96484896693081978, 177.5919119679930134 ) ) ;
#83932 = AXIS2_PLACEMENT_3D ( 'NONE', #28416, #27923, #4634 ) ;
#83933 = CARTESIAN_POINT ( 'NONE',  ( 184.8899540568645534, 269.3660042897924427, 16.00930444126497321 ) ) ;
#83934 = CARTESIAN_POINT ( 'NONE',  ( 86.23641098298274699, 232.8464784336661353, 1.353441290958777327E-15 ) ) ;
#83935 = CARTESIAN_POINT ( 'NONE',  ( 10.86724236217879458, 11.98920272979924206, 7.433330006724137462 ) ) ;
#83937 = EDGE_CURVE ( 'NONE', #34846, #54109, #93744, .T. ) ;
#83936 = CARTESIAN_POINT ( 'NONE',  ( 67.63114784964875525, 65.81005049607071555, 10.54782815381023831 ) ) ;
#83938 = DIRECTION ( 'NONE',  ( 0.5000000000000002220, -0.8660254037844385966, 0.000000000000000000 ) ) ;
#83940 = CARTESIAN_POINT ( 'NONE',  ( 85.53182313537475068, 42.77618286031957950, -1.864121902114932672 ) ) ;
#83939 = CARTESIAN_POINT ( 'NONE',  ( 11.07908504951724282, 25.13478043621386959, 8.090169943749478065 ) ) ;
#83941 = CARTESIAN_POINT ( 'NONE',  ( 196.4184597338679339, 290.4402435269564080, 17.72466505881568821 ) ) ;
#83942 = CARTESIAN_POINT ( 'NONE',  ( 173.9076247008792393, 277.9417859016587045, -16.84130823774900776 ) ) ;
#83943 = FACE_OUTER_BOUND ( 'NONE', #28885, .T. ) ;
#83944 = AXIS2_PLACEMENT_3D ( 'NONE', #51982, #13497, #29188 ) ;
#83945 = CARTESIAN_POINT ( 'NONE',  ( 37.59133656659162881, 37.10171378149920685, 9.188101187500008038 ) ) ;
#83946 = CARTESIAN_POINT ( 'NONE',  ( 127.6706609892855369, 244.5177522451418497, -10.00000000000009592 ) ) ;
#83947 = PLANE ( 'NONE',  #73369 ) ;
#83948 = ORIENTED_EDGE ( 'NONE', *, *, #70921, .T. ) ;
#83949 = CARTESIAN_POINT ( 'NONE',  ( 29.91980124543643171, 22.98920272979927759, 7.433330006724137462 ) ) ;
#83950 = CARTESIAN_POINT ( 'NONE',  ( 76.44525015969811932, 62.79367595106220534, -15.57143870397577778 ) ) ;
#83951 = CARTESIAN_POINT ( 'NONE',  ( 146.9370072200009645, 276.1446333132804511, -3.799807221059707363 ) ) ;
#83952 = EDGE_CURVE ( 'NONE', #44815, #6582, #39975, .T. ) ;
#83953 =( BOUNDED_CURVE ( )  B_SPLINE_CURVE ( 2, ( #43652, #75077, #27957, #29458, #76087, #44143, #89805, #20884, #74084 ),
 .UNSPECIFIED., .F., .F. ) 
 B_SPLINE_CURVE_WITH_KNOTS ( ( 3, 2, 2, 2, 3 ),
 ( 0.8266129032258064946, 0.8279569892473118697, 0.8306451612903226200, 0.8333333333333333703, 0.8346774193548387455 ),
 .UNSPECIFIED. ) 
 CURVE ( )  GEOMETRIC_REPRESENTATION_ITEM ( )  RATIONAL_B_SPLINE_CURVE ( ( 0.9330127018922194093, 0.9330127018922194093, 1.000000000000000000, 0.8660254037844387076, 1.000000000000000000, 0.8660254037844387076, 1.000000000000000000, 0.9330127018922194093, 0.9330127018922194093 ) ) 
 REPRESENTATION_ITEM ( '' )  );
#83954 = EDGE_CURVE ( 'NONE', #55638, #47161, #61508, .T. ) ;
#83955 = CARTESIAN_POINT ( 'NONE',  ( 70.39483845591227862, 61.02404926470979518, 14.91624238583182915 ) ) ;
#83956 = CARTESIAN_POINT ( 'NONE',  ( 159.9880386575927957, 253.5395837721924863, 15.85893018594752846 ) ) ;
#83957 = CARTESIAN_POINT ( 'NONE',  ( 179.8857559909177155, 262.7895619565915695, -12.79994536760057855 ) ) ;
#83958 = CARTESIAN_POINT ( 'NONE',  ( 173.2449941322521170, 253.6062056627853565, -9.189074487664372626 ) ) ;
#83959 = CARTESIAN_POINT ( 'NONE',  ( 152.6945189806187955, 266.1723304187151484, 16.62409282110771613 ) ) ;
#83960 = B_SPLINE_CURVE_WITH_KNOTS ( 'NONE', 3,
 ( #78943, #56607, #49021, #34311, #11031, #79954, #17618, #2433, #33835, #19139, #48523, #3435, #79459, #18628, #3914, #71330, #96652, #50013, #64722, #40391, #42392, #88577, #1922, #95671, #26219, #10024, #71835, #40886, #57095, #49505, #41908, #65210, #72843, #11532, #73325, #34795, #65698, #43394, #59075, #43893, #42878, #98120, #89087, #50496, #67705, #99118, #36793, #75824, #29700, #98632, #19636, #20618, #35302, #52491 ),
 .UNSPECIFIED., .F., .F.,
 ( 4, 2, 2, 2, 2, 2, 2, 2, 2, 2, 2, 2, 2, 2, 2, 2, 2, 2, 2, 2, 2, 2, 2, 2, 2, 2, 4 ),
 ( 0.0005556845649962375948, 0.001563194025267928330, 0.001815071390335872264, 0.002066948755403816632, 0.002192887437937828497, 0.002318826120471841230, 0.002444764803005853530, 0.002570703485539865829, 0.002822580850607883055, 0.003074458215675900715, 0.003578212945811939504, 0.004585722406084010577, 0.005593231866356081217, 0.006096986596492074903, 0.006348863961560030980, 0.006600741326627985323, 0.006663710667895039394, 0.006726680009162093465, 0.006789649350429147537, 0.006852618691696201608, 0.006978557374230344446, 0.007104496056764487283, 0.007356373421832811121, 0.007608250786901134960, 0.007860128151969458798, 0.008112005517037782637, 0.008615760247174428579 ),
 .UNSPECIFIED. ) ;
#83961 =( BOUNDED_CURVE ( )  B_SPLINE_CURVE ( 2, ( #22362, #69458, #37064, #99876, #6671, #23849, #565, #73, #60839 ),
 .UNSPECIFIED., .F., .T. ) 
 B_SPLINE_CURVE_WITH_KNOTS ( ( 3, 2, 2, 2, 3 ),
 ( 0.07661290322580645296, 0.07795698924731182811, 0.08064516129032257841, 0.08333333333333332871, 0.08467741935483871774 ),
 .UNSPECIFIED. ) 
 CURVE ( )  GEOMETRIC_REPRESENTATION_ITEM ( )  RATIONAL_B_SPLINE_CURVE ( ( 0.9330127018922194093, 0.9330127018922194093, 1.000000000000000000, 0.8660254037844387076, 1.000000000000000000, 0.8660254037844387076, 1.000000000000000000, 0.9330127018922189652, 0.9330127018922192983 ) ) 
 REPRESENTATION_ITEM ( '' )  );
#83962 = ORIENTED_EDGE ( 'NONE', *, *, #86968, .F. ) ;
#83963 = CARTESIAN_POINT ( 'NONE',  ( 73.63650596374165502, 69.59800771093053129, 10.20034856658873323 ) ) ;
#83964 = VECTOR ( 'NONE', #25034, 1000.000000000000114 ) ;
#83965 = ORIENTED_EDGE ( 'NONE', *, *, #47322, .T. ) ;
#83966 = CARTESIAN_POINT ( 'NONE',  ( 78.26458253827964029, 61.66843869688886315, 16.13698506349214057 ) ) ;
#83967 = CARTESIAN_POINT ( 'NONE',  ( 181.4778897503024098, 291.1215230031817214, -11.26139115722615536 ) ) ;
#83968 = EDGE_LOOP ( 'NONE', ( #66720, #85861, #86602, #43671, #94050, #65214 ) ) ;
#83969 = VECTOR ( 'NONE', #29948, 1000.000000000000114 ) ;
#83970 = CARTESIAN_POINT ( 'NONE',  ( 50.34412104557527812, 188.3262482093458061, 3.021315404115420679E-15 ) ) ;
#83971 = CARTESIAN_POINT ( 'NONE',  ( 58.47569090598247499, 179.7419560658249509, -18.47570218321543223 ) ) ;
#83972 = CARTESIAN_POINT ( 'NONE',  ( 84.90983652888880329, 50.15852115595398431, 13.71398460619150406 ) ) ;
#83973 = CARTESIAN_POINT ( 'NONE',  ( 153.4914073915022072, 264.7920792031019914, -16.65426974031797158 ) ) ;
#83974 = CARTESIAN_POINT ( 'NONE',  ( 152.9273493951901628, 265.7690563111299298, -17.70273273795505631 ) ) ;
#83975 = VECTOR ( 'NONE', #45213, 1000.000000000000000 ) ;
#83976 = CARTESIAN_POINT ( 'NONE',  ( -19.83262083840137180, 133.3759306620403891, 1.732050807568888073 ) ) ;
#83977 = AXIS2_PLACEMENT_3D ( 'NONE', #14282, #98406, #90839 ) ;
#83978 = CARTESIAN_POINT ( 'NONE',  ( 42.00264329202813229, 26.11110640527295601, -2.839279412974138328 ) ) ;
#83979 = CARTESIAN_POINT ( 'NONE',  ( -19.65312891409030271, 93.06504152958497400, 10.00000000000000888 ) ) ;
#83980 = CARTESIAN_POINT ( 'NONE',  ( 74.10991545788023416, 62.87482685241162272, -15.05254551912109306 ) ) ;
#83981 = CARTESIAN_POINT ( 'NONE',  ( 87.34834566700719449, 45.48627435691049214, 7.110058762634436924 ) ) ;
#83982 = ORIENTED_EDGE ( 'NONE', *, *, #78743, .F. ) ;
#83983 = ORIENTED_EDGE ( 'NONE', *, *, #10391, .T. ) ;
#83984 = CARTESIAN_POINT ( 'NONE',  ( 47.05668214639808156, 76.45164061169337799, -10.00000000000000000 ) ) ;
#83985 = CARTESIAN_POINT ( 'NONE',  ( 169.5454513700565258, 269.1796743676548544, 17.00868598083421546 ) ) ;
#83986 = AXIS2_PLACEMENT_3D ( 'NONE', #55042, #78880, #47445 ) ;
#83987 = EDGE_CURVE ( 'NONE', #61495, #72257, #45377, .T. ) ;
#83989 = CARTESIAN_POINT ( 'NONE',  ( 40.48539884740148409, 126.3902902409112556, -10.00000000000000000 ) ) ;
#83988 = CARTESIAN_POINT ( 'NONE',  ( -97.59541525468981149, 48.06504152958505216, 36.50000000000000000 ) ) ;
#83990 = CARTESIAN_POINT ( 'NONE',  ( 204.1411873440477223, 275.2830067746622262, 13.39149321096075163 ) ) ;
#83991 = CARTESIAN_POINT ( 'NONE',  ( 197.9681508493796116, 273.5361572027358079, -13.40667566358036211 ) ) ;
#83992 = CARTESIAN_POINT ( 'NONE',  ( 153.1198285439165545, 279.2890930352092482, 3.903594709581249322 ) ) ;
#83993 = CARTESIAN_POINT ( 'NONE',  ( 82.34540653027241319, 40.38296044905965232, 1.376546748157425171 ) ) ;
#83994 = CARTESIAN_POINT ( 'NONE',  ( 170.6068698651901627, 287.4926448325904857, -4.619150203187834869 ) ) ;
#83995 = CARTESIAN_POINT ( 'NONE',  ( 165.8826895886576835, 265.9047080510878800, 16.87347945222768786 ) ) ;
#83996 = ADVANCED_FACE ( 'NONE', ( #25818 ), #33921, .T. ) ;
#83997 = B_SPLINE_CURVE_WITH_KNOTS ( 'NONE', 3,
 ( #27629, #89468, #51914, #82854 ),
 .UNSPECIFIED., .F., .F.,
 ( 4, 4 ),
 ( 0.009100633809674477104, 0.01512941253790484920 ),
 .UNSPECIFIED. ) ;
#83998 = CARTESIAN_POINT ( 'NONE',  ( 186.7337682150368323, 287.1024196110707862, -15.92981707682468873 ) ) ;
#83999 = EDGE_CURVE ( 'NONE', #34456, #70878, #64808, .T. ) ;
#84000 = CARTESIAN_POINT ( 'NONE',  ( 105.6408794604690797, 240.9869531367911293, 4.594050593750046652 ) ) ;
#84001 = EDGE_LOOP ( 'NONE', ( #79802, #78850, #65548, #19086 ) ) ;
#84002 = CARTESIAN_POINT ( 'NONE',  ( 23.64814127513158226, 118.0650415295850451, -20.00000000000000355 ) ) ;
#84003 = CARTESIAN_POINT ( 'NONE',  ( 45.46674490716588224, 28.11110640527296312, -2.839279412974138328 ) ) ;
#84004 = DIRECTION ( 'NONE',  ( -0.4999999999999987788, 0.8660254037844392627, 0.000000000000000000 ) ) ;
#84005 = ORIENTED_EDGE ( 'NONE', *, *, #80039, .F. ) ;
#84006 = CIRCLE ( 'NONE', #61302, 70.00000000000001421 ) ;
#84007 = ORIENTED_EDGE ( 'NONE', *, *, #62394, .F. ) ;
#84008 = CARTESIAN_POINT ( 'NONE',  ( 74.18809600170575891, 68.48282398988669684, -11.62097119590897520 ) ) ;
#84009 = EDGE_CURVE ( 'NONE', #42330, #97214, #52798, .T. ) ;
#84010 = ADVANCED_FACE ( 'NONE', ( #19227 ), #89171, .F. ) ;
#84011 = CARTESIAN_POINT ( 'NONE',  ( 73.43762515466688967, 73.52662068827324049, 2.033788753608857291E-15 ) ) ;
#84012 = CARTESIAN_POINT ( 'NONE',  ( 42.33744422746375591, 122.7866300363639169, 10.00000000000000000 ) ) ;
#84013 = CARTESIAN_POINT ( 'NONE',  ( 25.43893178701101832, 38.18528772668521754, -1.583844403245329602 ) ) ;
#84014 = CARTESIAN_POINT ( 'NONE',  ( 22.53732574998906557, 13.41603393254324850, -1.583844403245362020 ) ) ;
#84015 = ORIENTED_EDGE ( 'NONE', *, *, #86491, .F. ) ;
#84016 = CARTESIAN_POINT ( 'NONE',  ( 148.6475519825707465, 273.1818828758886752, 9.184624051690363444 ) ) ;
#84017 = ORIENTED_EDGE ( 'NONE', *, *, #28193, .T. ) ;
#84018 = CARTESIAN_POINT ( 'NONE',  ( -41.40204166758637427, 67.93526189084366251, -10.00000000000000000 ) ) ;
#84019 = ORIENTED_EDGE ( 'NONE', *, *, #88568, .F. ) ;
#84020 = FACE_OUTER_BOUND ( 'NONE', #13080, .T. ) ;
#84021 = CARTESIAN_POINT ( 'NONE',  ( 192.7166103851607772, 263.3315064552393778, 4.497380725185501582 ) ) ;
#84022 = CARTESIAN_POINT ( 'NONE',  ( 156.6228368065803522, 262.3197220910723217, 17.02064833273061240 ) ) ;
#84023 = CARTESIAN_POINT ( 'NONE',  ( 15.22373782933244790, 168.0494855054051868, -2.679491924311274254 ) ) ;
#84025 = CARTESIAN_POINT ( 'NONE',  ( 82.30224259357629535, 41.51585266698759824, -5.837696018585297963 ) ) ;
#84024 = CARTESIAN_POINT ( 'NONE',  ( 151.8414195360447252, 269.4506305376710884, 14.13415052990332121 ) ) ;
#84026 = DIRECTION ( 'NONE',  ( 0.4999999999999998890, -0.8660254037844385966, 0.000000000000000000 ) ) ;
#84027 = EDGE_LOOP ( 'NONE', ( #42684, #30264, #78108, #18834 ) ) ;
#84028 = CARTESIAN_POINT ( 'NONE',  ( 146.9324727656309335, 276.1524872186338371, 3.813717745456558728 ) ) ;
#84029 = CARTESIAN_POINT ( 'NONE',  ( 71.84536423521903714, 63.91743456037271898, 13.36489245195331144 ) ) ;
#84030 = CARTESIAN_POINT ( 'NONE',  ( 189.1629689208399157, 263.9982617371560423, -9.142174876481732326 ) ) ;
#84031 = CARTESIAN_POINT ( 'NONE',  ( 173.3007741876858177, 251.6123024758747420, -0.5682592644679328453 ) ) ;
#84032 = CARTESIAN_POINT ( 'NONE',  ( 192.2191777777270261, 271.1093369735001488, -15.19916813630121410 ) ) ;
#84033 = CARTESIAN_POINT ( 'NONE',  ( 71.70420417316881867, 72.14386137618673445, 3.298165275896878246 ) ) ;
#84034 = CARTESIAN_POINT ( 'NONE',  ( 84.77469373108432649, 46.07232203156790717, 9.879153252899332216 ) ) ;
#84035 = CYLINDRICAL_SURFACE ( 'NONE', #89980, 70.00000000000002842 ) ;
#84036 = CARTESIAN_POINT ( 'NONE',  ( 155.5204415533959548, 261.2776889444089647, 17.19127227448963424 ) ) ;
#84037 = CARTESIAN_POINT ( 'NONE',  ( 191.4150545428761916, 282.8117087430050560, -17.65512190867960740 ) ) ;
#84038 = CARTESIAN_POINT ( 'NONE',  ( 82.49266829201729934, 54.25868459827957935, -15.95543171357395273 ) ) ;
#84039 = AXIS2_PLACEMENT_3D ( 'NONE', #84371, #6342, #76731 ) ;
#84040 = CARTESIAN_POINT ( 'NONE',  ( 79.14634863314516622, 210.3768266524160140, 9.188101187500098632 ) ) ;
#84041 = CARTESIAN_POINT ( 'NONE',  ( 206.4640281786353171, 273.0408085897082060, -10.81921452789957883 ) ) ;
#84042 = CARTESIAN_POINT ( 'NONE',  ( 147.1125781744767949, 275.8405354997948962, -5.216646253929903665 ) ) ;
#84043 = LINE ( 'NONE', #45480, #13970 ) ;
#84044 = EDGE_CURVE ( 'NONE', #35356, #826, #47956, .T. ) ;
#84045 = VECTOR ( 'NONE', #60064, 1000.000000000000114 ) ;
#84046 = AXIS2_PLACEMENT_3D ( 'NONE', #10356, #98948, #36616 ) ;
#84047 = CARTESIAN_POINT ( 'NONE',  ( 161.1061647010182583, 251.6029326557136585, -13.56144933775657613 ) ) ;
#84048 = DIRECTION ( 'NONE',  ( 0.8660254037844382635, 0.5000000000000004441, 0.000000000000000000 ) ) ;
#84050 = CARTESIAN_POINT ( 'NONE',  ( 159.1344352748853055, 279.7114264697810313, -10.00621538743078354 ) ) ;
#84049 = CARTESIAN_POINT ( 'NONE',  ( 73.71089132031853808, 69.41623407880213392, -9.892556164724735979 ) ) ;
#84051 = CARTESIAN_POINT ( 'NONE',  ( 196.2953682204578456, 263.5854184417236752, 0.8810977108677261471 ) ) ;
#84052 = CARTESIAN_POINT ( 'NONE',  ( 42.95298936059631245, 26.92755873383629250, 6.180339887498953466 ) ) ;
#84053 = FACE_OUTER_BOUND ( 'NONE', #71873, .T. ) ;
#84054 = CARTESIAN_POINT ( 'NONE',  ( 82.74911235343154203, 53.93399432278085470, 15.46284286724625368 ) ) ;
#84055 = B_SPLINE_CURVE_WITH_KNOTS ( 'NONE', 3,
 ( #84051, #37878, #61187, #92155 ),
 .UNSPECIFIED., .F., .F.,
 ( 4, 4 ),
 ( 0.01278664256632899843, 0.02134844601914220180 ),
 .UNSPECIFIED. ) ;
#84056 = CARTESIAN_POINT ( 'NONE',  ( 71.70420417316881867, 72.14386137618673445, 3.298165275896887128 ) ) ;
#84057 = VECTOR ( 'NONE', #35453, 1000.000000000000000 ) ;
#84058 = CARTESIAN_POINT ( 'NONE',  ( 35.79112540406921283, 179.2202760586659736, -5.415160957724236172E-17 ) ) ;
#84059 = CARTESIAN_POINT ( 'NONE',  ( 45.15450443884093090, 203.0024278399160949, 9.188101187500095079 ) ) ;
#84060 = CARTESIAN_POINT ( 'NONE',  ( 196.1613785401733878, 290.8855212161054737, 15.98157687694135021 ) ) ;
#84063 = ADVANCED_FACE ( 'NONE', ( #36378 ), #18710, .T. ) ;
#84062 = CARTESIAN_POINT ( 'NONE',  ( 199.4217651877295054, 277.6593044302092039, 15.26469614663150764 ) ) ;
#84061 = B_SPLINE_CURVE_WITH_KNOTS ( 'NONE', 3,
 ( #34342, #18657, #80490, #20645, #51533, #66242, #82495, #11061, #41938, #65237, #19169, #76346, #15007, #91557, #82974, #99141, #75856, #98153, #29241, #36825, #90590, #6920, #29728, #60602, #14032, #67734, #60107, #22126, #6438, #53019, #44421, #14536, #45414, #61107, #37807, #98657, #23106, #91073, #30729, #52519, #59610, #21636, #21155, #75351, #68717, #99641, #92080, #30223, #83467, #53997 ),
 .UNSPECIFIED., .F., .F.,
 ( 4, 2, 2, 2, 2, 2, 2, 2, 2, 2, 2, 2, 2, 2, 2, 2, 2, 2, 2, 2, 2, 2, 2, 2, 4 ),
 ( 0.0007347544931350308631, 0.0009412576793029640626, 0.001147760865470897262, 0.001251012458554859579, 0.001354264051638821896, 0.001560767237806692971, 0.001973773610142371369, 0.002386779982478049334, 0.003212792727149403529, 0.004038805471820757290, 0.004864818216492110617, 0.005277824588827823710, 0.005484327774995722757, 0.005587579368079672280, 0.005639205164621694313, 0.005690830961163716346, 0.005742456757705738379, 0.005794082554247760412, 0.005897334147331918103, 0.006103837333500335832, 0.006310340519668754429, 0.006516843705837173026, 0.006723346892005590755, 0.006929850078174008485, 0.007342856450510823127 ),
 .UNSPECIFIED. ) ;
#84064 = CARTESIAN_POINT ( 'NONE',  ( 78.75692787745495593, 50.96207330215147380, -15.15038416266403587 ) ) ;
#84065 = CARTESIAN_POINT ( 'NONE',  ( 141.2293712190596011, 252.3458772461660260, 9.188101187500095079 ) ) ;
#84066 = CARTESIAN_POINT ( 'NONE',  ( 54.70828104404427705, 193.2048013555409796, 4.594050593750051981 ) ) ;
#84067 = AXIS2_PLACEMENT_3D ( 'NONE', #56856, #71591, #26481 ) ;
#84068 = CARTESIAN_POINT ( 'NONE',  ( 19.41443888993109823, 32.18502408145592142, 5.678558825948276656 ) ) ;
#84069 = CARTESIAN_POINT ( 'NONE',  ( 199.2299651681423143, 285.5705732690366858, -17.65328173313980642 ) ) ;
#84070 = CARTESIAN_POINT ( 'NONE',  ( 196.4808189786114951, 290.3322341467384717, -17.84817245450773271 ) ) ;
#84071 = CARTESIAN_POINT ( 'NONE',  ( 9.185703322462060783, 20.70171378149917629, -9.188101187500004485 ) ) ;
#84072 = CARTESIAN_POINT ( 'NONE',  ( 26.07871176553302917, 38.55466486950701466, 7.012934429366973338E-14 ) ) ;
#84073 = CARTESIAN_POINT ( 'NONE',  ( 77.22649460905380181, 63.31555197798695644, 15.15381191669831651 ) ) ;
#84074 = CARTESIAN_POINT ( 'NONE',  ( 175.7016899852434335, 291.0303512684756697, 2.528121706571572425 ) ) ;
#84075 = CARTESIAN_POINT ( 'NONE',  ( 198.2819808855875863, 287.2125302111982705, 18.53535247371401695 ) ) ;
#84076 = CARTESIAN_POINT ( 'NONE',  ( 182.3130817044836931, 280.8266231767971703, -16.24680219230945966 ) ) ;
#84077 = CARTESIAN_POINT ( 'NONE',  ( 153.3114877943481815, 276.8159031518617326, 7.198048095202238983 ) ) ;
#84078 = ADVANCED_FACE ( 'NONE', ( #72930 ), #97231, .T. ) ;
#84079 = EDGE_CURVE ( 'NONE', #8947, #76337, #50097, .T. ) ;
#84080 = DIRECTION ( 'NONE',  ( -0.000000000000000000, -0.000000000000000000, 1.000000000000000000 ) ) ;
#84081 = CARTESIAN_POINT ( 'NONE',  ( 95.42925689777531773, 219.2365022471902023, -10.00000000000009059 ) ) ;
#84082 = CARTESIAN_POINT ( 'NONE',  ( 200.4775477985258760, 283.4096967665721536, 16.80647240730505487 ) ) ;
#84083 = B_SPLINE_CURVE_WITH_KNOTS ( 'NONE', 3,
 ( #95397, #41113, #73539, #57322 ),
 .UNSPECIFIED., .F., .F.,
 ( 4, 4 ),
 ( 0.009352860264968503035, 0.01452566192536472109 ),
 .UNSPECIFIED. ) ;
#84084 = CARTESIAN_POINT ( 'NONE',  ( 194.3231775528952312, 285.3053704592781514, -17.11556690190039376 ) ) ;
#84085 = ORIENTED_EDGE ( 'NONE', *, *, #36896, .T. ) ;
#84086 = CARTESIAN_POINT ( 'NONE',  ( 61.47358386746269332, 215.4869531367911009, 4.594050593750046652 ) ) ;
#84087 = VERTEX_POINT ( 'NONE', #11616 ) ;
#84088 = CARTESIAN_POINT ( 'NONE',  ( 165.5617726036975625, 265.0396632758227611, 16.58379757636856056 ) ) ;
#84089 = CARTESIAN_POINT ( 'NONE',  ( 190.3453568493779358, 278.9120622883270926, -16.55271846494312626 ) ) ;
#84090 = CARTESIAN_POINT ( 'NONE',  ( 77.38344707992528981, 49.10671604805792612, -15.27628165681131200 ) ) ;
#84091 = ORIENTED_EDGE ( 'NONE', *, *, #48834, .F. ) ;
#84092 = CARTESIAN_POINT ( 'NONE',  ( -71.61465314115659453, 63.06504152958490295, -60.00000000000000000 ) ) ;
#84093 = DIRECTION ( 'NONE',  ( -0.4493970231495795775, 0.7783784768652820540, -0.4383711467890876734 ) ) ;
#84094 = CARTESIAN_POINT ( 'NONE',  ( 148.1974503712686158, 273.9614817352322120, -7.884397846570731616 ) ) ;
#84095 = CARTESIAN_POINT ( 'NONE',  ( 72.71583986753169881, 70.26028652805152319, -8.041570622059433404 ) ) ;
#84096 = CARTESIAN_POINT ( 'NONE',  ( -22.42236680055709641, 157.8615022471902591, 0.000000000000000000 ) ) ;
#84097 = CARTESIAN_POINT ( 'NONE',  ( 204.9604304439480416, 275.6451162603322587, 13.28912526856024279 ) ) ;
#84098 = ORIENTED_EDGE ( 'NONE', *, *, #44935, .T. ) ;
#84099 = CARTESIAN_POINT ( 'NONE',  ( 21.45440292344354916, 18.10170272979926764, -7.433330006724141015 ) ) ;
#84100 = CARTESIAN_POINT ( 'NONE',  ( 70.34088726048339879, 70.18557938879432356, -5.457944947125428214 ) ) ;
#84101 = CARTESIAN_POINT ( 'NONE',  ( 173.7423250686665881, 275.4393285809401846, 17.42598933989775389 ) ) ;
#84102 = ORIENTED_EDGE ( 'NONE', *, *, #22539, .T. ) ;
#84103 = CARTESIAN_POINT ( 'NONE',  ( 202.9899429726835649, 270.3564826351193915, -9.180241878456698146 ) ) ;
#84104 = CARTESIAN_POINT ( 'NONE',  ( 159.2394649670193303, 254.8361514374751664, -16.43133403737800791 ) ) ;
#84105 = B_SPLINE_CURVE_WITH_KNOTS ( 'NONE', 3,
 ( #49341, #42220, #74151, #3262, #88400, #73157, #34627, #34145, #96476, #35122 ),
 .UNSPECIFIED., .F., .F.,
 ( 4, 2, 2, 2, 4 ),
 ( 0.000000000000000000, 0.0002622400424273028919, 0.0005244800848546057838, 0.0007867201272819086214, 0.001048960169709211568 ),
 .UNSPECIFIED. ) ;
#84106 = ORIENTED_EDGE ( 'NONE', *, *, #25046, .T. ) ;
#84107 = ORIENTED_EDGE ( 'NONE', *, *, #8336, .T. ) ;
#84108 = CARTESIAN_POINT ( 'NONE',  ( 173.8526494319628739, 285.7800503636065059, 10.50335656709346033 ) ) ;
#84109 = EDGE_CURVE ( 'NONE', #76921, #81902, #19149, .T. ) ;
#84111 = CARTESIAN_POINT ( 'NONE',  ( 68.32631950292746126, 65.68986423853067436, -10.34564397505435096 ) ) ;
#84110 = CARTESIAN_POINT ( 'NONE',  ( 70.58432976086416488, 62.10851096095700541, 14.48710700881215985 ) ) ;
#84112 = CARTESIAN_POINT ( 'NONE',  ( 163.0424334805279045, 248.2492167524936804, -9.671494865076915914 ) ) ;
#84113 = CARTESIAN_POINT ( 'NONE',  ( 204.4325665793906524, 276.5594032932251594, 13.33817701435311598 ) ) ;
#84114 = CARTESIAN_POINT ( 'NONE',  ( 159.7953104873542145, 253.8733987550956783, 15.41928249285404107 ) ) ;
#84115 = CARTESIAN_POINT ( 'NONE',  ( 164.0826012759681305, 264.7739101429210109, -16.65441687119937342 ) ) ;
#84116 = CARTESIAN_POINT ( 'NONE',  ( 138.1714793337695824, 241.3923013555409796, 4.594050593750050204 ) ) ;
#84117 = CIRCLE ( 'NONE', #79194, 70.00000000000001421 ) ;
#84118 = CARTESIAN_POINT ( 'NONE',  ( 177.6697782944580979, 268.6434933572430737, 17.08943839160881595 ) ) ;
#84119 = CARTESIAN_POINT ( 'NONE',  ( 195.7990362237038369, 290.8591192847630964, -16.03867274897940831 ) ) ;
#84120 = CARTESIAN_POINT ( 'NONE',  ( 79.14634863314516622, 210.3768266524160140, 9.188101187500098632 ) ) ;
#84121 = ORIENTED_EDGE ( 'NONE', *, *, #96190, .F. ) ;
#84122 = CARTESIAN_POINT ( 'NONE',  ( 41.50249547274756878, 124.4848494355456836, 10.00000000000000000 ) ) ;
#84123 = DIRECTION ( 'NONE',  ( 1.000000000000000000, 0.000000000000000000, 0.000000000000000000 ) ) ;
#84124 = ORIENTED_EDGE ( 'NONE', *, *, #28639, .F. ) ;
#84125 = AXIS2_PLACEMENT_3D ( 'NONE', #33569, #42637, #48261 ) ;
#84126 = CARTESIAN_POINT ( 'NONE',  ( -19.65312891409030271, 93.06504152958497400, 59.99999999999999289 ) ) ;
#84127 = VERTEX_POINT ( 'NONE', #35138 ) ;
#84128 = EDGE_LOOP ( 'NONE', ( #50694, #56521, #57393, #36983 ) ) ;
#84129 = FACE_BOUND ( 'NONE', #21049, .T. ) ;
#84130 = CARTESIAN_POINT ( 'NONE',  ( 66.90211989194618525, 67.97973764059037194, 6.975494484356386415 ) ) ;
#84131 = EDGE_CURVE ( 'NONE', #22055, #73884, #8761, .T. ) ;
#84132 = CARTESIAN_POINT ( 'NONE',  ( 197.8158846759225469, 287.0879278553931613, 16.95854422743263967 ) ) ;
#84133 = CARTESIAN_POINT ( 'NONE',  ( 84.06866697891398132, 42.24462045465304527, -5.118976631247559972 ) ) ;
#84134 = CARTESIAN_POINT ( 'NONE',  ( 67.76349224122205328, 65.58094410182457068, 10.12335088330697630 ) ) ;
#84135 = CARTESIAN_POINT ( 'NONE',  ( 154.8989000222956349, 262.3542304552891551, 17.41779271305265908 ) ) ;
#84136 = CARTESIAN_POINT ( 'NONE',  ( 72.65612776400872974, 69.70796105700785006, 8.715673431363931911 ) ) ;
#84137 = ORIENTED_EDGE ( 'NONE', *, *, #70293, .F. ) ;
#84138 = AXIS2_PLACEMENT_3D ( 'NONE', #64580, #56955, #87941 ) ;
#84139 = B_SPLINE_SURFACE_WITH_KNOTS ( 'NONE', 3, 1, ( 
 ( #15990, #785 ),
 ( #8397, #79837 ),
 ( #86455, #31671 ),
 ( #54463, #46890 ),
 ( #71720, #78308 ),
 ( #1301, #79343 ),
 ( #9910, #48901 ),
 ( #62069, #2312 ),
 ( #32185, #62567 ),
 ( #40271, #93531 ),
 ( #94529, #24087 ),
 ( #16979, #94033 ),
 ( #10403, #41273 ),
 ( #54983, #8889 ),
 ( #93017, #64092 ),
 ( #25081, #55962 ),
 ( #95037, #39758 ),
 ( #72215, #24583 ),
 ( #25601, #56487 ),
 ( #55469, #23571 ),
 ( #47871, #86956 ),
 ( #2819, #51376 ),
 ( #11422, #20503 ),
 ( #81828, #35688 ),
 ( #11910, #27103 ),
 ( #12912, #3803 ),
 ( #57475, #56976 ),
 ( #88969, #49392 ),
 ( #33709, #57988 ),
 ( #80338, #26102 ),
 ( #10906, #43270 ),
 ( #73698, #66588 ),
 ( #95556, #34199 ),
 ( #72728, #64601 ) ),
 .UNSPECIFIED., .T., .F., .F.,
 ( 4, 2, 2, 2, 2, 2, 2, 2, 2, 2, 2, 2, 2, 2, 2, 2, 4 ),
 ( 2, 2 ),
 ( 0.000000000000000000, 0.06250000000000000000, 0.1250000000000000000, 0.1875000000000000000, 0.2500000000000000000, 0.3125000000000000000, 0.3750000000000000000, 0.4375000000000000000, 0.5000000000000000000, 0.5625000000000000000, 0.6250000000000000000, 0.6875000000000000000, 0.7500000000000000000, 0.8125000000000000000, 0.8750000000000000000, 0.9375000000000000000, 1.000000000000000000 ),
 ( 0.000000000000000000, 1.000000000000000000 ),
 .UNSPECIFIED. ) ;
#84140 = CARTESIAN_POINT ( 'NONE',  ( -34.16292631813981728, 25.86630820016799248, -10.00000000000000000 ) ) ;
#84141 = ORIENTED_EDGE ( 'NONE', *, *, #44819, .F. ) ;
#84142 = CARTESIAN_POINT ( 'NONE',  ( 76.21282038944568171, 51.57770476861935549, -15.67853476563008819 ) ) ;
#84143 = CARTESIAN_POINT ( 'NONE',  ( 183.9506971135539004, 275.2367033331265702, 16.38750030320872852 ) ) ;
#84144 = EDGE_CURVE ( 'NONE', #20145, #38493, #41739, .T. ) ;
#84145 = VECTOR ( 'NONE', #55570, 1000.000000000000000 ) ;
#84146 = CARTESIAN_POINT ( 'NONE',  ( 195.5051761698225619, 279.3379179581851304, 16.32977475709600768 ) ) ;
#84147 = LINE ( 'NONE', #15170, #33490 ) ;
#84148 = CARTESIAN_POINT ( 'NONE',  ( 130.0249940097159254, 252.0024278399160949, -9.188101187500093303 ) ) ;
#84149 = ORIENTED_EDGE ( 'NONE', *, *, #6143, .T. ) ;
#84150 = CARTESIAN_POINT ( 'NONE',  ( 88.22000632671873177, 44.27423112938744509, 4.003506518527982116 ) ) ;
#84151 = CARTESIAN_POINT ( 'NONE',  ( 182.0908725605739278, 257.5538491103775414, 6.656128696890800889 ) ) ;
#84152 = CARTESIAN_POINT ( 'NONE',  ( -19.65312891409030271, 9.999999999999994671, -54.99999999999999289 ) ) ;
#84153 = CARTESIAN_POINT ( 'NONE',  ( 153.4613150239306094, 264.8442007126561748, -16.86932470306368259 ) ) ;
#84154 = CARTESIAN_POINT ( 'NONE',  ( 79.21773931386873357, 59.07529007650229147, -16.22247798074718617 ) ) ;
#84155 = CARTESIAN_POINT ( 'NONE',  ( 70.07046733978542363, 67.38152690267425271, -9.666843875404030229 ) ) ;
#84156 = ORIENTED_EDGE ( 'NONE', *, *, #23307, .T. ) ;
#84157 = CARTESIAN_POINT ( 'NONE',  ( 199.3492571032118974, 266.8521786015153907, 4.572492606930079084 ) ) ;
#84158 = CARTESIAN_POINT ( 'NONE',  ( 148.3881289992426105, 276.3505094388546581, -3.863952534650588522 ) ) ;
#84159 = CARTESIAN_POINT ( 'NONE',  ( 87.08779078562172060, 43.05500592647786107, 0.7967578903178703653 ) ) ;
#84160 = CARTESIAN_POINT ( 'NONE',  ( 80.71714504946366731, 50.25349500424252369, 14.48686000064734358 ) ) ;
#84161 = CARTESIAN_POINT ( 'NONE',  ( 198.5847843579792311, 266.2858474173958143, 0.8381617387219465476 ) ) ;
#84162 = CARTESIAN_POINT ( 'NONE',  ( 198.9327437650594845, 265.4802594572302041, 0.07579901079707679346 ) ) ;
#84163 = ORIENTED_EDGE ( 'NONE', *, *, #17547, .F. ) ;
#84164 = CARTESIAN_POINT ( 'NONE',  ( -19.65312891409030271, 93.06504152958497400, 177.5919119679930134 ) ) ;
#84165 = CARTESIAN_POINT ( 'NONE',  ( 186.8895883408185910, 282.0686240457306440, 16.84332228780022689 ) ) ;
#84166 = CARTESIAN_POINT ( 'NONE',  ( 164.9335952247126045, 244.9736285262353306, -1.661461410667423255 ) ) ;
#84168 = CARTESIAN_POINT ( 'NONE',  ( 196.8833167150979477, 269.7409658301617128, 12.25108723014616352 ) ) ;
#84167 = CARTESIAN_POINT ( 'NONE',  ( 177.3308938375265598, 264.6334632213029181, -15.29145188940869282 ) ) ;
#84169 = CARTESIAN_POINT ( 'NONE',  ( 21.11941962201201051, 24.14441083166261137, 10.00000000000000533 ) ) ;
#84170 = CARTESIAN_POINT ( 'NONE',  ( -13.42108286626701030, 23.34301056334150104, 177.5919119679930134 ) ) ;
#84171 = CARTESIAN_POINT ( 'NONE',  ( 166.5995791397127448, 286.3618139744101541, -3.233326376697027715 ) ) ;
#84172 = CARTESIAN_POINT ( 'NONE',  ( 19.40821860046903069, 26.90829794293880539, 10.00000000000000355 ) ) ;
#84173 = CARTESIAN_POINT ( 'NONE',  ( 159.5573297132660002, 254.2855935470410031, 16.91607698584599007 ) ) ;
#84174 = CARTESIAN_POINT ( 'NONE',  ( 145.9293632524074553, 248.3927522451417929, -10.00000000000009059 ) ) ;
#84175 = DIRECTION ( 'NONE',  ( 0.9819794923402651587, -0.1889875038809575580, 0.000000000000000000 ) ) ;
#84176 = ORIENTED_EDGE ( 'NONE', *, *, #32666, .T. ) ;
#84177 = AXIS2_PLACEMENT_3D ( 'NONE', #54020, #341, #15522 ) ;
#84178 = CARTESIAN_POINT ( 'NONE',  ( 66.78940807508750765, 67.55366617704474663, -6.509619371764820528 ) ) ;
#84179 = CARTESIAN_POINT ( 'NONE',  ( 72.69528318058601712, 70.26191488565096677, -8.019772805389131065 ) ) ;
#84180 = CARTESIAN_POINT ( 'NONE',  ( 179.3071757824324095, 289.7729440391376556, 11.79011794106743949 ) ) ;
#84181 = CARTESIAN_POINT ( 'NONE',  ( 11.32556065139379875, 177.3458772461660544, 9.188101187500095079 ) ) ;
#84182 = CARTESIAN_POINT ( 'NONE',  ( 181.8071258313758278, 275.6022297491251720, -16.43063624076323137 ) ) ;
#84183 = CARTESIAN_POINT ( 'NONE',  ( 21.76190656055422323, 36.65659080271452552, -1.878358725466461243E-16 ) ) ;
#84184 = CARTESIAN_POINT ( 'NONE',  ( 82.86315813168180000, 41.72223458103137261, -3.985406787420944674 ) ) ;
#84185 = CARTESIAN_POINT ( 'NONE',  ( 170.1804300311658551, 270.7854574292069287, -17.38281393466202829 ) ) ;
#84186 = CARTESIAN_POINT ( 'NONE',  ( 71.65684213956077997, 72.06054752937143348, -3.528960205221522095 ) ) ;
#84187 = DIRECTION ( 'NONE',  ( -0.5000000000000013323, 0.8660254037844378194, 0.000000000000000000 ) ) ;
#84188 = CARTESIAN_POINT ( 'NONE',  ( 175.5081009096628577, 253.5491181420100304, -3.811933576842129856 ) ) ;
#84189 = CARTESIAN_POINT ( 'NONE',  ( 190.6671659678193862, 261.9269538368635608, -0.7676713603561022836 ) ) ;
#84190 = EDGE_CURVE ( 'NONE', #25608, #32094, #19245, .T. ) ;
#84191 = EDGE_CURVE ( 'NONE', #32399, #36317, #63179, .T. ) ;
#84192 = AXIS2_PLACEMENT_3D ( 'NONE', #22803, #53682, #92732 ) ;
#84193 = CARTESIAN_POINT ( 'NONE',  ( 56.31377616017810084, 209.9865022471902876, -10.00000000000009415 ) ) ;
#84194 = DIRECTION ( 'NONE',  ( -0.8660254037844387076, -0.4999999999999998890, -0.000000000000000000 ) ) ;
#84195 = CARTESIAN_POINT ( 'NONE',  ( 148.2159754900428936, 273.9293952882992471, 9.267836332806297150 ) ) ;
#84196 = ADVANCED_FACE ( 'NONE', ( #3762 ), #71676, .T. ) ;
#84197 = CARTESIAN_POINT ( 'NONE',  ( 18.33521408509785644, 172.2048013555409796, 4.594050593750051981 ) ) ;
#84198 = CARTESIAN_POINT ( 'NONE',  ( 70.94848769240661568, 70.27665202542853251, -7.050353750945653530 ) ) ;
#84199 = EDGE_CURVE ( 'NONE', #26545, #17251, #96997, .T. ) ;
#84200 = CARTESIAN_POINT ( 'NONE',  ( 27.96887745124769253, 39.08080186712594895, -3.090169943749475845 ) ) ;
#84201 = CARTESIAN_POINT ( 'NONE',  ( 37.50955192761952617, 39.84336893147759184, -7.433330006724137462 ) ) ;
#84202 = DIRECTION ( 'NONE',  ( -0.000000000000000000, -0.000000000000000000, -1.000000000000000000 ) ) ;
#84203 = CARTESIAN_POINT ( 'NONE',  ( 207.1059763530604698, 271.9289217357780899, 6.370907250589925575 ) ) ;
#84204 = CARTESIAN_POINT ( 'NONE',  ( 81.79317580962712952, 59.05438242866674159, 0.4890738003669033995 ) ) ;
#84205 = CARTESIAN_POINT ( 'NONE',  ( 162.8927609601937263, 281.1658276129857086, -10.34727072843073614 ) ) ;
#84206 = CARTESIAN_POINT ( 'NONE',  ( 179.9016459768426728, 262.6902523525472475, -14.18888862508328685 ) ) ;
#84207 = CARTESIAN_POINT ( 'NONE',  ( 22.66683848874176022, 18.80170272979926693, 7.433330006724137462 ) ) ;
#84208 = CARTESIAN_POINT ( 'NONE',  ( 12.53574365251956912, 15.43677371833799938, -10.00000000000000355 ) ) ;
#84209 = CARTESIAN_POINT ( 'NONE',  ( 71.52294418693975331, 59.11029950019791812, 15.81128158456864341 ) ) ;
#84210 = CARTESIAN_POINT ( 'NONE',  ( 155.0303156110108489, 262.1266119787277944, 17.11986653161320859 ) ) ;
#84211 = ORIENTED_EDGE ( 'NONE', *, *, #50727, .F. ) ;
#84212 = CARTESIAN_POINT ( 'NONE',  ( 87.53583079710631409, 45.45925790797146249, -6.823327534849023657 ) ) ;
#84213 = CARTESIAN_POINT ( 'NONE',  ( 82.57543265243437247, 45.76368055541952629, -11.49294040874591438 ) ) ;
#84214 = CARTESIAN_POINT ( 'NONE',  ( 81.21214610088644292, 42.40786911149225347, 7.597942034095414243 ) ) ;
#84215 = CARTESIAN_POINT ( 'NONE',  ( 80.74781574657598071, 57.21644485803223290, 16.56566952311892749 ) ) ;
#84216 = VERTEX_POINT ( 'NONE', #65543 ) ;
#84217 = LINE ( 'NONE', #14270, #29592 ) ;
#84218 = CARTESIAN_POINT ( 'NONE',  ( 70.55924477032505138, 71.08919147220014167, -2.935579350952730593 ) ) ;
#84219 = CARTESIAN_POINT ( 'NONE',  ( 77.07146940206541785, 63.73911480020577613, 14.98531907972277644 ) ) ;
#84220 = CARTESIAN_POINT ( 'NONE',  ( 203.5555343017997529, 278.0784677578903370, -15.71723084798551362 ) ) ;
#84221 = B_SPLINE_CURVE_WITH_KNOTS ( 'NONE', 3,
 ( #52651, #30364, #92697, #66496, #54136, #66000, #29864, #14669, #27518, #84601, #30865, #46037, #60735, #14172, #21762, #27991 ),
 .UNSPECIFIED., .F., .F.,
 ( 4, 2, 2, 2, 2, 2, 2, 4 ),
 ( 0.0007292608245178773888, 0.001016117201828066604, 0.001302973579138255820, 0.001589829956448444818, 0.001876686333758634034, 0.002163542711068823250, 0.002450399088379012248, 0.003024111842999491727 ),
 .UNSPECIFIED. ) ;
#84222 = ORIENTED_EDGE ( 'NONE', *, *, #67059, .T. ) ;
#84223 = ORIENTED_EDGE ( 'NONE', *, *, #54135, .T. ) ;
#84225 = CARTESIAN_POINT ( 'NONE',  ( 204.2799274532736433, 276.8237820148827950, 13.55359442435934803 ) ) ;
#84224 = DIRECTION ( 'NONE',  ( 0.000000000000000000, 0.000000000000000000, 1.000000000000000000 ) ) ;
#84226 = ORIENTED_EDGE ( 'NONE', *, *, #5582, .T. ) ;
#84227 = CARTESIAN_POINT ( 'NONE',  ( 153.0927037754837556, 265.4826541232073964, -16.15085267704102634 ) ) ;
#84228 = FACE_OUTER_BOUND ( 'NONE', #55509, .T. ) ;
#84229 = CARTESIAN_POINT ( 'NONE',  ( 80.25249281668115486, 57.81819139295711807, 16.60223264289303557 ) ) ;
#84230 = CARTESIAN_POINT ( 'NONE',  ( 49.72837464868604940, 199.5177522451418781, -10.00000000000009592 ) ) ;
#84231 = ORIENTED_EDGE ( 'NONE', *, *, #9958, .F. ) ;
#84232 = CARTESIAN_POINT ( 'NONE',  ( 190.5969391768923913, 300.5234129089444650, -0.7564693504096553500 ) ) ;
#84233 = VERTEX_POINT ( 'NONE', #2267 ) ;
#84234 = CARTESIAN_POINT ( 'NONE',  ( 205.9642072045669465, 273.9065239114831911, 10.22128930895731536 ) ) ;
#84235 = CARTESIAN_POINT ( 'NONE',  ( 158.1669649540034186, 265.2021071281276363, 17.58525919077285593 ) ) ;
#84236 = VERTEX_POINT ( 'NONE', #11383 ) ;
#84237 = CARTESIAN_POINT ( 'NONE',  ( 190.8138402884741254, 300.1477291634665789, 4.037153726988762514 ) ) ;
#84238 = CARTESIAN_POINT ( 'NONE',  ( 189.5599828453989346, 263.0657735508838186, -9.804501003715218488 ) ) ;
#84239 = ORIENTED_EDGE ( 'NONE', *, *, #86010, .T. ) ;
#84240 = CARTESIAN_POINT ( 'NONE',  ( -18.15312891409030627, 78.77562236714182120, 13.81405534229504894 ) ) ;
#84241 = CARTESIAN_POINT ( 'NONE',  ( -19.65312891409030271, 93.06504152958497400, 60.00000000000000000 ) ) ;
#84242 = CARTESIAN_POINT ( 'NONE',  ( 78.43441866794225348, 47.91884018220574148, -14.51553613075758342 ) ) ;
#84243 = LINE ( 'NONE', #75610, #65729 ) ;
#84244 = ORIENTED_EDGE ( 'NONE', *, *, #91412, .F. ) ;
#84245 = ORIENTED_EDGE ( 'NONE', *, *, #6405, .F. ) ;
#84246 =( BOUNDED_CURVE ( )  B_SPLINE_CURVE ( 2, ( #82796, #13362, #22437, #53330, #68533, #97962, #29060, #76641, #82305 ),
 .UNSPECIFIED., .F., .T. ) 
 B_SPLINE_CURVE_WITH_KNOTS ( ( 3, 2, 2, 2, 3 ),
 ( 0.1008064516129032334, 0.1021505376344086086, 0.1048387096774193589, 0.1075268817204301092, 0.1088709677419354843 ),
 .UNSPECIFIED. ) 
 CURVE ( )  GEOMETRIC_REPRESENTATION_ITEM ( )  RATIONAL_B_SPLINE_CURVE ( ( 0.9330127018922192983, 0.9330127018922196314, 1.000000000000000000, 0.8660254037844387076, 1.000000000000000000, 0.8660254037844387076, 1.000000000000000000, 0.9330127018922194093, 0.9330127018922194093 ) ) 
 REPRESENTATION_ITEM ( '' )  );
#84247 = CARTESIAN_POINT ( 'NONE',  ( 73.29569962742016287, 69.82617127822150849, 9.116539184905871451 ) ) ;
#84248 = CARTESIAN_POINT ( 'NONE',  ( 146.8058449195592061, 276.3718130816831149, 4.181814292810413392 ) ) ;
#84249 = CARTESIAN_POINT ( 'NONE',  ( 82.29966782571446515, 53.62663270485408873, 15.81823675489985348 ) ) ;
#84250 = CARTESIAN_POINT ( 'NONE',  ( 149.7128599965862463, 271.3367152699035501, 12.33532264622322394 ) ) ;
#84251 = DIRECTION ( 'NONE',  ( -0.2639761180675095353, 0.9645292162967424865, 0.000000000000000000 ) ) ;
#84252 = CARTESIAN_POINT ( 'NONE',  ( 191.8453175503442196, 298.3611581390557035, 9.038225159363836525 ) ) ;
#84253 = CARTESIAN_POINT ( 'NONE',  ( 191.5324528500417216, 298.9030556958743432, -8.286652526617016790 ) ) ;
#84254 = CARTESIAN_POINT ( 'NONE',  ( 190.0274641710971082, 301.5097725526222803, 3.738976720635653450 ) ) ;
#84255 = EDGE_CURVE ( 'NONE', #8972, #66666, #41231, .T. ) ;
#84256 = CARTESIAN_POINT ( 'NONE',  ( 71.55865654871253412, 70.58727594908697256, 6.225150381871440430 ) ) ;
#84257 = CARTESIAN_POINT ( 'NONE',  ( 79.83401254395657531, 57.87045807247318407, 16.26439772172797404 ) ) ;
#84258 = CARTESIAN_POINT ( 'NONE',  ( 67.16256804578090112, 66.80979783321159005, 8.146902435796073760 ) ) ;
#84259 = CARTESIAN_POINT ( 'NONE',  ( 167.5421813246326792, 287.5986610761024167, 3.969292590682533373 ) ) ;
#84260 = CARTESIAN_POINT ( 'NONE',  ( 78.00127999931594047, 47.84930604673201060, 14.05929021715905414 ) ) ;
#84261 = VERTEX_POINT ( 'NONE', #18465 ) ;
#84262 = CARTESIAN_POINT ( 'NONE',  ( 190.8204521987322835, 300.1362769989643198, -4.254506460977580673 ) ) ;
#84263 = CARTESIAN_POINT ( 'NONE',  ( 71.60104883639283457, 68.65505837569367031, 9.270974577602569155 ) ) ;
#84264 = CARTESIAN_POINT ( 'NONE',  ( 148.8636819117637629, 274.0699646975406836, 8.926834414297511344 ) ) ;
#84265 = CARTESIAN_POINT ( 'NONE',  ( 79.50366146091808162, 45.80427587621628760, 12.91999808083510004 ) ) ;
#84266 = CARTESIAN_POINT ( 'NONE',  ( 179.7520283141993787, 283.0547433888561386, -15.89619356914058201 ) ) ;
#84267 = CARTESIAN_POINT ( 'NONE',  ( 189.9181943850632308, 301.6990333737651326, -1.201434020889846632 ) ) ;
#84268 = VECTOR ( 'NONE', #67094, 1000.000000000000000 ) ;
#84269 = CARTESIAN_POINT ( 'NONE',  ( 168.7885031894148256, 286.1153816027461403, -7.680432405603670354 ) ) ;
#84270 = ORIENTED_EDGE ( 'NONE', *, *, #44370, .F. ) ;
#84271 = CARTESIAN_POINT ( 'NONE',  ( 163.4084407101100851, 247.6152736349200438, -10.68829614238923931 ) ) ;
#84272 = CYLINDRICAL_SURFACE ( 'NONE', #27389, 17.82106496071139645 ) ;
#84274 = EDGE_CURVE ( 'NONE', #1103, #95115, #79304, .T. ) ;
#84273 = CARTESIAN_POINT ( 'NONE',  ( 72.44040225518423881, 71.75621485965102408, 5.770394931239954950 ) ) ;
#84275 = CARTESIAN_POINT ( 'NONE',  ( 39.40823858692142778, 206.8927522451419350, 2.944929066748280225E-16 ) ) ;
#84276 = CARTESIAN_POINT ( 'NONE',  ( 117.5758788303146076, 244.8149278399160949, 9.188101187500093303 ) ) ;
#84277 = CARTESIAN_POINT ( 'NONE',  ( 180.6753976046032051, 294.2641805748295951, -3.313934977364610734 ) ) ;
#84278 = CARTESIAN_POINT ( 'NONE',  ( -13.11024591527734451, 6.000000000000000000, 45.00000000000000000 ) ) ;
#84279 = CARTESIAN_POINT ( 'NONE',  ( 157.5042325173297684, 257.8416622032797818, 16.70595240278738203 ) ) ;
#84280 = CARTESIAN_POINT ( 'NONE',  ( 172.2717404889760928, 250.6514006074399674, -4.087445548495970193 ) ) ;
#84281 = CARTESIAN_POINT ( 'NONE',  ( 24.66750420662404508, 194.2369531367911293, -4.594050593750048428 ) ) ;
#84282 = CARTESIAN_POINT ( 'NONE',  ( 82.21410988452117863, 40.73976263626466476, 3.762362152834606732 ) ) ;
#84283 = B_SPLINE_CURVE_WITH_KNOTS ( 'NONE', 3,
 ( #40530, #40023, #1052, #32449, #23331, #71465, #57726, #10657, #10157, #95310, #42038, #2565, #4538, #87225, #11171, #25865, #33449, #79593, #41023, #64345, #96791, #41533, #26851, #19761, #97274, #81096, #80090, #34930, #56741, #17759, #27351, #49636, #57231, #71961, #88706, #3564, #87723, #64855, #19276, #18259, #50629, #72973, #88207 ),
 .UNSPECIFIED., .F., .F.,
 ( 4, 2, 2, 2, 2, 2, 1, 2, 2, 2, 2, 2, 2, 2, 2, 2, 2, 2, 2, 2, 2, 4 ),
 ( 0.000000000000000000, 0.001338277739954425337, 0.002007416609931637896, 0.002676555479908850673, 0.004014833219863313957, 0.004683972089840546249, 0.005353110959817779409, 0.006022249829795012568, 0.006691388699772244861, 0.008029666439726690363, 0.008698805309703908778, 0.009367944179681128927, 0.01070622191963556749, 0.01204449965959000259, 0.01271363852956721753, 0.01338277739954443248, 0.01472105513949887971, 0.01605933287945332175, 0.01739761061940776551, 0.01873588835936220928, 0.02007416609931665652, 0.02141244383927110029 ),
 .UNSPECIFIED. ) ;
#84284 = ORIENTED_EDGE ( 'NONE', *, *, #36694, .T. ) ;
#84285 = CARTESIAN_POINT ( 'NONE',  ( 191.3698991030772731, 298.7983559512333613, 7.726696955929065247 ) ) ;
#84286 = CARTESIAN_POINT ( 'NONE',  ( 181.3932036981916269, 267.7384658855342536, 14.96073790625240996 ) ) ;
#84287 = CARTESIAN_POINT ( 'NONE',  ( 23.64814127513154673, 118.0650415295851019, -45.00000000000000711 ) ) ;
#84288 = CARTESIAN_POINT ( 'NONE',  ( 147.3023124603499809, 275.5119060767245287, 5.196938859334171212 ) ) ;
#84289 = DIRECTION ( 'NONE',  ( -1.000000000000000000, -1.804112415015878589E-15, 0.000000000000000000 ) ) ;
#84290 = LINE ( 'NONE', #14836, #68911 ) ;
#84291 = CARTESIAN_POINT ( 'NONE',  ( 68.47880282939688357, 64.40332810061045166, -12.27537564787820479 ) ) ;
#84292 = CARTESIAN_POINT ( 'NONE',  ( 106.8138825148102740, 239.1427522451419065, -10.00000000000009415 ) ) ;
#84293 = DIRECTION ( 'NONE',  ( 1.000000000000000000, -1.687142489207157240E-13, 0.000000000000000000 ) ) ;
#84294 = EDGE_LOOP ( 'NONE', ( #88230, #57207, #61116, #12461 ) ) ;
#84295 = B_SPLINE_CURVE_WITH_KNOTS ( 'NONE', 3,
 ( #28388, #50201, #27414, #74018, #75014, #4603, #35495, #51711, #97326, #69755, #46961, #24163, #55048, #8464 ),
 .UNSPECIFIED., .F., .F.,
 ( 4, 2, 2, 2, 2, 2, 4 ),
 ( 3.469446951953614189E-18, 0.0004440166800142984912, 0.0008880333600285935129, 0.001110041700035716223, 0.001332050040042838824, 0.001554058380049961642, 0.001776066720057084243 ),
 .UNSPECIFIED. ) ;
#84296 = CARTESIAN_POINT ( 'NONE',  ( 158.2918428669640605, 281.5729122900692118, -1.602796375854172339 ) ) ;
#84297 = DIRECTION ( 'NONE',  ( -0.8660254037844387076, -0.4999999999999998890, -0.000000000000000000 ) ) ;
#84298 = CARTESIAN_POINT ( 'NONE',  ( 7.753205860782987457, 175.2833772461660544, -9.188101187500095079 ) ) ;
#84299 = CARTESIAN_POINT ( 'NONE',  ( 11.51180284259942610, 11.81029122506292595, 8.090169943749479842 ) ) ;
#84300 = CARTESIAN_POINT ( 'NONE',  ( -16.32499242613253543, 105.7308263295076216, 44.25048734575928222 ) ) ;
#84301 = CARTESIAN_POINT ( 'NONE',  ( 192.5076277540105423, 297.2140032159341558, -13.10094381206144298 ) ) ;
#84302 = LINE ( 'NONE', #92397, #18418 ) ;
#84304 = CARTESIAN_POINT ( 'NONE',  ( 65.45180129215621889, 220.8464784336661637, 1.353441290958777327E-15 ) ) ;
#84303 = CARTESIAN_POINT ( 'NONE',  ( 174.3777206541172404, 286.9002377562176207, 10.20102932312108557 ) ) ;
#84305 = CARTESIAN_POINT ( 'NONE',  ( 200.4775477985258760, 283.4096967665721536, 16.80647240730505487 ) ) ;
#84306 = CARTESIAN_POINT ( 'NONE',  ( 72.64662832737921860, 57.19814123590507648, 15.87563656662714351 ) ) ;
#84307 = CARTESIAN_POINT ( 'NONE',  ( 47.92415505746842541, 205.1427522451419065, 10.00000000000009415 ) ) ;
#84308 = CARTESIAN_POINT ( 'NONE',  ( 66.33628465374795269, 68.06039941485154543, -4.733060476579643350 ) ) ;
#84309 = EDGE_LOOP ( 'NONE', ( #35586, #97910, #6322, #57115 ) ) ;
#84310 = CARTESIAN_POINT ( 'NONE',  ( 162.5320791996320224, 267.5315774354641576, 16.48036321604684673 ) ) ;
#84311 = CARTESIAN_POINT ( 'NONE',  ( 10.91961124514375925, 187.1115022471903160, -5.000000000000047962 ) ) ;
#84312 = CARTESIAN_POINT ( 'NONE',  ( 164.1146561143383167, 246.3920726737087534, -7.362905700427413436 ) ) ;
#84313 = CARTESIAN_POINT ( 'NONE',  ( 128.2929432021470859, 251.0024278399160949, 9.188101187500095079 ) ) ;
#84314 = CARTESIAN_POINT ( 'NONE',  ( 32.24243340009443415, 30.56628583063843152, 9.188101187500006262 ) ) ;
#84315 = CARTESIAN_POINT ( 'NONE',  ( 164.7063722853443437, 260.9203034178046323, -16.15040340005176844 ) ) ;
#84316 = EDGE_CURVE ( 'NONE', #87203, #8463, #73172, .T. ) ;
#84317 = LINE ( 'NONE', #67071, #16049 ) ;
#84318 = CARTESIAN_POINT ( 'NONE',  ( -78.57153713424665398, 57.64153020465174393, -10.00000000000000000 ) ) ;
#84320 = CARTESIAN_POINT ( 'NONE',  ( 172.2313928256145630, 289.6871463590026679, -5.851927625370571207 ) ) ;
#84319 = CARTESIAN_POINT ( 'NONE',  ( 88.48118267945454818, 44.00993189541001982, 2.076335272536713905 ) ) ;
#84321 = CARTESIAN_POINT ( 'NONE',  ( 68.93235832526967499, 64.11431000937152191, 12.06237109868430579 ) ) ;
#84322 = ORIENTED_EDGE ( 'NONE', *, *, #23322, .T. ) ;
#84323 = CARTESIAN_POINT ( 'NONE',  ( -19.65312891409030271, 93.06504152958497400, -10.00000000000000888 ) ) ;
#84324 =( NAMED_UNIT ( * ) PLANE_ANGLE_UNIT ( ) SI_UNIT ( $, .RADIAN. ) );
#84325 = CARTESIAN_POINT ( 'NONE',  ( -19.73679784724330588, 93.17955462170891678, 59.99999999999999289 ) ) ;
#84326 = CARTESIAN_POINT ( 'NONE',  ( 156.0554005950856151, 280.4150375230931331, -5.525834068163355539 ) ) ;
#84327 = CARTESIAN_POINT ( 'NONE',  ( 12.88253908977640094, 9.298606405272902720, -2.839279412974138328 ) ) ;
#84328 = ORIENTED_EDGE ( 'NONE', *, *, #85239, .F. ) ;
#84329 = CARTESIAN_POINT ( 'NONE',  ( 206.6259318078842284, 272.7603832779192885, 8.129480779612674013 ) ) ;
#84330 = CARTESIAN_POINT ( 'NONE',  ( 167.9430779612994797, 282.0224708860221767, -12.05993733932491452 ) ) ;
#84331 = CARTESIAN_POINT ( 'NONE',  ( -22.42236680055709641, 157.8615022471902591, 0.000000000000000000 ) ) ;
#84332 = DIRECTION ( 'NONE',  ( 0.4999999999999998890, -0.8660254037844385966, 0.000000000000000000 ) ) ;
#84333 = DIRECTION ( 'NONE',  ( -0.9972444261165168689, 0.07418594597050684469, 0.000000000000000000 ) ) ;
#84334 = CARTESIAN_POINT ( 'NONE',  ( 66.66342508697567837, 67.67433879810248243, 6.129251300726011209 ) ) ;
#84335 = CIRCLE ( 'NONE', #14793, 15.50000000000000000 ) ;
#84336 = CARTESIAN_POINT ( 'NONE',  ( 152.7375212135632125, 266.0978483664162582, -16.47968945089317572 ) ) ;
#84337 = B_SPLINE_CURVE_WITH_KNOTS ( 'NONE', 3,
 ( #1960, #72883, #32846, #26261 ),
 .UNSPECIFIED., .F., .F.,
 ( 4, 4 ),
 ( 0.03823235658919261343, 0.04678228248050523425 ),
 .UNSPECIFIED. ) ;
#84338 = DIRECTION ( 'NONE',  ( -1.000000000000000000, 0.000000000000000000, 0.000000000000000000 ) ) ;
#84339 = DIRECTION ( 'NONE',  ( -0.7467472232290864875, 0.000000000000000000, -0.6651079495838618794 ) ) ;
#84340 = EDGE_LOOP ( 'NONE', ( #9167, #91596, #66030, #16893 ) ) ;
#84341 = CARTESIAN_POINT ( 'NONE',  ( 190.6023073677431512, 300.5141149296460981, 3.174888932019753973 ) ) ;
#84342 = CARTESIAN_POINT ( 'NONE',  ( 199.0230529003142692, 272.6643487552923375, 13.78389951960891047 ) ) ;
#84343 = CARTESIAN_POINT ( 'NONE',  ( 189.5301620294561360, 297.3496777562929196, 8.148958219677171044 ) ) ;
#84344 = EDGE_LOOP ( 'NONE', ( #64271, #22245, #96841, #23384 ) ) ;
#84345 = CARTESIAN_POINT ( 'NONE',  ( 191.0862225170008628, 299.6759493045793192, -9.402218231374108726 ) ) ;
#84346 = CARTESIAN_POINT ( 'NONE',  ( 79.22574914704956939, 60.04803162267381111, -16.48148452078547521 ) ) ;
#84347 = CARTESIAN_POINT ( 'NONE',  ( 196.8104339078508076, 289.7613243423628546, -16.40335862274955403 ) ) ;
#84348 = CARTESIAN_POINT ( 'NONE',  ( 70.00411547750407237, 62.73190158012358353, 13.40270835498630575 ) ) ;
#84349 = ORIENTED_EDGE ( 'NONE', *, *, #85808, .T. ) ;
#84350 = CARTESIAN_POINT ( 'NONE',  ( 100.7694865641816051, 238.1744531367911293, 4.594050593750047540 ) ) ;
#84351 = CARTESIAN_POINT ( 'NONE',  ( 161.2313178023453588, 251.3861611254901618, 13.12937145726518473 ) ) ;
#84352 = CARTESIAN_POINT ( 'NONE',  ( 181.1985647863735664, 271.1040133950066888, -15.97949505363916956 ) ) ;
#84353 = ORIENTED_EDGE ( 'NONE', *, *, #61885, .T. ) ;
#84354 = B_SPLINE_CURVE_WITH_KNOTS ( 'NONE', 3,
 ( #27850, #34940, #12161, #51137 ),
 .UNSPECIFIED., .F., .F.,
 ( 4, 4 ),
 ( 0.01377033617237334931, 0.02241479314274836751 ),
 .UNSPECIFIED. ) ;
#84355 = ORIENTED_EDGE ( 'NONE', *, *, #33767, .F. ) ;
#84356 = ORIENTED_EDGE ( 'NONE', *, *, #11993, .F. ) ;
#84357 = CARTESIAN_POINT ( 'NONE',  ( 138.1418008908465822, 79.75620593067000641, -17.47570218321535052 ) ) ;
#84358 = EDGE_LOOP ( 'NONE', ( #32883, #92190, #57767, #95694 ) ) ;
#84359 = CARTESIAN_POINT ( 'NONE',  ( -17.42236680055705023, 149.2012482093457777, 0.000000000000000000 ) ) ;
#84360 = VERTEX_POINT ( 'NONE', #79797 ) ;
#84361 = CARTESIAN_POINT ( 'NONE',  ( 207.8060684685902686, 270.7163266217015689, 2.015725026008670540 ) ) ;
#84362 = CARTESIAN_POINT ( 'NONE',  ( 82.41087058299665102, 41.30607584110375541, 3.329617797228953346 ) ) ;
#84363 = CARTESIAN_POINT ( 'NONE',  ( 165.2793717279795942, 271.1751283101625063, 17.08238418428851091 ) ) ;
#84365 = DIRECTION ( 'NONE',  ( -0.8325133752583718794, 0.5540049458406605121, 0.000000000000000000 ) ) ;
#84364 = B_SPLINE_CURVE_WITH_KNOTS ( 'NONE', 3,
 ( #4242, #73175, #65547, #72687 ),
 .UNSPECIFIED., .F., .F.,
 ( 4, 4 ),
 ( 0.009023986987182482794, 0.01512749127632531665 ),
 .UNSPECIFIED. ) ;
#84366 = CARTESIAN_POINT ( 'NONE',  ( 19.16720650933548953, 170.3262482093457777, 3.021315404115420679E-15 ) ) ;
#84367 = CARTESIAN_POINT ( 'NONE',  ( 200.4473000517033086, 270.8492857102374387, -11.53500569907702022 ) ) ;
#84368 = CARTESIAN_POINT ( 'NONE',  ( 17.75393198606386136, 12.11110640527291160, -2.839279412974138328 ) ) ;
#84369 = EDGE_CURVE ( 'NONE', #91598, #38047, #82053, .T. ) ;
#84370 = CARTESIAN_POINT ( 'NONE',  ( 198.5691746959190311, 277.5136763456665676, -15.35557735086660003 ) ) ;
#84371 = CARTESIAN_POINT ( 'NONE',  ( 48.48788556946983874, 102.1758113618167982, -10.00000000000000000 ) ) ;
#84373 = ORIENTED_EDGE ( 'NONE', *, *, #15747, .T. ) ;
#84372 = CARTESIAN_POINT ( 'NONE',  ( 14.65434579541627969, 179.2677522451418497, 10.00000000000009592 ) ) ;
#84374 = CARTESIAN_POINT ( 'NONE',  ( 202.4900219881211854, 279.9239892212719383, 15.63116161057562259 ) ) ;
#84375 = CARTESIAN_POINT ( 'NONE',  ( 188.8449905984804218, 259.7290283989091222, 2.370086273675485522 ) ) ;
#84376 = DIRECTION ( 'NONE',  ( -1.000000000000000000, 0.000000000000000000, 0.000000000000000000 ) ) ;
#84377 = CARTESIAN_POINT ( 'NONE',  ( 82.66171877364854481, 45.89212660847477565, -10.89646859988845407 ) ) ;
#84378 = CARTESIAN_POINT ( 'NONE',  ( 169.1186385402264420, 254.0988134251273038, 11.40381662627904014 ) ) ;
#84379 = CARTESIAN_POINT ( 'NONE',  ( 161.1720804342144788, 283.2912763611720379, 2.125355488856659036 ) ) ;
#84380 = ORIENTED_EDGE ( 'NONE', *, *, #3423, .T. ) ;
#84381 = CARTESIAN_POINT ( 'NONE',  ( 194.4048639213451679, 293.9278937801532834, -15.59881047903446927 ) ) ;
#84382 = CARTESIAN_POINT ( 'NONE',  ( 75.06185269395858484, 67.24559711482956459, -12.98328508234620848 ) ) ;
#84384 = ADVANCED_FACE ( 'NONE', ( #51331 ), #90892, .T. ) ;
#84383 = CARTESIAN_POINT ( 'NONE',  ( 54.07885559584777013, 190.4824982072973967, 3.021315404115420679E-15 ) ) ;
#84385 = CARTESIAN_POINT ( 'NONE',  ( 1.230952036757517520, 161.5177522451418213, 5.000000000000051514 ) ) ;
#84386 = CARTESIAN_POINT ( 'NONE',  ( 196.0942742968314860, 269.6800398832626229, -11.21024681009520840 ) ) ;
#84387 = CARTESIAN_POINT ( 'NONE',  ( 171.3390933369627191, 279.6671480371463758, -14.77428946034695834 ) ) ;
#84388 = CARTESIAN_POINT ( 'NONE',  ( 203.4842972674048269, 278.2018539208430639, -15.39142462160632263 ) ) ;
#84389 = CARTESIAN_POINT ( 'NONE',  ( 72.07832455930082460, 72.32227812425290381, 0.7968372639566179139 ) ) ;
#84390 = CARTESIAN_POINT ( 'NONE',  ( 72.65255621578388912, 70.92891038547531934, 7.631180297043450800 ) ) ;
#84392 = CARTESIAN_POINT ( 'NONE',  ( 188.1412547211656943, 273.5593357346770063, 17.08033167198486879 ) ) ;
#84391 = CARTESIAN_POINT ( 'NONE',  ( -1.394013918807642360, 163.8768266524159856, 9.188101187500098632 ) ) ;
#84393 = LINE ( 'NONE', #84890, #20415 ) ;
#84394 = ORIENTED_EDGE ( 'NONE', *, *, #49010, .T. ) ;
#84395 = ORIENTED_EDGE ( 'NONE', *, *, #28939, .F. ) ;
#84396 = DIRECTION ( 'NONE',  ( -0.5000000000000082157, 0.8660254037844338226, 0.000000000000000000 ) ) ;
#84397 = LINE ( 'NONE', #14942, #46406 ) ;
#84398 = EDGE_CURVE ( 'NONE', #75472, #1759, #60411, .T. ) ;
#84399 = LINE ( 'NONE', #24550, #25946 ) ;
#84400 = CARTESIAN_POINT ( 'NONE',  ( 86.83833563368834518, 43.79545931766734412, 3.564591285478730054 ) ) ;
#84401 = VECTOR ( 'NONE', #62448, 1000.000000000000000 ) ;
#84402 = CARTESIAN_POINT ( 'NONE',  ( 163.1248382027621062, 248.1064875868004549, -11.52679925016660079 ) ) ;
#84403 = CARTESIAN_POINT ( 'NONE',  ( 69.10006990169640062, 67.64574319074527864, 9.412775915974314955 ) ) ;
#84404 = CARTESIAN_POINT ( 'NONE',  ( 153.5650287317978950, 279.2224830237896640, 3.840963988500594617 ) ) ;
#84405 = CARTESIAN_POINT ( 'NONE',  ( 11.37951369124782453, 183.5024278399160949, 9.188101187500095079 ) ) ;
#84406 = CARTESIAN_POINT ( 'NONE',  ( 107.8059429699301575, 242.2369531367911009, -4.594050593750048428 ) ) ;
#84407 = CARTESIAN_POINT ( 'NONE',  ( 181.8184041672141120, 294.6703142210058104, -6.550043312232509685 ) ) ;
#84408 = CARTESIAN_POINT ( 'NONE',  ( 83.51092623577891061, 51.50185674319120466, -14.43088262691036583 ) ) ;
#84409 = CARTESIAN_POINT ( 'NONE',  ( 63.31414817410235685, 207.3615022471904012, 5.155647304959626652E-14 ) ) ;
#84410 = LINE ( 'NONE', #59562, #24284 ) ;
#84411 = CARTESIAN_POINT ( 'NONE',  ( 190.6088168084232279, 299.9436237569324248, -4.377057509834942906 ) ) ;
#84412 = CARTESIAN_POINT ( 'NONE',  ( 80.64963530044916240, 57.33823058590956379, -16.23392529860869260 ) ) ;
#84413 = CARTESIAN_POINT ( 'NONE',  ( 155.5888570658010508, 261.1591898008976500, 17.34682632352454945 ) ) ;
#84414 = CARTESIAN_POINT ( 'NONE',  ( 161.2488013048736377, 251.3558788108169040, -13.10044423494716170 ) ) ;
#84415 = CARTESIAN_POINT ( 'NONE',  ( 188.5288891056994203, 283.7822663309162294, 16.35679746564665749 ) ) ;
#84416 = CARTESIAN_POINT ( 'NONE',  ( 70.81256171061001226, 61.11968107447890475, -14.44615878937885967 ) ) ;
#84417 = EDGE_CURVE ( 'NONE', #70733, #48184, #36061, .T. ) ;
#84418 = EDGE_CURVE ( 'NONE', #67601, #14882, #29471, .T. ) ;
#84419 = CARTESIAN_POINT ( 'NONE',  ( 192.6383675332188830, 265.0412903862384724, 7.554505506666291836 ) ) ;
#84420 = CARTESIAN_POINT ( 'NONE',  ( 165.0478369365887374, 249.7899772327647270, -10.67719793920586469 ) ) ;
#84421 = CARTESIAN_POINT ( 'NONE',  ( 175.5041665230661465, 256.4755977299537335, -10.91805166175802633 ) ) ;
#84422 = FACE_OUTER_BOUND ( 'NONE', #63522, .T. ) ;
#84423 = FACE_OUTER_BOUND ( 'NONE', #57331, .T. ) ;
#84424 = CARTESIAN_POINT ( 'NONE',  ( -22.42236680055709641, 157.8615022471902591, 0.000000000000000000 ) ) ;
#84425 = ORIENTED_EDGE ( 'NONE', *, *, #76416, .F. ) ;
#84426 = CARTESIAN_POINT ( 'NONE',  ( 161.6021384458605326, 281.4729049090978492, -9.576418522834517333 ) ) ;
#84427 = ADVANCED_FACE ( 'NONE', ( #6740 ), #21526, .F. ) ;
#84428 = CARTESIAN_POINT ( 'NONE',  ( 42.45923888023187232, 122.5484010731363043, 10.00000000000000000 ) ) ;
#84429 = CARTESIAN_POINT ( 'NONE',  ( 104.8295012880686699, 222.1423013555409796, -4.594050593750043987 ) ) ;
#84430 = CARTESIAN_POINT ( 'NONE',  ( 19.81074232005190794, 13.29860640527291693, -2.839279412974138328 ) ) ;
#84431 = CARTESIAN_POINT ( 'NONE',  ( 76.02121808213912857, 59.89693054018422913, -16.23481010780869838 ) ) ;
#84432 = EDGE_CURVE ( 'NONE', #41822, #91585, #7221, .T. ) ;
#84433 = CARTESIAN_POINT ( 'NONE',  ( 10.06845959268932411, 31.07446838803123157, 10.00000000000000000 ) ) ;
#84435 = CARTESIAN_POINT ( 'NONE',  ( 112.9482291249501174, 226.0177522451418213, 5.000000000000051514 ) ) ;
#84434 = CARTESIAN_POINT ( 'NONE',  ( 136.1945356951059125, 260.9860189848785694, -2.679491924311252493 ) ) ;
#84436 = CARTESIAN_POINT ( 'NONE',  ( 159.9924463476198753, 283.3850188831759169, -3.371971149216307140 ) ) ;
#84437 = CARTESIAN_POINT ( 'NONE',  ( 151.0801312611820890, 268.9685319718947198, -15.83903210480701240 ) ) ;
#84438 = CARTESIAN_POINT ( 'NONE',  ( -73.66720466879952767, 50.53642055324488069, -10.00000000000000000 ) ) ;
#84439 = CARTESIAN_POINT ( 'NONE',  ( 36.89851624356406745, 36.70171378149922248, -9.188101187500004485 ) ) ;
#84440 = CARTESIAN_POINT ( 'NONE',  ( 33.92686603480522223, 41.36126292948897998, 6.180339887498949913 ) ) ;
#84441 = FACE_BOUND ( 'NONE', #6308, .T. ) ;
#84442 = VERTEX_POINT ( 'NONE', #54818 ) ;
#84443 = CARTESIAN_POINT ( 'NONE',  ( 29.64435718874111458, 29.06628583063843152, -9.188101187500006262 ) ) ;
#84444 = CARTESIAN_POINT ( 'NONE',  ( 179.0323333429434172, 280.8471605631614239, 16.29919625892006962 ) ) ;
#84445 = LINE ( 'NONE', #46379, #10239 ) ;
#84446 = CARTESIAN_POINT ( 'NONE',  ( 149.0598351764325002, 272.4677874370131576, -11.59078276432863674 ) ) ;
#84447 = EDGE_CURVE ( 'NONE', #49368, #85448, #26395, .T. ) ;
#84448 = EDGE_CURVE ( 'NONE', #56753, #11364, #46966, .T. ) ;
#84449 = VERTEX_POINT ( 'NONE', #94604 ) ;
#84450 = B_SPLINE_SURFACE_WITH_KNOTS ( 'NONE', 3, 1, ( 
 ( #2127, #62908 ),
 ( #1121, #62390 ),
 ( #33009, #31498 ),
 ( #15803, #9741 ),
 ( #71035, #25409 ),
 ( #79662, #92846 ),
 ( #16809, #85257 ),
 ( #77634, #47204 ),
 ( #8716, #56301 ),
 ( #93347, #1637 ),
 ( #47696, #78128 ),
 ( #16311, #40597 ),
 ( #55783, #8218 ),
 ( #71535, #23903 ),
 ( #10225, #70001 ),
 ( #23397, #54805 ),
 ( #32521, #78633 ),
 ( #63414, #94848 ),
 ( #63910, #94353 ),
 ( #31006, #61895 ),
 ( #54287, #24907 ),
 ( #86775, #85782 ),
 ( #17310, #48215 ),
 ( #17828, #89755 ),
 ( #81161, #95380 ),
 ( #80663, #27903 ),
 ( #26424, #96353 ),
 ( #3631, #88778 ),
 ( #35000, #73523 ),
 ( #49226, #35505 ),
 ( #97334, #89276 ),
 ( #25932, #73038 ),
 ( #12222, #34034 ),
 ( #51191, #34509 ) ),
 .UNSPECIFIED., .T., .F., .F.,
 ( 4, 2, 2, 2, 2, 2, 2, 2, 2, 2, 2, 2, 2, 2, 2, 2, 4 ),
 ( 2, 2 ),
 ( 0.000000000000000000, 0.06250000000000000000, 0.1250000000000000000, 0.1875000000000000000, 0.2500000000000000000, 0.3125000000000000000, 0.3750000000000000000, 0.4375000000000000000, 0.5000000000000000000, 0.5625000000000000000, 0.6250000000000000000, 0.6875000000000000000, 0.7500000000000000000, 0.8125000000000000000, 0.8750000000000000000, 0.9375000000000000000, 1.000000000000000000 ),
 ( 0.000000000000000000, 1.000000000000000000 ),
 .UNSPECIFIED. ) ;
#84451 = CARTESIAN_POINT ( 'NONE',  ( 84.51862751403463392, 49.89385305662934655, -13.69084041065644897 ) ) ;
#84452 = CARTESIAN_POINT ( 'NONE',  ( 159.8655504377736918, 253.7517395922482706, 15.51368179719542262 ) ) ;
#84453 = CARTESIAN_POINT ( 'NONE',  ( 179.9084428208875579, 262.7189347004215847, -12.75842409700454283 ) ) ;
#84454 = CARTESIAN_POINT ( 'NONE',  ( 169.3569635281594117, 252.0144808050329175, -8.621157649714792370 ) ) ;
#84455 = FACE_OUTER_BOUND ( 'NONE', #84574, .T. ) ;
#84456 = CARTESIAN_POINT ( 'NONE',  ( 149.1228319324105200, 250.2365022471901739, 10.00000000000009592 ) ) ;
#84457 = VERTEX_POINT ( 'NONE', #17567 ) ;
#84458 = B_SPLINE_CURVE_WITH_KNOTS ( 'NONE', 3,
 ( #2416, #85424, #53955, #24072, #69669, #70670, #38254, #93002, #15971, #84912, #25069, #40258, #55453, #14965, #23555, #94517 ),
 .UNSPECIFIED., .F., .F.,
 ( 4, 1, 2, 2, 2, 1, 2, 2, 4 ),
 ( 0.000000000000000000, 0.1250000000000077161, 0.1875000000000082712, 0.2500000000000088263, 0.5000000000000096589, 0.6250000000000094369, 0.6875000000000069944, 0.7500000000000045519, 1.000000000000000000 ),
 .UNSPECIFIED. ) ;
#84459 = CARTESIAN_POINT ( 'NONE',  ( 73.11654091825437263, 69.80299609433679109, 9.611781565164262631 ) ) ;
#84460 = CARTESIAN_POINT ( 'NONE',  ( 34.51575008502857855, 31.87878583063843863, -9.188101187500006262 ) ) ;
#84461 = ORIENTED_EDGE ( 'NONE', *, *, #35498, .F. ) ;
#84462 = CARTESIAN_POINT ( 'NONE',  ( 168.0266106847527681, 249.2181159516572393, 6.488127101935972973 ) ) ;
#84463 = CARTESIAN_POINT ( 'NONE',  ( 184.6854688042101600, 292.1945499485699997, -10.69498008038247505 ) ) ;
#84464 = VERTEX_POINT ( 'NONE', #93601 ) ;
#84465 = DIRECTION ( 'NONE',  ( 0.000000000000000000, 0.000000000000000000, 1.000000000000000000 ) ) ;
#84466 = DIRECTION ( 'NONE',  ( 0.000000000000000000, -0.000000000000000000, -1.000000000000000000 ) ) ;
#84467 = CARTESIAN_POINT ( 'NONE',  ( 84.78687102586546587, 50.23207448519301721, 13.79854428445948678 ) ) ;
#84468 = CARTESIAN_POINT ( 'NONE',  ( 153.7173656711216267, 264.4007079824105517, -16.52087364244192358 ) ) ;
#84469 = CARTESIAN_POINT ( 'NONE',  ( 169.3571508527084291, 283.0956279022483955, 12.63651818596384935 ) ) ;
#84470 = CARTESIAN_POINT ( 'NONE',  ( 37.97985170016632850, 33.87878583063844928, -9.188101187500006262 ) ) ;
#84471 = CARTESIAN_POINT ( 'NONE',  ( 81.46946648389129564, 55.43478263998397182, -16.31964423845217738 ) ) ;
#84472 = CARTESIAN_POINT ( 'NONE',  ( 76.34528211662409092, 62.05049414262115448, -15.76804433278676143 ) ) ;
#84473 = ORIENTED_EDGE ( 'NONE', *, *, #32916, .F. ) ;
#84474 = CARTESIAN_POINT ( 'NONE',  ( 87.11840409666331198, 45.31431352401795465, 7.035673371054458336 ) ) ;
#84475 = ORIENTED_EDGE ( 'NONE', *, *, #52413, .F. ) ;
#84476 = EDGE_LOOP ( 'NONE', ( #81133, #27741, #55843, #71638 ) ) ;
#84477 = CARTESIAN_POINT ( 'NONE',  ( 197.9827105953623061, 286.8556216960815846, 16.93946419794055558 ) ) ;
#84478 = CARTESIAN_POINT ( 'NONE',  ( 169.8667279133726424, 269.3604332311463168, 16.84841970499969932 ) ) ;
#84480 = CARTESIAN_POINT ( 'NONE',  ( -25.62627769214124740, 24.57763045674671432, -10.00000000000000000 ) ) ;
#84479 = CARTESIAN_POINT ( 'NONE',  ( 204.9432097630379417, 275.6749433546094679, 13.74700047688257776 ) ) ;
#84481 = DIRECTION ( 'NONE',  ( 0.4999999999999992784, -0.8660254037844390407, 0.000000000000000000 ) ) ;
#84482 = CARTESIAN_POINT ( 'NONE',  ( 197.8821111871073981, 272.3286829384299494, -13.44603622953895261 ) ) ;
#84483 = CARTESIAN_POINT ( 'NONE',  ( 203.5517807763935991, 276.4131063546051337, 14.32831804246049678 ) ) ;
#84484 = CARTESIAN_POINT ( 'NONE',  ( 82.56099630686816226, 41.03468078478306325, 1.095390248834374303 ) ) ;
#84485 = CARTESIAN_POINT ( 'NONE',  ( 171.6200503532151629, 250.8586239335233756, -5.669471818614393754 ) ) ;
#84486 = CARTESIAN_POINT ( 'NONE',  ( 76.77731254116882553, 64.09355814141258634, -15.16545583891342908 ) ) ;
#84487 = CARTESIAN_POINT ( 'NONE',  ( 188.7267243920021542, 295.1910411013678299, 11.79826141631466463 ) ) ;
#84488 = CARTESIAN_POINT ( 'NONE',  ( 116.5476472112030990, 238.0958772461660544, -9.188101187500095079 ) ) ;
#84490 = B_SPLINE_CURVE_WITH_KNOTS ( 'NONE', 3,
 ( #82003, #34365, #65262, #42931, #35357, #25785, #65751, #73870, #64777, #96206 ),
 .UNSPECIFIED., .F., .F.,
 ( 4, 2, 2, 2, 4 ),
 ( 0.000000000000000000, 0.0002622400424272904778, 0.0005244800848545809555, 0.0007867201272818714333, 0.001048960169709161911 ),
 .UNSPECIFIED. ) ;
#84489 = CARTESIAN_POINT ( 'NONE',  ( 187.1412927779018673, 261.9835105880691231, -10.20549468610707322 ) ) ;
#84491 = CARTESIAN_POINT ( 'NONE',  ( 41.11799749075662191, 32.24335787977766898, -9.188101187500008038 ) ) ;
#84492 = CARTESIAN_POINT ( 'NONE',  ( 190.0654284128779068, 274.4660007832150086, 15.78607938090247487 ) ) ;
#84493 = ORIENTED_EDGE ( 'NONE', *, *, #10202, .F. ) ;
#84494 = EDGE_CURVE ( 'NONE', #23594, #86318, #47023, .T. ) ;
#84495 = CARTESIAN_POINT ( 'NONE',  ( 162.8503517516483328, 249.0322973948848642, -10.17031201914153549 ) ) ;
#84496 = CARTESIAN_POINT ( 'NONE',  ( 71.89123681271787802, 63.83798092845757566, -13.42677533865197681 ) ) ;
#84497 = EDGE_CURVE ( 'NONE', #48849, #58283, #27695, .T. ) ;
#84498 = DIRECTION ( 'NONE',  ( -0.000000000000000000, -0.000000000000000000, 1.000000000000000000 ) ) ;
#84499 = CARTESIAN_POINT ( 'NONE',  ( 157.3025066944120454, 258.1910615777721887, 18.21299529665260053 ) ) ;
#84500 = CARTESIAN_POINT ( 'NONE',  ( 206.3423291502491566, 273.2515974901050413, -10.76717883871977577 ) ) ;
#84501 = CARTESIAN_POINT ( 'NONE',  ( 74.08065690531797998, 54.82731643721707826, -16.13522336645905142 ) ) ;
#84502 = ORIENTED_EDGE ( 'NONE', *, *, #26079, .T. ) ;
#84503 = CARTESIAN_POINT ( 'NONE',  ( 36.90034965944521872, 21.70852965304481685, 1.583844403245330712 ) ) ;
#84504 = ORIENTED_EDGE ( 'NONE', *, *, #41478, .T. ) ;
#84505 = FACE_OUTER_BOUND ( 'NONE', #70617, .T. ) ;
#84506 = LINE ( 'NONE', #29280, #70620 ) ;
#84507 = ORIENTED_EDGE ( 'NONE', *, *, #47205, .F. ) ;
#84509 = EDGE_CURVE ( 'NONE', #3476, #33732, #89521, .T. ) ;
#84508 = CARTESIAN_POINT ( 'NONE',  ( 191.5637510654044036, 267.2623274562577080, -12.69923334320934849 ) ) ;
#84510 = CARTESIAN_POINT ( 'NONE',  ( 191.8436243461450488, 298.3640908547560571, -10.97913512923284785 ) ) ;
#84511 = CARTESIAN_POINT ( 'NONE',  ( 158.4114053851006361, 263.3981549859118445, 17.73981754447373049 ) ) ;
#84512 = CARTESIAN_POINT ( 'NONE',  ( 72.23865006290039048, 71.95475215217994958, 3.607730569270007237 ) ) ;
#84514 = CARTESIAN_POINT ( 'NONE',  ( 69.80892481568059793, 63.14429736086585621, -13.67003195746243271 ) ) ;
#84513 = CARTESIAN_POINT ( 'NONE',  ( 184.3547604609693735, 288.6018926698813516, -13.48914676681425817 ) ) ;
#84515 = VECTOR ( 'NONE', #54356, 1000.000000000000000 ) ;
#84516 = CARTESIAN_POINT ( 'NONE',  ( 153.2906404175950854, 265.1398178023911782, -17.60231834963988007 ) ) ;
#84517 = EDGE_LOOP ( 'NONE', ( #5101, #18045, #32722, #59592 ) ) ;
#84518 = CARTESIAN_POINT ( 'NONE',  ( 147.5848197185516142, 275.0225891520124151, 4.420251097676741736 ) ) ;
#84519 = CARTESIAN_POINT ( 'NONE',  ( 190.6531941089592976, 264.1496977764022631, -9.546754457768564350 ) ) ;
#84520 = CARTESIAN_POINT ( 'NONE',  ( -77.74869931532472833, 54.01501336371526918, 177.5919119679930134 ) ) ;
#84522 = EDGE_CURVE ( 'NONE', #54608, #98801, #83300, .T. ) ;
#84521 = CARTESIAN_POINT ( 'NONE',  ( 190.3419708194589930, 270.7651379722268530, -14.14445603664571038 ) ) ;
#84523 = FACE_OUTER_BOUND ( 'NONE', #42458, .T. ) ;
#84524 = EDGE_CURVE ( 'NONE', #68842, #78966, #36746, .T. ) ;
#84525 = DIRECTION ( 'NONE',  ( 0.3653410243663972601, 0.9308737486442033582, 0.000000000000000000 ) ) ;
#84526 = CARTESIAN_POINT ( 'NONE',  ( 172.0630936339023265, 254.4764114392720273, 11.54978638049990103 ) ) ;
#84527 = CARTESIAN_POINT ( 'NONE',  ( 155.6559071247401960, 261.0430556921643870, 17.79853447468815375 ) ) ;
#84528 = CARTESIAN_POINT ( 'NONE',  ( 192.0172256599937555, 283.9084474676165541, -16.63802761579473710 ) ) ;
#84529 = CARTESIAN_POINT ( 'NONE',  ( 75.29676475605360508, 65.28063746041759430, -14.24902546994322883 ) ) ;
#84530 = CARTESIAN_POINT ( 'NONE',  ( 76.54827242179186442, 208.8768266524160140, 9.188101187500098632 ) ) ;
#84531 = CARTESIAN_POINT ( 'NONE',  ( 159.3995226465659982, 254.5589234043588078, -16.81133486613867234 ) ) ;
#84532 = FACE_OUTER_BOUND ( 'NONE', #90087, .T. ) ;
#84533 = CARTESIAN_POINT ( 'NONE',  ( 163.4084407101100851, 247.6152736349200438, -10.68829614238923931 ) ) ;
#84534 = FACE_OUTER_BOUND ( 'NONE', #55404, .T. ) ;
#84535 = CARTESIAN_POINT ( 'NONE',  ( 207.7296438747196134, 270.8486979012336633, -6.692930657757584001 ) ) ;
#84536 = CARTESIAN_POINT ( 'NONE',  ( 66.95904190137821388, 69.24049710015358983, 0.6601133702874718567 ) ) ;
#84538 = CARTESIAN_POINT ( 'NONE',  ( 75.85475627067550874, 51.57392296393066289, 15.72404477719369353 ) ) ;
#84537 = CYLINDRICAL_SURFACE ( 'NONE', #33830, 17.82106496071139645 ) ;
#84539 = CARTESIAN_POINT ( 'NONE',  ( 120.0388121219831277, 230.1115022471901739, -5.000000000000041744 ) ) ;
#84540 = EDGE_CURVE ( 'NONE', #24915, #30767, #6363, .T. ) ;
#84541 = CARTESIAN_POINT ( 'NONE',  ( -162.0327448629461742, 33.95614270198240803, 21.50000000000000000 ) ) ;
#84542 = B_SPLINE_CURVE_WITH_KNOTS ( 'NONE', 3,
 ( #97193, #20170, #97677, #88618 ),
 .UNSPECIFIED., .F., .F.,
 ( 4, 4 ),
 ( 0.000000000000000000, 0.006463808766467814271 ),
 .UNSPECIFIED. ) ;
#84543 = CARTESIAN_POINT ( 'NONE',  ( 205.2387912373514212, 275.1629812233222765, -12.22529801408222383 ) ) ;
#84544 =( BOUNDED_CURVE ( )  B_SPLINE_CURVE ( 2, ( #67020, #27555, #80796, #65532, #28520, #43716, #74660, #58902, #20447 ),
 .UNSPECIFIED., .F., .T. ) 
 B_SPLINE_CURVE_WITH_KNOTS ( ( 3, 2, 2, 2, 3 ),
 ( 0.6814516129032257563, 0.6827956989247311315, 0.6854838709677418818, 0.6881720430107527431, 0.6895161290322581182 ),
 .UNSPECIFIED. ) 
 CURVE ( )  GEOMETRIC_REPRESENTATION_ITEM ( )  RATIONAL_B_SPLINE_CURVE ( ( 0.9330127018922194093, 0.9330127018922194093, 1.000000000000000000, 0.8660254037844387076, 1.000000000000000000, 0.8660254037844387076, 1.000000000000000000, 0.9330127018922194093, 0.9330127018922194093 ) ) 
 REPRESENTATION_ITEM ( '' )  );
#84545 = CARTESIAN_POINT ( 'NONE',  ( 157.3412122618683497, 258.1240215684019290, 16.75554199904894048 ) ) ;
#84546 = CARTESIAN_POINT ( 'NONE',  ( 67.86860378221429357, 65.58690806574966814, -10.91583492536020294 ) ) ;
#84547 = EDGE_CURVE ( 'NONE', #81988, #49930, #10796, .T. ) ;
#84548 = CARTESIAN_POINT ( 'NONE',  ( 28.02335264628875677, 196.1744531367911293, 4.594050593750047540 ) ) ;
#84549 = B_SPLINE_CURVE_WITH_KNOTS ( 'NONE', 3,
 ( #2580, #72986, #2074, #94300 ),
 .UNSPECIFIED., .F., .F.,
 ( 4, 4 ),
 ( 0.008171735663598354502, 0.009370377214594900056 ),
 .UNSPECIFIED. ) ;
#84550 = CARTESIAN_POINT ( 'NONE',  ( 57.63111678181675757, 194.8923013555409796, 4.594050593750050204 ) ) ;
#84551 = DIRECTION ( 'NONE',  ( -0.4245406647209920559, -0.9054088711727195093, 0.000000000000000000 ) ) ;
#84552 = CARTESIAN_POINT ( 'NONE',  ( 27.21537010445219096, 39.21091486745862653, 7.012934429366973338E-14 ) ) ;
#84553 = ADVANCED_FACE ( 'NONE', ( #30146 ), #37247, .F. ) ;
#84554 = CARTESIAN_POINT ( 'NONE',  ( 165.5131940759252700, 248.9191784882033005, -9.449485365452053642 ) ) ;
#84555 = CARTESIAN_POINT ( 'NONE',  ( 152.3797953885492973, 246.5327760586659451, 1.948934522072303157E-15 ) ) ;
#84556 = CARTESIAN_POINT ( 'NONE',  ( 77.15888728817564868, 49.30424767902741934, 15.39427361423193652 ) ) ;
#84557 = CARTESIAN_POINT ( 'NONE',  ( 27.74991983456899902, 18.94754757982090254, 5.678558825948272215 ) ) ;
#84558 = CARTESIAN_POINT ( 'NONE',  ( -6.761740748788464650, 160.2365022471902023, 10.00000000000009948 ) ) ;
#84559 = FACE_OUTER_BOUND ( 'NONE', #98592, .T. ) ;
#84560 = CARTESIAN_POINT ( 'NONE',  ( 8.301057521190555732, 26.83396525600388571, -2.839279412974133887 ) ) ;
#84561 = CARTESIAN_POINT ( 'NONE',  ( 64.42391676880970408, 201.8768266524159856, -9.188101187500093303 ) ) ;
#84562 = CARTESIAN_POINT ( 'NONE',  ( 177.9552638626009298, 260.7378092407702184, -13.94576028113082877 ) ) ;
#84563 = CARTESIAN_POINT ( 'NONE',  ( 176.2149847824938433, 291.3419163123382987, 2.559328105002660614 ) ) ;
#84564 = EDGE_CURVE ( 'NONE', #73603, #49393, #95642, .T. ) ;
#84565 = CARTESIAN_POINT ( 'NONE',  ( 198.3523905153085423, 287.0905771551796306, 18.52598547438866206 ) ) ;
#84566 = CARTESIAN_POINT ( 'NONE',  ( 72.67973169220425689, 61.70005665674018758, 14.67617656207863952 ) ) ;
#84567 = CARTESIAN_POINT ( 'NONE',  ( 150.2766721647888062, 275.5052458213636442, 7.345517456364930808 ) ) ;
#84568 = CARTESIAN_POINT ( 'NONE',  ( 77.70055685185792527, 55.96283670942377597, -16.15846975066150293 ) ) ;
#84569 = CARTESIAN_POINT ( 'NONE',  ( 112.7497649734640817, 229.2365022471902023, 10.00000000000009592 ) ) ;
#84570 = CARTESIAN_POINT ( 'NONE',  ( 161.4726291907278721, 250.9681975403669867, 14.52346149734912117 ) ) ;
#84571 = CARTESIAN_POINT ( 'NONE',  ( 164.8869957832017690, 270.4589526275615867, -17.34276065877123330 ) ) ;
#84572 = ORIENTED_EDGE ( 'NONE', *, *, #24408, .F. ) ;
#84573 = LINE ( 'NONE', #54107, #89455 ) ;
#84574 = EDGE_LOOP ( 'NONE', ( #34952, #50667, #4717, #34518 ) ) ;
#84575 = CARTESIAN_POINT ( 'NONE',  ( 159.9788992190088948, 253.5554137441726255, -15.81862932303382330 ) ) ;
#84576 = CARTESIAN_POINT ( 'NONE',  ( 194.1186324107294752, 293.4280613340856689, 14.71475514768843951 ) ) ;
#84577 = CARTESIAN_POINT ( 'NONE',  ( 173.2412943989675398, 277.7050541934257240, 16.79641741871846250 ) ) ;
#84578 = ORIENTED_EDGE ( 'NONE', *, *, #5267, .F. ) ;
#84579 = CARTESIAN_POINT ( 'NONE',  ( 68.58246938045769525, 203.7365022471902307, 10.00000000000009948 ) ) ;
#84580 = CARTESIAN_POINT ( 'NONE',  ( 79.13141068964681324, 45.89859103142725871, -12.52778249399242405 ) ) ;
#84581 = CARTESIAN_POINT ( 'NONE',  ( 147.6508870500795467, 274.9081571770856272, -8.950912509993816712 ) ) ;
#84582 = CARTESIAN_POINT ( 'NONE',  ( 85.92861092779033072, 42.96335125230519481, 4.056038327995186599 ) ) ;
#84583 = LINE ( 'NONE', #6552, #50552 ) ;
#84585 = EDGE_LOOP ( 'NONE', ( #79761, #44818, #46707, #80851 ) ) ;
#84584 = VECTOR ( 'NONE', #9403, 1000.000000000000114 ) ;
#84586 = CARTESIAN_POINT ( 'NONE',  ( 14.90450122504689823, 30.64646525600389637, -2.839279412974133887 ) ) ;
#84587 = FACE_OUTER_BOUND ( 'NONE', #54659, .T. ) ;
#84588 = LINE ( 'NONE', #91682, #45613 ) ;
#84589 = EDGE_LOOP ( 'NONE', ( #43505, #66091, #75241, #2892 ) ) ;
#84590 = CARTESIAN_POINT ( 'NONE',  ( 132.5240116932087062, 253.9865022471903160, 10.00000000000009415 ) ) ;
#84591 = DIRECTION ( 'NONE',  ( 0.4999999999999992784, -0.8660254037844390407, 0.000000000000000000 ) ) ;
#84592 = ORIENTED_EDGE ( 'NONE', *, *, #8556, .T. ) ;
#84593 = CARTESIAN_POINT ( 'NONE',  ( 174.7910919356739328, 286.1561555264053709, 10.71420828047212659 ) ) ;
#84595 = CARTESIAN_POINT ( 'NONE',  ( 67.72007239575214044, 65.87765530913392809, -10.53033397204468535 ) ) ;
#84594 = CARTESIAN_POINT ( 'NONE',  ( 163.2724435917976678, 283.7496115282986011, -3.044820943940299784 ) ) ;
#84596 = CARTESIAN_POINT ( 'NONE',  ( -19.65312891409030271, 93.06504152958497400, 45.00000000000000711 ) ) ;
#84597 = CARTESIAN_POINT ( 'NONE',  ( 204.1793240545508752, 276.9980322128846524, 14.17550310845996187 ) ) ;
#84598 = CARTESIAN_POINT ( 'NONE',  ( 159.4889735931715222, 254.4039898200529706, 16.88104032092801887 ) ) ;
#84599 = CARTESIAN_POINT ( 'NONE',  ( 161.0576509603776003, 262.9785022463822202, -17.65625271138400976 ) ) ;
#84600 = CARTESIAN_POINT ( 'NONE',  ( 164.6290063521823868, 245.5011919288776028, 5.622032409704942779 ) ) ;
#84601 = CARTESIAN_POINT ( 'NONE',  ( 159.5585398265464221, 254.8728140044053134, -15.62969674525248642 ) ) ;
#84602 = VECTOR ( 'NONE', #24226, 1000.000000000000114 ) ;
#84603 = CARTESIAN_POINT ( 'NONE',  ( 181.8843194246268808, 260.3488174177143719, 9.482408816024305409 ) ) ;
#84604 = CARTESIAN_POINT ( 'NONE',  ( 70.72975101405640430, 202.4548013555409796, -4.594050593750042211 ) ) ;
#84605 = ORIENTED_EDGE ( 'NONE', *, *, #69177, .F. ) ;
#84606 = CARTESIAN_POINT ( 'NONE',  ( 173.9522839582943163, 265.4328302768140588, 16.77064627941505748 ) ) ;
#84607 = CARTESIAN_POINT ( 'NONE',  ( -22.42236680055709641, 157.8615022471902591, 0.000000000000000000 ) ) ;
#84608 = CARTESIAN_POINT ( 'NONE',  ( -16.25778278694858514, 23.14743555886465032, -10.00000000000000000 ) ) ;
#84609 = ORIENTED_EDGE ( 'NONE', *, *, #80886, .T. ) ;
#84610 = CARTESIAN_POINT ( 'NONE',  ( 160.8697417715285951, 254.0124291816641176, 15.72951850990217437 ) ) ;
#84611 = VERTEX_POINT ( 'NONE', #43848 ) ;
#84612 = EDGE_LOOP ( 'NONE', ( #59724, #76963, #10798, #86806 ) ) ;
#84613 = FACE_BOUND ( 'NONE', #15512, .T. ) ;
#84614 = CARTESIAN_POINT ( 'NONE',  ( 66.48824783888160539, 67.83064937571610642, 6.804944701791020734 ) ) ;
#84615 = CARTESIAN_POINT ( 'NONE',  ( 87.63077671684244763, 43.37939755374765838, -0.6475992473115442793 ) ) ;
#84616 = CARTESIAN_POINT ( 'NONE',  ( 81.22503698233943226, 55.71330003141861198, 16.38398667929945773 ) ) ;
#84617 = CARTESIAN_POINT ( 'NONE',  ( 194.2764122224708103, 294.1503786489221284, 15.46903869661980835 ) ) ;
#84618 = CARTESIAN_POINT ( 'NONE',  ( 72.70404828370719486, 224.3297689869269789, -2.679491924311252493 ) ) ;
#84619 = CARTESIAN_POINT ( 'NONE',  ( 75.30318735596920021, 214.2833772461660544, -9.188101187500095079 ) ) ;
#84620 = ORIENTED_EDGE ( 'NONE', *, *, #86371, .F. ) ;
#84621 = CARTESIAN_POINT ( 'NONE',  ( 201.0579808891486380, 282.4043571632192311, -17.91925047041473107 ) ) ;
#84622 = ORIENTED_EDGE ( 'NONE', *, *, #11273, .T. ) ;
#84623 = CARTESIAN_POINT ( 'NONE',  ( 93.04999876614748189, 212.9824982072973683, 3.021315404115420679E-15 ) ) ;
#84624 = EDGE_CURVE ( 'NONE', #24993, #92061, #59015, .T. ) ;
#84625 = CARTESIAN_POINT ( 'NONE',  ( 183.9161760165103772, 275.2808736645490626, 16.40347525101666193 ) ) ;
#84626 = CARTESIAN_POINT ( 'NONE',  ( 165.0565241268390366, 244.7607094220335568, 2.191926263411719589 ) ) ;
#84627 = CARTESIAN_POINT ( 'NONE',  ( 162.5349543250319471, 283.9950716909000903, 0.5116008960414863971 ) ) ;
#84628 = CARTESIAN_POINT ( 'NONE',  ( 195.1300253905141631, 279.2719974992415359, 16.35492678998735983 ) ) ;
#84629 = CARTESIAN_POINT ( 'NONE',  ( 160.4812992605921238, 260.2430605036401516, 16.67286839615865546 ) ) ;
#84630 = ORIENTED_EDGE ( 'NONE', *, *, #14349, .F. ) ;
#84631 = CARTESIAN_POINT ( 'NONE',  ( 192.1520400720565078, 296.4596862432644571, 11.25539976459215374 ) ) ;
#84632 = CARTESIAN_POINT ( 'NONE',  ( 185.4907235204558447, 259.9682112630936786, 5.899277730949330945 ) ) ;
#84633 = CARTESIAN_POINT ( 'NONE',  ( 87.85193346898986988, 44.00982651358195596, -1.829615609843908253 ) ) ;
#84635 = ADVANCED_FACE ( 'NONE', ( #71170 ), #54939, .F. ) ;
#84634 = CARTESIAN_POINT ( 'NONE',  ( 201.1755594471486859, 282.2007051268825535, -18.15567516623250910 ) ) ;
#84636 = CARTESIAN_POINT ( 'NONE',  ( 72.99830029227618411, 70.81959382475521636, 8.127746218293808056 ) ) ;
#84637 = EDGE_CURVE ( 'NONE', #13195, #71254, #5938, .T. ) ;
#84638 = CARTESIAN_POINT ( 'NONE',  ( 74.51773952002177737, 66.51868515611822374, -12.81989038982261597 ) ) ;
#84639 = ORIENTED_EDGE ( 'NONE', *, *, #15644, .T. ) ;
#84640 = CARTESIAN_POINT ( 'NONE',  ( 195.7061616849477730, 265.3944924174461448, 4.819710038644158701 ) ) ;
#84641 = CARTESIAN_POINT ( 'NONE',  ( 201.4430264223318261, 273.1213752465389462, 13.07311719109280546 ) ) ;
#84642 = DIRECTION ( 'NONE',  ( -0.4554470513245731378, -0.8902628732232696906, 0.000000000000000000 ) ) ;
#84643 = CARTESIAN_POINT ( 'NONE',  ( 184.6976757848609623, 263.8739595640468565, -12.18454262072885541 ) ) ;
#84644 = CARTESIAN_POINT ( 'NONE',  ( 84.04820955589276821, 51.68058956114519020, 14.75728579592695766 ) ) ;
#84645 = CARTESIAN_POINT ( 'NONE',  ( 195.8374195215319560, 264.5068004645912652, 0.8301787805199302150 ) ) ;
#84646 = ORIENTED_EDGE ( 'NONE', *, *, #99469, .F. ) ;
#84647 = CARTESIAN_POINT ( 'NONE',  ( 147.4963928429778264, 275.1757489932608109, 4.929816573182678852 ) ) ;
#84648 = CARTESIAN_POINT ( 'NONE',  ( 186.5996133936216097, 282.5293965020246674, 16.20464955667571871 ) ) ;
#84649 = VECTOR ( 'NONE', #93650, 1000.000000000000000 ) ;
#84650 = DIRECTION ( 'NONE',  ( -0.1710100716628374096, 0.2961981327260301833, 0.9396926207859057634 ) ) ;
#84652 = CARTESIAN_POINT ( 'NONE',  ( 73.67824366220462196, 55.52431661992799405, 16.58293632014991559 ) ) ;
#84651 = CARTESIAN_POINT ( 'NONE',  ( 167.5815824773973191, 259.8598515869122707, -16.53346283481762313 ) ) ;
#84653 = CARTESIAN_POINT ( 'NONE',  ( 19.21972384509095733, 29.83478043621388309, -8.090169943749479842 ) ) ;
#84654 = CARTESIAN_POINT ( 'NONE',  ( 148.9517569034208009, 272.6549844970639924, 12.50737104496728236 ) ) ;
#84655 = CARTESIAN_POINT ( 'NONE',  ( 166.1327689491646709, 286.5586531720609855, -3.311317316613562767 ) ) ;
#84656 = DIRECTION ( 'NONE',  ( 1.000000000000000000, 0.000000000000000000, 0.000000000000000000 ) ) ;
#84657 = DIRECTION ( 'NONE',  ( 0.000000000000000000, 0.000000000000000000, 1.000000000000000000 ) ) ;
#84658 = EDGE_CURVE ( 'NONE', #91719, #100031, #7339, .T. ) ;
#84659 = CARTESIAN_POINT ( 'NONE',  ( 144.0529748775411463, 260.6427522451418781, 10.00000000000009237 ) ) ;
#84660 = LINE ( 'NONE', #46100, #35540 ) ;
#84661 = ORIENTED_EDGE ( 'NONE', *, *, #71141, .T. ) ;
#84663 = CARTESIAN_POINT ( 'NONE',  ( 66.71375026165955546, 67.41994310576295391, -6.688024140652689020 ) ) ;
#84662 = VECTOR ( 'NONE', #29107, 1000.000000000000227 ) ;
#84664 = ADVANCED_FACE ( 'NONE', ( #86407, #84885 ), #78763, .F. ) ;
#84665 = CARTESIAN_POINT ( 'NONE',  ( 72.81630190666359681, 70.85884106002271210, -7.900673142507891100 ) ) ;
#84666 = DIRECTION ( 'NONE',  ( 0.4999999999999998890, -0.8660254037844385966, 0.000000000000000000 ) ) ;
#84667 = CARTESIAN_POINT ( 'NONE',  ( 7.969365115964080815, 187.6589784336661637, -6.496448406907676862E-16 ) ) ;
#84668 = CARTESIAN_POINT ( 'NONE',  ( 176.1757538807019330, 265.5509619629168583, -16.23131976009116784 ) ) ;
#84669 = CARTESIAN_POINT ( 'NONE',  ( 171.9467656383669123, 290.1344116725977642, 2.734564134658529877 ) ) ;
#84670 = CARTESIAN_POINT ( 'NONE',  ( 179.5568545132203440, 274.2926861780458125, -16.60646468900087314 ) ) ;
#84671 = CARTESIAN_POINT ( 'NONE',  ( 30.24436146177389162, 33.16454794089043645, -10.00000000000000355 ) ) ;
#84672 = CARTESIAN_POINT ( 'NONE',  ( 181.0304098800548331, 294.4207640661956020, 6.547035950180724484 ) ) ;
#84673 = CARTESIAN_POINT ( 'NONE',  ( 173.0199565421851560, 272.3281153120731233, -16.37689176781418610 ) ) ;
#84674 = CARTESIAN_POINT ( 'NONE',  ( 156.5950988087852238, 281.5581451644223421, -2.717916794402165603 ) ) ;
#84675 = B_SPLINE_SURFACE_WITH_KNOTS ( 'NONE', 3, 1, ( 
 ( #76434, #43513 ),
 ( #60191, #6525 ),
 ( #91152, #22215 ),
 ( #99230, #28311 ),
 ( #59189, #60690 ),
 ( #5523, #14622 ),
 ( #97258, #90165 ),
 ( #82577, #36910 ),
 ( #74452, #90674 ),
 ( #29816, #21717 ),
 ( #84069, #98239 ),
 ( #83558, #45501 ),
 ( #36407, #7009 ),
 ( #52109, #89675 ),
 ( #20738, #83056 ),
 ( #13629, #86573 ),
 ( #62193, #23201 ),
 ( #24219, #92171 ),
 ( #93654, #55099 ),
 ( #77929, #39389 ),
 ( #39886, #17106 ),
 ( #62697, #919 ),
 ( #53600, #47506 ),
 ( #48002, #45988 ),
 ( #1430, #8520 ),
 ( #78946, #37894 ),
 ( #76905, #22721 ),
 ( #86086, #30819 ),
 ( #69313, #93144 ),
 ( #24707, #9014 ),
 ( #16610, #70306 ),
 ( #77431, #54092 ),
 ( #78433, #94154 ),
 ( #55590, #7503 ) ),
 .UNSPECIFIED., .T., .F., .F.,
 ( 4, 2, 2, 2, 2, 2, 2, 2, 2, 2, 2, 2, 2, 2, 2, 2, 4 ),
 ( 2, 2 ),
 ( 0.000000000000000000, 0.06250000000000000000, 0.1250000000000000000, 0.1875000000000000000, 0.2500000000000000000, 0.3125000000000000000, 0.3750000000000000000, 0.4375000000000000000, 0.5000000000000000000, 0.5625000000000000000, 0.6250000000000000000, 0.6875000000000000000, 0.7500000000000000000, 0.8125000000000000000, 0.8750000000000000000, 0.9375000000000000000, 1.000000000000000000 ),
 ( 0.000000000000000000, 1.000000000000000000 ),
 .UNSPECIFIED. ) ;
#84676 = EDGE_CURVE ( 'NONE', #42808, #39213, #32646, .T. ) ;
#84677 = CARTESIAN_POINT ( 'NONE',  ( 120.8212928151578041, 69.75620593067000641, 5.188172501216618598E-14 ) ) ;
#84678 = CARTESIAN_POINT ( 'NONE',  ( 191.4137818629626508, 260.8670317507109644, -1.392421146808482169 ) ) ;
#84679 = CARTESIAN_POINT ( 'NONE',  ( 183.1080230832341726, 295.7359842595169539, 1.141048727436130727 ) ) ;
#84680 = CARTESIAN_POINT ( 'NONE',  ( 76.37669801451764329, 208.2365022471902023, 10.00000000000009592 ) ) ;
#84681 = CARTESIAN_POINT ( 'NONE',  ( 44.08964769951546714, 27.58380873178790793, 6.180339887498953466 ) ) ;
#84682 = CARTESIAN_POINT ( 'NONE',  ( 147.6947327179224487, 274.8322142526899370, 9.090449717876689206 ) ) ;
#84683 = CARTESIAN_POINT ( 'NONE',  ( 22.06942799527072907, 192.7369531367911293, -4.594050593750048428 ) ) ;
#84684 = CARTESIAN_POINT ( 'NONE',  ( 66.87061822793073418, 67.94793007289314346, 7.000923078224633223 ) ) ;
#84685 = CARTESIAN_POINT ( 'NONE',  ( 36.78662229117171734, 22.20801979619930933, -3.090169943749474069 ) ) ;
#84686 = CARTESIAN_POINT ( 'NONE',  ( 42.15419773769040290, 26.19860640527295814, 2.839279412974134775 ) ) ;
#84687 = CARTESIAN_POINT ( 'NONE',  ( 199.2205425252482200, 285.5868937652708155, -18.05012564782189344 ) ) ;
#84688 = CARTESIAN_POINT ( 'NONE',  ( 164.8329445879545290, 245.1479605429143760, -2.955380775890217304 ) ) ;
#84689 = CARTESIAN_POINT ( 'NONE',  ( 198.2505066714982149, 285.2670451491296149, 0.000000000000000000 ) ) ;
#84690 = CARTESIAN_POINT ( 'NONE',  ( 163.1799518951598600, 280.9192836996226674, -10.08564493774514403 ) ) ;
#84691 = CARTESIAN_POINT ( 'NONE',  ( 179.7565560748202813, 262.9145626453345130, -12.95070181807916043 ) ) ;
#84692 = PRODUCT_CONTEXT ( 'NONE', #51809, 'mechanical' ) ;
#84693 = CARTESIAN_POINT ( 'NONE',  ( 18.74326920199815305, 31.79752408145591858, -5.678558825948271327 ) ) ;
#84694 = CARTESIAN_POINT ( 'NONE',  ( 189.8147415777049218, 301.8782188922952514, -0.5019643756309712934 ) ) ;
#84695 = CARTESIAN_POINT ( 'NONE',  ( 72.04081558064058299, 59.27854915901136934, 15.34716367762108824 ) ) ;
#84696 = CARTESIAN_POINT ( 'NONE',  ( 194.2669918475045279, 294.1666952169902629, 14.00965265288584050 ) ) ;
#84697 = VERTEX_POINT ( 'NONE', #63045 ) ;
#84698 = CARTESIAN_POINT ( 'NONE',  ( 40.84394904227130496, 31.78052372038643725, -10.00000000000000355 ) ) ;
#84699 = CARTESIAN_POINT ( 'NONE',  ( 87.62133583293774564, 45.31115884160845297, -7.293173845241971875 ) ) ;
#84700 = DIRECTION ( 'NONE',  ( 0.000000000000000000, 0.000000000000000000, 1.000000000000000000 ) ) ;
#84701 = CARTESIAN_POINT ( 'NONE',  ( 81.74304277033319011, 42.07055560370181269, 7.558611063322482337 ) ) ;
#84702 = ORIENTED_EDGE ( 'NONE', *, *, #90559, .F. ) ;
#84703 = DIRECTION ( 'NONE',  ( 0.9746548163034763901, -0.2237140788069380548, 0.000000000000000000 ) ) ;
#84704 = CARTESIAN_POINT ( 'NONE',  ( 72.31870688955723381, 71.66728745601001549, -5.813503713761849490 ) ) ;
#84705 = B_SPLINE_CURVE_WITH_KNOTS ( 'NONE', 3,
 ( #83704, #6162, #16753, #78069, #23342, #17250, #16253, #94296, #85719, #62845, #8656, #71476, #40035, #70976, #32460, #79097, #25352, #47641, #40542, #48154, #56244, #86216, #1577, #9159, #38545, #61840, #55725, #46648, #87237, #54230, #31940, #9681, #78575, #30951, #46133, #94792, #63357, #85197, #68, #7654, #24851, #92787, #63854, #77046, #86713, #54736, #15740, #31442, #77573, #2069, #32949, #8162 ),
 .UNSPECIFIED., .F., .F.,
 ( 4, 2, 2, 2, 2, 2, 2, 2, 2, 2, 2, 2, 2, 2, 2, 2, 2, 2, 2, 2, 2, 2, 2, 2, 2, 4 ),
 ( 0.0008616133506683544942, 0.001349225619325013920, 0.001836837887981673453, 0.002080644022310002787, 0.002324450156638332987, 0.002446353223802498738, 0.002568256290966664922, 0.002690159358130831107, 0.002812062425294997291, 0.003055868559623329660, 0.003299674693951661596, 0.003787286962608326334, 0.004762511499921721729, 0.005737736037235116257, 0.006225348305891820894, 0.006469154440220215713, 0.006712960574548609664, 0.006773912108130736992, 0.006834863641712863452, 0.006895815175294989913, 0.006956766708877116373, 0.007200572843205529407, 0.007688185111862339861, 0.008175797380519149449, 0.008419603514847556411, 0.008663409649175963373 ),
 .UNSPECIFIED. ) ;
#84706 = CARTESIAN_POINT ( 'NONE',  ( 28.84760059290936951, 18.78380873178787880, -6.180339887498949025 ) ) ;
#84707 = CARTESIAN_POINT ( 'NONE',  ( -36.52772323645827868, 26.41323893245353105, 10.00000000000000000 ) ) ;
#84708 = EDGE_CURVE ( 'NONE', #68859, #8907, #53475, .T. ) ;
#84709 = EDGE_LOOP ( 'NONE', ( #71613, #14794, #54347, #28614 ) ) ;
#84711 =( LENGTH_UNIT ( ) NAMED_UNIT ( * ) SI_UNIT ( .MILLI., .METRE. ) );
#84710 = CARTESIAN_POINT ( 'NONE',  ( 73.05863210132505969, 69.60576123971952711, -9.808587366596247747 ) ) ;
#84712 = ORIENTED_EDGE ( 'NONE', *, *, #31466, .F. ) ;
#84713 = CARTESIAN_POINT ( 'NONE',  ( 151.3560786774222322, 268.4905770267490652, 15.54402364351346932 ) ) ;
#84714 = CYLINDRICAL_SURFACE ( 'NONE', #35119, 16.60714546451156792 ) ;
#84715 = CARTESIAN_POINT ( 'NONE',  ( 80.14478464935454838, 57.78471241749840459, 16.60281329265516348 ) ) ;
#84716 = CARTESIAN_POINT ( 'NONE',  ( 45.26186829773988052, 208.4860189848785410, -2.679491924311252493 ) ) ;
#84718 = ORIENTED_EDGE ( 'NONE', *, *, #36810, .T. ) ;
#84717 = EDGE_CURVE ( 'NONE', #2713, #5430, #92981, .T. ) ;
#84719 = CARTESIAN_POINT ( 'NONE',  ( 189.8136646974935786, 301.8800841035353528, -0.6430783927310335102 ) ) ;
#84720 = CARTESIAN_POINT ( 'NONE',  ( 149.2765980486851731, 272.0923431290771646, -11.40617906909507973 ) ) ;
#84721 = CARTESIAN_POINT ( 'NONE',  ( 174.6653058907003526, 271.2610659076526076, 17.81995586319052549 ) ) ;
#84722 = ORIENTED_EDGE ( 'NONE', *, *, #11582, .F. ) ;
#84723 = CARTESIAN_POINT ( 'NONE',  ( 157.0848929289108469, 258.5679796760466047, 17.57466231005294688 ) ) ;
#84724 = CARTESIAN_POINT ( 'NONE',  ( 158.3850792441787689, 265.2446733984589287, 17.11029620794053940 ) ) ;
#84725 = ORIENTED_EDGE ( 'NONE', *, *, #52233, .F. ) ;
#84726 = CYLINDRICAL_SURFACE ( 'NONE', #55198, 16.60714546451156792 ) ;
#84727 = PLANE ( 'NONE',  #59537 ) ;
#84728 = VERTEX_POINT ( 'NONE', #249 ) ;
#84729 = B_SPLINE_CURVE_WITH_KNOTS ( 'NONE', 3,
 ( #10495, #41378, #72317, #33814, #64701, #95652, #49486, #41887, #72826, #98100, #61559, #92506, #69163, #52973, #29193, #38248, #44862, #99587, #53461, #61057, #29681, #5393, #60061, #92028, #36277, #68169, #74814, #22574, #82449, #91024, #51481, #13986, #22077, #82926, #67176, #45365, #60554, #83418, #91511, #75803, #5884, #21588, #83923, #28678, #99097, #75303 ),
 .UNSPECIFIED., .F., .F.,
 ( 4, 1, 1, 1, 2, 2, 1, 1, 1, 2, 2, 1, 1, 2, 2, 1, 1, 2, 2, 1, 1, 2, 2, 1, 2, 2, 1, 2, 2, 4 ),
 ( 0.000000000000000000, 0.06250000000000432987, 0.09375000000000677236, 0.1093750000000077022, 0.1171875000000101169, 0.1250000000000125178, 0.1875000000000266454, 0.2187500000000355826, 0.2343750000000378308, 0.2421875000000389966, 0.2500000000000401346, 0.3125000000000325295, 0.3437500000000286993, 0.3593750000000287548, 0.3750000000000287548, 0.4375000000000236478, 0.4687500000000210942, 0.4843750000000198730, 0.5000000000000186517, 0.5625000000000140998, 0.5937500000000134337, 0.6093750000000115463, 0.6250000000000096589, 0.6875000000000064393, 0.7187500000000063283, 0.7500000000000063283, 0.8125000000000061062, 0.8437500000000059952, 0.8750000000000059952, 1.000000000000000000 ),
 .UNSPECIFIED. ) ;
#84730 = CARTESIAN_POINT ( 'NONE',  ( -5.530696300892750550, 75.41849186590253851, 14.61344814751857868 ) ) ;
#84731 = CARTESIAN_POINT ( 'NONE',  ( 24.39104846783644831, 37.58029201028042365, 1.583844403245397769 ) ) ;
#84732 = DIRECTION ( 'NONE',  ( 0.5000000000000013323, -0.8660254037844378194, 0.000000000000000000 ) ) ;
#84733 = CARTESIAN_POINT ( 'NONE',  ( 83.25425189550011851, 52.37281273071425858, 14.86008439172370110 ) ) ;
#84734 = EDGE_LOOP ( 'NONE', ( #21382, #31970, #36467, #47466 ) ) ;
#84735 = ORIENTED_EDGE ( 'NONE', *, *, #38578, .F. ) ;
#84736 = CARTESIAN_POINT ( 'NONE',  ( 86.68854498236711947, 46.42444261617848866, 9.093522239322870959 ) ) ;
#84737 = VECTOR ( 'NONE', #36408, 1000.000000000000000 ) ;
#84738 = CARTESIAN_POINT ( 'NONE',  ( 175.1013262022588037, 291.4808567457044433, 5.510497698069581674 ) ) ;
#84739 = CARTESIAN_POINT ( 'NONE',  ( 148.2980785574368952, 273.7871886041155562, 9.134436720559454770 ) ) ;
#84740 = CARTESIAN_POINT ( 'NONE',  ( 149.3883679478359454, 271.8987519849911223, 12.99187507659642371 ) ) ;
#84741 = CARTESIAN_POINT ( 'NONE',  ( 141.2767884429413243, 240.8262482093457777, 3.021315404115420679E-15 ) ) ;
#84742 = CARTESIAN_POINT ( 'NONE',  ( 7.533646096595723485, 16.30066082961419482, -10.00000000000000533 ) ) ;
#84743 = CARTESIAN_POINT ( 'NONE',  ( 147.1259762202154207, 275.8173294038533641, -0.6716460511724978710 ) ) ;
#84744 = CARTESIAN_POINT ( 'NONE',  ( -22.42236680055709641, 157.8615022471902591, 0.000000000000000000 ) ) ;
#84745 = LINE ( 'NONE', #23390, #88350 ) ;
#84746 = CARTESIAN_POINT ( 'NONE',  ( 49.93482446054090218, 85.48106202472366988, 177.5919119679930134 ) ) ;
#84747 = FACE_OUTER_BOUND ( 'NONE', #10854, .T. ) ;
#84748 = CARTESIAN_POINT ( 'NONE',  ( 73.78444379368663419, 64.77329786477272933, -13.56033333088950066 ) ) ;
#84749 = CARTESIAN_POINT ( 'NONE',  ( 78.15171962155767460, 47.58880439823153097, 14.43428839942771447 ) ) ;
#84750 = VERTEX_POINT ( 'NONE', #93989 ) ;
#84751 = CARTESIAN_POINT ( 'NONE',  ( 190.4076394944172250, 300.8512895768478188, -4.816292592624366264 ) ) ;
#84752 = B_SPLINE_CURVE_WITH_KNOTS ( 'NONE', 3,
 ( #14401, #687, #22491, #46788 ),
 .UNSPECIFIED., .F., .F.,
 ( 4, 4 ),
 ( 0.01075463767794331005, 0.01639907954706086926 ),
 .UNSPECIFIED. ) ;
#84753 = CARTESIAN_POINT ( 'NONE',  ( 84.43516343181975969, 42.02615065117144866, -0.07733096528512554968 ) ) ;
#84754 = CARTESIAN_POINT ( 'NONE',  ( 87.72955037964742075, 45.02833699891566255, -6.646681420800613971 ) ) ;
#84755 = CARTESIAN_POINT ( 'NONE',  ( 79.09664598837733251, 45.97851813324576398, 13.19840075976098426 ) ) ;
#84756 = ADVANCED_FACE ( 'NONE', ( #7855 ), #47338, .F. ) ;
#84757 = CARTESIAN_POINT ( 'NONE',  ( -110.0000000000000142, 4.999999999999999112, -14.21260523776211215 ) ) ;
#84758 = EDGE_CURVE ( 'NONE', #22248, #82006, #87834, .T. ) ;
#84759 = DIRECTION ( 'NONE',  ( -0.8660254037844377084, -0.5000000000000014433, -0.000000000000000000 ) ) ;
#84760 = CARTESIAN_POINT ( 'NONE',  ( 169.2719858167531584, 285.1210977770464865, -7.931911058023441541 ) ) ;
#84761 = ORIENTED_EDGE ( 'NONE', *, *, #94717, .T. ) ;
#84762 = CARTESIAN_POINT ( 'NONE',  ( 162.6262389125959373, 248.9700868899859074, -10.50380342094597808 ) ) ;
#84763 = ADVANCED_FACE ( 'NONE', ( #39221 ), #741, .T. ) ;
#84764 = DIRECTION ( 'NONE',  ( -0.8660254037844377084, -0.5000000000000014433, -0.000000000000000000 ) ) ;
#84765 = EDGE_CURVE ( 'NONE', #23591, #41972, #98018, .T. ) ;
#84766 = CARTESIAN_POINT ( 'NONE',  ( 46.26427303354824261, 207.5177522451419065, 5.000000000000046185 ) ) ;
#84767 = CARTESIAN_POINT ( 'NONE',  ( 123.0428377395863890, 241.8458772461660544, 9.188101187500095079 ) ) ;
#84768 = CARTESIAN_POINT ( 'NONE',  ( 198.8533049117289977, 286.2229679703367538, -18.60939981449148561 ) ) ;
#84769 = DIRECTION ( 'NONE',  ( 1.000000000000000000, 0.000000000000000000, 0.000000000000000000 ) ) ;
#84770 = CARTESIAN_POINT ( 'NONE',  ( 196.1613785401733878, 290.8855212161054737, 15.98157687694135021 ) ) ;
#84771 = CARTESIAN_POINT ( 'NONE',  ( 174.8240844530040761, 253.1383486689193774, -3.879012981929475856 ) ) ;
#84772 = CARTESIAN_POINT ( 'NONE',  ( 49.15987193134396449, 205.3149278399160949, -9.188101187500095079 ) ) ;
#84773 = CARTESIAN_POINT ( 'NONE',  ( 175.3149167492775860, 290.9749816300547991, -6.569057798006298299 ) ) ;
#84774 = CARTESIAN_POINT ( 'NONE',  ( 68.79270342570836760, 66.32932566076951275, -9.981102178220000454 ) ) ;
#84775 = ORIENTED_EDGE ( 'NONE', *, *, #13452, .T. ) ;
#84776 = CARTESIAN_POINT ( 'NONE',  ( 71.49814397558004941, 64.90871843161637855, 12.62364874555859551 ) ) ;
#84777 = CARTESIAN_POINT ( 'NONE',  ( 181.0877019475456962, 267.6761920141779569, 14.99829969603863944 ) ) ;
#84778 = CARTESIAN_POINT ( 'NONE',  ( -19.65312891409030271, 93.06504152958497400, 10.00000000000000888 ) ) ;
#84779 = CARTESIAN_POINT ( 'NONE',  ( 190.2648877593310317, 301.0985428348857340, -4.426259207433023590 ) ) ;
#84780 = CARTESIAN_POINT ( 'NONE',  ( 81.97090630940145672, 41.81567222034367859, -5.612609715771486485 ) ) ;
#84781 = CARTESIAN_POINT ( 'NONE',  ( 156.0916382163451601, 277.5285333452508212, -10.52960063827285886 ) ) ;
#84782 = CARTESIAN_POINT ( 'NONE',  ( 164.1065032853484240, 250.1265725945117140, 10.86380703882780452 ) ) ;
#84783 = ADVANCED_FACE ( 'NONE', ( #96553 ), #82361, .F. ) ;
#84784 = CARTESIAN_POINT ( 'NONE',  ( 99.88567928453477407, 235.1427522451419350, 10.00000000000009237 ) ) ;
#84785 = DIRECTION ( 'NONE',  ( -0.5000000000000012212, 0.8660254037844379305, -0.000000000000000000 ) ) ;
#84786 = ORIENTED_EDGE ( 'NONE', *, *, #74081, .T. ) ;
#84787 = CARTESIAN_POINT ( 'NONE',  ( 162.9796882977680639, 248.3578945969637743, 9.683801903336119565 ) ) ;
#84788 = CARTESIAN_POINT ( 'NONE',  ( 208.3699316049496133, 269.7396870210121733, -1.898463622294385811 ) ) ;
#84789 = CARTESIAN_POINT ( 'NONE',  ( 21.28450569914983248, 195.3464784336661637, 1.353441290958777327E-15 ) ) ;
#84790 = CARTESIAN_POINT ( 'NONE',  ( 11.88462290154380874, 22.56454794089040305, 10.00000000000000355 ) ) ;
#84791 = CARTESIAN_POINT ( 'NONE',  ( 192.3278524167367891, 272.0202382274233628, 14.20356147229779964 ) ) ;
#84792 = LINE ( 'NONE', #70546, #99885 ) ;
#84793 = PLANE ( 'NONE',  #86362 ) ;
#84795 = CARTESIAN_POINT ( 'NONE',  ( 68.80799682758592439, 210.5333772461660544, 9.188101187500095079 ) ) ;
#84794 = CARTESIAN_POINT ( 'NONE',  ( 198.2817570091511925, 277.3855417112700934, -15.35505783437617566 ) ) ;
#84796 = CARTESIAN_POINT ( 'NONE',  ( 161.1089126327036354, 251.5981730984191529, 13.95161017039218976 ) ) ;
#84797 = CARTESIAN_POINT ( 'NONE',  ( 72.75680339015909226, 57.15378132276418199, 15.89129174203703521 ) ) ;
#84798 = CARTESIAN_POINT ( 'NONE',  ( 45.49391910530875549, 208.6199935810940929, 2.679491924311251605 ) ) ;
#84799 = CARTESIAN_POINT ( 'NONE',  ( 16.09091216865756024, 14.45404122711132366, -8.090169943749478065 ) ) ;
#84800 = ORIENTED_EDGE ( 'NONE', *, *, #17566, .T. ) ;
#84801 = AXIS2_PLACEMENT_3D ( 'NONE', #61623, #6934, #54013 ) ;
#84802 = CARTESIAN_POINT ( 'NONE',  ( 3.125382611083808104, 182.6115022471903160, -5.000000000000047962 ) ) ;
#84803 = CARTESIAN_POINT ( 'NONE',  ( 208.1757572214753793, 270.0760069187178374, 2.172546422564154867 ) ) ;
#84804 = CARTESIAN_POINT ( 'NONE',  ( -8.674473839076844328, 174.9869531367911293, 4.594050593750046652 ) ) ;
#84805 = CARTESIAN_POINT ( 'NONE',  ( 35.63556891041371699, 26.28920272979929607, -7.433330006724141015 ) ) ;
#84806 = CARTESIAN_POINT ( 'NONE',  ( 166.6645348857815350, 262.0116583737346900, -16.28251305985784114 ) ) ;
#84807 = CARTESIAN_POINT ( 'NONE',  ( 189.0517344710061138, 261.8661741762242059, 6.550959291050514999 ) ) ;
#84808 = CARTESIAN_POINT ( 'NONE',  ( 206.0041637419966776, 273.8373171585603814, 11.66586596407113596 ) ) ;
#84809 = VECTOR ( 'NONE', #86119, 1000.000000000000114 ) ;
#84811 = CARTESIAN_POINT ( 'NONE',  ( 185.3943831185000874, 277.6506735163841313, -17.55462980397184580 ) ) ;
#84810 = CARTESIAN_POINT ( 'NONE',  ( 41.54267820409027934, 208.0707943907112849, -17.97570218321537894 ) ) ;
#84812 = CARTESIAN_POINT ( 'NONE',  ( 68.52700701264937777, 64.29941490235316337, 12.37827088797565978 ) ) ;
#84813 = ORIENTED_EDGE ( 'NONE', *, *, #16877, .F. ) ;
#84814 = CARTESIAN_POINT ( 'NONE',  ( 80.22679522040971278, 47.49802419697316225, 13.74028476495392681 ) ) ;
#84815 = CARTESIAN_POINT ( 'NONE',  ( 208.3303207624000777, 269.8082950128387552, -0.5527213369959232958 ) ) ;
#84816 = EDGE_CURVE ( 'NONE', #17862, #18980, #42170, .T. ) ;
#84817 = CARTESIAN_POINT ( 'NONE',  ( 177.9378665411170743, 286.3192117283503535, 13.07754552029243733 ) ) ;
#84818 = DIRECTION ( 'NONE',  ( -0.8660254037844387076, -0.4999999999999998890, -0.000000000000000000 ) ) ;
#84819 = CARTESIAN_POINT ( 'NONE',  ( 5.211622267866312441, 23.98502408145590081, -5.678558825948271327 ) ) ;
#84820 = ORIENTED_EDGE ( 'NONE', *, *, #83952, .T. ) ;
#84821 = CARTESIAN_POINT ( 'NONE',  ( 206.6055738272482927, 272.7956443347203503, 9.336287257528914196 ) ) ;
#84822 = CARTESIAN_POINT ( 'NONE',  ( -6.563276597302431625, 157.0177522451417929, 5.000000000000051514 ) ) ;
#84823 = CARTESIAN_POINT ( 'NONE',  ( 69.93840568465007834, 62.63376372532634662, 13.43677035550434873 ) ) ;
#84824 = DIRECTION ( 'NONE',  ( -0.8660254037844387076, -0.4999999999999998890, -0.000000000000000000 ) ) ;
#84825 = CARTESIAN_POINT ( 'NONE',  ( 191.1092559216791074, 295.6699157252775194, 12.62328014874510274 ) ) ;
#84826 = CYLINDRICAL_SURFACE ( 'NONE', #36405, 70.00000000000002842 ) ;
#84827 = CARTESIAN_POINT ( 'NONE',  ( 162.7070706717508699, 248.8300821762643693, -9.986337079333621247 ) ) ;
#84828 = CARTESIAN_POINT ( 'NONE',  ( 153.2513309553138470, 265.2079037882803618, -16.24091495603130397 ) ) ;
#84829 =( BOUNDED_CURVE ( )  B_SPLINE_CURVE ( 2, ( #65078, #96028, #49878, #47857, #11408, #71200, #42261, #73196, #34671 ),
 .UNSPECIFIED., .F., .T. ) 
 B_SPLINE_CURVE_WITH_KNOTS ( ( 3, 2, 2, 2, 3 ),
 ( 0.5362903225806451291, 0.5376344086021505042, 0.5403225806451612545, 0.5430107526881720048, 0.5443548387096773800 ),
 .UNSPECIFIED. ) 
 CURVE ( )  GEOMETRIC_REPRESENTATION_ITEM ( )  RATIONAL_B_SPLINE_CURVE ( ( 0.9330127018922194093, 0.9330127018922194093, 1.000000000000000000, 0.8660254037844387076, 1.000000000000000000, 0.8660254037844387076, 1.000000000000000000, 0.9330127018922194093, 0.9330127018922194093 ) ) 
 REPRESENTATION_ITEM ( '' )  );
#84830 = ORIENTED_EDGE ( 'NONE', *, *, #62519, .T. ) ;
#84831 = CARTESIAN_POINT ( 'NONE',  ( 190.8753273331982427, 280.9408420453412987, 16.64646941022040849 ) ) ;
#84832 = CARTESIAN_POINT ( 'NONE',  ( 190.0656191383575333, 292.0158714553608661, 14.79701615165662254 ) ) ;
#84833 = VERTEX_POINT ( 'NONE', #97530 ) ;
#84834 = CARTESIAN_POINT ( 'NONE',  ( 148.9230895364621574, 272.7046378331555161, 12.20434325797056019 ) ) ;
#84835 = CARTESIAN_POINT ( 'NONE',  ( 26.39431744575845684, 16.20801979619929156, -3.090169943749474069 ) ) ;
#84836 = CARTESIAN_POINT ( 'NONE',  ( 190.2248117571934642, 297.8128940847054196, 8.178623448509318550 ) ) ;
#84837 = VERTEX_POINT ( 'NONE', #80867 ) ;
#84838 = CARTESIAN_POINT ( 'NONE',  ( 146.5865263025993954, 276.7516840693029962, 0.4918294119671828835 ) ) ;
#84839 = CARTESIAN_POINT ( 'NONE',  ( 79.29174861055801671, 59.84975646172946995, -16.14905532231970042 ) ) ;
#84840 = CARTESIAN_POINT ( 'NONE',  ( 197.0184425104562820, 289.4010428742387262, -16.90752553128928426 ) ) ;
#84841 = DIRECTION ( 'NONE',  ( -1.000000000000000000, 0.000000000000000000, 0.000000000000000000 ) ) ;
#84842 = CARTESIAN_POINT ( 'NONE',  ( 69.75455253191417171, 62.54871372033364452, 13.42486103269802911 ) ) ;
#84843 = ORIENTED_EDGE ( 'NONE', *, *, #26826, .F. ) ;
#84844 = CARTESIAN_POINT ( 'NONE',  ( 107.7791399978856930, 233.0333772461660828, 9.188101187500095079 ) ) ;
#84845 = DIRECTION ( 'NONE',  ( 1.000000000000000000, 0.000000000000000000, 0.000000000000000000 ) ) ;
#84846 = CARTESIAN_POINT ( 'NONE',  ( 190.7851866479434761, 300.1973587246873194, 7.931162401707728016 ) ) ;
#84847 = CARTESIAN_POINT ( 'NONE',  ( 81.61705240089096947, 42.28877732484014729, -8.032517907699986637 ) ) ;
#84848 = EDGE_LOOP ( 'NONE', ( #39179, #496, #60244, #55607, #60003, #82795, #16136, #28396 ) ) ;
#84849 = VERTEX_POINT ( 'NONE', #27625 ) ;
#84850 = ORIENTED_EDGE ( 'NONE', *, *, #34910, .T. ) ;
#84851 = CARTESIAN_POINT ( 'NONE',  ( 74.29311029226887797, 65.49125867801090806, 13.36500919525239972 ) ) ;
#84852 = EDGE_LOOP ( 'NONE', ( #60459, #6744, #38449, #32329 ) ) ;
#84853 = CARTESIAN_POINT ( 'NONE',  ( 71.26884625214724167, 71.79727854084720207, 1.363308781743589604 ) ) ;
#84854 = ORIENTED_EDGE ( 'NONE', *, *, #79545, .F. ) ;
#84855 = CARTESIAN_POINT ( 'NONE',  ( 207.6590484093196096, 270.9709728340903894, 3.402057849327809524 ) ) ;
#84856 = DIRECTION ( 'NONE',  ( -0.4924038765061016787, 0.8528685319524424990, -0.1736481776669404342 ) ) ;
#84857 = CARTESIAN_POINT ( 'NONE',  ( 165.8975677354378035, 271.5909624305264174, 17.28637137770206067 ) ) ;
#84858 = CARTESIAN_POINT ( 'NONE',  ( 168.1505686650465350, 281.2677474040732477, 11.64546357986301750 ) ) ;
#84859 = CARTESIAN_POINT ( 'NONE',  ( 148.3874010092782498, 273.6324775792697892, -8.328854486678444857 ) ) ;
#84860 = B_SPLINE_CURVE_WITH_KNOTS ( 'NONE', 3,
 ( #44545, #89722, #75479, #82121, #12694, #36455, #67358, #98286, #6063, #36957, #67868, #29372, #60238, #91199, #73486, #52646, #83601, #4070, #330, #85481, #54503, #32725, #71753, #46930, #6571, #38818, #2346, #77847, #8931, #47913, #75994 ),
 .UNSPECIFIED., .F., .F.,
 ( 4, 3, 3, 3, 3, 3, 3, 3, 3, 3, 4 ),
 ( 0.000000000000000000, 0.1333490885032341255, 0.3007194338854348725, 0.4699862290245032659, 0.5844252810809253962, 0.6686540514502775645, 0.7354980260655532565, 0.8028463152565672445, 0.8633854507757174890, 0.9437142632667334663, 1.000000000000000000 ),
 .UNSPECIFIED. ) ;
#84861 = FACE_OUTER_BOUND ( 'NONE', #33626, .T. ) ;
#84862 = VERTEX_POINT ( 'NONE', #36685 ) ;
#84863 = CARTESIAN_POINT ( 'NONE',  ( 166.9825626143087050, 247.0767275159285816, 1.933851161157992271 ) ) ;
#84864 = CARTESIAN_POINT ( 'NONE',  ( 11.44039960990914651, 28.64646525600389282, -2.839279412974133887 ) ) ;
#84865 = CARTESIAN_POINT ( 'NONE',  ( 201.9679975669502312, 279.1647446829476280, -15.96203686199545579 ) ) ;
#84866 = DIRECTION ( 'NONE',  ( 0.000000000000000000, -0.000000000000000000, -1.000000000000000000 ) ) ;
#84868 = ORIENTED_EDGE ( 'NONE', *, *, #74536, .T. ) ;
#84867 = CARTESIAN_POINT ( 'NONE',  ( 115.9793180381955580, 247.7677522451419065, -5.000000000000047962 ) ) ;
#84869 = CARTESIAN_POINT ( 'NONE',  ( 202.6070187115982719, 279.7213449518906145, 15.56322169823762280 ) ) ;
#84870 = CARTESIAN_POINT ( 'NONE',  ( 206.1408608592916494, 273.6005508061571732, -10.42739367433323494 ) ) ;
#84871 = CARTESIAN_POINT ( 'NONE',  ( 79.73452763708452551, 44.91547317212032198, 11.49829713998203040 ) ) ;
#84872 = ADVANCED_FACE ( 'NONE', ( #5800 ), #36188, .F. ) ;
#84873 = CARTESIAN_POINT ( 'NONE',  ( 67.73992565572970648, 65.91850390810078864, -10.49939607295521959 ) ) ;
#84874 = TOROIDAL_SURFACE ( 'NONE', #24953, 15.10714546451156970, 0.5000000000000000000 ) ;
#84875 = CARTESIAN_POINT ( 'NONE',  ( 161.3227470381586102, 251.2278010437646856, 14.45097375514160731 ) ) ;
#84876 = EDGE_CURVE ( 'NONE', #15552, #43154, #90457, .T. ) ;
#84877 = CARTESIAN_POINT ( 'NONE',  ( 194.1200050480437653, 262.3566822754066834, -0.8120440885529029984 ) ) ;
#84878 = ORIENTED_EDGE ( 'NONE', *, *, #79291, .F. ) ;
#84879 = CARTESIAN_POINT ( 'NONE',  ( 155.0719444836497871, 262.0545086562551091, -18.28771400695536187 ) ) ;
#84880 = CARTESIAN_POINT ( 'NONE',  ( 75.03626624455306171, 62.25040173119386111, -15.04310718129558211 ) ) ;
#84881 = CARTESIAN_POINT ( 'NONE',  ( 174.8696466734779449, 292.3029143586743430, -1.153856708368909967 ) ) ;
#84882 = ADVANCED_FACE ( 'NONE', ( #4822 ), #42293, .T. ) ;
#84883 = CARTESIAN_POINT ( 'NONE',  ( 11.62325688217078223, 167.5177522451418213, 5.000000000000051514 ) ) ;
#84884 = CARTESIAN_POINT ( 'NONE',  ( 192.7752508616301839, 267.0407549221993690, -11.17594988838974501 ) ) ;
#84885 = FACE_OUTER_BOUND ( 'NONE', #1958, .T. ) ;
#84886 = CARTESIAN_POINT ( 'NONE',  ( 169.9163657913202314, 280.6881826668949316, -14.21246854472871490 ) ) ;
#84887 = CARTESIAN_POINT ( 'NONE',  ( 72.96752522106987726, 70.88037482455226268, 8.005050465142893756 ) ) ;
#84889 = CARTESIAN_POINT ( 'NONE',  ( 114.8426596992765099, 227.1115022471901739, -5.000000000000041744 ) ) ;
#84888 = CARTESIAN_POINT ( 'NONE',  ( 6.913983429043053519, 183.9869531367911009, 4.594050593750046652 ) ) ;
#84890 = CARTESIAN_POINT ( 'NONE',  ( 65.88310562893971678, 69.02589174555536999, 1.996831191813055240 ) ) ;
#84891 = ORIENTED_EDGE ( 'NONE', *, *, #71482, .T. ) ;
#84892 = ORIENTED_EDGE ( 'NONE', *, *, #45017, .T. ) ;
#84893 = CARTESIAN_POINT ( 'NONE',  ( 128.2864073861747727, 233.3262482093457493, 3.021315404115420679E-15 ) ) ;
#84894 = B_SPLINE_CURVE_WITH_KNOTS ( 'NONE', 3,
 ( #770, #62553, #31163, #47368, #61064, #31656, #7889, #76304, #69670, #30176, #276, #38766, #14491, #92033, #83927, #91515, #37278, #85945, #7370, #45854, #16473, #62052, #76777, #99102, #45371, #29686, #22082, #54448, #6876, #85425, #46874, #38255, #23061, #84913, #30685, #61565, #92513, #53956, #15456, #9381, #25070, #24569, #55948, #39742, #49378, #17995, #86944, #40756, #78291, #26589 ),
 .UNSPECIFIED., .F., .F.,
 ( 4, 2, 2, 2, 2, 2, 2, 2, 2, 2, 2, 2, 2, 2, 2, 2, 2, 2, 2, 2, 2, 2, 2, 2, 4 ),
 ( 0.0001377106324937234195, 0.001145886038797477424, 0.001397929890373450328, 0.001649973741949423232, 0.001775995667737409684, 0.001902017593525396136, 0.002028039519313382371, 0.002154061445101369040, 0.002406105296677414802, 0.002658149148253460565, 0.003162236851405497012, 0.004170412257709569907, 0.005178587664013642802, 0.005682675367165642387, 0.005934719218741604449, 0.006060741144529589383, 0.006186763070317573450, 0.006249774033211555509, 0.006312784996105537567, 0.006438806921893589288, 0.006690850773469821100, 0.007194938476622280386, 0.007699026179774738805, 0.007951070031351023526, 0.008203113882927307379 ),
 .UNSPECIFIED. ) ;
#84895 = DIRECTION ( 'NONE',  ( -0.000000000000000000, -0.000000000000000000, -1.000000000000000000 ) ) ;
#84896 = CARTESIAN_POINT ( 'NONE',  ( 84.82746753971869680, 42.25127123179836985, 0.4482709252177607961 ) ) ;
#84897 = CARTESIAN_POINT ( 'NONE',  ( 201.9545259124544145, 280.8514956315805193, -16.42775064268253615 ) ) ;
#84898 = CARTESIAN_POINT ( 'NONE',  ( 83.07807837777205862, 43.85925945439043971, 8.248572388415514212 ) ) ;
#84899 = CARTESIAN_POINT ( 'NONE',  ( 149.8380350131166949, 277.0589241956989781, 3.095230065015505350 ) ) ;
#84900 = CARTESIAN_POINT ( 'NONE',  ( 16.57566611395445477, 186.5024278399160949, 9.188101187500095079 ) ) ;
#84901 = CARTESIAN_POINT ( 'NONE',  ( 117.0621101165238542, 229.2048013555409796, 4.594050593750051981 ) ) ;
#84902 = CARTESIAN_POINT ( 'NONE',  ( 178.9043521614821941, 291.7907940003793783, -6.168293200034719703 ) ) ;
#84903 = CARTESIAN_POINT ( 'NONE',  ( 195.8788359694280814, 275.2028430888133812, 15.68988939746534328 ) ) ;
#84904 = CARTESIAN_POINT ( 'NONE',  ( 34.75566377745538205, 179.3262482093457493, 3.021315404115420679E-15 ) ) ;
#84905 = CARTESIAN_POINT ( 'NONE',  ( 177.8872019327756959, 273.7990604926155811, -17.82423047383818471 ) ) ;
#84906 = CARTESIAN_POINT ( 'NONE',  ( -7.835251407336910390, 166.2833772461660828, -9.188101187500095079 ) ) ;
#84907 = DIRECTION ( 'NONE',  ( 1.000000000000000000, 0.000000000000000000, 0.000000000000000000 ) ) ;
#84908 = CARTESIAN_POINT ( 'NONE',  ( 155.6126298223767890, 261.1180141786725244, 18.15400560664037855 ) ) ;
#84909 = CARTESIAN_POINT ( 'NONE',  ( 161.8935665241663457, 250.2391126920490194, -13.69501063978231770 ) ) ;
#84910 = CARTESIAN_POINT ( 'NONE',  ( 83.14218550195334956, 50.27791214501019113, 14.33927766777896906 ) ) ;
#84911 = DIRECTION ( 'NONE',  ( 0.5000000000000003331, -0.8660254037844385966, 8.877441173312408730E-15 ) ) ;
#84912 = CARTESIAN_POINT ( 'NONE',  ( 72.62777135225290692, 66.58284297640395266, 12.45031013499460038 ) ) ;
#84913 = CARTESIAN_POINT ( 'NONE',  ( 171.4787937661881756, 279.8757557646238183, 13.90305814568919018 ) ) ;
#84914 = CARTESIAN_POINT ( 'NONE',  ( 174.5508403973756515, 260.3590064504865040, -14.93617697178709314 ) ) ;
#84915 = CARTESIAN_POINT ( 'NONE',  ( 69.26629474405157794, 69.23362429141876362, 6.083831639397693891 ) ) ;
#84916 = CARTESIAN_POINT ( 'NONE',  ( 147.8465295590381743, 274.5692944114487091, 9.322947948439978205 ) ) ;
#84917 = CARTESIAN_POINT ( 'NONE',  ( 181.4235159426282564, 267.2807182867468327, -14.77487836696800194 ) ) ;
#84918 = VERTEX_POINT ( 'NONE', #43790 ) ;
#84919 = CARTESIAN_POINT ( 'NONE',  ( 74.69795600089807408, 60.20801014145679630, 16.00524392222005332 ) ) ;
#84920 = CARTESIAN_POINT ( 'NONE',  ( 81.98204644731730184, 41.14170830008083612, -5.380964918418897902 ) ) ;
#84921 = CARTESIAN_POINT ( 'NONE',  ( 94.51795245455393513, 231.5024278399160949, 9.188101187500095079 ) ) ;
#84922 = CARTESIAN_POINT ( 'NONE',  ( 15.62556418158687244, 11.94754757982088123, 5.678558825948272215 ) ) ;
#84923 = CARTESIAN_POINT ( 'NONE',  ( 151.3560786774222322, 268.4905770267490652, 15.54402364351346932 ) ) ;
#84924 = CARTESIAN_POINT ( 'NONE',  ( 40.37736971981244238, 56.55791953817036699, -10.00000000000000000 ) ) ;
#84926 = CARTESIAN_POINT ( 'NONE',  ( 195.1427698080798336, 279.1118193537853927, 16.30781815010357860 ) ) ;
#84925 = CARTESIAN_POINT ( 'NONE',  ( 14.19121639173650706, 20.14441083166259716, 10.00000000000000533 ) ) ;
#84927 = CARTESIAN_POINT ( 'NONE',  ( 201.1614673384707714, 270.3972314152816807, -10.08402632729127646 ) ) ;
#84928 = CYLINDRICAL_SURFACE ( 'NONE', #48734, 10.00000000000010658 ) ;
#84929 = CARTESIAN_POINT ( 'NONE',  ( 149.7819113862974802, 271.9648479771055918, -11.46454315534134238 ) ) ;
#84930 = EDGE_CURVE ( 'NONE', #28329, #96454, #20487, .T. ) ;
#84931 = CARTESIAN_POINT ( 'NONE',  ( 29.12701137275935181, 44.61184105132205957, -10.00000000000000000 ) ) ;
#84932 = FACE_OUTER_BOUND ( 'NONE', #66656, .T. ) ;
#84933 = CARTESIAN_POINT ( 'NONE',  ( 86.47816187992320636, 47.39707827577768029, 10.33711315380114115 ) ) ;
#84934 = ORIENTED_EDGE ( 'NONE', *, *, #2646, .F. ) ;
#84935 = CARTESIAN_POINT ( 'NONE',  ( 23.65314546706850862, 31.84336893147757408, -7.433330006724137462 ) ) ;
#84936 = CARTESIAN_POINT ( 'NONE',  ( 72.71768624772042244, 63.97145380353339306, -14.16538725607713012 ) ) ;
#84937 = CARTESIAN_POINT ( 'NONE',  ( 196.5898038174904343, 267.5261605945568135, 9.655523290058249941 ) ) ;
#84938 = CARTESIAN_POINT ( 'NONE',  ( 149.6191398986701415, 271.4990432411842676, -11.66821883946526839 ) ) ;
#84939 = ORIENTED_EDGE ( 'NONE', *, *, #21239, .F. ) ;
#84940 = CARTESIAN_POINT ( 'NONE',  ( 84.82070890866113189, 50.11195492342548619, -13.71672402108478295 ) ) ;
#84941 = CARTESIAN_POINT ( 'NONE',  ( 83.87686851671099930, 42.61110357726119702, 6.252421602106308818 ) ) ;
#84942 = VECTOR ( 'NONE', #58687, 1000.000000000000227 ) ;
#84944 = ADVANCED_FACE ( 'NONE', ( #53386 ), #60978, .T. ) ;
#84943 = CARTESIAN_POINT ( 'NONE',  ( 182.3700640764176342, 263.2847133751610045, -13.94439451147478337 ) ) ;
#84945 = LINE ( 'NONE', #53500, #45246 ) ;
#84946 = CARTESIAN_POINT ( 'NONE',  ( 152.6757560589063303, 266.2048287524194166, 16.73757896668104195 ) ) ;
#84947 = ORIENTED_EDGE ( 'NONE', *, *, #77158, .T. ) ;
#84948 = CARTESIAN_POINT ( 'NONE',  ( 187.5265405544104453, 278.9627198005699711, 16.98281552316259280 ) ) ;
#84949 = CARTESIAN_POINT ( 'NONE',  ( 36.63328578856461348, 23.01110640527294748, 2.839279412974134775 ) ) ;
#84950 = ORIENTED_EDGE ( 'NONE', *, *, #96210, .T. ) ;
#84951 = CARTESIAN_POINT ( 'NONE',  ( 167.5733308811266227, 249.8690179723528217, 6.942995308039366265 ) ) ;
#84952 = EDGE_CURVE ( 'NONE', #38602, #17814, #195, .T. ) ;
#84953 = LINE ( 'NONE', #25106, #58048 ) ;
#84955 = ORIENTED_EDGE ( 'NONE', *, *, #68907, .T. ) ;
#84954 = AXIS2_PLACEMENT_3D ( 'NONE', #61877, #46693, #31984 ) ;
#84956 = CARTESIAN_POINT ( 'NONE',  ( 86.51235478091771824, 47.18193832426288736, -10.10603714529630537 ) ) ;
#84957 = CARTESIAN_POINT ( 'NONE',  ( 158.7690100866489900, 256.4985079616176336, 16.45054074394984056 ) ) ;
#84958 = CARTESIAN_POINT ( 'NONE',  ( 84.54065070028998718, 50.22889876405420040, 13.87834917160721737 ) ) ;
#84959 = CARTESIAN_POINT ( 'NONE',  ( 192.8895823079093077, 296.5524385223993136, -11.97278429023368496 ) ) ;
#84960 = CARTESIAN_POINT ( 'NONE',  ( 179.9209375999747351, 276.5811748711908535, 17.74520275588677265 ) ) ;
#84961 = LINE ( 'NONE', #85475, #29190 ) ;
#84962 = CARTESIAN_POINT ( 'NONE',  ( 81.60881798005151211, 55.57634303931474307, -16.32954282162994275 ) ) ;
#84963 = CARTESIAN_POINT ( 'NONE',  ( 71.79755147005840854, 63.53309442284064801, -14.10203765313787017 ) ) ;
#84964 = ORIENTED_EDGE ( 'NONE', *, *, #17958, .F. ) ;
#84965 = CARTESIAN_POINT ( 'NONE',  ( 196.1370092075112268, 290.1209220278959720, 16.40156295354631411 ) ) ;
#84966 = ORIENTED_EDGE ( 'NONE', *, *, #6347, .F. ) ;
#84967 = VERTEX_POINT ( 'NONE', #15882 ) ;
#84968 = CARTESIAN_POINT ( 'NONE',  ( 169.4056471164851132, 269.1093820582442504, 17.36518709487519629 ) ) ;
#84969 = ORIENTED_EDGE ( 'NONE', *, *, #44193, .T. ) ;
#84970 = CARTESIAN_POINT ( 'NONE',  ( 164.4679336850620075, 246.2674076979392339, 2.485468002151889344 ) ) ;
#84971 = CARTESIAN_POINT ( 'NONE',  ( 205.9252530167937323, 273.9739945438741984, -10.37964514155334328 ) ) ;
#84972 = CARTESIAN_POINT ( 'NONE',  ( 199.7100744728227539, 274.3991700604664175, -13.57366607680039294 ) ) ;
#84973 = DIRECTION ( 'NONE',  ( -0.4999999999999987788, 0.8660254037844392627, 0.000000000000000000 ) ) ;
#84974 = CARTESIAN_POINT ( 'NONE',  ( 192.6247335881259630, 297.0111699613833594, -13.30158778996737290 ) ) ;
#84975 = CARTESIAN_POINT ( 'NONE',  ( 171.5508816557387206, 250.5181571520007537, -5.758755346447887113 ) ) ;
#84976 = CARTESIAN_POINT ( 'NONE',  ( 78.44203751522360335, 61.21016990572091032, 16.24725970467587999 ) ) ;
#84977 = CARTESIAN_POINT ( 'NONE',  ( 186.7062459033451489, 286.9011594067970350, -15.58169422348589350 ) ) ;
#84978 = CARTESIAN_POINT ( 'NONE',  ( 117.8466853168797428, 238.8458772461660544, 9.188101187500095079 ) ) ;
#84979 = CARTESIAN_POINT ( 'NONE',  ( 70.39799145693270077, 61.05877478468345743, -14.90226077307323393 ) ) ;
#84980 = CARTESIAN_POINT ( 'NONE',  ( 37.26657704017246431, 36.91421378149922816, 9.188101187500008038 ) ) ;
#84981 = CARTESIAN_POINT ( 'NONE',  ( 179.1400961457673304, 290.0475676899061455, -9.404149003805263973 ) ) ;
#84982 = ORIENTED_EDGE ( 'NONE', *, *, #76953, .F. ) ;
#84983 = VECTOR ( 'NONE', #70702, 1000.000000000000114 ) ;
#84984 = CARTESIAN_POINT ( 'NONE',  ( 73.86461842229320496, 68.29997319365683950, -11.61748300246921417 ) ) ;
#84985 = EDGE_CURVE ( 'NONE', #55984, #83319, #68723, .T. ) ;
#84986 = CARTESIAN_POINT ( 'NONE',  ( 74.72625485415514390, 63.07837140537560572, -14.64344360945962720 ) ) ;
#84987 = CARTESIAN_POINT ( 'NONE',  ( 17.26055046206296950, 33.28368158147418399, -10.00000000000000000 ) ) ;
#84988 = CARTESIAN_POINT ( 'NONE',  ( 146.7445232850756156, 276.4780252682116384, 2.895314788918020632 ) ) ;
#84989 = CARTESIAN_POINT ( 'NONE',  ( 73.55883212634472557, 67.59623184424712861, 11.56650193424350093 ) ) ;
#84990 = CARTESIAN_POINT ( 'NONE',  ( 153.3506059258413643, 265.0359544954067132, -16.39100908615009899 ) ) ;
#84991 = CARTESIAN_POINT ( 'NONE',  ( 20.69167212271446488, 17.11029122506294087, -8.090169943749478065 ) ) ;
#84992 = VERTEX_POINT ( 'NONE', #21993 ) ;
#84993 = CARTESIAN_POINT ( 'NONE',  ( 147.9909379325378609, 274.3191717715091045, 10.08496620488601181 ) ) ;
#84994 = ORIENTED_EDGE ( 'NONE', *, *, #55658, .T. ) ;
#84995 = CARTESIAN_POINT ( 'NONE',  ( 148.0826818691893152, 274.1602666119424043, -9.371267383421741926 ) ) ;
#84996 = DIRECTION ( 'NONE',  ( -0.000000000000000000, -0.000000000000000000, 1.000000000000000000 ) ) ;
#84997 = ORIENTED_EDGE ( 'NONE', *, *, #43100, .T. ) ;
#84998 = CARTESIAN_POINT ( 'NONE',  ( 188.0217698280969501, 266.1369699381889973, -11.79292520403407885 ) ) ;
#84999 = EDGE_CURVE ( 'NONE', #92184, #1733, #76694, .T. ) ;
#85000 = ADVANCED_FACE ( 'NONE', ( #83840 ), #13899, .F. ) ;
#85001 = CARTESIAN_POINT ( 'NONE',  ( 159.0065368070590353, 277.8476692937898065, 10.29608560019760155 ) ) ;
#85002 = CARTESIAN_POINT ( 'NONE',  ( 196.1341231099717959, 264.6386869773598960, 3.834808299373879237 ) ) ;
#85003 = CARTESIAN_POINT ( 'NONE',  ( 158.3858271822887218, 263.3851922276277833, 17.76837769191611116 ) ) ;
#85004 = CARTESIAN_POINT ( 'NONE',  ( 29.42114147039228200, 17.39040679176983772, 1.333680081654574804E-15 ) ) ;
#85006 = CARTESIAN_POINT ( 'NONE',  ( 69.76254693980804689, 63.15031056092325201, -13.65041900308473366 ) ) ;
#85005 = LINE ( 'NONE', #98704, #25821 ) ;
#85007 = CARTESIAN_POINT ( 'NONE',  ( 152.8651171364917900, 265.8768457450651113, -16.25664868183201861 ) ) ;
#85008 = ORIENTED_EDGE ( 'NONE', *, *, #79193, .F. ) ;
#85009 = CARTESIAN_POINT ( 'NONE',  ( 190.7403173041394950, 300.2750747078583800, -4.254144485856557800 ) ) ;
#85010 = FACE_OUTER_BOUND ( 'NONE', #40091, .T. ) ;
#85011 = CARTESIAN_POINT ( 'NONE',  ( 186.7460619612521953, 262.7540144476575961, -8.976403499855448942 ) ) ;
#85012 = DIRECTION ( 'NONE',  ( 0.05364311403569549386, 0.9985601716053735810, 0.000000000000000000 ) ) ;
#85013 = CARTESIAN_POINT ( 'NONE',  ( -41.73592930317598615, 44.85821161687699998, 59.99999999999999289 ) ) ;
#85014 = CARTESIAN_POINT ( 'NONE',  ( 189.0314999406332959, 269.9387407235815886, -14.02374420418258794 ) ) ;
#85015 = CARTESIAN_POINT ( 'NONE',  ( 188.5113832660517232, 298.5244903283103781, -4.265124716804361782 ) ) ;
#85016 = AXIS2_PLACEMENT_3D ( 'NONE', #36083, #18929, #11336 ) ;
#85017 = CARTESIAN_POINT ( 'NONE',  ( 82.95985630027486479, 42.92152901241345830, 6.769544279123342001 ) ) ;
#85018 = LINE ( 'NONE', #85537, #20385 ) ;
#85019 = CARTESIAN_POINT ( 'NONE',  ( 70.38723355792234315, 61.09782911607875633, -14.88300479815616484 ) ) ;
#85020 = CARTESIAN_POINT ( 'NONE',  ( 70.84106301243626547, 70.60106795950503056, -5.124797883556153621 ) ) ;
#85021 = CARTESIAN_POINT ( 'NONE',  ( 79.63366147065640632, 204.5327760586659451, 1.948934522072303157E-15 ) ) ;
#85022 = CARTESIAN_POINT ( 'NONE',  ( 66.47763888060634940, 67.99612994687967671, 6.463816603905435443 ) ) ;
#85023 = CARTESIAN_POINT ( 'NONE',  ( 41.25821923120311396, 128.0827283385945918, -10.00000000000000000 ) ) ;
#85024 = CARTESIAN_POINT ( 'NONE',  ( 49.55341318909624704, 210.9637435831424739, 2.679491924311251605 ) ) ;
#85025 = CARTESIAN_POINT ( 'NONE',  ( 203.1526193585190470, 278.7763369107815379, -16.67658907091021447 ) ) ;
#85026 = CARTESIAN_POINT ( 'NONE',  ( 207.8984236726843164, 270.5563627158673512, -6.084369154771423815 ) ) ;
#85027 = CARTESIAN_POINT ( 'NONE',  ( 84.84691229513632038, 49.95470102045879912, -13.19661209231484378 ) ) ;
#85028 = CARTESIAN_POINT ( 'NONE',  ( 40.12992642340848448, 200.6427522451419065, 10.00000000000009415 ) ) ;
#85030 = CARTESIAN_POINT ( 'NONE',  ( 75.84045651381646280, 51.64986437825746179, 15.74133474855197257 ) ) ;
#85029 = CARTESIAN_POINT ( 'NONE',  ( 73.22483582419529569, 69.61542381504622767, -9.909891866396675297 ) ) ;
#85031 = DIRECTION ( 'NONE',  ( -0.8660254037844392627, -0.4999999999999987232, 0.000000000000000000 ) ) ;
#85032 = CARTESIAN_POINT ( 'NONE',  ( 169.1058430229814462, 251.9997932694548126, -8.779696520905575952 ) ) ;
#85033 = CARTESIAN_POINT ( 'NONE',  ( 163.9708803696611028, 246.6410995683858118, -5.146160866179791071 ) ) ;
#85034 = CARTESIAN_POINT ( 'NONE',  ( 157.2168982216852555, 258.3393398020932636, 18.09635675623264106 ) ) ;
#85035 = CARTESIAN_POINT ( 'NONE',  ( 190.2244606332360490, 298.9447751924984118, -8.130533059491476422 ) ) ;
#85036 = CARTESIAN_POINT ( 'NONE',  ( 161.6923300915171922, 250.5876644177310482, -14.43081872899884566 ) ) ;
#85037 = CARTESIAN_POINT ( 'NONE',  ( 19.79611131033658111, 191.4244531367911293, -4.594050593750046652 ) ) ;
#85038 = CARTESIAN_POINT ( 'NONE',  ( 52.86797706100236383, 192.1423013555410080, -4.594050593750043987 ) ) ;
#85039 = CARTESIAN_POINT ( 'NONE',  ( 164.1964637989676987, 247.2500284144306022, -6.878198590015258240 ) ) ;
#85040 = CARTESIAN_POINT ( 'NONE',  ( 87.91358676412336592, 43.93313586519735736, 0.4560764699024720814 ) ) ;
#85041 = CARTESIAN_POINT ( 'NONE',  ( 83.14106290878449101, 49.68186538430950350, -13.54780265075754286 ) ) ;
#85042 = CARTESIAN_POINT ( 'NONE',  ( -4.163664537435148638, 161.7365022471902023, 10.00000000000009592 ) ) ;
#85043 = CARTESIAN_POINT ( 'NONE',  ( -42.47074677134371257, 28.21475011077167139, -10.00000000000000000 ) ) ;
#85044 = CARTESIAN_POINT ( 'NONE',  ( 23.01796646339240837, 172.5494855054051868, -2.679491924311248496 ) ) ;
#85046 = EDGE_CURVE ( 'NONE', #68592, #17528, #14405, .T. ) ;
#85045 = CIRCLE ( 'NONE', #54252, 14.21260523776213347 ) ;
#85047 = CARTESIAN_POINT ( 'NONE',  ( 18.53877768333399345, 26.10171378149918198, 9.188101187500008038 ) ) ;
#85048 = CARTESIAN_POINT ( 'NONE',  ( 197.0121621852902933, 287.4119207165142029, 17.64812647472269092 ) ) ;
#85049 = CARTESIAN_POINT ( 'NONE',  ( -78.10577900106846982, 54.55156729251706338, 10.00000000000000000 ) ) ;
#85050 = CARTESIAN_POINT ( 'NONE',  ( 12.32384911305235420, 19.06628583063839955, -9.188101187500006262 ) ) ;
#85051 = CARTESIAN_POINT ( 'NONE',  ( 57.82012596918833935, 210.3149278399160949, 9.188101187500093303 ) ) ;
#85052 = LINE ( 'NONE', #76909, #28679 ) ;
#85053 = FACE_OUTER_BOUND ( 'NONE', #60023, .T. ) ;
#85054 = CARTESIAN_POINT ( 'NONE',  ( 159.4285914931787431, 254.5085746851079023, 15.41072477910873673 ) ) ;
#85055 = CARTESIAN_POINT ( 'NONE',  ( 74.39841895140679640, 68.21392270468032848, 11.45628786500076579 ) ) ;
#85056 = CARTESIAN_POINT ( 'NONE',  ( 149.2964064632859049, 275.3583832525684443, 7.516923408081652269 ) ) ;
#85057 = EDGE_CURVE ( 'NONE', #68820, #44309, #47050, .T. ) ;
#85058 = VECTOR ( 'NONE', #64914, 1000.000000000000114 ) ;
#85059 = CARTESIAN_POINT ( 'NONE',  ( 80.00137380443280222, 55.11996643375317717, -15.99434914381717832 ) ) ;
#85060 = CARTESIAN_POINT ( 'NONE',  ( 116.0695290213044757, 224.4865022471901455, 1.119607411625061291E-15 ) ) ;
#85061 = LINE ( 'NONE', #69819, #50697 ) ;
#85062 = CARTESIAN_POINT ( 'NONE',  ( 164.8329445879545290, 245.1479605429143760, -2.955380775890217304 ) ) ;
#85063 = ORIENTED_EDGE ( 'NONE', *, *, #57842, .F. ) ;
#85064 = CARTESIAN_POINT ( 'NONE',  ( 77.48665757143110966, 49.22860469427720886, 15.29917572744006904 ) ) ;
#85065 = FACE_OUTER_BOUND ( 'NONE', #28014, .T. ) ;
#85066 = ORIENTED_EDGE ( 'NONE', *, *, #49498, .T. ) ;
#85067 = CARTESIAN_POINT ( 'NONE',  ( 159.5050723400634638, 254.3761059724978679, -15.34938048045353298 ) ) ;
#85068 = CARTESIAN_POINT ( 'NONE',  ( 187.1296147083845085, 276.7229790764539530, -17.49940255933115196 ) ) ;
#85069 = EDGE_CURVE ( 'NONE', #10423, #74959, #16319, .T. ) ;
#85070 = CARTESIAN_POINT ( 'NONE',  ( 67.65269435575517321, 68.60991329069676681, -5.309777227589590254 ) ) ;
#85071 = ORIENTED_EDGE ( 'NONE', *, *, #30850, .F. ) ;
#85072 = CARTESIAN_POINT ( 'NONE',  ( 173.3065076608714605, 251.6304707193385752, 8.836706110889046588E-05 ) ) ;
#85073 = ORIENTED_EDGE ( 'NONE', *, *, #52812, .T. ) ;
#85074 = CARTESIAN_POINT ( 'NONE',  ( 79.45382063701610775, 46.23955422872901977, -13.23447544246345409 ) ) ;
#85075 = CARTESIAN_POINT ( 'NONE',  ( 194.3442947553755005, 294.0328026529847421, -15.97648891113594871 ) ) ;
#85076 = DIRECTION ( 'NONE',  ( 0.000000000000000000, 0.000000000000000000, -1.000000000000000000 ) ) ;
#85077 = EDGE_LOOP ( 'NONE', ( #60304, #37470, #32726, #21646, #77339, #23798, #6559, #7375, #27148, #21137, #4105, #48637, #95223, #4889, #46655, #88612, #71924, #35223, #37233, #98255, #52067 ) ) ;
#85078 = CARTESIAN_POINT ( 'NONE',  ( 26.87427219475921092, 30.91421378149919974, 9.188101187500008038 ) ) ;
#85079 = AXIS2_PLACEMENT_3D ( 'NONE', #96805, #65356, #66846 ) ;
#85080 = CARTESIAN_POINT ( 'NONE',  ( 38.49039832772786696, 181.4824982072973683, 3.021315404115420679E-15 ) ) ;
#85081 = CARTESIAN_POINT ( 'NONE',  ( 75.01383350950911222, 67.34328350408776487, -12.89590634041038086 ) ) ;
#85082 = EDGE_CURVE ( 'NONE', #49707, #44730, #62466, .T. ) ;
#85083 = ORIENTED_EDGE ( 'NONE', *, *, #49408, .T. ) ;
#85084 = CARTESIAN_POINT ( 'NONE',  ( 0.5143710859096835009, 78.77562236714182120, 59.99999999999999289 ) ) ;
#85085 = EDGE_CURVE ( 'NONE', #58437, #91328, #3407, .T. ) ;
#85086 = B_SPLINE_CURVE_WITH_KNOTS ( 'NONE', 3,
 ( #39368, #78410, #38883, #17085, #46475, #39861, #16091, #56067, #8011, #69786, #62171, #70282, #62675, #396, #77406, #85027, #86553, #32785, #93122, #70798, #30801, #23673, #47485, #63190 ),
 .UNSPECIFIED., .F., .F.,
 ( 4, 2, 2, 2, 2, 2, 2, 2, 2, 2, 2, 4 ),
 ( 0.000000000000000000, 0.1250000000000021927, 0.2500000000000043854, 0.3750000000000065503, 0.4375000000000026090, 0.4999999999999986677, 0.5624999999999946709, 0.6249999999999906741, 0.6874999999999866773, 0.7499999999999825695, 0.8749999999999913403, 1.000000000000000000 ),
 .UNSPECIFIED. ) ;
#85087 = CARTESIAN_POINT ( 'NONE',  ( 197.0121621852902933, 287.4119207165142029, 17.64812647472269092 ) ) ;
#85088 = AXIS2_PLACEMENT_3D ( 'NONE', #96000, #42232, #89881 ) ;
#85089 = VERTEX_POINT ( 'NONE', #47772 ) ;
#85090 = LINE ( 'NONE', #8064, #45921 ) ;
#85092 = CARTESIAN_POINT ( 'NONE',  ( 67.91597355651013856, 65.35775589351075610, -10.44541676389640372 ) ) ;
#85091 = CARTESIAN_POINT ( 'NONE',  ( 67.90944760599185770, 65.67478569269405853, 10.85168271666284312 ) ) ;
#85093 = CARTESIAN_POINT ( 'NONE',  ( 69.31540213678381690, 70.94726294322936155, -2.438276973829965222 ) ) ;
#85094 = CARTESIAN_POINT ( 'NONE',  ( 204.3574891606595827, 276.6894411969685166, 13.41627538812899978 ) ) ;
#85095 = CARTESIAN_POINT ( 'NONE',  ( 187.5420919156053401, 294.0784138002250643, -10.86800630351413588 ) ) ;
#85096 = CARTESIAN_POINT ( 'NONE',  ( 157.8719920515997046, 257.2046840049564480, -17.69857783492101433 ) ) ;
#85097 = CARTESIAN_POINT ( 'NONE',  ( 141.2833242589136375, 258.5024278399160380, 9.188101187500095079 ) ) ;
#85098 = CARTESIAN_POINT ( 'NONE',  ( 177.1123716022877943, 269.3477771532123484, 16.09281802875675993 ) ) ;
#85099 = CARTESIAN_POINT ( 'NONE',  ( 195.7956752809994327, 291.0480278656929158, -15.87661460891315279 ) ) ;
#85100 = CARTESIAN_POINT ( 'NONE',  ( 77.41429782557628414, 209.3768266524159571, -9.188101187500091527 ) ) ;
#85101 = ORIENTED_EDGE ( 'NONE', *, *, #21060, .T. ) ;
#85102 = CARTESIAN_POINT ( 'NONE',  ( 151.4159295687746294, 268.3869122420484814, 14.78076517566594106 ) ) ;
#85103 = DIRECTION ( 'NONE',  ( -0.8660254037844387076, -0.4999999999999998890, -0.000000000000000000 ) ) ;
#85104 = EDGE_LOOP ( 'NONE', ( #44204, #46829, #88929, #90210 ) ) ;
#85105 = CARTESIAN_POINT ( 'NONE',  ( 195.9058436374999701, 291.3281206506429726, -17.17388571147666809 ) ) ;
#85106 = VERTEX_POINT ( 'NONE', #93432 ) ;
#85107 = EDGE_LOOP ( 'NONE', ( #34351, #87969, #63371, #13938, #17688, #56883 ) ) ;
#85108 = ADVANCED_FACE ( 'NONE', ( #1199 ), #9296, .F. ) ;
#85109 = CARTESIAN_POINT ( 'NONE',  ( 66.61936531471503997, 67.57008932741632634, 6.288575924362496572 ) ) ;
#85110 = CARTESIAN_POINT ( 'NONE',  ( 196.5475680726518988, 286.0355519910975772, 16.91030377461561685 ) ) ;
#85111 = CARTESIAN_POINT ( 'NONE',  ( 191.8000917695741805, 298.4394914891611847, -9.452573400474340914 ) ) ;
#85112 = CARTESIAN_POINT ( 'NONE',  ( 80.99918023960148616, 56.04449057398856127, 16.10194400669177384 ) ) ;
#85113 = CARTESIAN_POINT ( 'NONE',  ( 78.61788708802706083, 48.81601089383328684, -14.35964102986092605 ) ) ;
#85114 = CARTESIAN_POINT ( 'NONE',  ( 72.56631922146607394, 69.50290373287580792, 8.912124407776673252 ) ) ;
#85115 = CARTESIAN_POINT ( 'NONE',  ( 79.47110815956433783, 210.5643266524160424, 9.188101187500095079 ) ) ;
#85116 = VERTEX_POINT ( 'NONE', #9817 ) ;
#85117 = EDGE_CURVE ( 'NONE', #60349, #39911, #40522, .T. ) ;
#85118 = VERTEX_POINT ( 'NONE', #80238 ) ;
#85119 = CARTESIAN_POINT ( 'NONE',  ( 200.7808116640040055, 282.8844283434642648, -16.74230052443130390 ) ) ;
#85120 = ORIENTED_EDGE ( 'NONE', *, *, #90559, .T. ) ;
#85121 = CARTESIAN_POINT ( 'NONE',  ( 83.86025440731803826, 41.72852670257621810, 0.4223142476417495184 ) ) ;
#85122 = EDGE_CURVE ( 'NONE', #30031, #36428, #81303, .T. ) ;
#85123 = EDGE_CURVE ( 'NONE', #79865, #8628, #18409, .T. ) ;
#85124 = CARTESIAN_POINT ( 'NONE',  ( 183.9930990868905099, 275.1979307975402094, 16.37542179091846606 ) ) ;
#85125 = CARTESIAN_POINT ( 'NONE',  ( 205.9642072045669465, 273.9065239114831911, 10.22128930895731536 ) ) ;
#85127 = EDGE_CURVE ( 'NONE', #89587, #16529, #24983, .T. ) ;
#85126 = AXIS2_PLACEMENT_3D ( 'NONE', #5008, #35887, #51593 ) ;
#85128 = CARTESIAN_POINT ( 'NONE',  ( -32.57773935851065517, 93.92637809958223727, 43.89948692389421581 ) ) ;
#85129 = CARTESIAN_POINT ( 'NONE',  ( 207.2804460909495674, 270.7025114183682035, -2.311883053335581195 ) ) ;
#85130 = CARTESIAN_POINT ( 'NONE',  ( 159.8059924763540494, 259.8542309688582463, 16.66854085587838696 ) ) ;
#85131 = ORIENTED_EDGE ( 'NONE', *, *, #81003, .F. ) ;
#85132 = CARTESIAN_POINT ( 'NONE',  ( 192.4020620555409380, 296.6120898282274538, 11.26082810598535922 ) ) ;
#85133 = EDGE_CURVE ( 'NONE', #95124, #17862, #33777, .T. ) ;
#85134 = CARTESIAN_POINT ( 'NONE',  ( 185.2191931831976603, 260.2532633546392162, 6.303467285011207011 ) ) ;
#85135 = ADVANCED_FACE ( 'NONE', ( #26503 ), #58856, .T. ) ;
#85136 = CARTESIAN_POINT ( 'NONE',  ( 147.7724539486783044, 275.5393038904080640, -3.815232554072548687 ) ) ;
#85137 = CARTESIAN_POINT ( 'NONE',  ( 152.7729059155601021, 266.0365602647466972, -17.50667083025758686 ) ) ;
#85138 =( BOUNDED_CURVE ( )  B_SPLINE_CURVE ( 2, ( #76790, #54461, #45385, #44880, #83939, #15988, #84925, #46888, #75820, #6407, #93015, #99613, #22594 ),
 .UNSPECIFIED., .F., .T. ) 
 B_SPLINE_CURVE_WITH_KNOTS ( ( 3, 2, 2, 2, 2, 2, 3 ),
 ( 0.2124999999999999944, 0.2149999999999999967, 0.2200000000000000011, 0.2250000000000000056, 0.2300000000000000100, 0.2349999999999999867, 0.2374999999999999889 ),
 .UNSPECIFIED. ) 
 CURVE ( )  GEOMETRIC_REPRESENTATION_ITEM ( )  RATIONAL_B_SPLINE_CURVE ( ( 0.9755282581475768211, 0.9755282581475768211, 1.000000000000000000, 0.9510565162951535312, 1.000000000000000000, 0.9510565162951535312, 1.000000000000000000, 0.9510565162951535312, 1.000000000000000000, 0.9510565162951535312, 1.000000000000000000, 0.9755282581475768211, 0.9755282581475768211 ) ) 
 REPRESENTATION_ITEM ( '' )  );
#85139 = AXIS2_PLACEMENT_3D ( 'NONE', #99325, #60777, #39473 ) ;
#85140 = CARTESIAN_POINT ( 'NONE',  ( 72.53309028193872621, 70.86290320417140265, 7.626211012637808651 ) ) ;
#85141 = FACE_OUTER_BOUND ( 'NONE', #71534, .T. ) ;
#85142 = EDGE_LOOP ( 'NONE', ( #12192, #57062, #35269, #85401 ) ) ;
#85143 = DIRECTION ( 'NONE',  ( 0.5000000000000003331, -0.8660254037844385966, -5.484689767424254197E-16 ) ) ;
#85144 = CARTESIAN_POINT ( 'NONE',  ( 148.3187134315808748, 276.1718878684489482, -3.836830238838571550 ) ) ;
#85145 = CARTESIAN_POINT ( 'NONE',  ( 82.29787399700251171, 40.87733562811993693, 1.011763546004324166 ) ) ;
#85146 = CARTESIAN_POINT ( 'NONE',  ( 168.0624319142297054, 250.1787547974163033, 6.948285211281213236 ) ) ;
#85147 = CARTESIAN_POINT ( 'NONE',  ( 84.07404364193551771, 51.51966214638419927, 14.67759748506154516 ) ) ;
#85148 = CARTESIAN_POINT ( 'NONE',  ( 152.9231525498888118, 270.9783143214066854, 14.00607015262799671 ) ) ;
#85149 = ORIENTED_EDGE ( 'NONE', *, *, #67447, .F. ) ;
#85150 = CARTESIAN_POINT ( 'NONE',  ( 163.0683798854284703, 248.2042762609320903, 11.26611642476872710 ) ) ;
#85151 = AXIS2_PLACEMENT_3D ( 'NONE', #60666, #75923, #76883 ) ;
#85152 = CARTESIAN_POINT ( 'NONE',  ( 79.57426776854913442, 46.24084366570345850, -13.18946159588284317 ) ) ;
#85154 = FACE_BOUND ( 'NONE', #31324, .T. ) ;
#85153 = CARTESIAN_POINT ( 'NONE',  ( 155.4812142336614329, 261.3456326552338282, 18.45193178807985745 ) ) ;
#85155 = CARTESIAN_POINT ( 'NONE',  ( 176.1346035850542933, 285.3745144875404662, -12.06757559795553192 ) ) ;
#85156 = CARTESIAN_POINT ( 'NONE',  ( 24.92020183544706668, 36.16126292948897003, -6.180339887498951690 ) ) ;
#85157 = CARTESIAN_POINT ( 'NONE',  ( 170.3771428974362436, 273.8123333415551315, 16.01817606700219088 ) ) ;
#85158 = CARTESIAN_POINT ( 'NONE',  ( 166.5066175986279120, 286.1322789562391335, -3.204271455219934062 ) ) ;
#85159 = DIRECTION ( 'NONE',  ( -0.000000000000000000, -0.000000000000000000, -1.000000000000000000 ) ) ;
#85160 = VECTOR ( 'NONE', #85406, 1000.000000000000114 ) ;
#85161 = B_SPLINE_CURVE_WITH_KNOTS ( 'NONE', 3,
 ( #94726, #72423, #17701, #72924, #81048, #79025, #40478, #25286, #18704, #56172, #64803, #73405, #95244, #10602, #95748, #49585, #25813, #26794, #42470, #3990, #34877, #65777, #27299, #75399, #51071, #66783, #35879, #43473, #97708, #82542, #59153, #60158, #91122, #52079, #28786, #83024, #19712, #21687, #74904, #81528, #90123, #98203, #51586, #20697, #50578, #36371 ),
 .UNSPECIFIED., .F., .F.,
 ( 4, 1, 1, 1, 2, 2, 1, 1, 1, 2, 2, 1, 1, 2, 2, 1, 1, 2, 2, 1, 1, 2, 2, 1, 2, 2, 1, 2, 2, 4 ),
 ( 0.000000000000000000, 0.06250000000000525968, 0.09375000000000867362, 0.1093750000000097006, 0.1171875000000108941, 0.1250000000000120737, 0.1875000000000127676, 0.2187500000000126288, 0.2343750000000140166, 0.2421875000000151823, 0.2500000000000163758, 0.3125000000000134892, 0.3437500000000127676, 0.3593750000000120459, 0.3750000000000112133, 0.4375000000000153766, 0.4687500000000188183, 0.4843750000000199285, 0.5000000000000210942, 0.5625000000000184297, 0.5937500000000172085, 0.6093750000000160982, 0.6250000000000149880, 0.6875000000000138778, 0.7187500000000124345, 0.7500000000000108802, 0.8125000000000085487, 0.8437500000000075495, 0.8750000000000064393, 1.000000000000000000 ),
 .UNSPECIFIED. ) ;
#85162 = CARTESIAN_POINT ( 'NONE',  ( 192.2608584806236252, 262.0927522878173477, 3.022526856766069692 ) ) ;
#85163 = CARTESIAN_POINT ( 'NONE',  ( -7.835251407336910390, 166.2833772461660828, -9.188101187500095079 ) ) ;
#85164 = CARTESIAN_POINT ( 'NONE',  ( 10.06845959268932411, 31.07446838803123157, -10.00000000000000000 ) ) ;
#85165 = VERTEX_POINT ( 'NONE', #96435 ) ;
#85166 = CARTESIAN_POINT ( 'NONE',  ( 177.0173213845591249, 256.3747443458416910, 8.281083027831190435 ) ) ;
#85167 = B_SPLINE_CURVE_WITH_KNOTS ( 'NONE', 3,
 ( #56175, #17704, #79547, #64298, #25816, #95247, #11121, #39971, #26305, #31880 ),
 .UNSPECIFIED., .F., .F.,
 ( 4, 2, 2, 2, 4 ),
 ( 0.000000000000000000, 0.0002622400424273102102, 0.0005244800848546204205, 0.0007867201272819306307, 0.001048960169709240841 ),
 .UNSPECIFIED. ) ;
#85168 = CARTESIAN_POINT ( 'NONE',  ( 72.75722467535679527, 70.26520034150425431, -8.071865018468246333 ) ) ;
#85169 = CARTESIAN_POINT ( 'NONE',  ( 202.5511068033279685, 273.9590694375769999, -13.16333768474205357 ) ) ;
#85170 = CARTESIAN_POINT ( 'NONE',  ( 99.93749413994396491, 240.0530062829862743, -4.648177544792955347E-16 ) ) ;
#85171 = CARTESIAN_POINT ( 'NONE',  ( 30.64892602121659593, 182.3768266524160140, -9.188101187500093303 ) ) ;
#85172 = CARTESIAN_POINT ( 'NONE',  ( 58.10966550219799132, 178.3759306620403606, 17.47570218321536473 ) ) ;
#85173 = CARTESIAN_POINT ( 'NONE',  ( 181.9416707481567812, 275.7034555988952889, -16.43191976972476809 ) ) ;
#85174 = CARTESIAN_POINT ( 'NONE',  ( 32.64838280634442214, 30.80066082961423746, 10.00000000000000533 ) ) ;
#85175 = CARTESIAN_POINT ( 'NONE',  ( 83.27929122224395542, 41.83289114379940798, -3.541494727109722351 ) ) ;
#85176 = CARTESIAN_POINT ( 'NONE',  ( 170.0877722087189170, 270.7013820935941339, -17.07221500441185214 ) ) ;
#85177 = CARTESIAN_POINT ( 'NONE',  ( 81.57324034346744668, 55.97255112923638620, 16.04000112846837212 ) ) ;
#85178 = CARTESIAN_POINT ( 'NONE',  ( 83.27435412308909690, 44.55311305779904529, 9.827056061616449512 ) ) ;
#85179 = CARTESIAN_POINT ( 'NONE',  ( 168.2820353728258738, 287.7095463320123940, -5.019694092131335772 ) ) ;
#85180 = CARTESIAN_POINT ( 'NONE',  ( 79.69646206235805153, 203.4865022471901455, 1.119607411625061291E-15 ) ) ;
#85181 = PLANE ( 'NONE',  #18332 ) ;
#85182 = FACE_OUTER_BOUND ( 'NONE', #91457, .T. ) ;
#85183 = CARTESIAN_POINT ( 'NONE',  ( 32.86828966629671811, 177.5327760586659736, 1.948934522072303157E-15 ) ) ;
#85184 = PLANE ( 'NONE',  #30989 ) ;
#85185 = DIRECTION ( 'NONE',  ( 0.5000000000000013323, -0.8660254037844378194, 0.000000000000000000 ) ) ;
#85186 = CARTESIAN_POINT ( 'NONE',  ( 151.2567985338353935, 268.6625352796243646, -15.71756535662528798 ) ) ;
#85187 = EDGE_CURVE ( 'NONE', #70849, #27171, #24421, .T. ) ;
#85188 = DIRECTION ( 'NONE',  ( -0.8660254037844384856, -0.5000000000000002220, 0.000000000000000000 ) ) ;
#85189 = CARTESIAN_POINT ( 'NONE',  ( -2.575951297163730835, 175.9865022471903160, 10.00000000000009415 ) ) ;
#85190 = CARTESIAN_POINT ( 'NONE',  ( 159.8838727533587587, 278.4444054329620712, -9.946836423640300850 ) ) ;
#85191 = CARTESIAN_POINT ( 'NONE',  ( 69.95523204135938045, 62.90150226501648234, 13.86126985460704297 ) ) ;
#85192 = ITEM_DEFINED_TRANSFORMATION ( 'NONE', 'NONE', #5732,  #68784 ) ;
#85193 = CARTESIAN_POINT ( 'NONE',  ( 18.65184876021338312, 28.95586893147755703, 7.433330006724141015 ) ) ;
#85194 = CARTESIAN_POINT ( 'NONE',  ( 147.9710862514405960, 274.3535558917855042, 7.785500222159708272 ) ) ;
#85195 = CARTESIAN_POINT ( 'NONE',  ( 71.42966913292450215, 59.23173737558743568, 15.26165678737305065 ) ) ;
#85196 = VECTOR ( 'NONE', #81616, 1000.000000000000227 ) ;
#85197 = CARTESIAN_POINT ( 'NONE',  ( 188.9038075421769918, 270.0326964921503645, -14.10267558245943320 ) ) ;
#85198 = ORIENTED_EDGE ( 'NONE', *, *, #69952, .T. ) ;
#85199 = VECTOR ( 'NONE', #64798, 1000.000000000000000 ) ;
#85200 = CARTESIAN_POINT ( 'NONE',  ( 15.64721481668148328, 11.96004757982089295, -5.678558825948275768 ) ) ;
#85201 = CARTESIAN_POINT ( 'NONE',  ( 73.98867670750783532, 59.60256495767924179, -15.59328569222777183 ) ) ;
#85202 = CARTESIAN_POINT ( 'NONE',  ( 81.51617444448474714, 41.98210561432389909, 7.630276461086227258 ) ) ;
#85203 = EDGE_CURVE ( 'NONE', #42320, #89828, #17774, .T. ) ;
#85204 = ORIENTED_EDGE ( 'NONE', *, *, #1583, .T. ) ;
#85205 = CARTESIAN_POINT ( 'NONE',  ( 16.68302997285341149, 191.9860189848785410, -2.679491924311252493 ) ) ;
#85206 = CARTESIAN_POINT ( 'NONE',  ( 72.61141802365665399, 71.36933893402679985, -5.910933643996240328 ) ) ;
#85207 = VECTOR ( 'NONE', #44334, 1000.000000000000227 ) ;
#85208 = DIRECTION ( 'NONE',  ( -0.000000000000000000, -0.000000000000000000, -1.000000000000000000 ) ) ;
#85209 = EDGE_CURVE ( 'NONE', #4349, #38493, #43674, .T. ) ;
#85210 = CARTESIAN_POINT ( 'NONE',  ( 66.29454943693276903, 69.24199052626691753, -2.144636311159408226 ) ) ;
#85211 = ORIENTED_EDGE ( 'NONE', *, *, #26966, .T. ) ;
#85212 = ORIENTED_EDGE ( 'NONE', *, *, #22512, .F. ) ;
#85214 = CARTESIAN_POINT ( 'NONE',  ( 86.62800554614717896, 43.31088370039552160, -1.499291040926804763 ) ) ;
#85213 = CARTESIAN_POINT ( 'NONE',  ( 202.4421998307519743, 279.5209983176915216, 15.52974020151914480 ) ) ;
#85215 = ORIENTED_EDGE ( 'NONE', *, *, #14071, .T. ) ;
#85216 = CARTESIAN_POINT ( 'NONE',  ( 153.4361244163197000, 264.8878321249116539, -17.23169627811277493 ) ) ;
#85217 = DIRECTION ( 'NONE',  ( 0.9708212084269294273, -0.2398044646550112069, 0.000000000000000000 ) ) ;
#85218 = PLANE ( 'NONE',  #79128 ) ;
#85219 = CARTESIAN_POINT ( 'NONE',  ( 84.14312167556933275, 48.98415679381830756, 0.000000000000000000 ) ) ;
#85220 = ORIENTED_EDGE ( 'NONE', *, *, #31776, .F. ) ;
#85221 = CARTESIAN_POINT ( 'NONE',  ( 190.6071113721798156, 300.5057941498820924, -0.4754021072632813594 ) ) ;
#85222 = DIRECTION ( 'NONE',  ( 0.000000000000000000, 0.000000000000000000, 1.000000000000000000 ) ) ;
#85223 = VERTEX_POINT ( 'NONE', #74616 ) ;
#85224 = DIRECTION ( 'NONE',  ( -0.000000000000000000, 0.000000000000000000, 1.000000000000000000 ) ) ;
#85225 = VECTOR ( 'NONE', #59905, 1000.000000000000000 ) ;
#85226 = CARTESIAN_POINT ( 'NONE',  ( 161.3793624665346158, 266.8670659500822921, 16.51829894754524730 ) ) ;
#85227 = ORIENTED_EDGE ( 'NONE', *, *, #77006, .T. ) ;
#85228 = CARTESIAN_POINT ( 'NONE',  ( 33.16918417342686354, 21.01110640527294038, 2.839279412974134775 ) ) ;
#85229 = CARTESIAN_POINT ( 'NONE',  ( 190.7516742497373059, 300.2554039010641418, 4.342609251298632067 ) ) ;
#85230 = CARTESIAN_POINT ( 'NONE',  ( 78.19043972245502516, 47.52173921620315156, -13.84048554213443261 ) ) ;
#85231 = ORIENTED_EDGE ( 'NONE', *, *, #393, .F. ) ;
#85232 = CARTESIAN_POINT ( 'NONE',  ( -4.696717224021703885, 77.89375390941042099, 14.01032106654459142 ) ) ;
#85233 = CARTESIAN_POINT ( 'NONE',  ( 159.5111797645456306, 254.9608776620166850, 15.67735860260454928 ) ) ;
#85234 = CARTESIAN_POINT ( 'NONE',  ( 78.19098230064227550, 47.51660667919665570, -14.38750087007935186 ) ) ;
#85236 = AXIS2_PLACEMENT_3D ( 'NONE', #83060, #14627, #23206 ) ;
#85235 = CARTESIAN_POINT ( 'NONE',  ( 83.81658881107364323, 52.06750489740826993, 14.58996321880578151 ) ) ;
#85237 = VERTEX_POINT ( 'NONE', #50776 ) ;
#85238 = ORIENTED_EDGE ( 'NONE', *, *, #97792, .T. ) ;
#85239 = EDGE_CURVE ( 'NONE', #2126, #19964, #65001, .T. ) ;
#85240 = DIRECTION ( 'NONE',  ( 0.4999999999999998890, -0.8660254037844385966, 0.000000000000000000 ) ) ;
#85241 = CARTESIAN_POINT ( 'NONE',  ( -11.70629829599211646, 23.25616956148705938, 10.00000000000000000 ) ) ;
#85242 = CARTESIAN_POINT ( 'NONE',  ( 190.3144310910409445, 301.0127312671879167, -1.334877248546042949 ) ) ;
#85243 = ORIENTED_EDGE ( 'NONE', *, *, #99719, .F. ) ;
#85244 = DIRECTION ( 'NONE',  ( 0.000000000000000000, -0.000000000000000000, -1.000000000000000000 ) ) ;
#85245 = CARTESIAN_POINT ( 'NONE',  ( 170.9861191376329259, 275.4057932803170274, -16.08545443273202125 ) ) ;
#85246 = CARTESIAN_POINT ( 'NONE',  ( 207.8844858873204657, 270.5805036682629066, -6.251308616122969397 ) ) ;
#85247 = CARTESIAN_POINT ( 'NONE',  ( 192.7705129102570822, 296.7586727687594816, -13.39629674907774692 ) ) ;
#85248 = ADVANCED_FACE ( 'NONE', ( #82734 ), #13305, .T. ) ;
#85249 = CARTESIAN_POINT ( 'NONE',  ( 47.39496755818311158, 108.2889530649357681, -10.00000000000000000 ) ) ;
#85250 = CARTESIAN_POINT ( 'NONE',  ( 70.80090459924991819, 69.25659177360545016, 7.761957622020450920 ) ) ;
#85251 = FACE_OUTER_BOUND ( 'NONE', #16854, .T. ) ;
#85252 = CARTESIAN_POINT ( 'NONE',  ( 67.56978446451059028, 66.68927659431298594, 8.641485439713591177 ) ) ;
#85253 = CARTESIAN_POINT ( 'NONE',  ( 68.80791472686313170, 65.65516334055519110, -10.66944597666374861 ) ) ;
#85254 = CARTESIAN_POINT ( 'NONE',  ( 78.21265317814797413, 47.50325902310300563, 14.37429833372570620 ) ) ;
#85255 = CARTESIAN_POINT ( 'NONE',  ( 114.7887934315897382, 227.8923013555410080, 4.594050593750050204 ) ) ;
#85256 = ORIENTED_EDGE ( 'NONE', *, *, #89789, .T. ) ;
#85257 = CARTESIAN_POINT ( 'NONE',  ( 146.9456733906991417, 276.1296230653242105, -0.7988785540157754550 ) ) ;
#85258 = CARTESIAN_POINT ( 'NONE',  ( 70.21724893432667614, 65.14247767143801582, 11.87715301600730911 ) ) ;
#85259 = EDGE_CURVE ( 'NONE', #66385, #1218, #43162, .T. ) ;
#85260 = CARTESIAN_POINT ( 'NONE',  ( 87.60591442325252842, 44.91970625728536959, -6.572271063428638982 ) ) ;
#85261 = DIRECTION ( 'NONE',  ( 0.1039558454088763267, -0.1800568059919503139, 0.9781476007338069101 ) ) ;
#85262 = CARTESIAN_POINT ( 'NONE',  ( 191.3471005483181102, 298.1160726331887645, -9.452014560043723534 ) ) ;
#85263 = CARTESIAN_POINT ( 'NONE',  ( 83.91468266313496827, 51.82819685387456587, -14.47034327719529045 ) ) ;
#85264 = CARTESIAN_POINT ( 'NONE',  ( 165.9607527239562614, 283.6245786231995112, -8.165966701861027133 ) ) ;
#85265 = ORIENTED_EDGE ( 'NONE', *, *, #10768, .F. ) ;
#85266 = DIRECTION ( 'NONE',  ( 0.7162481363636786780, 0.000000000000000000, -0.6978456900745014790 ) ) ;
#85267 = CARTESIAN_POINT ( 'NONE',  ( 72.05417303993513656, 71.64307123591491688, 5.506498905688426149 ) ) ;
#85268 = CARTESIAN_POINT ( 'NONE',  ( 47.92415505746842541, 205.1427522451419065, 10.00000000000009237 ) ) ;
#85269 = CARTESIAN_POINT ( 'NONE',  ( 120.7963240266967375, 249.7369531367911293, -4.594050593750048428 ) ) ;
#85270 = CARTESIAN_POINT ( 'NONE',  ( 189.8390163498603158, 294.5874093566309284, -12.44163422039437528 ) ) ;
#85271 = CARTESIAN_POINT ( 'NONE',  ( 20.94669640352213236, 37.57748520232516398, 10.00000000000000000 ) ) ;
#85272 = CARTESIAN_POINT ( 'NONE',  ( 196.0727848089514964, 291.0389700598140621, 17.56388901715066808 ) ) ;
#85273 = CARTESIAN_POINT ( 'NONE',  ( -112.5954152546897120, 74.04580364311804885, 30.52142883766498116 ) ) ;
#85274 = CARTESIAN_POINT ( 'NONE',  ( 51.59574192737019160, 200.5958772461660544, -9.188101187500095079 ) ) ;
#85275 = CIRCLE ( 'NONE', #93366, 70.00000000000001421 ) ;
#85277 = CARTESIAN_POINT ( 'NONE',  ( 188.0333306978322128, 299.5241197090491028, 3.603443727378835781 ) ) ;
#85276 = AXIS2_PLACEMENT_3D ( 'NONE', #54244, #85217, #15762 ) ;
#85278 = ORIENTED_EDGE ( 'NONE', *, *, #50979, .F. ) ;
#85279 = CARTESIAN_POINT ( 'NONE',  ( 72.55067284226147706, 68.13922894791654983, 10.49063991969712184 ) ) ;
#85280 = CARTESIAN_POINT ( 'NONE',  ( 88.03972809732340465, 44.75281308623453924, -4.524080385986239961 ) ) ;
#85281 = B_SPLINE_SURFACE_WITH_KNOTS ( 'NONE', 3, 1, ( 
 ( #18203, #49097 ),
 ( #27298, #57175 ),
 ( #97224, #88155 ),
 ( #96230, #10099 ),
 ( #56171, #58181 ),
 ( #25812, #18703 ),
 ( #41987, #19220 ),
 ( #72422, #56686 ),
 ( #66292, #35380 ),
 ( #80032, #41473 ),
 ( #11610, #3025 ),
 ( #17700, #64802 ),
 ( #88655, #11117 ),
 ( #50577, #49584 ),
 ( #3514, #81527 ),
 ( #4487, #42469 ),
 ( #40963, #72923 ),
 ( #42957, #2509 ),
 ( #34391, #65290 ),
 ( #50091, #81047 ),
 ( #73403, #48602 ),
 ( #3989, #34875 ),
 ( #65776, #96733 ),
 ( #89165, #19711 ),
 ( #79541, #73898 ),
 ( #58666, #74903 ),
 ( #36370, #6488 ),
 ( #28275, #98708 ),
 ( #51070, #66782 ),
 ( #28784, #43965 ),
 ( #29779, #52565 ),
 ( #14587, #83022 ),
 ( #67783, #37366 ),
 ( #60652, #21199 ) ),
 .UNSPECIFIED., .T., .F., .F.,
 ( 4, 2, 2, 2, 2, 2, 2, 2, 2, 2, 2, 2, 2, 2, 2, 2, 4 ),
 ( 2, 2 ),
 ( 0.000000000000000000, 0.06250000000000000000, 0.1250000000000000000, 0.1875000000000000000, 0.2500000000000000000, 0.3125000000000000000, 0.3750000000000000000, 0.4375000000000000000, 0.5000000000000000000, 0.5625000000000000000, 0.6250000000000000000, 0.6875000000000000000, 0.7500000000000000000, 0.8125000000000000000, 0.8750000000000000000, 0.9375000000000000000, 1.000000000000000000 ),
 ( 0.000000000000000000, 1.000000000000000000 ),
 .UNSPECIFIED. ) ;
#85282 = CARTESIAN_POINT ( 'NONE',  ( 24.41517378745132660, 178.2365022471902307, 10.00000000000009948 ) ) ;
#85283 = FACE_OUTER_BOUND ( 'NONE', #60540, .T. ) ;
#85284 = CARTESIAN_POINT ( 'NONE',  ( 177.6444986370304946, 293.6980009803469329, 2.770296639708824227 ) ) ;
#85285 = LINE ( 'NONE', #91380, #12321 ) ;
#85286 = CARTESIAN_POINT ( 'NONE',  ( 179.1341793956848676, 261.5303873598331847, 12.21931224842648511 ) ) ;
#85287 = CARTESIAN_POINT ( 'NONE',  ( 96.56591523669439425, 239.8927522451419350, 2.944929066748280225E-16 ) ) ;
#85288 = CIRCLE ( 'NONE', #23770, 70.00000000000001421 ) ;
#85289 = LINE ( 'NONE', #77140, #77424 ) ;
#85290 = ORIENTED_EDGE ( 'NONE', *, *, #91287, .F. ) ;
#85291 = EDGE_CURVE ( 'NONE', #7311, #60486, #77806, .T. ) ;
#85292 = CARTESIAN_POINT ( 'NONE',  ( 189.8136646974935786, 301.8800841035353528, -0.6430783927310335102 ) ) ;
#85293 = CARTESIAN_POINT ( 'NONE',  ( 88.01007674647709678, 44.79289111569436699, 4.713013503925086667 ) ) ;
#85294 = AXIS2_PLACEMENT_3D ( 'NONE', #41238, #24548, #40738 ) ;
#85295 = CARTESIAN_POINT ( 'NONE',  ( 22.39418752168989712, 192.9244531367911293, -4.594050593750046652 ) ) ;
#85296 = CARTESIAN_POINT ( 'NONE',  ( 11.69612814616573893, 25.49103043416548076, -8.090169943749479842 ) ) ;
#85297 = AXIS2_PLACEMENT_3D ( 'NONE', #13703, #82155, #89273 ) ;
#85298 = CARTESIAN_POINT ( 'NONE',  ( -29.62033169268383404, 35.98430678844710684, 59.99999999999999289 ) ) ;
#85299 = CARTESIAN_POINT ( 'NONE',  ( -19.65312891409030271, 93.06504152958497400, 203.6502102582797420 ) ) ;
#85300 = DIRECTION ( 'NONE',  ( -0.3766285016932073293, 0.9263643838751195458, 0.000000000000000000 ) ) ;
#85302 = CARTESIAN_POINT ( 'NONE',  ( 69.59257202794182717, 220.1744531367911293, 4.594050593750047540 ) ) ;
#85301 = CARTESIAN_POINT ( 'NONE',  ( 196.9509217096318423, 276.5932595302290906, -15.33546036893861420 ) ) ;
#85303 = CARTESIAN_POINT ( 'NONE',  ( 200.1444820856229967, 283.9865835035790269, 17.93386694781497326 ) ) ;
#85304 = CARTESIAN_POINT ( 'NONE',  ( 73.16329361895407146, 57.31197931467701068, 16.38585881187776749 ) ) ;
#85305 = CARTESIAN_POINT ( 'NONE',  ( 56.56090640341663800, 191.9155109091896350, 2.679491924311254714 ) ) ;
#85306 = CARTESIAN_POINT ( 'NONE',  ( 18.98444911510674160, 11.36477965099639675, 1.583844403245364907 ) ) ;
#85307 = ORIENTED_EDGE ( 'NONE', *, *, #36985, .T. ) ;
#85308 = CARTESIAN_POINT ( 'NONE',  ( 165.2390926464214260, 269.1549683505341477, 16.83750853429537031 ) ) ;
#85309 = CARTESIAN_POINT ( 'NONE',  ( 25.20903040758703284, 185.3615022471902591, -10.00000000000009592 ) ) ;
#85310 = CARTESIAN_POINT ( 'NONE',  ( 164.2090401137261892, 246.2285947913476889, -5.787448100099915393 ) ) ;
#85311 = CARTESIAN_POINT ( 'NONE',  ( 148.0493212738620628, 256.2833772461660828, -9.188101187500095079 ) ) ;
#85312 = CARTESIAN_POINT ( 'NONE',  ( 25.62156559687931434, 36.83396525600391413, -2.839279412974133887 ) ) ;
#85313 = CARTESIAN_POINT ( 'NONE',  ( 164.0862216042829402, 260.4305047126978252, -16.14355404909294123 ) ) ;
#85314 = CARTESIAN_POINT ( 'NONE',  ( 189.2475850683314889, 261.5409228790725251, 6.709830765752542447 ) ) ;
#85315 = CARTESIAN_POINT ( 'NONE',  ( 164.2813349609167517, 246.1033764428878214, 1.949810150281061638 ) ) ;
#85316 = EDGE_CURVE ( 'NONE', #92799, #5666, #44655, .T. ) ;
#85317 = CARTESIAN_POINT ( 'NONE',  ( 71.63103492117565452, 72.07843208848032646, 3.395715836721224790 ) ) ;
#85318 = CARTESIAN_POINT ( 'NONE',  ( 66.50888126359876651, 68.78582482296066303, 2.298140800692767716 ) ) ;
#85319 = VERTEX_POINT ( 'NONE', #46663 ) ;
#85320 = CARTESIAN_POINT ( 'NONE',  ( 191.1489696025915919, 299.5672681643093256, 8.892130899335590755 ) ) ;
#85321 = DIRECTION ( 'NONE',  ( -0.8660254037844387076, -0.4999999999999998890, -0.000000000000000000 ) ) ;
#85322 = CARTESIAN_POINT ( 'NONE',  ( 177.8663784656789062, 286.4429601165666099, 13.25884385786000230 ) ) ;
#85323 = CARTESIAN_POINT ( 'NONE',  ( 196.1245817477023650, 288.9492551302209336, 17.30641872853625074 ) ) ;
#85324 = CARTESIAN_POINT ( 'NONE',  ( 9.878523645489616811, 21.10171378149916777, 9.188101187500008038 ) ) ;
#85325 = ORIENTED_EDGE ( 'NONE', *, *, #48498, .T. ) ;
#85326 = CARTESIAN_POINT ( 'NONE',  ( -22.42236680055709641, 157.8615022471902591, 0.000000000000000000 ) ) ;
#85327 = CARTESIAN_POINT ( 'NONE',  ( 88.21965799167087141, 44.33377460087322675, -2.453011004722113420 ) ) ;
#85328 = EDGE_CURVE ( 'NONE', #95622, #36742, #22866, .T. ) ;
#85329 = LINE ( 'NONE', #17903, #83003 ) ;
#85330 = LINE ( 'NONE', #22975, #1298 ) ;
#85331 = FACE_OUTER_BOUND ( 'NONE', #77786, .T. ) ;
#85332 = EDGE_CURVE ( 'NONE', #17413, #77961, #82, .T. ) ;
#85333 = FACE_OUTER_BOUND ( 'NONE', #20417, .T. ) ;
#85334 = CARTESIAN_POINT ( 'NONE',  ( 201.0468719883840265, 282.4235983437597497, -16.59631526626950659 ) ) ;
#85335 = ORIENTED_EDGE ( 'NONE', *, *, #66078, .T. ) ;
#85336 = ORIENTED_EDGE ( 'NONE', *, *, #22702, .T. ) ;
#85337 = CARTESIAN_POINT ( 'NONE',  ( 190.5217943342473745, 281.4870030958396683, 17.81127109971334121 ) ) ;
#85338 = CARTESIAN_POINT ( 'NONE',  ( 164.0651280066704771, 248.4778578725967861, 9.975266483072225299 ) ) ;
#85339 = EDGE_LOOP ( 'NONE', ( #41789, #78738, #4474, #30956 ) ) ;
#85340 = CARTESIAN_POINT ( 'NONE',  ( -17.42236680055705023, 149.2012482093457777, 0.000000000000000000 ) ) ;
#85341 = CARTESIAN_POINT ( 'NONE',  ( 85.21473396346020479, 45.07546406142533613, -8.320173855083872638 ) ) ;
#85342 = ORIENTED_EDGE ( 'NONE', *, *, #33431, .F. ) ;
#85343 = CARTESIAN_POINT ( 'NONE',  ( -27.77457187288641904, 24.79904599702367562, -10.00000000000000000 ) ) ;
#85344 = CARTESIAN_POINT ( 'NONE',  ( 79.13444159074370532, 60.15296345131730504, -16.46386276767553269 ) ) ;
#85345 = CARTESIAN_POINT ( 'NONE',  ( 11.19180257851625448, 22.16454794089040092, -10.00000000000000355 ) ) ;
#85346 = CIRCLE ( 'NONE', #9304, 17.82106496071138224 ) ;
#85347 = CARTESIAN_POINT ( 'NONE',  ( 69.94244964693436373, 62.64957029637712083, 13.42917468561056715 ) ) ;
#85348 = ORIENTED_EDGE ( 'NONE', *, *, #3505, .T. ) ;
#85349 = CARTESIAN_POINT ( 'NONE',  ( 155.4218027583364687, 261.4485363490496184, 18.59640492044406557 ) ) ;
#85350 = VECTOR ( 'NONE', #26226, 1000.000000000000000 ) ;
#85351 = CARTESIAN_POINT ( 'NONE',  ( 191.5694344253287511, 298.8390017285333897, 8.250976118904059575 ) ) ;
#85352 = CARTESIAN_POINT ( 'NONE',  ( 81.49773370583855581, 42.20892728461021193, -8.015322006907149799 ) ) ;
#85353 = ORIENTED_EDGE ( 'NONE', *, *, #58813, .F. ) ;
#85354 = EDGE_LOOP ( 'NONE', ( #74130, #93437, #31474, #1089 ) ) ;
#85355 = VERTEX_POINT ( 'NONE', #7162 ) ;
#85356 = CARTESIAN_POINT ( 'NONE',  ( 73.27092031662876082, 60.84575549105485948, 15.12685931616829649 ) ) ;
#85358 = ORIENTED_EDGE ( 'NONE', *, *, #39011, .T. ) ;
#85357 = B_SPLINE_CURVE_WITH_KNOTS ( 'NONE', 3,
 ( #2237, #95481, #56904, #80264, #13325, #13802, #29019, #60876, #21896, #74639, #52784, #37097, #67496, #98429, #66996, #44188 ),
 .UNSPECIFIED., .F., .F.,
 ( 4, 1, 2, 2, 2, 1, 2, 2, 4 ),
 ( 0.000000000000000000, 0.1249999999999920619, 0.1874999999999899247, 0.2499999999999877875, 0.4999999999999824585, 0.6249999999999813483, 0.6874999999999823475, 0.7499999999999832356, 1.000000000000000000 ),
 .UNSPECIFIED. ) ;
#85359 = CARTESIAN_POINT ( 'NONE',  ( 68.84931682549257914, 69.27838879186909082, 5.464616672756219096 ) ) ;
#85360 = ORIENTED_EDGE ( 'NONE', *, *, #97792, .F. ) ;
#85361 = CARTESIAN_POINT ( 'NONE',  ( 208.2555382576270233, 269.9378221106229034, 3.215405476967123199 ) ) ;
#85362 = VECTOR ( 'NONE', #79408, 1000.000000000000000 ) ;
#85363 = ADVANCED_FACE ( 'NONE', ( #52757 ), #61853, .T. ) ;
#85364 = CARTESIAN_POINT ( 'NONE',  ( 81.05763270389509501, 43.67158023151814916, 9.470390458390101074 ) ) ;
#85365 = CARTESIAN_POINT ( 'NONE',  ( 165.7697680452210989, 271.5089577923188813, 17.25749984557730343 ) ) ;
#85366 = B_SPLINE_CURVE_WITH_KNOTS ( 'NONE', 3,
 ( #33832, #65208, #48521, #25203, #80965, #1424, #40884, #24703, #55585, #56087, #10022, #87591 ),
 .UNSPECIFIED., .F., .F.,
 ( 4, 2, 2, 2, 2, 4 ),
 ( 7.835778008535133478E-15, 0.0004471628226844677760, 0.0008943256453610996977, 0.001341488468037731674, 0.001565069879376075092, 0.001788651290714418510 ),
 .UNSPECIFIED. ) ;
#85367 = CARTESIAN_POINT ( 'NONE',  ( 92.93017357788669131, 158.0650415295850735, 36.50000000000000000 ) ) ;
#85368 = CARTESIAN_POINT ( 'NONE',  ( 194.1852025340051284, 294.3083584634874796, -15.46421316575964688 ) ) ;
#85369 = CARTESIAN_POINT ( 'NONE',  ( 82.73042059842214258, 53.63367031839453603, -15.74978661431508264 ) ) ;
#85370 = CARTESIAN_POINT ( 'NONE',  ( 197.6411165541630339, 288.3225397939841628, -17.98373575462852614 ) ) ;
#85372 = CARTESIAN_POINT ( 'NONE',  ( 165.3992151465029110, 246.6496888978224433, 1.887000115222200458 ) ) ;
#85371 = B_SPLINE_CURVE_WITH_KNOTS ( 'NONE', 3,
 ( #3391, #18076, #50454, #96108 ),
 .UNSPECIFIED., .F., .F.,
 ( 4, 4 ),
 ( 0.04580664796786450277, 0.04887120950165272509 ),
 .UNSPECIFIED. ) ;
#85373 = B_SPLINE_CURVE_WITH_KNOTS ( 'NONE', 3,
 ( #2839, #26119, #39776, #9414 ),
 .UNSPECIFIED., .F., .F.,
 ( 4, 4 ),
 ( 0.006146573736721493500, 0.01114496846602976675 ),
 .UNSPECIFIED. ) ;
#85374 = CARTESIAN_POINT ( 'NONE',  ( 17.19524200933981817, 21.87878583063841020, -9.188101187500006262 ) ) ;
#85375 = CARTESIAN_POINT ( 'NONE',  ( 198.8358800211527750, 276.4754353779146641, -15.71425324584650340 ) ) ;
#85376 = CARTESIAN_POINT ( 'NONE',  ( 80.02542612678608691, 57.59583086733049839, 16.60012225046075329 ) ) ;
#85378 = ORIENTED_EDGE ( 'NONE', *, *, #93329, .T. ) ;
#85377 = PLANE ( 'NONE',  #60589 ) ;
#85379 = AXIS2_PLACEMENT_3D ( 'NONE', #54052, #93610, #24178 ) ;
#85380 = CARTESIAN_POINT ( 'NONE',  ( 55.71838369152838766, 209.6427522451419350, 10.00000000000009415 ) ) ;
#85381 = CARTESIAN_POINT ( 'NONE',  ( 159.9531724557437826, 253.5999738052623229, -15.71074128491364874 ) ) ;
#85382 = FACE_OUTER_BOUND ( 'NONE', #45645, .T. ) ;
#85383 = CARTESIAN_POINT ( 'NONE',  ( 83.83491441254412280, 45.74439801777876369, -10.08379609569576196 ) ) ;
#85384 = FACE_OUTER_BOUND ( 'NONE', #25138, .T. ) ;
#85385 = CARTESIAN_POINT ( 'NONE',  ( 161.3206464153366824, 283.6027336028535615, 2.150076420610042671 ) ) ;
#85386 = ORIENTED_EDGE ( 'NONE', *, *, #56220, .T. ) ;
#85387 = CARTESIAN_POINT ( 'NONE',  ( 155.3185753361098591, 261.6273314890805750, -17.01637887179724373 ) ) ;
#85388 = AXIS2_PLACEMENT_3D ( 'NONE', #89694, #21248, #44013 ) ;
#85389 = CARTESIAN_POINT ( 'NONE',  ( 126.8046355855010603, 254.0177522451418781, 5.000000000000046185 ) ) ;
#85390 = CARTESIAN_POINT ( 'NONE',  ( -13.11024591527734628, 6.000000000000000000, 32.50000000000000000 ) ) ;
#85391 = CARTESIAN_POINT ( 'NONE',  ( 1.663964738649697406, 171.7677522451418781, 10.00000000000009592 ) ) ;
#85392 = CARTESIAN_POINT ( 'NONE',  ( 90.40467888234286420, 216.8768266524159571, -9.188101187500093303 ) ) ;
#85393 = CARTESIAN_POINT ( 'NONE',  ( 193.6044853607075140, 267.0230459576156932, -11.54443625195158063 ) ) ;
#85394 = CARTESIAN_POINT ( 'NONE',  ( 11.59314018038319283, 18.64441083166259361, -10.00000000000000533 ) ) ;
#85395 = CARTESIAN_POINT ( 'NONE',  ( 170.3121876137535651, 280.6933715238725426, -13.94289214494337159 ) ) ;
#85396 = ADVANCED_FACE ( 'NONE', ( #37556 ), #54240, .T. ) ;
#85397 = CARTESIAN_POINT ( 'NONE',  ( 8.321535033790526725, 165.6115022471902023, -5.000000000000041744 ) ) ;
#85399 = CARTESIAN_POINT ( 'NONE',  ( 75.79515598915105556, 65.48576791014883725, 14.28791538466101585 ) ) ;
#85398 = CARTESIAN_POINT ( 'NONE',  ( 1.717831006336420607, 180.9869531367911293, 4.594050593750046652 ) ) ;
#85400 = CARTESIAN_POINT ( 'NONE',  ( 200.9111546617170916, 282.6586676490145464, 17.66063511622358106 ) ) ;
#85401 = ORIENTED_EDGE ( 'NONE', *, *, #29935, .F. ) ;
#85402 = VERTEX_POINT ( 'NONE', #7672 ) ;
#85403 = FACE_OUTER_BOUND ( 'NONE', #31750, .T. ) ;
#85404 = CARTESIAN_POINT ( 'NONE',  ( 197.5495010542000216, 265.0987281629911081, -2.962445677173857206 ) ) ;
#85405 = CARTESIAN_POINT ( 'NONE',  ( 148.1316126177475496, 276.0755160693871630, 5.020219949272568094 ) ) ;
#85406 = DIRECTION ( 'NONE',  ( -0.3715724127386920705, 0.6435822975543701308, -0.6691306063588670083 ) ) ;
#85407 = CARTESIAN_POINT ( 'NONE',  ( 185.8122761056181105, 286.6146716806434256, 15.85193406119726056 ) ) ;
#85408 = CARTESIAN_POINT ( 'NONE',  ( 74.02866129013209218, 68.91877476116354728, -11.13505360475025263 ) ) ;
#85409 = CARTESIAN_POINT ( 'NONE',  ( 37.90188877791127453, 186.5643266524160424, 9.188101187500095079 ) ) ;
#85410 = CARTESIAN_POINT ( 'NONE',  ( 121.9060058492368483, 247.3149278399160949, -9.188101187500095079 ) ) ;
#85411 = CIRCLE ( 'NONE', #41681, 0.1418229129680828593 ) ;
#85412 = CARTESIAN_POINT ( 'NONE',  ( 199.4572827948314284, 277.5277167264244440, 15.18863414768032349 ) ) ;
#85413 = VERTEX_POINT ( 'NONE', #68962 ) ;
#85414 = CARTESIAN_POINT ( 'NONE',  ( 152.0058074760499665, 272.8430352715865865, -11.69865300651101592 ) ) ;
#85415 = LINE ( 'NONE', #32667, #43641 ) ;
#85416 = VECTOR ( 'NONE', #94587, 1000.000000000000000 ) ;
#85417 = DIRECTION ( 'NONE',  ( 0.000000000000000000, 0.000000000000000000, 1.000000000000000000 ) ) ;
#85418 = CARTESIAN_POINT ( 'NONE',  ( 80.35245384971769056, 57.10990684815718765, -16.23186976984165852 ) ) ;
#85419 = AXIS2_PLACEMENT_3D ( 'NONE', #53992, #46397, #38301 ) ;
#85420 = CARTESIAN_POINT ( 'NONE',  ( 155.0929244053699847, 262.0181703658971628, 18.51426604808664678 ) ) ;
#85421 = CARTESIAN_POINT ( 'NONE',  ( 58.11799575139567509, 214.3615022471903160, 5.000000000000046185 ) ) ;
#85422 = CARTESIAN_POINT ( 'NONE',  ( 189.5680078729632214, 284.4452857818997131, 16.60658711706803103 ) ) ;
#85423 = FACE_OUTER_BOUND ( 'NONE', #31373, .T. ) ;
#85424 = CARTESIAN_POINT ( 'NONE',  ( 71.08204727005846735, 61.55506161651749153, 14.86215617804459832 ) ) ;
#85425 = CARTESIAN_POINT ( 'NONE',  ( 171.2717486985798701, 279.7763900546701166, 13.89510435958859524 ) ) ;
#85426 = LINE ( 'NONE', #8875, #92830 ) ;
#85427 = CARTESIAN_POINT ( 'NONE',  ( 67.69237348538018750, 66.82088825431439716, 8.559571887000263501 ) ) ;
#85428 = CARTESIAN_POINT ( 'NONE',  ( 189.8136646974935786, 301.8800841035353528, -0.6430783927310335102 ) ) ;
#85429 = LINE ( 'NONE', #8878, #31805 ) ;
#85430 = ORIENTED_EDGE ( 'NONE', *, *, #68774, .T. ) ;
#85431 = CARTESIAN_POINT ( 'NONE',  ( 183.8836432619000050, 293.1766604090298074, 10.99787141183991501 ) ) ;
#85432 = VECTOR ( 'NONE', #91139, 1000.000000000000000 ) ;
#85433 =( BOUNDED_CURVE ( )  B_SPLINE_CURVE ( 2, ( #39245, #55942, #85421, #765, #85941, #70667, #16467, #47363, #78286 ),
 .UNSPECIFIED., .F., .T. ) 
 B_SPLINE_CURVE_WITH_KNOTS ( ( 3, 2, 2, 2, 3 ),
 ( 0.4717741935483871218, 0.4731182795698924970, 0.4758064516129032473, 0.4784946236559139976, 0.4798387096774193727 ),
 .UNSPECIFIED. ) 
 CURVE ( )  GEOMETRIC_REPRESENTATION_ITEM ( )  RATIONAL_B_SPLINE_CURVE ( ( 0.9330127018922194093, 0.9330127018922194093, 1.000000000000000000, 0.8660254037844387076, 1.000000000000000000, 0.8660254037844387076, 1.000000000000000000, 0.9330127018922194093, 0.9330127018922194093 ) ) 
 REPRESENTATION_ITEM ( '' )  );
#85434 = PLANE ( 'NONE',  #19090 ) ;
#85435 = CARTESIAN_POINT ( 'NONE',  ( 119.3082767336485404, 233.5643266524159856, -9.188101187500093303 ) ) ;
#85436 = CARTESIAN_POINT ( 'NONE',  ( 10.03310832875943603, 27.83396525600388571, -2.839279412974133887 ) ) ;
#85437 = CARTESIAN_POINT ( 'NONE',  ( 151.2648146047323507, 268.6486510375538614, 15.71323890031163550 ) ) ;
#85438 = CYLINDRICAL_SURFACE ( 'NONE', #7962, 70.00000000000002842 ) ;
#85439 = AXIS2_PLACEMENT_3D ( 'NONE', #100267, #1466, #3472 ) ;
#85441 = CARTESIAN_POINT ( 'NONE',  ( 192.5936405006954431, 277.6276709648686847, 16.42609391667364704 ) ) ;
#85440 = CARTESIAN_POINT ( 'NONE',  ( 39.25774830830064843, 55.25619937740605536, 10.00000000000000000 ) ) ;
#85442 = CARTESIAN_POINT ( 'NONE',  ( 204.6717125599631686, 272.9637062319359870, -9.753211108311461430 ) ) ;
#85443 = CARTESIAN_POINT ( 'NONE',  ( 151.1126408083691501, 268.9122237844355254, -15.82705194100464396 ) ) ;
#85444 = DIRECTION ( 'NONE',  ( 0.4999999999999998890, -0.8660254037844385966, 0.000000000000000000 ) ) ;
#85445 = FACE_OUTER_BOUND ( 'NONE', #82345, .T. ) ;
#85446 = DIRECTION ( 'NONE',  ( -1.000000000000000000, -1.804112415015878589E-15, 0.000000000000000000 ) ) ;
#85447 = CARTESIAN_POINT ( 'NONE',  ( 81.35996782917339942, 56.22057934968196946, -16.44131086233301531 ) ) ;
#85448 = VERTEX_POINT ( 'NONE', #83719 ) ;
#85449 = DIRECTION ( 'NONE',  ( -0.8660254037844387076, -0.4999999999999998890, -0.000000000000000000 ) ) ;
#85450 = VECTOR ( 'NONE', #39948, 1000.000000000000000 ) ;
#85451 = DIRECTION ( 'NONE',  ( 1.000000000000000000, 0.000000000000000000, 0.000000000000000000 ) ) ;
#85452 = CARTESIAN_POINT ( 'NONE',  ( 199.2928477948540547, 269.7932124880637161, 9.247559850577539819 ) ) ;
#85453 = CARTESIAN_POINT ( 'NONE',  ( 149.4965729687386045, 271.7113353911534546, -11.48413836595348059 ) ) ;
#85454 = ORIENTED_EDGE ( 'NONE', *, *, #2735, .F. ) ;
#85455 = EDGE_CURVE ( 'NONE', #10482, #30385, #52931, .T. ) ;
#85456 = CARTESIAN_POINT ( 'NONE',  ( 79.22961533192220429, 50.25035061149957727, 14.80838524028136050 ) ) ;
#85457 = CARTESIAN_POINT ( 'NONE',  ( 75.28650001057752661, 66.67572118895705557, 13.44401380721711270 ) ) ;
#85458 = EDGE_CURVE ( 'NONE', #51698, #78822, #76106, .T. ) ;
#85459 = CARTESIAN_POINT ( 'NONE',  ( 189.3832291599495079, 300.6256203239445313, 1.753828516883770838 ) ) ;
#85460 = DIRECTION ( 'NONE',  ( -0.8660254037844387076, -0.4999999999999998890, -0.000000000000000000 ) ) ;
#85461 = VECTOR ( 'NONE', #76889, 1000.000000000000114 ) ;
#85462 = ORIENTED_EDGE ( 'NONE', *, *, #6421, .T. ) ;
#85463 = CARTESIAN_POINT ( 'NONE',  ( 190.1875296108910334, 280.4995553090359408, 16.63324803487314796 ) ) ;
#85464 = EDGE_CURVE ( 'NONE', #65130, #18732, #28993, .T. ) ;
#85465 = CARTESIAN_POINT ( 'NONE',  ( 43.56148901884012048, 27.01110640527296169, 2.839279412974134775 ) ) ;
#85466 = VERTEX_POINT ( 'NONE', #6680 ) ;
#85467 = CARTESIAN_POINT ( 'NONE',  ( 167.6493030671569500, 249.8575448609487921, 6.851470149181726477 ) ) ;
#85468 = EDGE_CURVE ( 'NONE', #36195, #92664, #98888, .T. ) ;
#85469 = DIRECTION ( 'NONE',  ( 0.4999999999999992784, -0.8660254037844390407, 0.000000000000000000 ) ) ;
#85470 = ORIENTED_EDGE ( 'NONE', *, *, #45017, .F. ) ;
#85471 = FACE_OUTER_BOUND ( 'NONE', #52764, .T. ) ;
#85472 = CARTESIAN_POINT ( 'NONE',  ( 147.8527080755910958, 276.5585929068648170, -2.411454450074328903 ) ) ;
#85473 = FACE_OUTER_BOUND ( 'NONE', #15904, .T. ) ;
#85474 = DIRECTION ( 'NONE',  ( 0.000000000000000000, -0.000000000000000000, -1.000000000000000000 ) ) ;
#85475 = CARTESIAN_POINT ( 'NONE',  ( -52.58585057098314053, 88.59772970696691630, -10.00000000000000000 ) ) ;
#85476 = CARTESIAN_POINT ( 'NONE',  ( 80.33241032415608629, 44.91708578747144287, 11.19148706010553163 ) ) ;
#85477 = CARTESIAN_POINT ( 'NONE',  ( 86.32721218574307898, 47.55264674982593931, -11.12316258729872054 ) ) ;
#85478 = ORIENTED_EDGE ( 'NONE', *, *, #98104, .F. ) ;
#85479 = CARTESIAN_POINT ( 'NONE',  ( 201.3363518313238956, 277.3271591401824026, -15.70882811787338618 ) ) ;
#85480 = ORIENTED_EDGE ( 'NONE', *, *, #4454, .F. ) ;
#85481 = CARTESIAN_POINT ( 'NONE',  ( 81.32396741884589630, 55.80035763937271298, 16.38826086546822580 ) ) ;
#85482 = ORIENTED_EDGE ( 'NONE', *, *, #47166, .F. ) ;
#85483 = CARTESIAN_POINT ( 'NONE',  ( 169.7343602353587926, 269.2857159740701150, 16.89834073576611573 ) ) ;
#85484 = ORIENTED_EDGE ( 'NONE', *, *, #13656, .F. ) ;
#85485 = CARTESIAN_POINT ( 'NONE',  ( 165.4473470637335879, 246.0837842385732301, 3.196113342258863899 ) ) ;
#85486 = CARTESIAN_POINT ( 'NONE',  ( 46.43574122514301195, 74.10519008736565638, 10.00000000000000000 ) ) ;
#85487 = FACE_OUTER_BOUND ( 'NONE', #80616, .T. ) ;
#85488 = FACE_OUTER_BOUND ( 'NONE', #64495, .T. ) ;
#85489 = CARTESIAN_POINT ( 'NONE',  ( 82.57480368249606784, 41.04376301281223505, 1.111617510708537093 ) ) ;
#85490 = VECTOR ( 'NONE', #95429, 1000.000000000000114 ) ;
#85491 = CARTESIAN_POINT ( 'NONE',  ( 168.0790033696603416, 248.3996430977109355, -4.949810391468747461 ) ) ;
#85492 = CARTESIAN_POINT ( 'NONE',  ( 76.71798530001490235, 63.32448642232582614, -15.43374014074777989 ) ) ;
#85493 = CARTESIAN_POINT ( 'NONE',  ( 178.0988699194678588, 255.3435402841193707, 5.564670213749401739 ) ) ;
#85494 = CARTESIAN_POINT ( 'NONE',  ( 123.3136442261515526, 235.8768266524159856, 9.188101187500098632 ) ) ;
#85495 = CARTESIAN_POINT ( 'NONE',  ( 70.40053591592641169, 61.13412726347223725, -14.87056803518813908 ) ) ;
#85496 = CARTESIAN_POINT ( 'NONE',  ( 160.7670569121125084, 283.7960714782474270, 2.206094026959618315 ) ) ;
#85497 = CARTESIAN_POINT ( 'NONE',  ( 177.9903043249979930, 289.2672226302933041, -9.336760805543203645 ) ) ;
#85498 = VECTOR ( 'NONE', #66168, 1000.000000000000227 ) ;
#85499 = EDGE_LOOP ( 'NONE', ( #74969, #28782, #94698, #2177 ) ) ;
#85500 = CONICAL_SURFACE ( 'NONE', #6189, 16.82106496071143908, 0.7853981633974241872 ) ;
#85501 = ORIENTED_EDGE ( 'NONE', *, *, #93047, .T. ) ;
#85502 = CARTESIAN_POINT ( 'NONE',  ( 200.2184649266326915, 273.7011556189854105, 13.93284857238957741 ) ) ;
#85503 = AXIS2_PLACEMENT_3D ( 'NONE', #80710, #14125, #83561 ) ;
#85504 = CARTESIAN_POINT ( 'NONE',  ( 177.7357342257776907, 253.3636629150184945, 1.391642827436562424 ) ) ;
#85505 = CARTESIAN_POINT ( 'NONE',  ( 171.0816347564833961, 287.7379295750013739, -5.004374939593263960 ) ) ;
#85506 = CARTESIAN_POINT ( 'NONE',  ( 196.1573359623355088, 290.8925231663144473, 17.55680092534192482 ) ) ;
#85507 = CARTESIAN_POINT ( 'NONE',  ( 72.07340273975241018, 61.96641754224930310, 14.42752318807301748 ) ) ;
#85508 = CARTESIAN_POINT ( 'NONE',  ( 201.1679199471075492, 282.2139371290980989, -16.62385308864941535 ) ) ;
#85509 = CARTESIAN_POINT ( 'NONE',  ( 173.4619051054469878, 287.5670256320814246, -9.876641005795255168 ) ) ;
#85510 = VERTEX_POINT ( 'NONE', #24865 ) ;
#85511 = CARTESIAN_POINT ( 'NONE',  ( 194.8191165606777702, 293.2103871616598099, 16.46019522012304037 ) ) ;
#85512 = CARTESIAN_POINT ( 'NONE',  ( 176.1919805722776005, 255.3928090292563695, -7.299666310701137917 ) ) ;
#85513=STYLED_ITEM('',(#100310),#77374);
#85514 = ORIENTED_EDGE ( 'NONE', *, *, #41856, .T. ) ;
#85515 = CARTESIAN_POINT ( 'NONE',  ( 194.7900911235093133, 293.2606606935473792, -14.66228443412922999 ) ) ;
#85516 = CARTESIAN_POINT ( 'NONE',  ( 65.74174769441147248, 69.08343887585857601, -0.02323972613207190424 ) ) ;
#85517 = VERTEX_POINT ( 'NONE', #25367 ) ;
#85518 = CARTESIAN_POINT ( 'NONE',  ( 188.5361412926528430, 265.1671748825110626, -11.87835921727136146 ) ) ;
#85519 = VECTOR ( 'NONE', #72161, 1000.000000000000000 ) ;
#85520 = CARTESIAN_POINT ( 'NONE',  ( 190.7968079096152110, 283.1981913049548325, -16.56890853126571983 ) ) ;
#85521 = CARTESIAN_POINT ( 'NONE',  ( 192.7845724167702031, 262.6087076098646094, 4.680582376611854833 ) ) ;
#85522 = CARTESIAN_POINT ( 'NONE',  ( 190.4249800432324662, 300.8212548652687133, 3.085047376053959400 ) ) ;
#85523 = EDGE_CURVE ( 'NONE', #23117, #65477, #27469, .T. ) ;
#85524 = DIRECTION ( 'NONE',  ( -0.9999990636452668058, -0.001368469433204066998, 0.000000000000000000 ) ) ;
#85526 = CARTESIAN_POINT ( 'NONE',  ( 154.8543500088721885, 277.6552608316904980, -8.992244201135354942 ) ) ;
#85525 = CARTESIAN_POINT ( 'NONE',  ( 162.1138636377163493, 281.8676824225443625, -6.599314908080229358 ) ) ;
#85527 = CARTESIAN_POINT ( 'NONE',  ( 200.6985908945154335, 283.0268388936558495, -17.74173253065502820 ) ) ;
#85528 = EDGE_LOOP ( 'NONE', ( #100106, #22013, #75203, #84356 ) ) ;
#85529 = CARTESIAN_POINT ( 'NONE',  ( 190.1693911629507738, 301.2639477917662703, -5.112716700269980485 ) ) ;
#85531 = CARTESIAN_POINT ( 'NONE',  ( 47.83996289752659692, 111.6306699247848968, 10.00000000000000000 ) ) ;
#85530 = B_SPLINE_SURFACE_WITH_KNOTS ( 'NONE', 3, 1, ( 
 ( #2701, #72611 ),
 ( #51257, #4168 ),
 ( #95932, #26492 ),
 ( #18901, #96419 ),
 ( #4681, #26986 ),
 ( #88848, #19413 ),
 ( #50270, #81223 ),
 ( #58362, #11799 ),
 ( #74602, #13763 ),
 ( #83199, #84210 ),
 ( #68450, #92304 ),
 ( #97887, #61345 ),
 ( #53255, #22853 ),
 ( #75085, #99378 ),
 ( #82721, #45638 ),
 ( #53737, #37544 ),
 ( #84696, #90319 ),
 ( #59340, #68945 ),
 ( #5665, #91794 ),
 ( #37058, #91296 ),
 ( #29957, #7147 ),
 ( #76566, #13290 ),
 ( #15236, #28979 ),
 ( #76093, #44150 ),
 ( #36554, #60834 ),
 ( #60338, #14756 ),
 ( #59855, #38034 ),
 ( #99870, #98883 ),
 ( #22358, #44642 ),
 ( #51781, #30456 ),
 ( #5176, #36056 ),
 ( #67460, #52258 ),
 ( #98388, #66958 ),
 ( #14263, #6667 ) ),
 .UNSPECIFIED., .T., .F., .F.,
 ( 4, 2, 2, 2, 2, 2, 2, 2, 2, 2, 2, 2, 2, 2, 2, 2, 4 ),
 ( 2, 2 ),
 ( 0.000000000000000000, 0.06250000000000000000, 0.1250000000000000000, 0.1875000000000000000, 0.2500000000000000000, 0.3125000000000000000, 0.3750000000000000000, 0.4375000000000000000, 0.5000000000000000000, 0.5625000000000000000, 0.6250000000000000000, 0.6875000000000000000, 0.7500000000000000000, 0.8125000000000000000, 0.8750000000000000000, 0.9375000000000000000, 1.000000000000000000 ),
 ( 0.000000000000000000, 1.000000000000000000 ),
 .UNSPECIFIED. ) ;
#85532 = CARTESIAN_POINT ( 'NONE',  ( 187.3763199732122189, 261.5962347827016288, -9.077379491631687003 ) ) ;
#85533 = CARTESIAN_POINT ( 'NONE',  ( 118.2400530232016251, 250.6199935810940929, 2.679491924311251605 ) ) ;
#85534 = FACE_OUTER_BOUND ( 'NONE', #58591, .T. ) ;
#85535 = CARTESIAN_POINT ( 'NONE',  ( 188.2004726365935880, 299.2930532709519866, -3.673125411237516680 ) ) ;
#85536 = CARTESIAN_POINT ( 'NONE',  ( 204.3518858691784885, 276.1737321026752170, 13.13371718507185015 ) ) ;
#85537 = CARTESIAN_POINT ( 'NONE',  ( 44.44844410339183582, 68.22168590943847732, 10.00000000000000000 ) ) ;
#85538 = CARTESIAN_POINT ( 'NONE',  ( 74.41143754142076716, 68.29725791098579180, 11.39274163773210446 ) ) ;
#85539 = CARTESIAN_POINT ( 'NONE',  ( 68.07599697842495345, 69.84362665757917910, 1.500371073846174408 ) ) ;
#85540 = VECTOR ( 'NONE', #44905, 1000.000000000000227 ) ;
#85541 = CARTESIAN_POINT ( 'NONE',  ( 68.59054070044055607, 66.75779901073921963, -10.13948842260730743 ) ) ;
#85542 = CARTESIAN_POINT ( 'NONE',  ( 97.33288211261837830, 220.8768266524160140, 9.188101187500098632 ) ) ;
#85543 = LINE ( 'NONE', #87054, #37883 ) ;
#85544 = CARTESIAN_POINT ( 'NONE',  ( 193.1028332910263998, 296.1830769848763225, -12.04975758233223893 ) ) ;
#85545 = CARTESIAN_POINT ( 'NONE',  ( -50.41871976035449165, 31.58591985673634639, -10.00000000000000000 ) ) ;
#85546 = ADVANCED_FACE ( 'NONE', ( #47159 ), #54751, .T. ) ;
#85547 = CARTESIAN_POINT ( 'NONE',  ( 155.0304386007204016, 262.1263989543018056, -17.12961552904782181 ) ) ;
#85548 = AXIS2_PLACEMENT_3D ( 'NONE', #88790, #19359, #50219 ) ;
#85549 = CARTESIAN_POINT ( 'NONE',  ( 33.47037235539275457, 49.41749479597460493, 10.00000000000000000 ) ) ;
#85550 = FILL_AREA_STYLE ('',( #8991 ) ) ;
#85551 = CARTESIAN_POINT ( 'NONE',  ( 37.69969047124883588, 204.1199935810940644, 2.679491924311303119 ) ) ;
#85553 = CARTESIAN_POINT ( 'NONE',  ( 76.14697209829881785, 51.34588985376412751, 15.63759721918819778 ) ) ;
#85552 = CARTESIAN_POINT ( 'NONE',  ( 73.44884507967250897, 69.80860085198864340, -9.835095417347671898 ) ) ;
#85554 = CARTESIAN_POINT ( 'NONE',  ( -17.81126293257622706, 23.08927765589692527, 10.00000000000000000 ) ) ;
#85555 = CARTESIAN_POINT ( 'NONE',  ( -4.831225789733595732, 168.0177522451418781, -10.00000000000009592 ) ) ;
#85556 = CARTESIAN_POINT ( 'NONE',  ( 164.3918206888665168, 245.9120095485675392, -4.218277793461358449 ) ) ;
#85557 = CARTESIAN_POINT ( 'NONE',  ( 157.1135969804030310, 258.5182628004787944, 17.19660297500358226 ) ) ;
#85558 = DIRECTION ( 'NONE',  ( 0.000000000000000000, 0.000000000000000000, 1.000000000000000000 ) ) ;
#85559 = CARTESIAN_POINT ( 'NONE',  ( 38.93012039702277605, 193.2833772461660544, -9.188101187500095079 ) ) ;
#85560 = AXIS2_PLACEMENT_3D ( 'NONE', #49477, #11006, #22566 ) ;
#85561 = CARTESIAN_POINT ( 'NONE',  ( 74.00414925029257063, 213.5333772461660544, 9.188101187500095079 ) ) ;
#85562 = CARTESIAN_POINT ( 'NONE',  ( 164.4567835344609534, 247.2182797030277754, -7.041210626572695475 ) ) ;
#85563 = CARTESIAN_POINT ( 'NONE',  ( 88.22650267082845232, 44.11417692641830968, 0.5019829077109546622 ) ) ;
#85564 = AXIS2_PLACEMENT_3D ( 'NONE', #61435, #38119, #15834 ) ;
#85565 = CARTESIAN_POINT ( 'NONE',  ( 83.67203105669065621, 49.52337951222926193, -13.28627613491497605 ) ) ;
#85566 = CARTESIAN_POINT ( 'NONE',  ( 149.2944063396847412, 250.8768266524159856, 9.188101187500098632 ) ) ;
#85567 = CARTESIAN_POINT ( 'NONE',  ( 77.06710730379538177, 49.53326525838865280, 15.49076735042929442 ) ) ;
#85568 = B_SPLINE_CURVE_WITH_KNOTS ( 'NONE', 3,
 ( #17374, #55356, #79723, #87364 ),
 .UNSPECIFIED., .F., .F.,
 ( 4, 4 ),
 ( 0.01386548592622738850, 0.02021667511850969504 ),
 .UNSPECIFIED. ) ;
#85569 = CIRCLE ( 'NONE', #48357, 49.99999999999999289 ) ;
#85570 = CARTESIAN_POINT ( 'NONE',  ( 196.3099158349245670, 269.5646035672020844, -10.80014497079675451 ) ) ;
#85571 = CARTESIAN_POINT ( 'NONE',  ( 23.88951478931043937, 35.83396525600391413, -2.839279412974133887 ) ) ;
#85572 = LINE ( 'NONE', #32311, #41772 ) ;
#85573 = CARTESIAN_POINT ( 'NONE',  ( 149.1429535397850827, 272.3238222086447990, -12.91457852089092384 ) ) ;
#85574 = CARTESIAN_POINT ( 'NONE',  ( 9.878523645489616811, 21.10171378149917487, 9.188101187500008038 ) ) ;
#85575 = CARTESIAN_POINT ( 'NONE',  ( 65.61435460324828739, 214.8149278399160664, 9.188101187500093303 ) ) ;
#85576 = CARTESIAN_POINT ( 'NONE',  ( 77.23319965423435463, 63.36835149973478565, 15.13843137913277914 ) ) ;
#85577 = CARTESIAN_POINT ( 'NONE',  ( 203.3041373168503299, 278.5139001086923827, -16.61929732091214973 ) ) ;
#85578 = VECTOR ( 'NONE', #12548, 1000.000000000000114 ) ;
#85579 = CARTESIAN_POINT ( 'NONE',  ( 159.3169041484411537, 254.7020228407560580, 16.67170756419672628 ) ) ;
#85580 = CARTESIAN_POINT ( 'NONE',  ( 69.39596420143790567, 62.75002488050670024, -13.76244142531616887 ) ) ;
#85581 = CARTESIAN_POINT ( 'NONE',  ( 201.4223166756717660, 281.7733090699454692, 16.49648508032364091 ) ) ;
#85582 = EDGE_CURVE ( 'NONE', #21527, #9589, #33476, .T. ) ;
#85584 = CARTESIAN_POINT ( 'NONE',  ( 87.42519804963990282, 45.01967495469427405, -6.116160441020238814 ) ) ;
#85583 = VECTOR ( 'NONE', #61956, 1000.000000000000000 ) ;
#85585 = CARTESIAN_POINT ( 'NONE',  ( 107.5536125507574354, 226.2365022471902307, 10.00000000000009592 ) ) ;
#85586 = CARTESIAN_POINT ( 'NONE',  ( 183.8714358366006820, 278.0135913153196725, -17.80700656249756619 ) ) ;
#85587 = CARTESIAN_POINT ( 'NONE',  ( 164.9971748156432056, 244.8635054444190757, -1.825016704039769788 ) ) ;
#85588 = EDGE_LOOP ( 'NONE', ( #39965, #53622, #71749, #8573 ) ) ;
#85589 = DIRECTION ( 'NONE',  ( 0.2398044646550112069, 0.9708212084269294273, 0.000000000000000000 ) ) ;
#85590 = CARTESIAN_POINT ( 'NONE',  ( 82.31933756389703660, 53.70313499084333131, 15.83617117143144881 ) ) ;
#85591 = ORIENTED_EDGE ( 'NONE', *, *, #51700, .T. ) ;
#85592 = CARTESIAN_POINT ( 'NONE',  ( 159.3237119419271437, 254.6902313965507858, -15.56765445935501191 ) ) ;
#85593 = CARTESIAN_POINT ( 'NONE',  ( 190.0854368897034874, 279.3748410864815241, -17.22451792153772132 ) ) ;
#85594 = CARTESIAN_POINT ( 'NONE',  ( 67.55901250501347022, 68.59136760746119421, -5.217548882598939564 ) ) ;
#85595 = ADVANCED_FACE ( 'NONE', ( #64372 ), #86229, .T. ) ;
#85596 = ORIENTED_EDGE ( 'NONE', *, *, #12408, .F. ) ;
#85597 = CARTESIAN_POINT ( 'NONE',  ( 173.4062743000620515, 251.7440124803043204, -0.2412133965101034005 ) ) ;
#85598 = EDGE_LOOP ( 'NONE', ( #34390, #9708, #28341, #20832 ) ) ;
#85599 = CARTESIAN_POINT ( 'NONE',  ( -27.12601731895737700, 23.20384585402105770, 10.00000000000000000 ) ) ;
#85600 = CARTESIAN_POINT ( 'NONE',  ( 148.3625667886952044, 273.6754917110858401, -8.960758510948144462 ) ) ;
#85601 = CARTESIAN_POINT ( 'NONE',  ( 81.46486379701710234, 43.57149586615976489, 9.885361616454591882 ) ) ;
#85602 = VECTOR ( 'NONE', #99959, 1000.000000000000000 ) ;
#85603 = ORIENTED_EDGE ( 'NONE', *, *, #56178, .F. ) ;
#85604 = CARTESIAN_POINT ( 'NONE',  ( 32.62131273085646654, 21.76004757982090965, 5.678558825948272215 ) ) ;
#85605 = LINE ( 'NONE', #83922, #51699 ) ;
#85606 = CARTESIAN_POINT ( 'NONE',  ( 75.06349586682162567, 67.01194365216524318, -13.14257922886206664 ) ) ;
#85607 = ORIENTED_EDGE ( 'NONE', *, *, #22347, .T. ) ;
#85608 = CARTESIAN_POINT ( 'NONE',  ( 138.7305270869972560, 244.2365022471902307, 10.00000000000009948 ) ) ;
#85609 = CARTESIAN_POINT ( 'NONE',  ( 159.8946522441011382, 253.7013337850969492, -16.68230890105693121 ) ) ;
#85610 = ORIENTED_EDGE ( 'NONE', *, *, #76368, .F. ) ;
#85611 = CARTESIAN_POINT ( 'NONE',  ( 174.4457123674840489, 286.1056755372895850, 10.49813771419831987 ) ) ;
#85612 = CARTESIAN_POINT ( 'NONE',  ( 67.84042995000689302, 66.00558543355286645, -10.46828802347326359 ) ) ;
#85613 = CARTESIAN_POINT ( 'NONE',  ( 81.57878911124544175, 55.16394943497986958, -15.91603754490293632 ) ) ;
#85614 = CARTESIAN_POINT ( 'NONE',  ( 204.8762144138505903, 275.7909827032724479, 14.60855957933206817 ) ) ;
#85615 = CARTESIAN_POINT ( 'NONE',  ( 35.44051388448051654, 36.16454794089043645, -10.00000000000000355 ) ) ;
#85616 = CARTESIAN_POINT ( 'NONE',  ( 205.2937235227012707, 275.0678357141204629, -12.80017165135291535 ) ) ;
#85617 = CARTESIAN_POINT ( 'NONE',  ( 136.3579783227721691, 249.5333772461660544, 9.188101187500095079 ) ) ;
#85618 = CARTESIAN_POINT ( 'NONE',  ( 206.4254562207697461, 270.5990383981129526, 2.448344251486097356 ) ) ;
#85619 = CARTESIAN_POINT ( 'NONE',  ( 195.7512027426080294, 291.1991186218746748, -15.77572119551195939 ) ) ;
#85620 = CARTESIAN_POINT ( 'NONE',  ( 72.92127039979699532, 225.1589784336661637, -6.496448406907675876E-16 ) ) ;
#85621 = ORIENTED_EDGE ( 'NONE', *, *, #94713, .T. ) ;
#85622 = CARTESIAN_POINT ( 'NONE',  ( 190.7851866479434761, 300.1973587246873194, 7.931162401707728016 ) ) ;
#85623 = CARTESIAN_POINT ( 'NONE',  ( 191.2649737798357705, 297.3663430354321235, 11.06343876070684296 ) ) ;
#85624 = VERTEX_POINT ( 'NONE', #70989 ) ;
#85625 = CARTESIAN_POINT ( 'NONE',  ( 196.1152085310149573, 290.9654900177533818, -16.34875648285824568 ) ) ;
#85626 = ORIENTED_EDGE ( 'NONE', *, *, #42615, .F. ) ;
#85627 = CARTESIAN_POINT ( 'NONE',  ( 66.81926193948103787, 67.91930224376029912, 6.999017448319921009 ) ) ;
#85628 = CARTESIAN_POINT ( 'NONE',  ( 72.84093999290330146, 56.97456911652175648, -16.40692799624909171 ) ) ;
#85629 = B_SPLINE_CURVE_WITH_KNOTS ( 'NONE', 3,
 ( #95599, #26643, #88006, #41828, #80387, #10957, #81385, #57526, #42811, #88502, #73252, #41644, #25455, #18371, #72587, #25977, #16851, #17352, #47251, #62953, #9266, #56847, #95421, #93903, #70551, #34076, #64967, #3193, #56343, #1678 ),
 .UNSPECIFIED., .F., .F.,
 ( 4, 2, 2, 2, 2, 2, 2, 2, 2, 2, 2, 2, 2, 2, 4 ),
 ( 0.0005501412985831557892, 0.001170896183476429191, 0.001791651068369702702, 0.003033160838156182502, 0.003653915723049342822, 0.003964293165495931873, 0.004041887526107601145, 0.004080684706413485220, 0.004119481886719368428, 0.004197076247331136579, 0.004274670607942904731, 0.004585048050390315606, 0.004895425492837726482, 0.005205802935285142562, 0.005516180377732559509 ),
 .UNSPECIFIED. ) ;
#85630 = CYLINDRICAL_SURFACE ( 'NONE', #28783, 10.00000000000001421 ) ;
#85631 = CARTESIAN_POINT ( 'NONE',  ( 81.14348526936038297, 56.16770390221125098, 16.10765411318869411 ) ) ;
#85632 = CARTESIAN_POINT ( 'NONE',  ( 54.99669585504140912, 195.8927522451417929, -10.00000000000009237 ) ) ;
#85633 = CARTESIAN_POINT ( 'NONE',  ( 158.9281150132903520, 281.5174227188211944, 6.950568428669476440 ) ) ;
#85634 = CARTESIAN_POINT ( 'NONE',  ( 78.44218234892278474, 228.3464784336661353, 1.353441290958777327E-15 ) ) ;
#85635 = ORIENTED_EDGE ( 'NONE', *, *, #99046, .F. ) ;
#85636 = ORIENTED_EDGE ( 'NONE', *, *, #31894, .T. ) ;
#85637 = CARTESIAN_POINT ( 'NONE',  ( 161.6469353826265660, 250.6662903599244316, -14.26861606608829902 ) ) ;
#85638 = VECTOR ( 'NONE', #57553, 1000.000000000000000 ) ;
#85639 = ORIENTED_EDGE ( 'NONE', *, *, #46259, .F. ) ;
#85640 = B_SPLINE_CURVE_WITH_KNOTS ( 'NONE', 3,
 ( #97222, #81525, #80535, #73895 ),
 .UNSPECIFIED., .F., .F.,
 ( 4, 4 ),
 ( 0.008124507445708663983, 0.01396828671364515329 ),
 .UNSPECIFIED. ) ;
#85641 = CARTESIAN_POINT ( 'NONE',  ( 76.45097149964601613, 51.61755418639809534, -15.65867827852782845 ) ) ;
#85642 = VECTOR ( 'NONE', #81810, 1000.000000000000000 ) ;
#85643 = CARTESIAN_POINT ( 'NONE',  ( 76.23134959265127009, 65.22726518599165502, -14.14128234971493647 ) ) ;
#85644 = AXIS2_PLACEMENT_3D ( 'NONE', #88095, #57113, #72861 ) ;
#85645 = CARTESIAN_POINT ( 'NONE',  ( 205.8379285891498682, 274.1252448892948905, 10.44730901608240181 ) ) ;
#85646 = EDGE_CURVE ( 'NONE', #14328, #37072, #78590, .T. ) ;
#85647 = CARTESIAN_POINT ( 'NONE',  ( -29.57042460543627982, 94.20560631922556638, 44.48281236311225939 ) ) ;
#85648 = DIRECTION ( 'NONE',  ( 0.000000000000000000, -0.000000000000000000, 1.000000000000000000 ) ) ;
#85649 = CARTESIAN_POINT ( 'NONE',  ( 159.5818694439545311, 259.7229583450298378, 16.67297602109374566 ) ) ;
#85650 = VECTOR ( 'NONE', #96727, 1000.000000000000000 ) ;
#85651 = EDGE_LOOP ( 'NONE', ( #95992, #36081, #61903, #97811 ) ) ;
#85652 = CARTESIAN_POINT ( 'NONE',  ( 158.0398765280698683, 259.7347367507720151, 17.70793151717339597 ) ) ;
#85653 = B_SPLINE_CURVE_WITH_KNOTS ( 'NONE', 3,
 ( #71765, #57029, #838, #79393 ),
 .UNSPECIFIED., .F., .F.,
 ( 4, 4 ),
 ( 0.04619905480260320940, 0.04887120950165262795 ),
 .UNSPECIFIED. ) ;
#85654 = LINE ( 'NONE', #37973, #35143 ) ;
#85655 = ADVANCED_FACE ( 'NONE', ( #9695 ), #6139, .F. ) ;
#85656 = CARTESIAN_POINT ( 'NONE',  ( 147.7401540708734728, 275.1386901812263659, -4.214051892962178414 ) ) ;
#85657 = CARTESIAN_POINT ( 'NONE',  ( 152.9273493951901628, 265.7690563111299298, -17.70273273795505631 ) ) ;
#85658 = CARTESIAN_POINT ( 'NONE',  ( 102.5355703512972809, 241.5530062829863027, -4.648177544792955347E-16 ) ) ;
#85659 = CARTESIAN_POINT ( 'NONE',  ( 72.02537281085561460, 67.13575061744317907, -11.13262944115481545 ) ) ;
#85660 = ORIENTED_EDGE ( 'NONE', *, *, #76595, .F. ) ;
#85661 = LINE ( 'NONE', #93746, #47761 ) ;
#85662 = VECTOR ( 'NONE', #65271, 1000.000000000000341 ) ;
#85663 = CARTESIAN_POINT ( 'NONE',  ( 181.8770762757046668, 291.4574127364229525, 9.786853623632657317 ) ) ;
#85664 = CARTESIAN_POINT ( 'NONE',  ( 72.22505610272034460, 71.11034894417089447, -5.995499026437220103 ) ) ;
#85665 = CARTESIAN_POINT ( 'NONE',  ( 171.6338951559981183, 251.5524196502057634, 7.220225173970846733 ) ) ;
#85666 = CARTESIAN_POINT ( 'NONE',  ( 198.5095128836955212, 266.2414960645399447, 0.9413577709342229038 ) ) ;
#85667 = EDGE_CURVE ( 'NONE', #33229, #5854, #6993, .T. ) ;
#85668 = CARTESIAN_POINT ( 'NONE',  ( 156.5497824763685912, 272.6770023486104719, 14.78669166138748814 ) ) ;
#85669 = ORIENTED_EDGE ( 'NONE', *, *, #29555, .T. ) ;
#85670 = FACE_OUTER_BOUND ( 'NONE', #95825, .T. ) ;
#85671 = CARTESIAN_POINT ( 'NONE',  ( 162.8037981520209314, 248.6625452659484381, 9.809699077002424161 ) ) ;
#85672 = VECTOR ( 'NONE', #36167, 1000.000000000000000 ) ;
#85673 = CARTESIAN_POINT ( 'NONE',  ( 164.7243055739305078, 245.3361288348881999, -1.445094907380085170 ) ) ;
#85675 = FACE_BOUND ( 'NONE', #23882, .T. ) ;
#85674 = CARTESIAN_POINT ( 'NONE',  ( 178.2593621835967497, 264.8045418315043094, -15.94341754528856292 ) ) ;
#85676 = CARTESIAN_POINT ( 'NONE',  ( 175.8611927472028640, 285.7234504611549255, -13.40660829471084980 ) ) ;
#85677 = CARTESIAN_POINT ( 'NONE',  ( 33.32252067603396029, 20.20801979619930577, -3.090169943749474069 ) ) ;
#85678 = EDGE_CURVE ( 'NONE', #35956, #27521, #21271, .T. ) ;
#85679 = CARTESIAN_POINT ( 'NONE',  ( 169.1077096135931015, 273.0669116561859937, 15.96758563191977665 ) ) ;
#85680 = CARTESIAN_POINT ( 'NONE',  ( 166.4590851264997582, 286.5435392614748480, -3.277556783383077654 ) ) ;
#85681 = CARTESIAN_POINT ( 'NONE',  ( -45.75347490765856406, 28.11296735934751823, 177.5919119679930134 ) ) ;
#85682 = CARTESIAN_POINT ( 'NONE',  ( 188.3874671557833551, 260.9085831127977144, 2.874786128283515207 ) ) ;
#85683 = CARTESIAN_POINT ( 'NONE',  ( 207.8996209429610360, 270.5542889829179103, -5.987818313449536411 ) ) ;
#85684 = CARTESIAN_POINT ( 'NONE',  ( -7.673045192009834814, 172.5024278399160664, -9.188101187500093303 ) ) ;
#85685 = CARTESIAN_POINT ( 'NONE',  ( 148.4047294057049271, 273.6024639162449716, 1.815056976409021644E-15 ) ) ;
#85686 = ORIENTED_EDGE ( 'NONE', *, *, #3118, .F. ) ;
#85687 = CARTESIAN_POINT ( 'NONE',  ( 160.8493410219326165, 253.1035779242602928, -14.73755040960339002 ) ) ;
#85688 = B_SPLINE_CURVE_WITH_KNOTS ( 'NONE', 3,
 ( #77954, #24731, #78973, #71356, #8053, #47530, #23721, #24244, #54115, #62218 ),
 .UNSPECIFIED., .F., .F.,
 ( 4, 2, 2, 2, 4 ),
 ( 0.000000000000000000, 0.0002622400424272615296, 0.0005244800848545230591, 0.0007867201272817845887, 0.001048960169709046118 ),
 .UNSPECIFIED. ) ;
#85689 = DIRECTION ( 'NONE',  ( -0.8660254037844384856, -0.5000000000000004441, 0.000000000000000000 ) ) ;
#85690 = CARTESIAN_POINT ( 'NONE',  ( 151.0801312611820890, 268.9685319718947198, -15.83903210480701240 ) ) ;
#85691 = CARTESIAN_POINT ( 'NONE',  ( 21.71786549680706102, 183.3458772461660544, 9.188101187500095079 ) ) ;
#85692 = CARTESIAN_POINT ( 'NONE',  ( 62.31174343829394502, 218.3297689869269220, -2.679491924311252493 ) ) ;
#85693 = CARTESIAN_POINT ( 'NONE',  ( 31.78235740255998820, 30.30066082961423746, -10.00000000000000533 ) ) ;
#85694 = CARTESIAN_POINT ( 'NONE',  ( 193.8848781386269309, 267.1185884883711879, -11.59377028749509364 ) ) ;
#85695 = CARTESIAN_POINT ( 'NONE',  ( 191.8232488616404225, 298.3993822291468518, -9.342381338555176384 ) ) ;
#85696 = CARTESIAN_POINT ( 'NONE',  ( 81.52168578289229117, 56.03111392393292078, 16.05417868975104057 ) ) ;
#85697 = EDGE_CURVE ( 'NONE', #58741, #50517, #84335, .T. ) ;
#85698 = EDGE_CURVE ( 'NONE', #65030, #70217, #40604, .T. ) ;
#85699 = DIRECTION ( 'NONE',  ( -0.4999999999999987788, 0.8660254037844392627, 0.000000000000000000 ) ) ;
#85700 = CARTESIAN_POINT ( 'NONE',  ( 190.0214546701687652, 261.5450160817866845, -0.7541398968587580409 ) ) ;
#85701 = EDGE_CURVE ( 'NONE', #34750, #2250, #23846, .T. ) ;
#85702 = CARTESIAN_POINT ( 'NONE',  ( 70.67536410627003818, 221.6115022471903160, -5.000000000000047962 ) ) ;
#85703 = CARTESIAN_POINT ( 'NONE',  ( 164.5351584576669381, 246.1509890714488336, 1.273074117816153983 ) ) ;
#85704 = CARTESIAN_POINT ( 'NONE',  ( 203.3628419156056282, 270.1034488468966970, 6.158600121215549450 ) ) ;
#85705 = CARTESIAN_POINT ( 'NONE',  ( 27.69859311986958872, 195.9869531367911293, 4.594050593750046652 ) ) ;
#85706 = CARTESIAN_POINT ( 'NONE',  ( 169.2145527580371152, 252.8177965952870920, -11.54809748734068720 ) ) ;
#85707 = EDGE_CURVE ( 'NONE', #82473, #40420, #60090, .T. ) ;
#85708 = CARTESIAN_POINT ( 'NONE',  ( 202.9918396203695465, 270.0308483619746198, -6.392315799726350889 ) ) ;
#85709 = CARTESIAN_POINT ( 'NONE',  ( 198.8194531333411419, 286.2816009704309863, -17.01510935557533344 ) ) ;
#85711 = CARTESIAN_POINT ( 'NONE',  ( 67.16990927158769864, 66.79708245712438952, -9.067759095352206700 ) ) ;
#85710 = AXIS2_PLACEMENT_3D ( 'NONE', #913, #28951, #97862 ) ;
#85712 = ADVANCED_FACE ( 'NONE', ( #63253 ), #91121, .T. ) ;
#85713 = CARTESIAN_POINT ( 'NONE',  ( -5.006187249323398092, 179.4637435831425023, 2.679491924311264039 ) ) ;
#85714 = CARTESIAN_POINT ( 'NONE',  ( 202.7544846896944080, 279.0752537093788419, -15.21816053415730963 ) ) ;
#85715 = DIRECTION ( 'NONE',  ( -1.000000000000000000, 0.000000000000000000, 0.000000000000000000 ) ) ;
#85716 = CARTESIAN_POINT ( 'NONE',  ( 18.54180792094154029, 32.74646525600390135, 2.839279412974139660 ) ) ;
#85717 = CARTESIAN_POINT ( 'NONE',  ( 202.8499463704053198, 279.3005819042728604, 17.04674939340617001 ) ) ;
#85718 = CARTESIAN_POINT ( 'NONE',  ( 148.9194629746633893, 272.7109192224475009, -12.27648025871169679 ) ) ;
#85719 = CARTESIAN_POINT ( 'NONE',  ( 185.7622240277081289, 267.5937315954845417, -14.89893092516080841 ) ) ;
#85720 = EDGE_LOOP ( 'NONE', ( #40717, #65149, #34467, #40736 ) ) ;
#85721 = VECTOR ( 'NONE', #41015, 1000.000000000000000 ) ;
#85722 = CARTESIAN_POINT ( 'NONE',  ( 185.2961235551778714, 291.2460235572835927, 13.48139818756336616 ) ) ;
#85723 = CARTESIAN_POINT ( 'NONE',  ( 11.28581492663932906, 21.91421378149917487, 9.188101187500008038 ) ) ;
#85724 = ADVANCED_FACE ( 'NONE', ( #74382 ), #44970, .F. ) ;
#85725 = DIRECTION ( 'NONE',  ( 0.4999999999999992784, -0.8660254037844390407, 0.000000000000000000 ) ) ;
#85726 = CARTESIAN_POINT ( 'NONE',  ( 74.53866558554922506, 59.42414767716603308, -15.71004193905537250 ) ) ;
#85727 = CARTESIAN_POINT ( 'NONE',  ( 71.65515660876562265, 72.43366598492664821, -1.354044368658560815 ) ) ;
#85728 = CARTESIAN_POINT ( 'NONE',  ( 39.59743582264582784, 38.56454794089045635, 10.00000000000000355 ) ) ;
#85729 = ADVANCED_FACE ( 'NONE', ( #75873 ), #90601, .F. ) ;
#85730 = ORIENTED_EDGE ( 'NONE', *, *, #85697, .T. ) ;
#85731 = CARTESIAN_POINT ( 'NONE',  ( 177.4877928417686803, 293.5951873982637608, -2.837372163671336267 ) ) ;
#85732 = CARTESIAN_POINT ( 'NONE',  ( 72.32516777325903945, 71.91622842696713747, -5.210293257461823480 ) ) ;
#85733 = CARTESIAN_POINT ( 'NONE',  ( 150.7254409736883645, 269.5828735707850683, 14.54962197351449049 ) ) ;
#85734 = CARTESIAN_POINT ( 'NONE',  ( 84.69349035698814987, 42.09509699793907345, 3.525966048916779449 ) ) ;
#85735 =( BOUNDED_CURVE ( )  B_SPLINE_CURVE ( 2, ( #92486, #21091, #84889, #52953, #15429, #67660, #99568, #76278, #46327 ),
 .UNSPECIFIED., .F., .T. ) 
 B_SPLINE_CURVE_WITH_KNOTS ( ( 3, 2, 2, 2, 3 ),
 ( 0.7701612903225806273, 0.7715053763440860024, 0.7741935483870967527, 0.7768817204301075030, 0.7782258064516128782 ),
 .UNSPECIFIED. ) 
 CURVE ( )  GEOMETRIC_REPRESENTATION_ITEM ( )  RATIONAL_B_SPLINE_CURVE ( ( 0.9330127018922194093, 0.9330127018922194093, 1.000000000000000000, 0.8660254037844387076, 1.000000000000000000, 0.8660254037844387076, 1.000000000000000000, 0.9330127018922194093, 0.9330127018922194093 ) ) 
 REPRESENTATION_ITEM ( '' )  );
#85736 = ORIENTED_EDGE ( 'NONE', *, *, #47408, .F. ) ;
#85738 = CARTESIAN_POINT ( 'NONE',  ( 83.30637669978878534, 42.44484529871528622, -5.357148773537285358 ) ) ;
#85737 = CARTESIAN_POINT ( 'NONE',  ( 67.66242840994728169, 69.85685045095124224, 3.195176300350167420 ) ) ;
#85739 = B_SPLINE_CURVE_WITH_KNOTS ( 'NONE', 3,
 ( #13034, #43896, #84933, #39272, #31676, #31183, #71724, #86962, #1808, #61585, #70182, #40773, #93536, #1307, #62074, #46373, #24588, #8894, #62574, #70692, #790, #94038, #94534, #86460 ),
 .UNSPECIFIED., .F., .F.,
 ( 4, 2, 2, 2, 2, 2, 2, 2, 2, 2, 2, 4 ),
 ( 0.000000000000000000, 0.1250000000000079103, 0.2500000000000158207, 0.3750000000000237588, 0.4375000000000213718, 0.5000000000000189848, 0.5625000000000166533, 0.6250000000000142109, 0.6875000000000118794, 0.7500000000000094369, 0.8750000000000047740, 1.000000000000000000 ),
 .UNSPECIFIED. ) ;
#85740 = VERTEX_POINT ( 'NONE', #83988 ) ;
#85741 = CARTESIAN_POINT ( 'NONE',  ( 153.3939648708017387, 264.9608545997728015, -16.49556533540763681 ) ) ;
#85742 = CARTESIAN_POINT ( 'NONE',  ( 72.09323793696012217, 72.40190342410335234, -3.152634433464706287 ) ) ;
#85743 = CARTESIAN_POINT ( 'NONE',  ( 72.67720189414116305, 57.07760858790099689, -16.37924670756266110 ) ) ;
#85744 = CARTESIAN_POINT ( 'NONE',  ( 76.62413771374467331, 63.45693921867285070, 15.36854489724363759 ) ) ;
#85745 = CARTESIAN_POINT ( 'NONE',  ( 190.4744901378711290, 300.7355008658671522, 0.04566709859947504224 ) ) ;
#85746 = AXIS2_PLACEMENT_3D ( 'NONE', #87742, #19296, #95329 ) ;
#85747 = CARTESIAN_POINT ( 'NONE',  ( 180.3656040069006110, 287.1229193970689835, -13.78812687696878037 ) ) ;
#85748 = ORIENTED_EDGE ( 'NONE', *, *, #81679, .F. ) ;
#85749 = CARTESIAN_POINT ( 'NONE',  ( 195.9359860111818250, 291.2759125279654882, 17.49638312768267312 ) ) ;
#85750 = LINE ( 'NONE', #23369, #880 ) ;
#85751 = EDGE_LOOP ( 'NONE', ( #4987, #15760, #9963, #24774 ) ) ;
#85752 = CARTESIAN_POINT ( 'NONE',  ( 32.96772289237024012, 21.96004757982091959, -5.678558825948276656 ) ) ;
#85753 = CARTESIAN_POINT ( 'NONE',  ( 159.3767386493506137, 254.5983864451355032, 15.47015898230477760 ) ) ;
#85754 = DIRECTION ( 'NONE',  ( -0.8393827800519415572, -0.5435407515102007592, 0.000000000000000000 ) ) ;
#85755 = CARTESIAN_POINT ( 'NONE',  ( 61.79834339388186493, 215.6744531367911293, 4.594050593750047540 ) ) ;
#85756 = ORIENTED_EDGE ( 'NONE', *, *, #32439, .F. ) ;
#85757 = DIRECTION ( 'NONE',  ( 0.6833540297821637521, -0.7300871660154543141, 0.000000000000000000 ) ) ;
#85758 =( BOUNDED_CURVE ( )  B_SPLINE_CURVE ( 2, ( #46135, #77049, #70, #30953, #36557, #98391, #28983, #21374, #94299, #48158, #32951, #62847, #40544, #2579, #78072, #64359, #77577, #40038, #32463, #39036, #63856, #1065, #79099, #63359, #87239, #55727, #24853, #70454, #8658, #95322, #31445, #39530, #1580, #86715, #47147, #2072, #9683, #17253, #71479, #16256, #31944, #94794, #93803, #25879, #23844, #25355, #79607, #56247, #17773, #70979, #48674, #10170, #55234, #41037, #71974, #78578, #33464, #85200, #15743, #24363, #46650, #86218, #9163, #8165, #69946, #563, #62338, #93292, #54738, #85723, #57741, #5062, #10670, #95815, #64868, #42537, #20266, #27363, #41547, #97773, #35944, #26369, #72492, #18274, #43026, #73967, #19774, #57244, #51140, #34943, #27854, #4551, #33984, #88219, #66845, #89706, #12164, #50642, #35451, #65840, #3093, #82104, #12675, #88719, #58246, #43543, #56754, #87736, #66354, #97287, #81595, #73470, #19289, #49650, #49168, #74484, #80104, #18771, #80607, #11184, #42051, #72985, #3577, #34457, #65355, #96294, #26863, #50156, #81108, #11676, #4053, #96804, #89225, #14651, #5551, #28858, #7537, #99757, #84099, #91680, #76460, #30346, #52631, #61232, #84586, #29357, #29847, #92197, #69343, #76934, #45528, #68833, #53142, #14151, #91185, #21259, #28342, #15123, #38428, #21747, #60222, #75981, #83088, #90704, #67343, #22751, #46018, #75462, #7040, #44029, #45037, #6555, #53630, #59736, #52139, #98270, #98775, #60716, #22241, #59220, #90196, #20770, #51658, #83587, #37428, #82607, #37920, #13173, #74970, #68338, #67854, #6047, #13659, #36436, #44530, #36942, #99262, #48035, #9046, #32341, #25238, #17137, #24737, #63244, #94184, #31338, #47042, #87120, #46524, #77958, #61730, #71360, #39916, #8549, #62727, #100263, #48552, #86604, #62222, #70852, #63747, #93684, #56124, #55620, #32838, #54621, #47534, #40427, #94681, #78979, #69835, #1461, #9565, #17654, #79492, #38930, #93174, #10054, #1952, #40919, #39419, #86112, #78462, #30844, #92679, #77463, #447, #23231, #54119, #85078, #15625, #8057, #23726, #85604, #16143, #70337, #948, #31826, #24248, #55125, #16639, #58137, #12055, #96684, #57630, #34346, #64758, #12556, #58619, #81981, #65241, #3469, #10556, #66247, #51027, #41430, #88110, #89594, #41942, #3945, #95706, #88608, #50047, #97183, #2980, #33872, #72373, #72877, #34828, #65728, #42909, #27749, #96187, #26254, #71866, #81000, #33344, #57128, #20159, #18661, #27254, #11067, #49540, #80494, #2464, #26747, #19666, #56640, #50529, #11564, #89117, #64243, #19175, #81485, #42424, #95194, #73849, #4438, #73357, #35337, #25766, #87624, #18152, #49051, #79987, #5935, #43430, #92085, #29732, #5445, #83472, #6923, #60605, #97665, #91561, #59109, #43923, #82978, #99144, #13552, #52038, #13064, #52523, #22131, #99644, #22632, #82499, #74863, #37811, #45417, #44916, #44426, #90594, #53022, #68720, #53518, #83978, #66732, #21639, #36328, #84470, #4957, #14540, #76351, #6441, #51538, #30229, #67230, #61110, #14036, #74375, #35838, #20649, #98158, #28233, #28740, #59616, #37320, #21158, #75862, #75355, #36830, #67739, #98663, #29244, #60111, #91076, #68220, #78339, #38812, #17013, #46407, #39789, #16023, #55995, #7940, #69717, #62100, #70210, #62604, #324 ),
 .UNSPECIFIED., .F., .T. ) 
 B_SPLINE_CURVE_WITH_KNOTS ( ( 3, 2, 2, 2, 2, 2, 2, 2, 2, 2, 2, 2, 2, 2, 2, 2, 2, 2, 2, 2, 2, 2, 2, 2, 2, 2, 2, 2, 2, 2, 2, 2, 2, 2, 2, 2, 2, 2, 2, 2, 2, 2, 2, 2, 2, 2, 2, 2, 2, 2, 2, 2, 2, 2, 2, 2, 2, 2, 2, 2, 2, 2, 2, 2, 2, 2, 2, 2, 2, 2, 2, 2, 2, 2, 2, 2, 2, 2, 2, 2, 2, 2, 2, 2, 2, 2, 2, 2, 2, 2, 2, 2, 2, 2, 2, 2, 2, 2, 2, 2, 2, 2, 2, 2, 2, 2, 2, 2, 2, 2, 2, 2, 2, 2, 2, 2, 2, 2, 2, 2, 2, 2, 2, 2, 2, 2, 2, 2, 2, 2, 2, 2, 2, 2, 2, 2, 2, 2, 2, 2, 2, 2, 2, 2, 2, 2, 2, 2, 2, 2, 2, 2, 2, 2, 2, 2, 2, 2, 2, 2, 2, 2, 2, 2, 2, 2, 2, 2, 2, 2, 2, 2, 2, 2, 2, 2, 2, 2, 2, 2, 2, 2, 2, 2, 2, 2, 2, 2, 2, 2, 2, 2, 2, 2, 2, 2, 2, 2, 2, 2, 3 ),
 ( 0.000000000000000000, 0.005000000000000000104, 0.01000000000000000021, 0.01499999999999999944, 0.02000000000000000042, 0.02500000000000000139, 0.02999999999999999889, 0.03500000000000000333, 0.04000000000000000083, 0.04499999999999999833, 0.05000000000000000278, 0.05500000000000000028, 0.05999999999999999778, 0.06500000000000000222, 0.07000000000000000666, 0.07499999999999999722, 0.08000000000000000167, 0.08500000000000000611, 0.08999999999999999667, 0.09500000000000000111, 0.1000000000000000056, 0.1049999999999999961, 0.1100000000000000006, 0.1150000000000000050, 0.1199999999999999956, 0.1250000000000000000, 0.1300000000000000044, 0.1350000000000000089, 0.1400000000000000133, 0.1449999999999999900, 0.1499999999999999944, 0.1549999999999999989, 0.1600000000000000033, 0.1650000000000000078, 0.1700000000000000122, 0.1749999999999999889, 0.1799999999999999933, 0.1849999999999999978, 0.1900000000000000022, 0.1950000000000000067, 0.2000000000000000111, 0.2049999999999999878, 0.2099999999999999922, 0.2149999999999999967, 0.2200000000000000011, 0.2250000000000000056, 0.2300000000000000100, 0.2349999999999999867, 0.2399999999999999911, 0.2449999999999999956, 0.2500000000000000000, 0.2550000000000000044, 0.2600000000000000089, 0.2650000000000000133, 0.2700000000000000178, 0.2750000000000000222, 0.2800000000000000266, 0.2849999999999999756, 0.2899999999999999800, 0.2949999999999999845, 0.2999999999999999889, 0.3049999999999999933, 0.3099999999999999978, 0.3150000000000000022, 0.3200000000000000067, 0.3250000000000000111, 0.3300000000000000155, 0.3350000000000000200, 0.3400000000000000244, 0.3449999999999999734, 0.3499999999999999778, 0.3549999999999999822, 0.3599999999999999867, 0.3649999999999999911, 0.3699999999999999956, 0.3750000000000000000, 0.3800000000000000044, 0.3850000000000000089, 0.3900000000000000133, 0.3950000000000000178, 0.4000000000000000222, 0.4050000000000000266, 0.4099999999999999756, 0.4149999999999999800, 0.4199999999999999845, 0.4249999999999999889, 0.4299999999999999933, 0.4349999999999999978, 0.4400000000000000022, 0.4450000000000000067, 0.4500000000000000111, 0.4550000000000000155, 0.4600000000000000200, 0.4650000000000000244, 0.4699999999999999734, 0.4749999999999999778, 0.4799999999999999822, 0.4849999999999999867, 0.4899999999999999911, 0.4949999999999999956, 0.5000000000000000000, 0.5050000000000000044, 0.5100000000000000089, 0.5150000000000000133, 0.5200000000000000178, 0.5250000000000000222, 0.5300000000000000266, 0.5350000000000000311, 0.5400000000000000355, 0.5450000000000000400, 0.5500000000000000444, 0.5550000000000000488, 0.5600000000000000533, 0.5649999999999999467, 0.5699999999999999512, 0.5749999999999999556, 0.5799999999999999600, 0.5849999999999999645, 0.5899999999999999689, 0.5949999999999999734, 0.5999999999999999778, 0.6049999999999999822, 0.6099999999999999867, 0.6149999999999999911, 0.6199999999999999956, 0.6250000000000000000, 0.6300000000000000044, 0.6350000000000000089, 0.6400000000000000133, 0.6450000000000000178, 0.6500000000000000222, 0.6550000000000000266, 0.6600000000000000311, 0.6650000000000000355, 0.6700000000000000400, 0.6750000000000000444, 0.6800000000000000488, 0.6850000000000000533, 0.6899999999999999467, 0.6949999999999999512, 0.6999999999999999556, 0.7049999999999999600, 0.7099999999999999645, 0.7149999999999999689, 0.7199999999999999734, 0.7249999999999999778, 0.7299999999999999822, 0.7349999999999999867, 0.7399999999999999911, 0.7449999999999999956, 0.7500000000000000000, 0.7550000000000000044, 0.7600000000000000089, 0.7650000000000000133, 0.7700000000000000178, 0.7750000000000000222, 0.7800000000000000266, 0.7850000000000000311, 0.7900000000000000355, 0.7950000000000000400, 0.8000000000000000444, 0.8050000000000000488, 0.8100000000000000533, 0.8149999999999999467, 0.8199999999999999512, 0.8249999999999999556, 0.8299999999999999600, 0.8349999999999999645, 0.8399999999999999689, 0.8449999999999999734, 0.8499999999999999778, 0.8549999999999999822, 0.8599999999999999867, 0.8649999999999999911, 0.8699999999999999956, 0.8750000000000000000, 0.8800000000000000044, 0.8850000000000000089, 0.8900000000000000133, 0.8950000000000000178, 0.9000000000000000222, 0.9050000000000000266, 0.9100000000000000311, 0.9150000000000000355, 0.9200000000000000400, 0.9250000000000000444, 0.9300000000000000488, 0.9350000000000000533, 0.9399999999999999467, 0.9449999999999999512, 0.9499999999999999556, 0.9549999999999999600, 0.9599999999999999645, 0.9649999999999999689, 0.9699999999999999734, 0.9749999999999999778, 0.9799999999999999822, 0.9849999999999999867, 0.9899999999999999911, 0.9949999999999999956, 1.000000000000000000 ),
 .UNSPECIFIED. ) 
 CURVE ( )  GEOMETRIC_REPRESENTATION_ITEM ( )  RATIONAL_B_SPLINE_CURVE ( ( 1.000000000000000000, 0.9510565162951535312, 1.000000000000000000, 0.9510565162951535312, 1.000000000000000000, 0.9510565162951535312, 1.000000000000000000, 0.9510565162951535312, 1.000000000000000000, 0.9510565162951535312, 1.000000000000000000, 0.9510565162951535312, 1.000000000000000000, 0.9510565162951535312, 1.000000000000000000, 0.9510565162951535312, 1.000000000000000000, 0.9510565162951535312, 1.000000000000000000, 0.9510565162951535312, 1.000000000000000000, 0.9510565162951535312, 1.000000000000000000, 0.9510565162951535312, 1.000000000000000000, 0.9510565162951535312, 1.000000000000000000, 0.9510565162951535312, 1.000000000000000000, 0.9510565162951535312, 1.000000000000000000, 0.9510565162951535312, 1.000000000000000000, 0.9510565162951535312, 1.000000000000000000, 0.9510565162951535312, 1.000000000000000000, 0.9510565162951535312, 1.000000000000000000, 0.9510565162951535312, 1.000000000000000000, 0.9510565162951535312, 1.000000000000000000, 0.9510565162951535312, 1.000000000000000000, 0.9510565162951535312, 1.000000000000000000, 0.9510565162951535312, 1.000000000000000000, 0.9510565162951535312, 1.000000000000000000, 0.9510565162951535312, 1.000000000000000000, 0.9510565162951535312, 1.000000000000000000, 0.9510565162951535312, 1.000000000000000000, 0.9510565162951535312, 1.000000000000000000, 0.9510565162951535312, 1.000000000000000000, 0.9510565162951535312, 1.000000000000000000, 0.9510565162951535312, 1.000000000000000000, 0.9510565162951535312, 1.000000000000000000, 0.9510565162951535312, 1.000000000000000000, 0.9510565162951535312, 1.000000000000000000, 0.9510565162951535312, 1.000000000000000000, 0.9510565162951535312, 1.000000000000000000, 0.9510565162951535312, 1.000000000000000000, 0.9510565162951535312, 1.000000000000000000, 0.9510565162951535312, 1.000000000000000000, 0.9510565162951535312, 1.000000000000000000, 0.9510565162951535312, 1.000000000000000000, 0.9510565162951535312, 1.000000000000000000, 0.9510565162951535312, 1.000000000000000000, 0.9510565162951535312, 1.000000000000000000, 0.9510565162951535312, 1.000000000000000000, 0.9510565162951535312, 1.000000000000000000, 0.9510565162951535312, 1.000000000000000000, 0.9510565162951535312, 1.000000000000000000, 0.9510565162951535312, 1.000000000000000000, 0.9510565162951535312, 1.000000000000000000, 0.9510565162951535312, 1.000000000000000000, 0.9510565162951535312, 1.000000000000000000, 0.9510565162951535312, 1.000000000000000000, 0.9510565162951535312, 1.000000000000000000, 0.9510565162951535312, 1.000000000000000000, 0.9510565162951535312, 1.000000000000000000, 0.9510565162951535312, 1.000000000000000000, 0.9510565162951535312, 1.000000000000000000, 0.9510565162951535312, 1.000000000000000000, 0.9510565162951535312, 1.000000000000000000, 0.9510565162951535312, 1.000000000000000000, 0.9510565162951535312, 1.000000000000000000, 0.9510565162951535312, 1.000000000000000000, 0.9510565162951535312, 1.000000000000000000, 0.9510565162951535312, 1.000000000000000000, 0.9510565162951535312, 1.000000000000000000, 0.9510565162951535312, 1.000000000000000000, 0.9510565162951535312, 1.000000000000000000, 0.9510565162951535312, 1.000000000000000000, 0.9510565162951535312, 1.000000000000000000, 0.9510565162951535312, 1.000000000000000000, 0.9510565162951535312, 1.000000000000000000, 0.9510565162951535312, 1.000000000000000000, 0.9510565162951535312, 1.000000000000000000, 0.9510565162951535312, 1.000000000000000000, 0.9510565162951535312, 1.000000000000000000, 0.9510565162951535312, 1.000000000000000000, 0.9510565162951535312, 1.000000000000000000, 0.9510565162951535312, 1.000000000000000000, 0.9510565162951535312, 1.000000000000000000, 0.9510565162951535312, 1.000000000000000000, 0.9510565162951535312, 1.000000000000000000, 0.9510565162951535312, 1.000000000000000000, 0.9510565162951535312, 1.000000000000000000, 0.9510565162951535312, 1.000000000000000000, 0.9510565162951535312, 1.000000000000000000, 0.9510565162951535312, 1.000000000000000000, 0.9510565162951535312, 1.000000000000000000, 0.9510565162951535312, 1.000000000000000000, 0.9510565162951535312, 1.000000000000000000, 0.9510565162951535312, 1.000000000000000000, 0.9510565162951535312, 1.000000000000000000, 0.9510565162951535312, 1.000000000000000000, 0.9510565162951535312, 1.000000000000000000, 0.9510565162951535312, 1.000000000000000000, 0.9510565162951535312, 1.000000000000000000, 0.9510565162951535312, 1.000000000000000000, 0.9510565162951535312, 1.000000000000000000, 0.9510565162951535312, 1.000000000000000000, 0.9510565162951535312, 1.000000000000000000, 0.9510565162951535312, 1.000000000000000000, 0.9510565162951535312, 1.000000000000000000, 0.9510565162951535312, 1.000000000000000000, 0.9510565162951535312, 1.000000000000000000, 0.9510565162951535312, 1.000000000000000000, 0.9510565162951535312, 1.000000000000000000, 0.9510565162951535312, 1.000000000000000000, 0.9510565162951535312, 1.000000000000000000, 0.9510565162951535312, 1.000000000000000000, 0.9510565162951535312, 1.000000000000000000, 0.9510565162951535312, 1.000000000000000000, 0.9510565162951535312, 1.000000000000000000, 0.9510565162951535312, 1.000000000000000000, 0.9510565162951535312, 1.000000000000000000, 0.9510565162951535312, 1.000000000000000000, 0.9510565162951535312, 1.000000000000000000, 0.9510565162951535312, 1.000000000000000000, 0.9510565162951535312, 1.000000000000000000, 0.9510565162951535312, 1.000000000000000000, 0.9510565162951535312, 1.000000000000000000, 0.9510565162951535312, 1.000000000000000000, 0.9510565162951535312, 1.000000000000000000, 0.9510565162951535312, 1.000000000000000000, 0.9510565162951535312, 1.000000000000000000, 0.9510565162951535312, 1.000000000000000000, 0.9510565162951535312, 1.000000000000000000, 0.9510565162951535312, 1.000000000000000000, 0.9510565162951535312, 1.000000000000000000, 0.9510565162951535312, 1.000000000000000000, 0.9510565162951535312, 1.000000000000000000, 0.9510565162951535312, 1.000000000000000000, 0.9510565162951535312, 1.000000000000000000, 0.9510565162951535312, 1.000000000000000000, 0.9510565162951535312, 1.000000000000000000, 0.9510565162951535312, 1.000000000000000000, 0.9510565162951535312, 1.000000000000000000, 0.9510565162951535312, 1.000000000000000000, 0.9510565162951535312, 1.000000000000000000, 0.9510565162951535312, 1.000000000000000000, 0.9510565162951535312, 1.000000000000000000, 0.9510565162951535312, 1.000000000000000000, 0.9510565162951535312, 1.000000000000000000, 0.9510565162951535312, 1.000000000000000000, 0.9510565162951535312, 1.000000000000000000, 0.9510565162951535312, 1.000000000000000000, 0.9510565162951535312, 1.000000000000000000, 0.9510565162951535312, 1.000000000000000000, 0.9510565162951535312, 1.000000000000000000, 0.9510565162951535312, 1.000000000000000000, 0.9510565162951535312, 1.000000000000000000, 0.9510565162951535312, 1.000000000000000000, 0.9510565162951535312, 1.000000000000000000, 0.9510565162951535312, 1.000000000000000000, 0.9510565162951535312, 1.000000000000000000, 0.9510565162951535312, 1.000000000000000000, 0.9510565162951535312, 1.000000000000000000, 0.9510565162951535312, 1.000000000000000000, 0.9510565162951535312, 1.000000000000000000, 0.9510565162951535312, 1.000000000000000000, 0.9510565162951535312, 1.000000000000000000, 0.9510565162951535312, 1.000000000000000000, 0.9510565162951535312, 1.000000000000000000, 0.9510565162951535312, 1.000000000000000000, 0.9510565162951535312, 1.000000000000000000, 0.9510565162951535312, 1.000000000000000000, 0.9510565162951535312, 1.000000000000000000, 0.9510565162951535312, 1.000000000000000000, 0.9510565162951535312, 1.000000000000000000, 0.9510565162951535312, 1.000000000000000000, 0.9510565162951535312, 1.000000000000000000, 0.9510565162951535312, 1.000000000000000000, 0.9510565162951535312, 1.000000000000000000, 0.9510565162951535312, 1.000000000000000000, 0.9510565162951535312, 1.000000000000000000, 0.9510565162951535312, 1.000000000000000000, 0.9510565162951535312, 1.000000000000000000, 0.9510565162951535312, 1.000000000000000000, 0.9510565162951535312, 1.000000000000000000, 0.9510565162951535312, 1.000000000000000000, 0.9510565162951535312, 1.000000000000000000, 0.9510565162951535312, 1.000000000000000000, 0.9510565162951535312, 1.000000000000000000, 0.9510565162951535312, 1.000000000000000000, 0.9510565162951535312, 1.000000000000000000, 0.9510565162951535312, 1.000000000000000000, 0.9510565162951535312, 1.000000000000000000, 0.9510565162951535312, 1.000000000000000000, 0.9510565162951535312, 1.000000000000000000, 0.9510565162951535312, 1.000000000000000000, 0.9510565162951535312, 1.000000000000000000, 0.9510565162951535312, 1.000000000000000000, 0.9510565162951535312, 1.000000000000000000, 0.9510565162951535312, 1.000000000000000000, 0.9510565162951535312, 1.000000000000000000, 0.9510565162951535312, 1.000000000000000000, 0.9510565162951535312, 1.000000000000000000, 0.9510565162951535312, 1.000000000000000000, 0.9510565162951535312, 1.000000000000000000, 0.9510565162951535312, 1.000000000000000000 ) ) 
 REPRESENTATION_ITEM ( '' )  );
#85759 = CARTESIAN_POINT ( 'NONE',  ( 43.16562282991920085, 123.9487658730721904, 177.5919119679930134 ) ) ;
#85760 = CARTESIAN_POINT ( 'NONE',  ( 87.06313848696181878, 232.6199935810941213, 2.679491924311251605 ) ) ;
#85761 = DIRECTION ( 'NONE',  ( -0.000000000000000000, -0.000000000000000000, -1.000000000000000000 ) ) ;
#85762 = VERTEX_POINT ( 'NONE', #22643 ) ;
#85763 = EDGE_LOOP ( 'NONE', ( #28139, #38815, #87745, #25931 ) ) ;
#85764 = CARTESIAN_POINT ( 'NONE',  ( 190.2114739955665073, 299.5471927289356699, 6.539000334076677134 ) ) ;
#85765 = LINE ( 'NONE', #54271, #83647 ) ;
#85766 = DIRECTION ( 'NONE',  ( -0.1239754375649670948, -0.9922852870422774751, 0.000000000000000000 ) ) ;
#85767 = CARTESIAN_POINT ( 'NONE',  ( 190.5893431400089923, 300.5365696307625853, -0.3099240395267599535 ) ) ;
#85768 = VERTEX_POINT ( 'NONE', #68731 ) ;
#85769 = CARTESIAN_POINT ( 'NONE',  ( 149.0359194785865498, 272.5092106407810206, 12.76357969772040590 ) ) ;
#85770 = CARTESIAN_POINT ( 'NONE',  ( 35.39012114306879653, 16.59285393851897084, 10.00000000000000000 ) ) ;
#85771 = CARTESIAN_POINT ( 'NONE',  ( 207.8984236726843164, 270.5563627158673512, -6.084369154771423815 ) ) ;
#85772 = CARTESIAN_POINT ( 'NONE',  ( 192.5076277540105423, 297.2140032159341558, -13.10094381206144298 ) ) ;
#85773 = CARTESIAN_POINT ( 'NONE',  ( 160.5559693517773781, 255.9979613941079037, 15.97241449062581076 ) ) ;
#85774 = CARTESIAN_POINT ( 'NONE',  ( 69.95426054967219898, 67.58280296741347115, 9.346954025415000089 ) ) ;
#85775 = EDGE_CURVE ( 'NONE', #35245, #11947, #68231, .T. ) ;
#85776 = CARTESIAN_POINT ( 'NONE',  ( 206.4537138826727301, 273.0586734743599209, 11.45643784582899016 ) ) ;
#85777 = DIRECTION ( 'NONE',  ( 0.2803049773603250028, -0.9599109957006575211, 0.000000000000000000 ) ) ;
#85778 = CARTESIAN_POINT ( 'NONE',  ( 103.9969882237314351, 242.3967562850347122, -4.648177544792955347E-16 ) ) ;
#85779 = CARTESIAN_POINT ( 'NONE',  ( 78.51983995760878088, 47.43908030793226516, 14.25121724663956790 ) ) ;
#85780 = CARTESIAN_POINT ( 'NONE',  ( 114.1121243109418799, 230.5643266524159856, -9.188101187500093303 ) ) ;
#85781 = ORIENTED_EDGE ( 'NONE', *, *, #29723, .F. ) ;
#85782 = CARTESIAN_POINT ( 'NONE',  ( 146.9235493515124062, 276.1679430252639804, 0.7994986043261682607 ) ) ;
#85783 = CARTESIAN_POINT ( 'NONE',  ( 82.30608073536585323, 41.08216667689982415, -2.629353525907028644 ) ) ;
#85784 = CARTESIAN_POINT ( 'NONE',  ( 87.53367671268780725, 44.88112536278567433, -6.578546970659244764 ) ) ;
#85785 = CARTESIAN_POINT ( 'NONE',  ( 203.5258219653775313, 278.1299310341851765, -16.21052911601769608 ) ) ;
#85786 = CARTESIAN_POINT ( 'NONE',  ( 204.8284483594339065, 275.8737159363993214, 14.69997973035875383 ) ) ;
#85787 = CARTESIAN_POINT ( 'NONE',  ( -12.62545442379354554, 163.5177522451418781, -10.00000000000009592 ) ) ;
#85788 = CARTESIAN_POINT ( 'NONE',  ( 168.5060701671863796, 284.6850982760621491, -7.967140632246684895 ) ) ;
#85789 = ORIENTED_EDGE ( 'NONE', *, *, #47834, .F. ) ;
#85790 = CARTESIAN_POINT ( 'NONE',  ( 162.7007457333762090, 248.8410372908842021, -10.94671474643812914 ) ) ;
#85791 = CARTESIAN_POINT ( 'NONE',  ( 72.39889165046784569, 71.58181683135407525, 5.112090114424422183 ) ) ;
#85792 = CARTESIAN_POINT ( 'NONE',  ( 206.3712092866207968, 272.8206792488882115, 8.318967530036161406 ) ) ;
#85793 = CARTESIAN_POINT ( 'NONE',  ( 125.9117204375048544, 237.3768266524159856, 9.188101187500096856 ) ) ;
#85794 = ADVANCED_FACE ( 'NONE', ( #14552 ), #61121, .T. ) ;
#85795 = CARTESIAN_POINT ( 'NONE',  ( 190.0654709403812319, 294.6198108877256345, -12.35559205623138723 ) ) ;
#85796 = AXIS2_PLACEMENT_3D ( 'NONE', #82149, #36481, #12208 ) ;
#85797 = CARTESIAN_POINT ( 'NONE',  ( 185.8803129279731365, 296.7512827758666276, 4.593912753767370738 ) ) ;
#85798 = CARTESIAN_POINT ( 'NONE',  ( 196.3720681610792553, 290.5205960880691691, 16.18360420724715354 ) ) ;
#85799 = LINE ( 'NONE', #10241, #17468 ) ;
#85800 = CARTESIAN_POINT ( 'NONE',  ( 51.05482314576993730, 188.0327760586659451, 1.948934522072303157E-15 ) ) ;
#85801 = B_SPLINE_CURVE_WITH_KNOTS ( 'NONE', 3,
 ( #42800, #5332, #73735, #12951 ),
 .UNSPECIFIED., .F., .F.,
 ( 4, 4 ),
 ( 0.006434672157312129256, 0.01144118791506597635 ),
 .UNSPECIFIED. ) ;
#85802 = CARTESIAN_POINT ( 'NONE',  ( 85.55409210693744626, 48.30986647782642507, -11.71318688851061651 ) ) ;
#85803 = ORIENTED_EDGE ( 'NONE', *, *, #98843, .F. ) ;
#85804 = CARTESIAN_POINT ( 'NONE',  ( 70.76613391576567835, 62.53219004156024141, 13.77722632876776920 ) ) ;
#85805 = CARTESIAN_POINT ( 'NONE',  ( 79.58936028502597537, 59.22294857574252802, 16.56770033466462166 ) ) ;
#85806 = EDGE_CURVE ( 'NONE', #31218, #21771, #45912, .T. ) ;
#85807 = DIRECTION ( 'NONE',  ( 0.3956464567955564338, -0.9184028970038813355, 0.000000000000000000 ) ) ;
#85808 = EDGE_CURVE ( 'NONE', #8735, #70726, #83482, .T. ) ;
#85809 = CARTESIAN_POINT ( 'NONE',  ( 171.5340268345807146, 259.8473005894099970, 15.39510975745485233 ) ) ;
#85810 = DIRECTION ( 'NONE',  ( -0.000000000000000000, 0.000000000000000000, -1.000000000000000000 ) ) ;
#85811 = CARTESIAN_POINT ( 'NONE',  ( 154.8833801513861772, 262.3811116602312268, -17.49275566389638215 ) ) ;
#85812 = AXIS2_PLACEMENT_3D ( 'NONE', #22063, #68158, #83405 ) ;
#85813 = CARTESIAN_POINT ( 'NONE',  ( 155.2509783050690544, 269.7933175191985811, -14.93214736645873586 ) ) ;
#85814 = CARTESIAN_POINT ( 'NONE',  ( 109.5562962934609459, 247.3927522451419634, 2.944929066748280225E-16 ) ) ;
#85815 = B_SPLINE_SURFACE_WITH_KNOTS ( 'NONE', 3, 1, ( 
 ( #28978, #59854 ),
 ( #90817, #21370 ),
 ( #52256, #83198 ),
 ( #46132, #8160 ),
 ( #13761, #14755 ),
 ( #6161, #60832 ),
 ( #15739, #85195 ),
 ( #45637, #37057 ),
 ( #44640, #38544 ),
 ( #14262, #21859 ),
 ( #84209, #53736 ),
 ( #46647, #61839 ),
 ( #68943, #30454 ),
 ( #38033, #76565 ),
 ( #62335, #31441 ),
 ( #29462, #67964 ),
 ( #75574, #77572 ),
 ( #69451, #98882 ),
 ( #77045, #52741 ),
 ( #7146, #60337 ),
 ( #91294, #67 ),
 ( #39033, #6666 ),
 ( #83703, #45153 ),
 ( #76092, #37543 ),
 ( #22357, #68449 ),
 ( #99377, #29956 ),
 ( #30950, #91792 ),
 ( #53254, #61344 ),
 ( #92303, #93286 ),
 ( #22852, #84695 ),
 ( #7653, #92786 ) ),
 .UNSPECIFIED., .F., .F., .F.,
 ( 4, 3, 3, 3, 3, 3, 3, 3, 3, 3, 4 ),
 ( 2, 2 ),
 ( 0.000000000000000000, 0.1122669598086816489, 0.2243161639709700117, 0.3396355846219164532, 0.4553962076585098551, 0.5677860799922355151, 0.6749047109689640944, 0.7773884377078206231, 0.8775581155834345504, 0.9782364162378064387, 1.000000000000000000 ),
 ( 0.000000000000000000, 1.000000000000000000 ),
 .UNSPECIFIED. ) ;
#85816 = CARTESIAN_POINT ( 'NONE',  ( 194.4565572889705152, 292.7111445759336448, -15.25152910787323357 ) ) ;
#85817 = ORIENTED_EDGE ( 'NONE', *, *, #93715, .F. ) ;
#85818 = CARTESIAN_POINT ( 'NONE',  ( 202.9216520459657147, 279.1763840310111391, 15.75371595331685803 ) ) ;
#85819 = CARTESIAN_POINT ( 'NONE',  ( 88.04376564059177213, 44.77267915597603576, 4.588252583283844999 ) ) ;
#85820 = CARTESIAN_POINT ( 'NONE',  ( 27.50958393249801404, 180.5643266524160424, 9.188101187500095079 ) ) ;
#85821 = CARTESIAN_POINT ( 'NONE',  ( 11.19180257851625448, 22.16454794089040092, -10.00000000000000355 ) ) ;
#85822 = DIRECTION ( 'NONE',  ( -0.4270171210482543445, 0.9042435392811277728, 0.000000000000000000 ) ) ;
#85823 = CARTESIAN_POINT ( 'NONE',  ( 19.31801425620939483, 115.5650415295850451, -20.00000000000000355 ) ) ;
#85824 = CARTESIAN_POINT ( 'NONE',  ( 73.97544314932677878, 54.88016228234857152, -16.13337635542186277 ) ) ;
#85826 = CARTESIAN_POINT ( 'NONE',  ( 68.02342162723002161, 200.8923013555409796, 4.594050593750050204 ) ) ;
#85825 = CARTESIAN_POINT ( 'NONE',  ( 198.0795109501767115, 277.7783264603462499, -16.13655660432609906 ) ) ;
#85827 = CARTESIAN_POINT ( 'NONE',  ( 164.4963285489318991, 245.7309966251440301, -6.672251175510283794 ) ) ;
#85828 = CARTESIAN_POINT ( 'NONE',  ( 119.4694200880668831, 251.3297689869269504, -2.679491924311252493 ) ) ;
#85829 = CARTESIAN_POINT ( 'NONE',  ( 180.8078237589699029, 256.2600327853984936, 1.558727462200503400 ) ) ;
#85830 = CARTESIAN_POINT ( 'NONE',  ( 71.12491932460929434, 69.18585904456776348, 8.936385494539548446 ) ) ;
#85831 = CARTESIAN_POINT ( 'NONE',  ( 8.916318567990060728, 28.08080186712591342, -3.090169943749475845 ) ) ;
#85832 = ORIENTED_EDGE ( 'NONE', *, *, #89920, .F. ) ;
#85833 = EDGE_CURVE ( 'NONE', #61735, #47657, #10601, .T. ) ;
#85834 = CARTESIAN_POINT ( 'NONE',  ( 37.40555484421791022, 185.7365022471902023, 10.00000000000009592 ) ) ;
#85835 = DIRECTION ( 'NONE',  ( 0.000000000000000000, 0.000000000000000000, 1.000000000000000000 ) ) ;
#85836 = DIRECTION ( 'NONE',  ( -0.4999999999999987788, 0.8660254037844392627, 0.000000000000000000 ) ) ;
#85837 = CARTESIAN_POINT ( 'NONE',  ( -16.46870247313679059, 170.4869531367911293, 4.594050593750046652 ) ) ;
#85838 = CARTESIAN_POINT ( 'NONE',  ( 35.02453322635827959, 23.14754757982091959, -5.678558825948276656 ) ) ;
#85840 = CARTESIAN_POINT ( 'NONE',  ( 199.9809106644752035, 283.6121499399518484, 16.99530978087883071 ) ) ;
#85839 = CARTESIAN_POINT ( 'NONE',  ( 167.7942285755875957, 262.4949493498345987, -16.83134817174553532 ) ) ;
#85841 = CARTESIAN_POINT ( 'NONE',  ( 189.2732718030835599, 261.7774826209242178, 6.629783814786226692 ) ) ;
#85842 = EDGE_CURVE ( 'NONE', #5449, #38097, #78725, .T. ) ;
#85843 = CARTESIAN_POINT ( 'NONE',  ( 206.2456893945931142, 273.4189824569319285, 10.13882547285618152 ) ) ;
#85844 = CARTESIAN_POINT ( 'NONE',  ( 87.98804127167099409, 43.77408088403166175, 2.388364124389108945 ) ) ;
#85845 = EDGE_CURVE ( 'NONE', #85624, #4581, #55236, .T. ) ;
#85846 = CARTESIAN_POINT ( 'NONE',  ( 65.86157430945659996, 69.00948543913943922, 2.025254867008428050 ) ) ;
#85847 = ORIENTED_EDGE ( 'NONE', *, *, #85046, .T. ) ;
#85848 = CARTESIAN_POINT ( 'NONE',  ( 150.4638999619119204, 271.8026217546109251, -12.79869408032183742 ) ) ;
#85849 = CARTESIAN_POINT ( 'NONE',  ( 181.0855840883816938, 287.1795278100775590, 13.27675118985169433 ) ) ;
#85850 = FACE_OUTER_BOUND ( 'NONE', #18513, .T. ) ;
#85851 = CARTESIAN_POINT ( 'NONE',  ( 6.742211794378569323, 25.93396525600388003, 2.839279412974139660 ) ) ;
#85852 = CARTESIAN_POINT ( 'NONE',  ( 160.4207999851416560, 252.7900191653268394, 16.17069880550225847 ) ) ;
#85853 = EDGE_CURVE ( 'NONE', #12944, #38056, #95960, .T. ) ;
#85854 = CARTESIAN_POINT ( 'NONE',  ( 204.8878784573704195, 275.7707799872745795, -14.13380496213581594 ) ) ;
#85855 = ADVANCED_FACE ( 'NONE', ( #25000 ), #17926, .T. ) ;
#85856 = CARTESIAN_POINT ( 'NONE',  ( 115.2960263294082068, 225.8262482093458061, 3.021315404115420679E-15 ) ) ;
#85857 = LINE ( 'NONE', #61961, #70872 ) ;
#85858 = CARTESIAN_POINT ( 'NONE',  ( 191.3441257904396764, 298.1785231045369642, 9.312382026386032408 ) ) ;
#85859 = CARTESIAN_POINT ( 'NONE',  ( 163.2000388741132895, 247.9762362032568035, -11.19676374274550312 ) ) ;
#85860 = CARTESIAN_POINT ( 'NONE',  ( 152.9273493951901628, 265.7690563111299298, -17.70273273795505631 ) ) ;
#85861 = ORIENTED_EDGE ( 'NONE', *, *, #77637, .F. ) ;
#85862 = ORIENTED_EDGE ( 'NONE', *, *, #9625, .F. ) ;
#85863 = CARTESIAN_POINT ( 'NONE',  ( 155.8157825667570080, 277.1861924174589262, -10.41322603298928051 ) ) ;
#85864 = CARTESIAN_POINT ( 'NONE',  ( 188.7930588916510999, 290.9633865388665299, 14.97457979531618832 ) ) ;
#85865 = ORIENTED_EDGE ( 'NONE', *, *, #12703, .T. ) ;
#85866 = CARTESIAN_POINT ( 'NONE',  ( 68.45344762042827824, 64.57392882346940155, 12.12708197196866600 ) ) ;
#85867 = CARTESIAN_POINT ( 'NONE',  ( 155.5207183646172950, 261.6826666266933898, -16.99780945766855922 ) ) ;
#85868 = ORIENTED_EDGE ( 'NONE', *, *, #23855, .T. ) ;
#85869 = AXIS2_PLACEMENT_3D ( 'NONE', #94065, #77330, #100148 ) ;
#85870 = CARTESIAN_POINT ( 'NONE',  ( 68.69482932751195392, 64.02698956824444565, -12.02621948774222993 ) ) ;
#85871 = PLANE ( 'NONE',  #94507 ) ;
#85872 = CARTESIAN_POINT ( 'NONE',  ( 164.3330377059402849, 246.0138246616164110, 7.208046019122525294 ) ) ;
#85873 = CARTESIAN_POINT ( 'NONE',  ( 69.96429914230955660, 62.67588759707778934, 13.42142011397352874 ) ) ;
#85874 = VERTEX_POINT ( 'NONE', #92577 ) ;
#85875 = CARTESIAN_POINT ( 'NONE',  ( 161.2799361541916028, 251.3019516699124836, 14.40628917569557110 ) ) ;
#85876 = CARTESIAN_POINT ( 'NONE',  ( 166.1070111784138703, 253.4115428555481344, -13.60050710122670559 ) ) ;
#85877 = CARTESIAN_POINT ( 'NONE',  ( 66.34774863042578374, 68.89465645501611846, 3.924861168553110513 ) ) ;
#85878 = CARTESIAN_POINT ( 'NONE',  ( 29.54281338067077911, 40.55466486950702176, -1.111400068045478839E-16 ) ) ;
#85879 = VERTEX_POINT ( 'NONE', #86370 ) ;
#85880 = ORIENTED_EDGE ( 'NONE', *, *, #93770, .T. ) ;
#85881 = ORIENTED_EDGE ( 'NONE', *, *, #33054, .F. ) ;
#85882 = CARTESIAN_POINT ( 'NONE',  ( 80.25311165466112584, 46.21449285432851184, 12.30778873727355638 ) ) ;
#85883 = ORIENTED_EDGE ( 'NONE', *, *, #49379, .T. ) ;
#85884 = FACE_OUTER_BOUND ( 'NONE', #30725, .T. ) ;
#85885 = AXIS2_PLACEMENT_3D ( 'NONE', #38984, #9102, #94237 ) ;
#85886 = ORIENTED_EDGE ( 'NONE', *, *, #40551, .T. ) ;
#85887 = CARTESIAN_POINT ( 'NONE',  ( 164.4698008747318738, 245.7769439046653019, -6.272955660526681854 ) ) ;
#85888 = DIRECTION ( 'NONE',  ( 0.5000000000000014433, -0.8660254037844378194, 0.000000000000000000 ) ) ;
#85889 = CARTESIAN_POINT ( 'NONE',  ( 165.1033008171500001, 270.9562025061328541, 16.67780619943411580 ) ) ;
#85891 = EDGE_CURVE ( 'NONE', #91334, #94724, #33563, .T. ) ;
#85890 = CARTESIAN_POINT ( 'NONE',  ( 167.6723227085472558, 281.1242618559421089, 11.55074042278067559 ) ) ;
#85892 = CARTESIAN_POINT ( 'NONE',  ( 194.9385458806846430, 293.0035295114944347, -15.70518692812489192 ) ) ;
#85893 = CARTESIAN_POINT ( 'NONE',  ( 82.61614429202859355, 53.50419195261176242, -15.73127852458025622 ) ) ;
#85894 = CARTESIAN_POINT ( 'NONE',  ( 159.0424690102808256, 255.1773584434317570, -17.34001589335112925 ) ) ;
#85895 = CARTESIAN_POINT ( 'NONE',  ( 200.8532844524641803, 271.0267732368380962, -11.47671578755057986 ) ) ;
#85896 = CARTESIAN_POINT ( 'NONE',  ( 26.78885238572174998, 16.26216523072495690, -2.296566073217252530E-15 ) ) ;
#85897 = DIRECTION ( 'NONE',  ( -0.3374500364938435304, -0.9413434404457831084, 0.000000000000000000 ) ) ;
#85898 = CARTESIAN_POINT ( 'NONE',  ( 191.6400076255916076, 298.3370758160374976, -8.690192626989791336 ) ) ;
#85900 = ORIENTED_EDGE ( 'NONE', *, *, #18526, .F. ) ;
#85899 = CARTESIAN_POINT ( 'NONE',  ( 206.7921793621094650, 271.5292813338429596, 6.134403222006724832 ) ) ;
#85901 = CARTESIAN_POINT ( 'NONE',  ( 190.8738732131464246, 300.0437490878071003, 5.255515203389859558 ) ) ;
#85902 = LINE ( 'NONE', #39205, #18902 ) ;
#85903 = CARTESIAN_POINT ( 'NONE',  ( 159.3451320108506764, 254.6531307488737355, -16.72997986213134425 ) ) ;
#85904 = LINE ( 'NONE', #24529, #21440 ) ;
#85905 = CARTESIAN_POINT ( 'NONE',  ( 83.71006973597178558, 45.75904905664672384, -10.17439447765971039 ) ) ;
#85906 = CARTESIAN_POINT ( 'NONE',  ( 200.3765029811139584, 283.5847115241710981, 16.85207472104531590 ) ) ;
#85907 = CARTESIAN_POINT ( 'NONE',  ( 191.1252388389400778, 261.3801678008247791, -0.002822319849339915022 ) ) ;
#85908 = ORIENTED_EDGE ( 'NONE', *, *, #41095, .F. ) ;
#85909 = CARTESIAN_POINT ( 'NONE',  ( 194.3387753395540472, 294.0423625616157892, -15.64827765940100868 ) ) ;
#85910 = PLANE ( 'NONE',  #51164 ) ;
#85911 = DIRECTION ( 'NONE',  ( -0.7957378174433814566, 0.6056412518070772855, 0.000000000000000000 ) ) ;
#85912 = CARTESIAN_POINT ( 'NONE',  ( 18.62362889609489969, 194.8927522451419634, 2.944929066748280225E-16 ) ) ;
#85913 = CARTESIAN_POINT ( 'NONE',  ( 85.37073267496330686, 220.0958772461660544, -9.188101187500095079 ) ) ;
#85914 = EDGE_CURVE ( 'NONE', #84849, #28495, #56896, .T. ) ;
#85915 = CARTESIAN_POINT ( 'NONE',  ( 196.3918367485927376, 269.1678964851112141, -12.08347791044659303 ) ) ;
#85916 = CARTESIAN_POINT ( 'NONE',  ( -4.653128914090325807, 78.77562236714182120, 52.49999999999999289 ) ) ;
#85917 = CARTESIAN_POINT ( 'NONE',  ( 169.0459840413011534, 279.5632588650593107, -13.46217358039099921 ) ) ;
#85919 = CARTESIAN_POINT ( 'NONE',  ( 75.64192366613818308, 65.38353595949358521, 14.29496885373930581 ) ) ;
#85918 = CARTESIAN_POINT ( 'NONE',  ( 3.260525530768699998, 178.8149278399161233, 9.188101187500093303 ) ) ;
#85920 = CARTESIAN_POINT ( 'NONE',  ( 161.4844649541891499, 250.9476973967054789, 12.93553496455142415 ) ) ;
#85921 = ORIENTED_EDGE ( 'NONE', *, *, #14221, .T. ) ;
#85923 = VERTEX_POINT ( 'NONE', #63507 ) ;
#85922 = UNCERTAINTY_MEASURE_WITH_UNIT (LENGTH_MEASURE( 1.000000000000000082E-05 ), #100216, 'distance_accuracy_value', 'NONE');
#85924 = LINE ( 'NONE', #70649, #59760 ) ;
#85925 = CARTESIAN_POINT ( 'NONE',  ( 201.2505344690289064, 267.2087450970302029, -3.778420330458906573 ) ) ;
#85926 = EDGE_CURVE ( 'NONE', #67254, #47702, #98921, .T. ) ;
#85927 = FACE_OUTER_BOUND ( 'NONE', #44749, .T. ) ;
#85928 = EDGE_CURVE ( 'NONE', #71782, #69624, #73404, .T. ) ;
#85929 = CARTESIAN_POINT ( 'NONE',  ( 84.92266591929319475, 45.12665518879106941, 8.618535221689526793 ) ) ;
#85930 = CARTESIAN_POINT ( 'NONE',  ( 161.8926315922002743, 250.2407320417157166, -13.77020595223768495 ) ) ;
#85931 = CARTESIAN_POINT ( 'NONE',  ( 105.1336465626505969, 243.0530062829863027, -4.648177544792955347E-16 ) ) ;
#85932 = CARTESIAN_POINT ( 'NONE',  ( 74.34814666111280701, 67.93757562633051350, -11.69177540040551655 ) ) ;
#85933 = CARTESIAN_POINT ( 'NONE',  ( 37.27951979288245354, 183.1423013555409796, -4.594050593750043987 ) ) ;
#85934 = CARTESIAN_POINT ( 'NONE',  ( 199.5106878072222685, 277.4853542194088618, 15.16379332014005321 ) ) ;
#85935 = ORIENTED_EDGE ( 'NONE', *, *, #76851, .T. ) ;
#85936 = CARTESIAN_POINT ( 'NONE',  ( 153.4303388563101862, 273.9525667856884183, -11.93370399901073853 ) ) ;
#85937 = CARTESIAN_POINT ( 'NONE',  ( 182.3263212693539685, 260.8467281569974716, -10.61505835826066502 ) ) ;
#85938 = CARTESIAN_POINT ( 'NONE',  ( -4.215479392844351914, 156.8262482093458061, -4.415768667553308270E-15 ) ) ;
#85939 = DIRECTION ( 'NONE',  ( 0.4999999999999992784, -0.8660254037844390407, 0.000000000000000000 ) ) ;
#85940 = CARTESIAN_POINT ( 'NONE',  ( 155.1376601545389917, 261.9406857754215707, 18.55063430030667959 ) ) ;
#85941 = CARTESIAN_POINT ( 'NONE',  ( 62.88113547221012567, 207.1115022471902307, 10.00000000000009592 ) ) ;
#85942 = CARTESIAN_POINT ( 'NONE',  ( 77.22649460905378760, 63.31555197798695644, 15.15381191669832184 ) ) ;
#85943 = CARTESIAN_POINT ( 'NONE',  ( 147.8819534105757043, 274.5079385007862811, -9.338341377131436971 ) ) ;
#85944 = CARTESIAN_POINT ( 'NONE',  ( 189.8033664021961613, 262.5080370049500971, 8.283948267418471900 ) ) ;
#85945 = CARTESIAN_POINT ( 'NONE',  ( 168.1784323372465906, 278.2753528722733449, 14.27304841468856722 ) ) ;
#85946 = CARTESIAN_POINT ( 'NONE',  ( 22.61095419623372038, 183.8615022471902591, -10.00000000000009592 ) ) ;
#85947 = CARTESIAN_POINT ( 'NONE',  ( 71.43092631454221930, 71.71198063924084920, 2.470412517165702759 ) ) ;
#85948 = CARTESIAN_POINT ( 'NONE',  ( 147.8503508990560533, 274.5626756563852950, 7.845851077393495743 ) ) ;
#85949 = CARTESIAN_POINT ( 'NONE',  ( 181.2456060316003743, 265.9490061796501550, -15.17417357770760944 ) ) ;
#85950 = ORIENTED_EDGE ( 'NONE', *, *, #13247, .F. ) ;
#85951 = CARTESIAN_POINT ( 'NONE',  ( 74.93919869194499483, 61.43846615714554815, 15.72264986953730492 ) ) ;
#85952 = AXIS2_PLACEMENT_3D ( 'NONE', #31625, #62524, #20022 ) ;
#85953 = ADVANCED_FACE ( 'NONE', ( #65502 ), #58074, .F. ) ;
#85954 = CARTESIAN_POINT ( 'NONE',  ( 161.5753992217405823, 251.8338521006345161, -13.71391156857418281 ) ) ;
#85955 = CARTESIAN_POINT ( 'NONE',  ( 104.0442318961827652, 237.0024278399160949, -9.188101187500093303 ) ) ;
#85956 = CARTESIAN_POINT ( 'NONE',  ( 13.18987451683679524, 19.56628583063839244, 9.188101187500006262 ) ) ;
#85957 = B_SPLINE_CURVE_WITH_KNOTS ( 'NONE', 3,
 ( #38226, #7858, #38737, #8354 ),
 .UNSPECIFIED., .F., .F.,
 ( 4, 4 ),
 ( 0.01442566870911189854, 0.02312499380068684662 ),
 .UNSPECIFIED. ) ;
#85958 = CARTESIAN_POINT ( 'NONE',  ( 150.7226148805041817, 269.5877685077668957, 15.52819754351937576 ) ) ;
#85959 = CARTESIAN_POINT ( 'NONE',  ( -22.42236680055709641, 157.8615022471902591, 0.000000000000000000 ) ) ;
#85961 = CARTESIAN_POINT ( 'NONE',  ( 191.6210545128721776, 276.9003016344976800, 17.04950522666647217 ) ) ;
#85960 = CARTESIAN_POINT ( 'NONE',  ( 205.4925884257800988, 274.0740247280971857, 10.80283695292349222 ) ) ;
#85962 = CARTESIAN_POINT ( 'NONE',  ( 48.98007068238332096, 88.97864505566217019, -10.00000000000000000 ) ) ;
#85963 = CARTESIAN_POINT ( 'NONE',  ( 192.8725807964287924, 263.8132596570546298, -4.373067053639174695 ) ) ;
#85964 = CARTESIAN_POINT ( 'NONE',  ( 149.9052967174216917, 271.6272115183317624, -11.69003756284735829 ) ) ;
#85965 = CARTESIAN_POINT ( 'NONE',  ( 74.83655476910676896, 53.51806293180212037, 16.54630480343736920 ) ) ;
#85966 = CARTESIAN_POINT ( 'NONE',  ( 189.9879251633717558, 299.5782561228834879, -6.671532329245590809 ) ) ;
#85967 = DIRECTION ( 'NONE',  ( 0.000000000000000000, 1.000000000000000000, 0.000000000000000000 ) ) ;
#85968 = ORIENTED_EDGE ( 'NONE', *, *, #48834, .T. ) ;
#85969 = CARTESIAN_POINT ( 'NONE',  ( 192.7355331156994964, 267.2041169143933530, 11.12292375133700517 ) ) ;
#85970 = DIRECTION ( 'NONE',  ( -1.000000000000000000, -1.387778780781445478E-15, -0.000000000000000000 ) ) ;
#85971 = CARTESIAN_POINT ( 'NONE',  ( 81.67261577379798609, 49.77584566285921852, 14.52435489019822690 ) ) ;
#85972 = EDGE_CURVE ( 'NONE', #75236, #37985, #38064, .T. ) ;
#85973 = ORIENTED_EDGE ( 'NONE', *, *, #74099, .T. ) ;
#85974 = FACE_OUTER_BOUND ( 'NONE', #83847, .T. ) ;
#85975 = CARTESIAN_POINT ( 'NONE',  ( 196.1749740761792111, 288.8619730569873809, -17.33086882175758703 ) ) ;
#85976 = CARTESIAN_POINT ( 'NONE',  ( 81.37674444193763179, 55.19836804271280783, -15.94010240901345199 ) ) ;
#85977 = CARTESIAN_POINT ( 'NONE',  ( 142.9163165386219703, 259.9865022471903444, 10.00000000000009237 ) ) ;
#85978 = VERTEX_POINT ( 'NONE', #61377 ) ;
#85979 = CARTESIAN_POINT ( 'NONE',  ( 73.62250635243425734, 69.55784274833358438, 10.23584637956793308 ) ) ;
#85980 = CARTESIAN_POINT ( 'NONE',  ( 39.54951596113196644, 25.76004757982093096, 5.678558825948272215 ) ) ;
#85981 = EDGE_LOOP ( 'NONE', ( #81913, #95079, #56448, #56791, #46413, #94490, #62005, #78245, #81235, #79965, #73734, #81866, #51854, #44957, #56300, #72378, #62422, #30585, #39048, #87630 ) ) ;
#85982 = CARTESIAN_POINT ( 'NONE',  ( 78.44203751522358914, 61.21016990572090322, 16.24725970467587643 ) ) ;
#85983 = LINE ( 'NONE', #8417, #71003 ) ;
#85984 = CARTESIAN_POINT ( 'NONE',  ( 49.07419501245632887, 91.40403951869188859, -10.00000000000000000 ) ) ;
#85985 = EDGE_LOOP ( 'NONE', ( #64115, #40962, #77481, #23220 ) ) ;
#85986 = CARTESIAN_POINT ( 'NONE',  ( 86.40472769894839189, 47.00022269315729773, -10.52150423465797502 ) ) ;
#85987 = DIRECTION ( 'NONE',  ( -0.2805612043866616001, -0.9598361373656993933, 0.000000000000000000 ) ) ;
#85988 = CARTESIAN_POINT ( 'NONE',  ( 163.9704062730716032, 246.6419207277664327, 7.317582738093436845 ) ) ;
#85989 = DIRECTION ( 'NONE',  ( 0.000000000000000000, 0.000000000000000000, -1.000000000000000000 ) ) ;
#85990 = ADVANCED_FACE ( 'NONE', ( #92332 ), #84726, .T. ) ;
#85991 = CARTESIAN_POINT ( 'NONE',  ( 170.5924673348125964, 258.8840003614211582, 15.37362746749550624 ) ) ;
#85992 = CARTESIAN_POINT ( 'NONE',  ( 80.90512323705502240, 45.42831638329423072, -12.03671141704919556 ) ) ;
#85993 = CARTESIAN_POINT ( 'NONE',  ( 33.34606076043043998, 183.3927522451418497, 10.00000000000009948 ) ) ;
#85994 = ORIENTED_EDGE ( 'NONE', *, *, #31863, .T. ) ;
#85995 = ORIENTED_EDGE ( 'NONE', *, *, #17553, .F. ) ;
#85996 = CARTESIAN_POINT ( 'NONE',  ( 162.8386403195304410, 249.0994062285972461, 10.29435687412694911 ) ) ;
#85997 = VERTEX_POINT ( 'NONE', #92818 ) ;
#85998 = CARTESIAN_POINT ( 'NONE',  ( 77.20442761108157015, 49.22956228998022965, -15.35833876822225186 ) ) ;
#86000 = VERTEX_POINT ( 'NONE', #40569 ) ;
#85999 = EDGE_CURVE ( 'NONE', #86029, #79763, #15411, .T. ) ;
#86001 = CARTESIAN_POINT ( 'NONE',  ( 87.02439212704567240, 45.81336919377327632, -8.633490303204487404 ) ) ;
#86002 = CARTESIAN_POINT ( 'NONE',  ( 79.30460723929135725, 53.73768979410964164, 15.82503211290379674 ) ) ;
#86003 = VERTEX_POINT ( 'NONE', #87270 ) ;
#86004 = CARTESIAN_POINT ( 'NONE',  ( 190.4750788177879883, 300.1286839245400415, -3.520404030213226676 ) ) ;
#86005 = CARTESIAN_POINT ( 'NONE',  ( 164.4306612431381325, 245.8447357351751066, -2.314684942147286595 ) ) ;
#86006 = CARTESIAN_POINT ( 'NONE',  ( 147.4018083154577994, 275.3395742005352531, -7.372329269489205750 ) ) ;
#86007 = CARTESIAN_POINT ( 'NONE',  ( 196.1019265324206629, 284.4571118909283314, -17.79305111687722274 ) ) ;
#86008 = CARTESIAN_POINT ( 'NONE',  ( 82.67120877686448921, 40.53284241866003867, 0.8934199165528524667 ) ) ;
#86010 = EDGE_CURVE ( 'NONE', #54888, #95476, #17801, .T. ) ;
#86009 = CARTESIAN_POINT ( 'NONE',  ( 171.5849702451724852, 250.5752846868085726, -5.747692145100161021 ) ) ;
#86011 = DIRECTION ( 'NONE',  ( 0.6116140086401538056, -0.7911563084720502070, 0.000000000000000000 ) ) ;
#86012 = CARTESIAN_POINT ( 'NONE',  ( 157.6776325807875878, 281.5257696872717474, 2.944928808717816704 ) ) ;
#86013 = CARTESIAN_POINT ( 'NONE',  ( 129.3758220526426044, 239.3768266524160140, -9.188101187500091527 ) ) ;
#86014 = CARTESIAN_POINT ( 'NONE',  ( 183.6008598791219129, 260.5699149889866248, -9.267803207057191628 ) ) ;
#86015 = CARTESIAN_POINT ( 'NONE',  ( 34.13026518906141860, 41.74646525600392977, 2.839279412974139660 ) ) ;
#86016 = VERTEX_POINT ( 'NONE', #64389 ) ;
#86018 = ORIENTED_EDGE ( 'NONE', *, *, #46900, .T. ) ;
#86017 = CARTESIAN_POINT ( 'NONE',  ( 85.57852021786813168, 48.96074862228688573, -12.66870494374460066 ) ) ;
#86019 = CARTESIAN_POINT ( 'NONE',  ( 200.1188775601148109, 273.7126575094745817, 13.85740573495379557 ) ) ;
#86020 = CARTESIAN_POINT ( 'NONE',  ( 178.2114048607894858, 253.3878526894902166, 1.409026425838265872 ) ) ;
#86021 = DIRECTION ( 'NONE',  ( 0.000000000000000000, 1.000000000000000000, 0.000000000000000000 ) ) ;
#86022 = CARTESIAN_POINT ( 'NONE',  ( 147.1444677838046573, 275.7853010762056556, 2.585175795350988626 ) ) ;
#86023 = CARTESIAN_POINT ( 'NONE',  ( 73.29586284545086983, 66.59957193289693578, 12.21858630789641076 ) ) ;
#86024 = CARTESIAN_POINT ( 'NONE',  ( 201.1060504099706350, 282.3210983108598384, -18.18000168485860257 ) ) ;
#86025 = CARTESIAN_POINT ( 'NONE',  ( 79.26867134682716198, 56.64247672455211102, 16.58182463307725385 ) ) ;
#86026 = CARTESIAN_POINT ( 'NONE',  ( 174.8987400875574281, 282.4155400008056631, 14.62834699329571286 ) ) ;
#86027 = AXIS2_PLACEMENT_3D ( 'NONE', #88376, #54012, #18931 ) ;
#86028 = LINE ( 'NONE', #32255, #33549 ) ;
#86029 = VERTEX_POINT ( 'NONE', #23874 ) ;
#86030 = CARTESIAN_POINT ( 'NONE',  ( 194.3708539535661259, 293.9868007723104029, -16.01585187499628304 ) ) ;
#86031 = DIRECTION ( 'NONE',  ( -0.1654779384134575371, 0.9862134920484671996, 0.000000000000000000 ) ) ;
#86032 = ORIENTED_EDGE ( 'NONE', *, *, #20114, .F. ) ;
#86034 = CARTESIAN_POINT ( 'NONE',  ( 191.3399829603070827, 267.7330644374129065, -12.16091939637846231 ) ) ;
#86033 = B_SPLINE_CURVE_WITH_KNOTS ( 'NONE', 3,
 ( #51742, #70416, #63817, #33421, #16219, #16716, #24811, #23809, #71435, #86676, #85162, #15706, #31410, #2025, #25314, #32910, #62297, #54698, #23306, #55688, #94257, #8129, #47610, #69908, #92752, #46606, #87197, #56201, #1025, #94752, #17730, #10125, #93254, #85682, #70933, #9644, #86182, #77538, #93765, #31904, #63316, #523, #39003, #48633, #47111, #79566, #40991, #71934, #78031, #8623, #1539, #40503 ),
 .UNSPECIFIED., .F., .F.,
 ( 4, 2, 2, 2, 2, 2, 2, 2, 2, 2, 2, 2, 2, 2, 2, 2, 2, 2, 2, 2, 2, 2, 2, 2, 2, 4 ),
 ( 0.0001164149332258714178, 0.0006113509262942967790, 0.001106286919362722181, 0.001353754915896962637, 0.001601222912431203094, 0.001724956910698308794, 0.001848690908965414711, 0.001972424907232520411, 0.002096158905499626111, 0.002343626902033844016, 0.002591094898568061054, 0.003086030891636534160, 0.004075902877773479940, 0.005065774863910425287, 0.005560710856978898393, 0.005808178853513132345, 0.005931912851780252356, 0.006055646850047372368, 0.006117513849180932807, 0.006179380848314493246, 0.006303114846581607186, 0.006550582843115837668, 0.007045518836184282152, 0.007292986832718569012, 0.007540454829252855005, 0.008035390822321386226 ),
 .UNSPECIFIED. ) ;
#86035 = CARTESIAN_POINT ( 'NONE',  ( 190.2972692340288177, 282.9090305667509142, -16.56549508821761663 ) ) ;
#86036 = CARTESIAN_POINT ( 'NONE',  ( 151.7124930133047371, 267.8732492884548719, -16.17794402247774244 ) ) ;
#86037 = CARTESIAN_POINT ( 'NONE',  ( 190.0259678364800493, 301.5123642802043946, 4.004183174499006626 ) ) ;
#86038 = CARTESIAN_POINT ( 'NONE',  ( 71.64316818921395225, 72.05741665177615118, -3.509880912999884917 ) ) ;
#86040 = CARTESIAN_POINT ( 'NONE',  ( 160.4448519566613243, 282.3920345168493782, 6.649608260177227059 ) ) ;
#86039 = CARTESIAN_POINT ( 'NONE',  ( 161.9065591971467768, 281.7447826133235367, -6.599482603196943131 ) ) ;
#86041 = DIRECTION ( 'NONE',  ( -0.2270762630343691746, 0.9738769792773346312, 0.000000000000000000 ) ) ;
#86042 = ORIENTED_EDGE ( 'NONE', *, *, #49194, .F. ) ;
#86043 = CARTESIAN_POINT ( 'NONE',  ( 146.8000281410530192, 276.3818880375922049, 4.652863924796177386 ) ) ;
#86044 = CARTESIAN_POINT ( 'NONE',  ( 73.10296688250903685, 63.30412816941502285, 14.61027101223241864 ) ) ;
#86045 = CARTESIAN_POINT ( 'NONE',  ( 20.94669640352213236, 37.57748520232516398, 10.00000000000000000 ) ) ;
#86046 = DIRECTION ( 'NONE',  ( -1.000000000000000000, 0.000000000000000000, 5.984665299743594308E-16 ) ) ;
#86047 = ADVANCED_FACE ( 'NONE', ( #31972 ), #62877, .T. ) ;
#86048 = CARTESIAN_POINT ( 'NONE',  ( -20.95882727533908252, 95.12657743062730731, 45.19937630303415688 ) ) ;
#86049 = CARTESIAN_POINT ( 'NONE',  ( 185.5568049818104726, 266.1438378612298834, 14.60334785453874140 ) ) ;
#86050 = EDGE_CURVE ( 'NONE', #23431, #72257, #71509, .T. ) ;
#86051 = CARTESIAN_POINT ( 'NONE',  ( 74.28707621773548908, 68.55768173149772338, 11.60544092197707755 ) ) ;
#86052 =( BOUNDED_CURVE ( )  B_SPLINE_CURVE ( 2, ( #83324, #75701, #4812, #35694, #30081, #51897, #45276, #6288, #37181, #68081, #14392, #43777, #99003, #60968, #74722, #66594, #84327, #16874, #76685, #54351, #55847, #45762, #70063, #84819, #39150, #32583, #38155, #63480, #40160, #78698, #8780, #9285, #681, #15357, #32065, #31562, #47270, #100000, #62453, #7782, #16379, #54870, #46253, #69073, #30583, #23461, #85851, #61471, #71101, #85324, #1700, #77177, #93420, #94417, #22969, #47759, #24970, #23971, #92419, #78192, #86842, #39650, #70571, #1189, #7273, #38672, #62976, #53856, #69575, #93924, #24478, #55359, #183, #31066, #61957, #92909, #86337, #15869, #46778, #77701, #8284, #88846, #50268, #49286, #40664, #95930, #17377, #73102, #3694, #95444, #48795, #72609, #87851, #57367, #72097, #34573, #88341, #49777, #25996, #87368, #18391, #18898, #80222, #17898, #80734, #73586, #56867, #25479, #10790, #81221, #4166, #79726, #34096, #96922, #3211, #56371, #11308, #79231, #41664, #64986, #9804, #26490, #10288, #65474, #42166, #96416, #71601, #26983, #41160, #57867, #19409, #11797, #27490, #42652, #2697, #35063, #2197, #65970, #58359, #48286, #33080, #63973, #94916, #64484, #33588, #13628, #76904, #38399, #30316, #85047, #60689, #14621, #68802, #15096, #36909, #99729, #92650, #75431, #61203, #92170, #45500, #90673, #44502, #43996, #45002, #6015, #36406, #91151, #21229, #45987, #7501, #69312, #75948, #67310, #22214, #74938, #22720, #53599, #21716, #67822, #99229, #91647, #29815, #52600, #61698, #83557, #53111, #84068, #76433, #7008, #37893, #6524, #98744, #84557, #100234, #14121, #52108, #37400, #30818, #23200, #29324, #68306, #54091, #83055, #98238, #5522, #28824, #60190, #59707, #38901, #56610, #55589, #69805, #39885, #9013, #17105, #15594, #77430, #71836, #77928, #87084, #17620, #25207, #94153, #70820, #24218, #95162, #86085, #86572, #39388, #415, #23693, #1429, #31304, #33312, #46494, #32310, #54589, #63211, #2434, #8029, #62192, #93143, #16609, #85571, #16115, #93653, #47013, #48000, #8519, #55098, #62696, #71331, #70305, #918, #31794, #47505, #78432, #24706, #78945, #9533, #40394, #1923, #32809, #63714, #94652, #56090, #48524, #79461, #10025, #40887, #64211, #25730, #34797, #73327, #34313, #4927, #65211, #65699, #96653, #27223, #80461, #89088, #57598, #88578, #49022, #58106, #41909, #66215, #58588, #42879, #96153, #66700, #19140, #20123, #64724, #10523, #73815, #26716, #11032, #72844, #50014, #3436, #80968, #28200, #50995, #26220, #18629, #49507, #11533, #74338, #42393, #35303, #81946, #97154, #19637, #50497, #81451, #97635, #12023, #4407, #43395, #12524, #18120, #27720, #87594, #35806, #79955, #41398, #2947, #72341, #33836, #95673, #20619, #98633, #91045, #51503, #29215, #6412, #83440, #82470, #60578, #13032, #14007, #21129, #29701, #99119, #99618, #69189, #53487, #13522, #30196, #43894, #44885, #60082, #75826, #21612, #61082, #7388, #76795, #5904, #84439, #68190, #74834, #91534, #38278, #5414, #22098, #92053, #83945, #36297, #52492, #14507, #67200, #45390, #76320, #6895, #98122, #82949, #28706, #59076, #52006, #37784, #68686, #22599, #100118, #14984, #44390, #45871, #59584, #90047, #90560, #75325, #36794, #67706, #79347, #48400, #77817, #47387, #294, #63591 ),
 .UNSPECIFIED., .F., .T. ) 
 B_SPLINE_CURVE_WITH_KNOTS ( ( 3, 2, 2, 2, 2, 2, 2, 2, 2, 2, 2, 2, 2, 2, 2, 2, 2, 2, 2, 2, 2, 2, 2, 2, 2, 2, 2, 2, 2, 2, 2, 2, 2, 2, 2, 2, 2, 2, 2, 2, 2, 2, 2, 2, 2, 2, 2, 2, 2, 2, 2, 2, 2, 2, 2, 2, 2, 2, 2, 2, 2, 2, 2, 2, 2, 2, 2, 2, 2, 2, 2, 2, 2, 2, 2, 2, 2, 2, 2, 2, 2, 2, 2, 2, 2, 2, 2, 2, 2, 2, 2, 2, 2, 2, 2, 2, 2, 2, 2, 2, 2, 2, 2, 2, 2, 2, 2, 2, 2, 2, 2, 2, 2, 2, 2, 2, 2, 2, 2, 2, 2, 2, 2, 2, 2, 2, 2, 2, 2, 2, 2, 2, 2, 2, 2, 2, 2, 2, 2, 2, 2, 2, 2, 2, 2, 2, 2, 2, 2, 2, 2, 2, 2, 2, 2, 2, 2, 2, 2, 2, 2, 2, 2, 2, 2, 2, 2, 2, 2, 2, 2, 2, 2, 2, 2, 2, 2, 2, 2, 2, 2, 2, 2, 2, 2, 2, 2, 2, 2, 2, 2, 2, 2, 2, 2, 2, 2, 2, 2, 2, 3 ),
 ( 0.000000000000000000, 0.005000000000000000104, 0.01000000000000000021, 0.01499999999999999944, 0.02000000000000000042, 0.02500000000000000139, 0.02999999999999999889, 0.03500000000000000333, 0.04000000000000000083, 0.04499999999999999833, 0.05000000000000000278, 0.05500000000000000028, 0.05999999999999999778, 0.06500000000000000222, 0.07000000000000000666, 0.07499999999999999722, 0.08000000000000000167, 0.08500000000000000611, 0.08999999999999999667, 0.09500000000000000111, 0.1000000000000000056, 0.1049999999999999961, 0.1100000000000000006, 0.1150000000000000050, 0.1199999999999999956, 0.1250000000000000000, 0.1300000000000000044, 0.1350000000000000089, 0.1400000000000000133, 0.1449999999999999900, 0.1499999999999999944, 0.1549999999999999989, 0.1600000000000000033, 0.1650000000000000078, 0.1700000000000000122, 0.1749999999999999889, 0.1799999999999999933, 0.1849999999999999978, 0.1900000000000000022, 0.1950000000000000067, 0.2000000000000000111, 0.2049999999999999878, 0.2099999999999999922, 0.2149999999999999967, 0.2200000000000000011, 0.2250000000000000056, 0.2300000000000000100, 0.2349999999999999867, 0.2399999999999999911, 0.2449999999999999956, 0.2500000000000000000, 0.2550000000000000044, 0.2600000000000000089, 0.2650000000000000133, 0.2700000000000000178, 0.2750000000000000222, 0.2800000000000000266, 0.2849999999999999756, 0.2899999999999999800, 0.2949999999999999845, 0.2999999999999999889, 0.3049999999999999933, 0.3099999999999999978, 0.3150000000000000022, 0.3200000000000000067, 0.3250000000000000111, 0.3300000000000000155, 0.3350000000000000200, 0.3400000000000000244, 0.3449999999999999734, 0.3499999999999999778, 0.3549999999999999822, 0.3599999999999999867, 0.3649999999999999911, 0.3699999999999999956, 0.3750000000000000000, 0.3800000000000000044, 0.3850000000000000089, 0.3900000000000000133, 0.3950000000000000178, 0.4000000000000000222, 0.4050000000000000266, 0.4099999999999999756, 0.4149999999999999800, 0.4199999999999999845, 0.4249999999999999889, 0.4299999999999999933, 0.4349999999999999978, 0.4400000000000000022, 0.4450000000000000067, 0.4500000000000000111, 0.4550000000000000155, 0.4600000000000000200, 0.4650000000000000244, 0.4699999999999999734, 0.4749999999999999778, 0.4799999999999999822, 0.4849999999999999867, 0.4899999999999999911, 0.4949999999999999956, 0.5000000000000000000, 0.5050000000000000044, 0.5100000000000000089, 0.5150000000000000133, 0.5200000000000000178, 0.5250000000000000222, 0.5300000000000000266, 0.5350000000000000311, 0.5400000000000000355, 0.5450000000000000400, 0.5500000000000000444, 0.5550000000000000488, 0.5600000000000000533, 0.5649999999999999467, 0.5699999999999999512, 0.5749999999999999556, 0.5799999999999999600, 0.5849999999999999645, 0.5899999999999999689, 0.5949999999999999734, 0.5999999999999999778, 0.6049999999999999822, 0.6099999999999999867, 0.6149999999999999911, 0.6199999999999999956, 0.6250000000000000000, 0.6300000000000000044, 0.6350000000000000089, 0.6400000000000000133, 0.6450000000000000178, 0.6500000000000000222, 0.6550000000000000266, 0.6600000000000000311, 0.6650000000000000355, 0.6700000000000000400, 0.6750000000000000444, 0.6800000000000000488, 0.6850000000000000533, 0.6899999999999999467, 0.6949999999999999512, 0.6999999999999999556, 0.7049999999999999600, 0.7099999999999999645, 0.7149999999999999689, 0.7199999999999999734, 0.7249999999999999778, 0.7299999999999999822, 0.7349999999999999867, 0.7399999999999999911, 0.7449999999999999956, 0.7500000000000000000, 0.7550000000000000044, 0.7600000000000000089, 0.7650000000000000133, 0.7700000000000000178, 0.7750000000000000222, 0.7800000000000000266, 0.7850000000000000311, 0.7900000000000000355, 0.7950000000000000400, 0.8000000000000000444, 0.8050000000000000488, 0.8100000000000000533, 0.8149999999999999467, 0.8199999999999999512, 0.8249999999999999556, 0.8299999999999999600, 0.8349999999999999645, 0.8399999999999999689, 0.8449999999999999734, 0.8499999999999999778, 0.8549999999999999822, 0.8599999999999999867, 0.8649999999999999911, 0.8699999999999999956, 0.8750000000000000000, 0.8800000000000000044, 0.8850000000000000089, 0.8900000000000000133, 0.8950000000000000178, 0.9000000000000000222, 0.9050000000000000266, 0.9100000000000000311, 0.9150000000000000355, 0.9200000000000000400, 0.9250000000000000444, 0.9300000000000000488, 0.9350000000000000533, 0.9399999999999999467, 0.9449999999999999512, 0.9499999999999999556, 0.9549999999999999600, 0.9599999999999999645, 0.9649999999999999689, 0.9699999999999999734, 0.9749999999999999778, 0.9799999999999999822, 0.9849999999999999867, 0.9899999999999999911, 0.9949999999999999956, 1.000000000000000000 ),
 .UNSPECIFIED. ) 
 CURVE ( )  GEOMETRIC_REPRESENTATION_ITEM ( )  RATIONAL_B_SPLINE_CURVE ( ( 1.000000000000000000, 0.9510565162951535312, 1.000000000000000000, 0.9510565162951535312, 1.000000000000000000, 0.9510565162951535312, 1.000000000000000000, 0.9510565162951535312, 1.000000000000000000, 0.9510565162951535312, 1.000000000000000000, 0.9510565162951535312, 1.000000000000000000, 0.9510565162951535312, 1.000000000000000000, 0.9510565162951535312, 1.000000000000000000, 0.9510565162951535312, 1.000000000000000000, 0.9510565162951535312, 1.000000000000000000, 0.9510565162951535312, 1.000000000000000000, 0.9510565162951535312, 1.000000000000000000, 0.9510565162951535312, 1.000000000000000000, 0.9510565162951535312, 1.000000000000000000, 0.9510565162951535312, 1.000000000000000000, 0.9510565162951535312, 1.000000000000000000, 0.9510565162951535312, 1.000000000000000000, 0.9510565162951535312, 1.000000000000000000, 0.9510565162951535312, 1.000000000000000000, 0.9510565162951535312, 1.000000000000000000, 0.9510565162951535312, 1.000000000000000000, 0.9510565162951535312, 1.000000000000000000, 0.9510565162951535312, 1.000000000000000000, 0.9510565162951535312, 1.000000000000000000, 0.9510565162951535312, 1.000000000000000000, 0.9510565162951535312, 1.000000000000000000, 0.9510565162951535312, 1.000000000000000000, 0.9510565162951535312, 1.000000000000000000, 0.9510565162951535312, 1.000000000000000000, 0.9510565162951535312, 1.000000000000000000, 0.9510565162951535312, 1.000000000000000000, 0.9510565162951535312, 1.000000000000000000, 0.9510565162951535312, 1.000000000000000000, 0.9510565162951535312, 1.000000000000000000, 0.9510565162951535312, 1.000000000000000000, 0.9510565162951535312, 1.000000000000000000, 0.9510565162951535312, 1.000000000000000000, 0.9510565162951535312, 1.000000000000000000, 0.9510565162951535312, 1.000000000000000000, 0.9510565162951535312, 1.000000000000000000, 0.9510565162951535312, 1.000000000000000000, 0.9510565162951535312, 1.000000000000000000, 0.9510565162951535312, 1.000000000000000000, 0.9510565162951535312, 1.000000000000000000, 0.9510565162951535312, 1.000000000000000000, 0.9510565162951535312, 1.000000000000000000, 0.9510565162951535312, 1.000000000000000000, 0.9510565162951535312, 1.000000000000000000, 0.9510565162951535312, 1.000000000000000000, 0.9510565162951535312, 1.000000000000000000, 0.9510565162951535312, 1.000000000000000000, 0.9510565162951535312, 1.000000000000000000, 0.9510565162951535312, 1.000000000000000000, 0.9510565162951535312, 1.000000000000000000, 0.9510565162951535312, 1.000000000000000000, 0.9510565162951535312, 1.000000000000000000, 0.9510565162951535312, 1.000000000000000000, 0.9510565162951535312, 1.000000000000000000, 0.9510565162951535312, 1.000000000000000000, 0.9510565162951535312, 1.000000000000000000, 0.9510565162951535312, 1.000000000000000000, 0.9510565162951535312, 1.000000000000000000, 0.9510565162951535312, 1.000000000000000000, 0.9510565162951535312, 1.000000000000000000, 0.9510565162951535312, 1.000000000000000000, 0.9510565162951535312, 1.000000000000000000, 0.9510565162951535312, 1.000000000000000000, 0.9510565162951535312, 1.000000000000000000, 0.9510565162951535312, 1.000000000000000000, 0.9510565162951535312, 1.000000000000000000, 0.9510565162951535312, 1.000000000000000000, 0.9510565162951535312, 1.000000000000000000, 0.9510565162951535312, 1.000000000000000000, 0.9510565162951535312, 1.000000000000000000, 0.9510565162951535312, 1.000000000000000000, 0.9510565162951535312, 1.000000000000000000, 0.9510565162951535312, 1.000000000000000000, 0.9510565162951535312, 1.000000000000000000, 0.9510565162951535312, 1.000000000000000000, 0.9510565162951535312, 1.000000000000000000, 0.9510565162951535312, 1.000000000000000000, 0.9510565162951535312, 1.000000000000000000, 0.9510565162951535312, 1.000000000000000000, 0.9510565162951535312, 1.000000000000000000, 0.9510565162951535312, 1.000000000000000000, 0.9510565162951535312, 1.000000000000000000, 0.9510565162951535312, 1.000000000000000000, 0.9510565162951535312, 1.000000000000000000, 0.9510565162951535312, 1.000000000000000000, 0.9510565162951535312, 1.000000000000000000, 0.9510565162951535312, 1.000000000000000000, 0.9510565162951535312, 1.000000000000000000, 0.9510565162951535312, 1.000000000000000000, 0.9510565162951535312, 1.000000000000000000, 0.9510565162951535312, 1.000000000000000000, 0.9510565162951535312, 1.000000000000000000, 0.9510565162951535312, 1.000000000000000000, 0.9510565162951535312, 1.000000000000000000, 0.9510565162951535312, 1.000000000000000000, 0.9510565162951535312, 1.000000000000000000, 0.9510565162951535312, 1.000000000000000000, 0.9510565162951535312, 1.000000000000000000, 0.9510565162951535312, 1.000000000000000000, 0.9510565162951535312, 1.000000000000000000, 0.9510565162951535312, 1.000000000000000000, 0.9510565162951535312, 1.000000000000000000, 0.9510565162951535312, 1.000000000000000000, 0.9510565162951535312, 1.000000000000000000, 0.9510565162951535312, 1.000000000000000000, 0.9510565162951535312, 1.000000000000000000, 0.9510565162951535312, 1.000000000000000000, 0.9510565162951535312, 1.000000000000000000, 0.9510565162951535312, 1.000000000000000000, 0.9510565162951535312, 1.000000000000000000, 0.9510565162951535312, 1.000000000000000000, 0.9510565162951535312, 1.000000000000000000, 0.9510565162951535312, 1.000000000000000000, 0.9510565162951535312, 1.000000000000000000, 0.9510565162951535312, 1.000000000000000000, 0.9510565162951535312, 1.000000000000000000, 0.9510565162951535312, 1.000000000000000000, 0.9510565162951535312, 1.000000000000000000, 0.9510565162951535312, 1.000000000000000000, 0.9510565162951535312, 1.000000000000000000, 0.9510565162951535312, 1.000000000000000000, 0.9510565162951535312, 1.000000000000000000, 0.9510565162951535312, 1.000000000000000000, 0.9510565162951535312, 1.000000000000000000, 0.9510565162951535312, 1.000000000000000000, 0.9510565162951535312, 1.000000000000000000, 0.9510565162951535312, 1.000000000000000000, 0.9510565162951535312, 1.000000000000000000, 0.9510565162951535312, 1.000000000000000000, 0.9510565162951535312, 1.000000000000000000, 0.9510565162951535312, 1.000000000000000000, 0.9510565162951535312, 1.000000000000000000, 0.9510565162951535312, 1.000000000000000000, 0.9510565162951535312, 1.000000000000000000, 0.9510565162951535312, 1.000000000000000000, 0.9510565162951535312, 1.000000000000000000, 0.9510565162951535312, 1.000000000000000000, 0.9510565162951535312, 1.000000000000000000, 0.9510565162951535312, 1.000000000000000000, 0.9510565162951535312, 1.000000000000000000, 0.9510565162951535312, 1.000000000000000000, 0.9510565162951535312, 1.000000000000000000, 0.9510565162951535312, 1.000000000000000000, 0.9510565162951535312, 1.000000000000000000, 0.9510565162951535312, 1.000000000000000000, 0.9510565162951535312, 1.000000000000000000, 0.9510565162951535312, 1.000000000000000000, 0.9510565162951535312, 1.000000000000000000, 0.9510565162951535312, 1.000000000000000000, 0.9510565162951535312, 1.000000000000000000, 0.9510565162951535312, 1.000000000000000000, 0.9510565162951535312, 1.000000000000000000, 0.9510565162951535312, 1.000000000000000000, 0.9510565162951535312, 1.000000000000000000, 0.9510565162951535312, 1.000000000000000000, 0.9510565162951535312, 1.000000000000000000, 0.9510565162951535312, 1.000000000000000000, 0.9510565162951535312, 1.000000000000000000, 0.9510565162951535312, 1.000000000000000000, 0.9510565162951535312, 1.000000000000000000, 0.9510565162951535312, 1.000000000000000000, 0.9510565162951535312, 1.000000000000000000, 0.9510565162951535312, 1.000000000000000000, 0.9510565162951535312, 1.000000000000000000, 0.9510565162951535312, 1.000000000000000000, 0.9510565162951535312, 1.000000000000000000, 0.9510565162951535312, 1.000000000000000000, 0.9510565162951535312, 1.000000000000000000, 0.9510565162951535312, 1.000000000000000000, 0.9510565162951535312, 1.000000000000000000, 0.9510565162951535312, 1.000000000000000000, 0.9510565162951535312, 1.000000000000000000, 0.9510565162951535312, 1.000000000000000000, 0.9510565162951535312, 1.000000000000000000, 0.9510565162951535312, 1.000000000000000000, 0.9510565162951535312, 1.000000000000000000, 0.9510565162951535312, 1.000000000000000000, 0.9510565162951535312, 1.000000000000000000, 0.9510565162951535312, 1.000000000000000000, 0.9510565162951535312, 1.000000000000000000, 0.9510565162951535312, 1.000000000000000000, 0.9510565162951535312, 1.000000000000000000, 0.9510565162951535312, 1.000000000000000000, 0.9510565162951535312, 1.000000000000000000, 0.9510565162951535312, 1.000000000000000000, 0.9510565162951535312, 1.000000000000000000, 0.9510565162951535312, 1.000000000000000000, 0.9510565162951535312, 1.000000000000000000, 0.9510565162951535312, 1.000000000000000000, 0.9510565162951535312, 1.000000000000000000, 0.9510565162951535312, 1.000000000000000000, 0.9510565162951535312, 1.000000000000000000, 0.9510565162951535312, 1.000000000000000000, 0.9510565162951535312, 1.000000000000000000, 0.9510565162951535312, 1.000000000000000000, 0.9510565162951535312, 1.000000000000000000 ) ) 
 REPRESENTATION_ITEM ( '' )  );
#86053 = CARTESIAN_POINT ( 'NONE',  ( 74.04521871459132853, 68.62337475623881744, 10.92041412683466106 ) ) ;
#86054 = CARTESIAN_POINT ( 'NONE',  ( 71.04896452076110336, 71.47008843830593605, -2.670135699880026969 ) ) ;
#86055 = CARTESIAN_POINT ( 'NONE',  ( -0.5819415548772214342, 158.2202760586659451, -5.415160957724236172E-17 ) ) ;
#86056 = ADVANCED_FACE ( 'NONE', ( #1609 ), #90522, .F. ) ;
#86057 = CARTESIAN_POINT ( 'NONE',  ( 94.46399941469991290, 225.3458772461660544, 9.188101187500095079 ) ) ;
#86058 = CARTESIAN_POINT ( 'NONE',  ( 26.94108121515588294, 196.3615022471903160, 5.000000000000046185 ) ) ;
#86059 = CARTESIAN_POINT ( 'NONE',  ( 192.6789561813392595, 296.9172536750198219, -11.84591848451790952 ) ) ;
#86060 = CARTESIAN_POINT ( 'NONE',  ( -19.65312891409030271, 93.06504152958497400, 10.00000000000000888 ) ) ;
#86061 = ADVANCED_FACE ( 'NONE', ( #58276, #97312, #27879, #13199, #19802, #58761, #57274, #42563, #50183, #4584, #88250, #20292, #73012, #18798, #49680, #80636, #82132, #50669, #81621, #11213, #96325, #12194, #26895, #57773, #43053, #12704, #43574, #73999, #29385, #98298, #84613, #91709, #14184, #15152, #61258, #99785, #67372, #45559, #22271, #45069, #37951, #22778, #37457, #53175, #14678, #53655, #76008, #84129, #28887, #21772, #52662 ), #68860, .F. ) ;
#86062 = CARTESIAN_POINT ( 'NONE',  ( -16.76269525828470464, 104.2312461070085021, 45.19948692389422717 ) ) ;
#86063 = CARTESIAN_POINT ( 'NONE',  ( -50.07135831343601495, 43.74682248199032841, 59.99999999999999289 ) ) ;
#86064 = CARTESIAN_POINT ( 'NONE',  ( 174.0424481033923314, 287.4814580433055653, 10.99910921803667208 ) ) ;
#86066 = FACE_OUTER_BOUND ( 'NONE', #65878, .T. ) ;
#86065 = DIRECTION ( 'NONE',  ( -1.000000000000000000, 0.000000000000000000, -0.000000000000000000 ) ) ;
#86067 = CARTESIAN_POINT ( 'NONE',  ( 179.7416253924201897, 290.4642672521716236, 9.368538271801467587 ) ) ;
#86068 = CARTESIAN_POINT ( 'NONE',  ( 169.2145703546568427, 252.0716163555370883, -8.781996148431376881 ) ) ;
#86069 = CARTESIAN_POINT ( 'NONE',  ( 164.7496056545292049, 245.2923078098555436, -4.800585399662008257 ) ) ;
#86070 = CARTESIAN_POINT ( 'NONE',  ( 168.3038276672707809, 273.7088255811268596, 16.50406143123535685 ) ) ;
#86071 = CARTESIAN_POINT ( 'NONE',  ( 196.1613785401733878, 290.8855212161054737, 15.98157687694135021 ) ) ;
#86072 = B_SPLINE_CURVE_WITH_KNOTS ( 'NONE', 3,
 ( #21275, #68848, #21758, #52152, #15136, #99769, #30360, #83101, #61245, #7550, #100275, #30861, #92694, #23245, #44544, #54132, #85095, #15641, #48565, #47056, #48050, #55633, #86618, #9063, #47549, #56137, #77970, #77475, #17152, #31352, #462, #1475, #39432, #24752, #54636, #71878, #8565, #32356, #78992, #87638, #9578, #40442, #39930, #63760, #2477, #64258, #25778, #32851, #24261, #18166, #56653, #62742 ),
 .UNSPECIFIED., .F., .F.,
 ( 4, 2, 2, 2, 2, 2, 2, 2, 2, 2, 2, 2, 2, 2, 2, 2, 2, 2, 2, 2, 2, 2, 2, 2, 2, 4 ),
 ( 0.0008473748616542479744, 0.001046208493274463670, 0.001145625309084543492, 0.001245042124894623313, 0.001443875756514765392, 0.001642709388134907687, 0.002040376651375070197, 0.002438043914615233357, 0.003233378441095451257, 0.004028712967575669157, 0.004824047494055886190, 0.005221714757295984298, 0.005420548388916032918, 0.005519965204726057229, 0.005569673612631022112, 0.005619382020535987864, 0.005669090428440952747, 0.005718798836345917631, 0.005818215652155869951, 0.006017049283775706935, 0.006215882915395543919, 0.006414716547015380903, 0.006613550178635217887, 0.006812383810255055738, 0.007011217441874892722, 0.007210051073494728839 ),
 .UNSPECIFIED. ) ;
#86073 = CARTESIAN_POINT ( 'NONE',  ( -15.31269525828471068, 104.2312461070085021, 45.19948692389422717 ) ) ;
#86074 = CARTESIAN_POINT ( 'NONE',  ( 72.94248495762835205, 57.43054579428017803, -15.86422397714476773 ) ) ;
#86075 = CARTESIAN_POINT ( 'NONE',  ( 39.87759600423577666, 184.6423013555410080, -4.594050593750043987 ) ) ;
#86076 = CARTESIAN_POINT ( 'NONE',  ( 65.07308872588301085, 214.5024278399160949, -9.188101187500093303 ) ) ;
#86077 = DIRECTION ( 'NONE',  ( -0.7135562106085605594, 0.7005979833698863235, 0.000000000000000000 ) ) ;
#86078 = CARTESIAN_POINT ( 'NONE',  ( 88.35351169220642475, 43.78681510747281180, 0.1754685934989752005 ) ) ;
#86079 = B_SPLINE_CURVE_WITH_KNOTS ( 'NONE', 3,
 ( #16717, #23810, #55199, #54699 ),
 .UNSPECIFIED., .F., .F.,
 ( 4, 4 ),
 ( 0.004402801596837424558, 0.009103939997633007583 ),
 .UNSPECIFIED. ) ;
#86080 = CARTESIAN_POINT ( 'NONE',  ( 97.08913892169542237, 236.8615022471903160, 5.000000000000046185 ) ) ;
#86081 = CARTESIAN_POINT ( 'NONE',  ( 146.4255236417662616, 255.3458772461660260, 9.188101187500095079 ) ) ;
#86083 = CARTESIAN_POINT ( 'NONE',  ( 70.84625275103223885, 71.05098293809255949, -5.242152369257887301 ) ) ;
#86082 = CARTESIAN_POINT ( 'NONE',  ( 71.67184923690800247, 72.06465046553262255, -3.547063142499712551 ) ) ;
#86084 = CARTESIAN_POINT ( 'NONE',  ( 196.2549797335509538, 269.5255532092754720, -10.78968121037139305 ) ) ;
#86085 = CARTESIAN_POINT ( 'NONE',  ( 22.87854050506884818, 34.18502408145592852, 5.678558825948276656 ) ) ;
#86086 = CARTESIAN_POINT ( 'NONE',  ( 198.4860348845112981, 286.8590983175747056, -18.20461732983060088 ) ) ;
#86087 = CARTESIAN_POINT ( 'NONE',  ( 83.86604369230676070, 46.91831489429971214, -11.24295167143095497 ) ) ;
#86088 = CARTESIAN_POINT ( 'NONE',  ( 16.17343562415726765, 11.19860640527290840, 2.839279412974134775 ) ) ;
#86089 = CARTESIAN_POINT ( 'NONE',  ( 72.89481452351749624, 203.7048013555409796, 4.594050593750051981 ) ) ;
#86090 = CARTESIAN_POINT ( 'NONE',  ( 76.75190111695991391, 63.66135907976974551, 15.32171075625996259 ) ) ;
#86091 = CARTESIAN_POINT ( 'NONE',  ( 154.8786460229866577, 262.3893114111486398, -18.06164891362396929 ) ) ;
#86092 = CARTESIAN_POINT ( 'NONE',  ( 198.6742831389107096, 286.5330427765190393, 17.60232614297041565 ) ) ;
#86093 = CARTESIAN_POINT ( 'NONE',  ( 73.92247914240149953, 66.41009877986448373, 12.60535242438584191 ) ) ;
#86094 = CARTESIAN_POINT ( 'NONE',  ( 198.9746108066164254, 281.0633597085003998, 17.36576938231656442 ) ) ;
#86095 = AXIS2_PLACEMENT_3D ( 'NONE', #20515, #99010, #22490 ) ;
#86096 = CARTESIAN_POINT ( 'NONE',  ( 101.3470971569689283, 235.9865022471903160, 10.00000000000009237 ) ) ;
#86097 = CARTESIAN_POINT ( 'NONE',  ( -20.78562219458220284, 95.22657743062728741, 45.19937630303414267 ) ) ;
#86098 = ORIENTED_EDGE ( 'NONE', *, *, #78821, .F. ) ;
#86099 = CARTESIAN_POINT ( 'NONE',  ( 77.03809386778178236, 49.55778004163211392, 14.99421684170569335 ) ) ;
#86100 = CARTESIAN_POINT ( 'NONE',  ( 185.1165591157377150, 271.2723187119548811, 16.65506677990856943 ) ) ;
#86101 = ORIENTED_EDGE ( 'NONE', *, *, #84930, .T. ) ;
#86102 = CARTESIAN_POINT ( 'NONE',  ( 159.9647205790309101, 253.5799718689968927, -16.48298384325780219 ) ) ;
#86103 = CARTESIAN_POINT ( 'NONE',  ( 190.3444704496978659, 278.7135669931259940, -16.51019796646277271 ) ) ;
#86104 = CARTESIAN_POINT ( 'NONE',  ( 71.74269501503555091, 72.54435722921776630, -0.3765977487197710860 ) ) ;
#86105 = CARTESIAN_POINT ( 'NONE',  ( 174.0867956421258498, 252.1420213558926946, -0.2508409156989133693 ) ) ;
#86106 = VERTEX_POINT ( 'NONE', #68369 ) ;
#86107 = CARTESIAN_POINT ( 'NONE',  ( 72.49520321802694411, 71.62171839754151392, 6.144630347475399823 ) ) ;
#86108 = CARTESIAN_POINT ( 'NONE',  ( 194.6943296385021824, 293.4265244509877562, -16.10917128197217352 ) ) ;
#86109 = CARTESIAN_POINT ( 'NONE',  ( 206.7325995683429767, 270.5756292972641859, -5.459556455514786855 ) ) ;
#86110 = EDGE_CURVE ( 'NONE', #14295, #69000, #56074, .T. ) ;
#86111 = ORIENTED_EDGE ( 'NONE', *, *, #71507, .F. ) ;
#86112 = CARTESIAN_POINT ( 'NONE',  ( 26.18145187173165311, 30.51421378149920116, -9.188101187500004485 ) ) ;
#86113 = CARTESIAN_POINT ( 'NONE',  ( -19.65312891409030271, 93.06504152958497400, 177.5919119679930134 ) ) ;
#86114 = CARTESIAN_POINT ( 'NONE',  ( 84.60735463175657856, 50.53152741511170376, -13.60229262011999296 ) ) ;
#86115 = ORIENTED_EDGE ( 'NONE', *, *, #22591, .F. ) ;
#86116 = DIRECTION ( 'NONE',  ( -0.8660254037844379305, -0.5000000000000014433, -0.000000000000000000 ) ) ;
#86117 = CYLINDRICAL_SURFACE ( 'NONE', #93367, 10.00000000000010658 ) ;
#86118 = VERTEX_POINT ( 'NONE', #7067 ) ;
#86119 = DIRECTION ( 'NONE',  ( -0.8560416229147732592, -0.5169068966820244970, 0.000000000000000000 ) ) ;
#86121 = CARTESIAN_POINT ( 'NONE',  ( 67.90305891752841205, 66.04211081269261285, -10.46789290119909843 ) ) ;
#86120 = CARTESIAN_POINT ( 'NONE',  ( 68.14508661930936739, 65.47790460345626684, 10.45464874189764615 ) ) ;
#86122 = CARTESIAN_POINT ( 'NONE',  ( 168.7621418133986424, 265.8582162196448166, -17.70435637355228664 ) ) ;
#86123 = CARTESIAN_POINT ( 'NONE',  ( 154.9226727788713731, 262.3130548330639726, 18.22497199616848818 ) ) ;
#86124 = CARTESIAN_POINT ( 'NONE',  ( 70.27722316875779995, 71.69590253475411146, -0.4825279500921932363 ) ) ;
#86125 = CARTESIAN_POINT ( 'NONE',  ( 157.1458804504438831, 258.4623461901232417, -17.08829597948888335 ) ) ;
#86126 = EDGE_CURVE ( 'NONE', #52672, #10803, #30375, .T. ) ;
#86127 = CARTESIAN_POINT ( 'NONE',  ( 137.8192226437758450, 256.5024278399160380, -9.188101187500093303 ) ) ;
#86128 = CARTESIAN_POINT ( 'NONE',  ( 203.1890483204367115, 268.4214926066569546, 2.485490542415017767 ) ) ;
#86129 = CARTESIAN_POINT ( 'NONE',  ( 79.35100834308954632, 59.73271264539057057, 16.51943372556189971 ) ) ;
#86130 = CARTESIAN_POINT ( 'NONE',  ( 97.82019495012963262, 215.0327760586659451, 1.948934522072303157E-15 ) ) ;
#86131 = EDGE_LOOP ( 'NONE', ( #67621, #86374, #16254, #36494 ) ) ;
#86132 = CARTESIAN_POINT ( 'NONE',  ( 151.4361976351029000, 268.3518069213970421, 15.15218985681980612 ) ) ;
#86133 = CARTESIAN_POINT ( 'NONE',  ( 192.1779685593947420, 266.1842805242176269, 11.64530923862864142 ) ) ;
#86134 = VERTEX_POINT ( 'NONE', #69370 ) ;
#86135 = AXIS2_PLACEMENT_3D ( 'NONE', #33467, #95324, #25881 ) ;
#86136 = CARTESIAN_POINT ( 'NONE',  ( 195.5954130450106732, 291.8658022090583017, -15.71558652822518987 ) ) ;
#86137 = VERTEX_POINT ( 'NONE', #21290 ) ;
#86138 = DIRECTION ( 'NONE',  ( 0.5000000000000003331, -0.8660254037844385966, 8.877441173312408730E-15 ) ) ;
#86139 = CARTESIAN_POINT ( 'NONE',  ( -19.65312891409030271, 93.06504152958497400, -10.00000000000000000 ) ) ;
#86141 = B_SPLINE_SURFACE_WITH_KNOTS ( 'NONE', 3, 1, ( 
 ( #31484, #92342 ),
 ( #99914, #22401 ),
 ( #62376, #29996 ),
 ( #45193, #39073 ),
 ( #108, #54788 ),
 ( #29505, #60878 ),
 ( #22891, #14797 ),
 ( #23383, #46694 ),
 ( #92832, #16295 ),
 ( #54273, #38076 ),
 ( #85242, #45679 ),
 ( #68989, #8204 ),
 ( #15786, #14307 ),
 ( #600, #61388 ),
 ( #39569, #6707 ),
 ( #52787, #37585 ),
 ( #77619, #53776 ),
 ( #38589, #23886 ),
 ( #93333, #69986 ),
 ( #85767, #47190 ),
 ( #78111, #84739 ),
 ( #8701, #7697 ),
 ( #98927, #60382 ),
 ( #91338, #21898 ),
 ( #83744, #69495 ),
 ( #15280, #46175 ),
 ( #99419, #77095 ),
 ( #71521, #41076 ),
 ( #94833, #40075 ),
 ( #40580, #1107 ),
 ( #78616, #70492 ),
 ( #80645, #25396 ),
 ( #95365, #41586 ),
 ( #25918, #11223 ) ),
 .UNSPECIFIED., .T., .F., .F.,
 ( 4, 2, 2, 2, 2, 2, 2, 2, 2, 2, 2, 2, 2, 2, 2, 2, 4 ),
 ( 2, 2 ),
 ( 0.000000000000000000, 0.06250000000000000000, 0.1250000000000000000, 0.1875000000000000000, 0.2500000000000000000, 0.3125000000000000000, 0.3750000000000000000, 0.4375000000000000000, 0.5000000000000000000, 0.5625000000000000000, 0.6250000000000000000, 0.6875000000000000000, 0.7500000000000000000, 0.8125000000000000000, 0.8750000000000000000, 0.9375000000000000000, 1.000000000000000000 ),
 ( 0.000000000000000000, 1.000000000000000000 ),
 .UNSPECIFIED. ) ;
#86140 = FACE_OUTER_BOUND ( 'NONE', #75588, .T. ) ;
#86142 = CARTESIAN_POINT ( 'NONE',  ( 80.98575723459396158, 56.01296387717067660, 16.09851198889879242 ) ) ;
#86143 = CARTESIAN_POINT ( 'NONE',  ( -22.42236680055709641, 157.8615022471902591, 0.000000000000000000 ) ) ;
#86144 = CARTESIAN_POINT ( 'NONE',  ( 162.6684717218148251, 248.8969375186720754, 11.76041465758671833 ) ) ;
#86145 = CARTESIAN_POINT ( 'NONE',  ( 79.55186417146283873, 225.9244531367911293, -4.594050593750046652 ) ) ;
#86146 = ORIENTED_EDGE ( 'NONE', *, *, #26322, .F. ) ;
#86147 = ORIENTED_EDGE ( 'NONE', *, *, #63926, .F. ) ;
#86148 = CARTESIAN_POINT ( 'NONE',  ( 121.6806519464431773, 234.3927522451418213, 10.00000000000009948 ) ) ;
#86149 = AXIS2_PLACEMENT_3D ( 'NONE', #24949, #87832, #17353 ) ;
#86150 = CARTESIAN_POINT ( 'NONE',  ( 163.1096928939807924, 248.1327200311062882, -9.690381021358412283 ) ) ;
#86151 = VERTEX_POINT ( 'NONE', #52165 ) ;
#86152 = CARTESIAN_POINT ( 'NONE',  ( 57.56414817410228579, 217.3207943907112281, -18.47570218321542868 ) ) ;
#86153 = CARTESIAN_POINT ( 'NONE',  ( 75.84431516675671503, 65.82088634210550993, -14.12726274127321169 ) ) ;
#86154 = CARTESIAN_POINT ( 'NONE',  ( -30.02241387713131004, 93.66080434060147297, 44.35815572581725519 ) ) ;
#86155 = CARTESIAN_POINT ( 'NONE',  ( -24.92236680055712839, 162.1916292661124999, 6.123233995736853057E-16 ) ) ;
#86156 = CARTESIAN_POINT ( 'NONE',  ( 87.51647913336859119, 44.56403561216111342, 4.883618514853089287 ) ) ;
#86157 = CARTESIAN_POINT ( 'NONE',  ( 84.48772039313885784, 43.72266692861629878, -6.677769858850941986 ) ) ;
#86158 = CARTESIAN_POINT ( 'NONE',  ( 185.7058167950441145, 259.5999620644902848, 5.848445963200036957 ) ) ;
#86159 = CARTESIAN_POINT ( 'NONE',  ( 206.1798448551755598, 273.5330285446045195, -10.53862763475382813 ) ) ;
#86160 = CARTESIAN_POINT ( 'NONE',  ( 147.8652489956357101, 275.2099377555215369, -4.764731639000758356 ) ) ;
#86161 = CARTESIAN_POINT ( 'NONE',  ( -17.42236680055705023, 149.2012482093457777, 0.000000000000000000 ) ) ;
#86162 = CARTESIAN_POINT ( 'NONE',  ( 198.9145269359414669, 284.9342556184034265, -17.40143518274985723 ) ) ;
#86163 = DIRECTION ( 'NONE',  ( 0.8660254037844377084, 0.5000000000000015543, -0.000000000000000000 ) ) ;
#86164 = EDGE_LOOP ( 'NONE', ( #65036, #99150, #67162, #2371 ) ) ;
#86165 = CARTESIAN_POINT ( 'NONE',  ( 196.2335616883709122, 265.6660282062799183, 4.428010252653890255 ) ) ;
#86166 = CARTESIAN_POINT ( 'NONE',  ( 200.6129772034685175, 283.1751261563724142, 18.36811917402039640 ) ) ;
#86167 = CARTESIAN_POINT ( 'NONE',  ( 80.87517248313827167, 58.64441083166272506, 0.000000000000000000 ) ) ;
#86168 = CARTESIAN_POINT ( 'NONE',  ( 187.8291388526744186, 266.0904899704142963, -11.84232036284073253 ) ) ;
#86169 = CARTESIAN_POINT ( 'NONE',  ( 198.5095674088818782, 266.2393955469675575, 0.9580096654556583546 ) ) ;
#86170 = CARTESIAN_POINT ( 'NONE',  ( 153.0105784145868881, 270.8266541147344810, 13.92684810197993350 ) ) ;
#86171 = EDGE_CURVE ( 'NONE', #14510, #93933, #45558, .T. ) ;
#86172 = VERTEX_POINT ( 'NONE', #90557 ) ;
#86173 = CARTESIAN_POINT ( 'NONE',  ( 162.6264071486809542, 248.9697954965390920, 10.36322805486644683 ) ) ;
#86174 = CARTESIAN_POINT ( 'NONE',  ( 207.3502731283117555, 271.5057873089173768, 6.280625384230454245 ) ) ;
#86176 = CARTESIAN_POINT ( 'NONE',  ( 73.70324744805795092, 55.29378421878942618, 16.59304382234686770 ) ) ;
#86175 = CARTESIAN_POINT ( 'NONE',  ( 57.56414817410227158, 217.3207943907112281, -18.47570218321543578 ) ) ;
#86177 = CARTESIAN_POINT ( 'NONE',  ( 186.8123841630082040, 258.3999256946553942, 3.104652050626591553 ) ) ;
#86178 = CARTESIAN_POINT ( 'NONE',  ( 27.37565231528585485, 31.50829794293882458, -10.00000000000000355 ) ) ;
#86179 = CARTESIAN_POINT ( 'NONE',  ( 171.4574563581475388, 274.7666223272099160, 17.16070901681419514 ) ) ;
#86180 = CARTESIAN_POINT ( 'NONE',  ( 164.2119285677552796, 284.2824924003866158, -3.118288404568473560 ) ) ;
#86181 = CARTESIAN_POINT ( 'NONE',  ( 124.7815979145579632, 254.3967562850346553, -4.648177544792955347E-16 ) ) ;
#86182 = CARTESIAN_POINT ( 'NONE',  ( 188.2791287928231156, 260.8518096374758102, 2.898815310248603172 ) ) ;
#86183 = CARTESIAN_POINT ( 'NONE',  ( 66.22544472841278207, 69.36168339246576409, 0.1681495645362244273 ) ) ;
#86184 = CARTESIAN_POINT ( 'NONE',  ( 3.504529045289348055, 163.6423013555410080, -4.594050593750043987 ) ) ;
#86185 = ORIENTED_EDGE ( 'NONE', *, *, #80627, .F. ) ;
#86186 = CARTESIAN_POINT ( 'NONE',  ( 174.8738442610398067, 255.2983538659211433, 8.879037836851004784 ) ) ;
#86187 = CARTESIAN_POINT ( 'NONE',  ( 180.7942833579522812, 266.7097690628117448, -16.23795806611159520 ) ) ;
#86188 = CARTESIAN_POINT ( 'NONE',  ( 189.4308808934198680, 289.8491723414206831, 15.72891001903047048 ) ) ;
#86189 = CARTESIAN_POINT ( 'NONE',  ( 81.83513327003998938, 41.26677966152606558, 5.885019063842929832 ) ) ;
#86190 = CARTESIAN_POINT ( 'NONE',  ( 24.31594170816038059, 184.8458772461660544, 9.188101187500095079 ) ) ;
#86191 = VECTOR ( 'NONE', #67851, 1000.000000000000114 ) ;
#86192 = DIRECTION ( 'NONE',  ( 0.5000000000000014433, -0.8660254037844378194, 0.000000000000000000 ) ) ;
#86193 = CARTESIAN_POINT ( 'NONE',  ( 27.54669006335486614, 38.83705186507756224, 3.090169943749475401 ) ) ;
#86194 = CARTESIAN_POINT ( 'NONE',  ( 78.44203751522358914, 61.21016990572090322, 16.24725970467587643 ) ) ;
#86195 = CARTESIAN_POINT ( 'NONE',  ( 147.0660117096331874, 275.9211909828330249, -0.7354350123930680772 ) ) ;
#86196 = CARTESIAN_POINT ( 'NONE',  ( 73.68461719894507667, 68.07295893857846636, 11.72993004162934483 ) ) ;
#86197 = CARTESIAN_POINT ( 'NONE',  ( 87.18660594880147130, 46.21918437583570238, -8.412104891579501142 ) ) ;
#86198 = CARTESIAN_POINT ( 'NONE',  ( 87.98594423550160570, 43.75089820288620501, -2.253463800273097561 ) ) ;
#86199 = CARTESIAN_POINT ( 'NONE',  ( 70.67536410627006660, 211.6115022471902591, 10.00000000000009592 ) ) ;
#86200 = CARTESIAN_POINT ( 'NONE',  ( 165.4315485841760278, 245.8874648686309854, 0.7284626796912114788 ) ) ;
#86201 = CARTESIAN_POINT ( 'NONE',  ( 203.3725525628211699, 270.0917528869257467, 6.095119953602265106 ) ) ;
#86202 = CARTESIAN_POINT ( 'NONE',  ( 37.30632276492696064, 192.3458772461660544, 9.188101187500095079 ) ) ;
#86203 = CARTESIAN_POINT ( 'NONE',  ( 67.68514482100736984, 66.83340866827894899, -8.536435324610977204 ) ) ;
#86204 = CARTESIAN_POINT ( 'NONE',  ( 77.54361356138011274, 49.75803992512373952, -14.96129575302290249 ) ) ;
#86205 = CARTESIAN_POINT ( 'NONE',  ( 206.3592393881182545, 269.7258222359968158, -3.299573838669981551 ) ) ;
#86206 = B_SPLINE_CURVE_WITH_KNOTS ( 'NONE', 3,
 ( #91562, #52524, #14038, #16024 ),
 .UNSPECIFIED., .F., .F.,
 ( 4, 4 ),
 ( 0.001920166038260726462, 0.003922728456736315761 ),
 .UNSPECIFIED. ) ;
#86207 = FACE_OUTER_BOUND ( 'NONE', #19924, .T. ) ;
#86209 = DIRECTION ( 'NONE',  ( 0.5000000000000014433, -0.8660254037844378194, 0.000000000000000000 ) ) ;
#86208 = AXIS2_PLACEMENT_3D ( 'NONE', #95501, #728, #48342 ) ;
#86210 = CARTESIAN_POINT ( 'NONE',  ( 202.0661878422603763, 279.1895584290143120, -16.02388874507808225 ) ) ;
#86211 = CARTESIAN_POINT ( 'NONE',  ( 205.8195061805951696, 269.6042235147296537, -1.323967559255036175 ) ) ;
#86212 = CARTESIAN_POINT ( 'NONE',  ( 20.38389956778225809, 29.95586893147755703, 7.433330006724141015 ) ) ;
#86213 = CARTESIAN_POINT ( 'NONE',  ( 202.5245888501533216, 279.8641176599742266, 15.60152447840272494 ) ) ;
#86214 = CARTESIAN_POINT ( 'NONE',  ( 149.4965729687386045, 271.7113353911534546, -11.48413836595348059 ) ) ;
#86215 = ADVANCED_FACE ( 'NONE', ( #19138 ), #66176, .F. ) ;
#86216 = CARTESIAN_POINT ( 'NONE',  ( 186.0519134971170843, 268.1729366909127066, -14.31315269452955441 ) ) ;
#86217 = ORIENTED_EDGE ( 'NONE', *, *, #48882, .F. ) ;
#86218 = CARTESIAN_POINT ( 'NONE',  ( 10.59299460361177303, 21.51421378149917629, -9.188101187500004485 ) ) ;
#86219 = CARTESIAN_POINT ( 'NONE',  ( 71.63674389864488035, 60.29001788040124410, -14.97147996658655345 ) ) ;
#86220 = CARTESIAN_POINT ( 'NONE',  ( 71.54037008220826976, 72.37285432226113358, -1.295160433098011543 ) ) ;
#86221 = ORIENTED_EDGE ( 'NONE', *, *, #46075, .F. ) ;
#86222 = LINE ( 'NONE', #76, #11828 ) ;
#86223 = CARTESIAN_POINT ( 'NONE',  ( 69.80538936212087719, 70.80406902493081134, -1.980385850607123688 ) ) ;
#86224 = CARTESIAN_POINT ( 'NONE',  ( 85.57888796130104936, 49.00383361444075803, 12.24411226656481588 ) ) ;
#86225 = LINE ( 'NONE', #23856, #37152 ) ;
#86226 = EDGE_CURVE ( 'NONE', #84464, #48146, #21610, .T. ) ;
#86227 = ORIENTED_EDGE ( 'NONE', *, *, #71828, .T. ) ;
#86228 = EDGE_LOOP ( 'NONE', ( #7971, #12309, #68246, #2880 ) ) ;
#86230 = CARTESIAN_POINT ( 'NONE',  ( 86.80341134427941086, 43.38235068936107552, -1.253824059860942697 ) ) ;
#86229 = CYLINDRICAL_SURFACE ( 'NONE', #77878, 10.00000000000001066 ) ;
#86231 = ORIENTED_EDGE ( 'NONE', *, *, #77053, .F. ) ;
#86232 = DIRECTION ( 'NONE',  ( -0.000000000000000000, -0.000000000000000000, -1.000000000000000000 ) ) ;
#86233 = CARTESIAN_POINT ( 'NONE',  ( 71.73704408672971056, 72.08698097738312072, -3.607164568159269891 ) ) ;
#86234 = CARTESIAN_POINT ( 'NONE',  ( 79.88594259850813728, 58.03267954034458143, 16.26759869156149563 ) ) ;
#86235 = CARTESIAN_POINT ( 'NONE',  ( 76.83059214691050443, 63.69233987691562504, 15.32693845983791547 ) ) ;
#86236 = EDGE_CURVE ( 'NONE', #947, #46582, #5741, .T. ) ;
#86237 = CARTESIAN_POINT ( 'NONE',  ( 189.8480911035503880, 301.8204558191226283, -0.8992086515915015399 ) ) ;
#86238 = CARTESIAN_POINT ( 'NONE',  ( 184.1636269873439460, 288.8002302501334952, -13.16066999487799372 ) ) ;
#86239 = ORIENTED_EDGE ( 'NONE', *, *, #30161, .F. ) ;
#86240 = CARTESIAN_POINT ( 'NONE',  ( 172.9438399295877957, 262.8668947608421718, -16.49499919880818766 ) ) ;
#86241 = CARTESIAN_POINT ( 'NONE',  ( 162.1853085131137675, 266.5774002991370821, 17.48035941305625940 ) ) ;
#86242 = ORIENTED_EDGE ( 'NONE', *, *, #4120, .F. ) ;
#86243 = CARTESIAN_POINT ( 'NONE',  ( 23.73796034364816521, 35.74646525600390845, 2.839279412974139660 ) ) ;
#86244 = CARTESIAN_POINT ( 'NONE',  ( 159.3169041484411537, 254.7020228407560580, 16.67170756419672628 ) ) ;
#86245 = CARTESIAN_POINT ( 'NONE',  ( 78.55537653917157570, 48.00561504237174404, -13.97647359956258484 ) ) ;
#86246 = CARTESIAN_POINT ( 'NONE',  ( 55.54680928425421627, 209.0024278399160949, 9.188101187500095079 ) ) ;
#86247 = CARTESIAN_POINT ( 'NONE',  ( 74.20995892610953604, 68.60058487300136676, 11.02733404855581867 ) ) ;
#86248 = CARTESIAN_POINT ( 'NONE',  ( 28.06847263831340555, 31.90829794293881960, 10.00000000000000355 ) ) ;
#86249 = CARTESIAN_POINT ( 'NONE',  ( 150.3470217762446737, 270.2383148473169854, 15.04338213197856078 ) ) ;
#86250 = CARTESIAN_POINT ( 'NONE',  ( 173.1064412035568409, 271.2423724309499562, 16.42374108768880347 ) ) ;
#86251 = EDGE_LOOP ( 'NONE', ( #2251, #88515, #26641, #51815, #89751, #33983, #24436, #57465, #92453, #47792, #4535, #76235, #86101, #61952, #3017, #45189, #36347, #34815, #39909, #4724, #54231 ) ) ;
#86252 = CARTESIAN_POINT ( 'NONE',  ( 86.58038954912636598, 46.32280579057140812, 9.040469064792965526 ) ) ;
#86253 = CARTESIAN_POINT ( 'NONE',  ( 84.47030363695364485, 42.96640489140571617, -4.988567256042748532 ) ) ;
#86254 = FACE_OUTER_BOUND ( 'NONE', #75985, .T. ) ;
#86255 = CARTESIAN_POINT ( 'NONE',  ( 77.75744084045382465, 52.33839962637683385, 16.14298180521786108 ) ) ;
#86256 = ORIENTED_EDGE ( 'NONE', *, *, #24228, .F. ) ;
#86257 = CARTESIAN_POINT ( 'NONE',  ( 172.1481527822565454, 258.6007877254482423, -14.00111594278938298 ) ) ;
#86258 = CARTESIAN_POINT ( 'NONE',  ( 157.0906402174166487, 259.4234253662278888, -17.15993715312605516 ) ) ;
#86259 = CARTESIAN_POINT ( 'NONE',  ( 161.6127771116929921, 250.7254542206800352, -12.96229604595372464 ) ) ;
#86260 = CARTESIAN_POINT ( 'NONE',  ( 192.5551423381268989, 297.1317055421444024, -13.20528585388119858 ) ) ;
#86262 = CARTESIAN_POINT ( 'NONE',  ( 149.5593209768671841, 271.6026526530012575, 11.55487339793564949 ) ) ;
#86261 = B_SPLINE_CURVE_WITH_KNOTS ( 'NONE', 3,
 ( #82521, #13083, #43943, #31237, #18437, #65513, #34613, #17938, #93071, #23625, #41709, #10829, #54519, #16046, #87892, #96462, #64526, #57406, #46948, #49327, #95483, #56413, #54026, #39322, #84981, #73140, #34131, #85497, #65024, #80266, #79769, #10334, #77865, #26035, #62123, #46428, #15527, #87408, #56906, #72653, #41200, #3248, #77353, #8451, #49818, #7960, #11349, #95970, #70238, #38834, #72138, #80777 ),
 .UNSPECIFIED., .F., .F.,
 ( 4, 2, 2, 2, 2, 2, 2, 2, 2, 2, 2, 2, 2, 2, 2, 2, 2, 2, 2, 2, 2, 2, 2, 2, 2, 4 ),
 ( 0.0003287865336021304915, 0.0007948713104775596231, 0.001027913698915235022, 0.001260956087352910204, 0.001377477281571752024, 0.001493998475790593626, 0.001610519670009435663, 0.001727040864228277482, 0.001960083252665935968, 0.002193125641103594453, 0.002659210417979031987, 0.003125295194854469955, 0.004057464748605345457, 0.004989634302356220526, 0.005455719079231613824, 0.005688761467669310040, 0.005805282661888203251, 0.005863543258997684117, 0.005921803856107164983, 0.005980064453216645849, 0.006038325050326125848, 0.006154846244545025130, 0.006387888632982837572, 0.006853973409858459855, 0.007320058186734081269, 0.007786142963609704419 ),
 .UNSPECIFIED. ) ;
#86263 = AXIS2_PLACEMENT_3D ( 'NONE', #63838, #69066, #70958 ) ;
#86264 = CARTESIAN_POINT ( 'NONE',  ( 40.00363105557123333, 187.2365022471902023, 10.00000000000009948 ) ) ;
#86265 = CARTESIAN_POINT ( 'NONE',  ( 164.2572333502590709, 246.1451216570909253, 2.155809084027023204 ) ) ;
#86266 = CARTESIAN_POINT ( 'NONE',  ( 67.62155312284794206, 66.73364273201507046, 8.622086810066367235 ) ) ;
#86267 = DIRECTION ( 'NONE',  ( 0.5000000000000048850, -0.8660254037844358210, 0.000000000000000000 ) ) ;
#86268 = LINE ( 'NONE', #2628, #86919 ) ;
#86269 = CARTESIAN_POINT ( 'NONE',  ( 112.6237299221286321, 226.6423013555409796, -4.594050593750043987 ) ) ;
#86270 = ORIENTED_EDGE ( 'NONE', *, *, #3737, .T. ) ;
#86271 = FACE_OUTER_BOUND ( 'NONE', #11482, .T. ) ;
#86272 = ADVANCED_FACE ( 'NONE', ( #7386 ), #84928, .T. ) ;
#86273 = CARTESIAN_POINT ( 'NONE',  ( 83.48755897335753673, 41.55649808380166377, -1.266732648212113288 ) ) ;
#86274 = EDGE_CURVE ( 'NONE', #95220, #1951, #61650, .T. ) ;
#86275 = CARTESIAN_POINT ( 'NONE',  ( 155.1865148098964937, 261.8560670301561686, -16.99758927948949605 ) ) ;
#86276 = CARTESIAN_POINT ( 'NONE',  ( 204.3371846825755824, 276.7246095846310823, 14.72513001683937262 ) ) ;
#86277 = CARTESIAN_POINT ( 'NONE',  ( 83.81305692926204642, 51.81190264249386956, -14.87427321595085417 ) ) ;
#86278 = CARTESIAN_POINT ( 'NONE',  ( 174.9266790960579954, 252.5411525110792184, 5.174313525909879807 ) ) ;
#86279 = ORIENTED_EDGE ( 'NONE', *, *, #52940, .F. ) ;
#86280 = CARTESIAN_POINT ( 'NONE',  ( 207.6875671281972870, 270.9215769640275653, -2.211577121115235300 ) ) ;
#86281 = CARTESIAN_POINT ( 'NONE',  ( 110.0000000000000000, -8.000000000000000000, 9.212605237762131694 ) ) ;
#86282 = DIRECTION ( 'NONE',  ( 1.000000000000000000, 0.000000000000000000, 0.000000000000000000 ) ) ;
#86283 = CARTESIAN_POINT ( 'NONE',  ( 74.59316757514828566, 66.97468268737705444, 12.54339389648529490 ) ) ;
#86284 = CARTESIAN_POINT ( 'NONE',  ( 132.1361044793229951, 247.0958772461660544, -9.188101187500095079 ) ) ;
#86285 = CARTESIAN_POINT ( 'NONE',  ( 198.9225589249066957, 286.1030165008847916, -17.03502353404871883 ) ) ;
#86286 = EDGE_CURVE ( 'NONE', #44968, #43056, #89281, .T. ) ;
#86287 = VECTOR ( 'NONE', #90588, 1000.000000000000114 ) ;
#86288 = CARTESIAN_POINT ( 'NONE',  ( 186.7776399068530395, 297.3129196693114977, 4.679761716601873012 ) ) ;
#86289 = CARTESIAN_POINT ( 'NONE',  ( 196.0355168007595523, 291.1035201434990540, 17.55377893960077884 ) ) ;
#86290 = DIRECTION ( 'NONE',  ( 0.7059494278973770243, -0.7082622432767159415, 0.000000000000000000 ) ) ;
#86291 = CARTESIAN_POINT ( 'NONE',  ( 52.62397354648171444, 207.3149278399161233, 9.188101187500093303 ) ) ;
#86292 = CARTESIAN_POINT ( 'NONE',  ( 85.39315930365103213, 48.29864428352725980, -11.77802199426026952 ) ) ;
#86293 = ORIENTED_EDGE ( 'NONE', *, *, #37502, .F. ) ;
#86294 = CARTESIAN_POINT ( 'NONE',  ( 70.78878230292833962, 62.60719215080742828, 13.74527488084627969 ) ) ;
#86295 = CARTESIAN_POINT ( 'NONE',  ( -32.04500338604974985, 25.44370296803430520, 10.00000000000000000 ) ) ;
#86296 = EDGE_CURVE ( 'NONE', #69987, #54157, #60576, .T. ) ;
#86297 = CARTESIAN_POINT ( 'NONE',  ( 80.07527276020931595, 44.25619389524629810, -11.41694498886655751 ) ) ;
#86298 = CARTESIAN_POINT ( 'NONE',  ( 171.2278541772891742, 259.7605199901955189, 15.25628007220308469 ) ) ;
#86299 = CARTESIAN_POINT ( 'NONE',  ( 151.2863714812464764, 278.3609153730897674, -1.671033152792061438 ) ) ;
#86300 = CARTESIAN_POINT ( 'NONE',  ( 155.6535436963908694, 261.0471492701456668, -17.87366571046205976 ) ) ;
#86301 = CARTESIAN_POINT ( 'NONE',  ( 153.9942695716630965, 269.2746656473301528, -15.26336082132222138 ) ) ;
#86302 = CARTESIAN_POINT ( 'NONE',  ( 116.4123307400877820, 248.0177522451419065, 5.000000000000046185 ) ) ;
#86303 = CARTESIAN_POINT ( 'NONE',  ( 69.81243019392553606, 62.22010195957141576, -13.63492759933605392 ) ) ;
#86304 = VERTEX_POINT ( 'NONE', #38275 ) ;
#86305 = CARTESIAN_POINT ( 'NONE',  ( 202.4900219881211854, 279.9239892212719383, 15.63116161057562259 ) ) ;
#86306 = CARTESIAN_POINT ( 'NONE',  ( -51.35363524361505227, 103.0449678370604687, -10.00000000000000000 ) ) ;
#86307 = CARTESIAN_POINT ( 'NONE',  ( 23.34166312890287998, 184.2833772461660544, -9.188101187500095079 ) ) ;
#86308 = CARTESIAN_POINT ( 'NONE',  ( 17.55409693860148579, 9.944730856513913864, 1.475505719884397138E-15 ) ) ;
#86309 = CARTESIAN_POINT ( 'NONE',  ( 188.9122134955663910, 290.7695941481946988, -15.11888497690123678 ) ) ;
#86310 = CARTESIAN_POINT ( 'NONE',  ( -31.49356256989596758, 94.88921800892812541, 45.19948692389422717 ) ) ;
#86311 = CARTESIAN_POINT ( 'NONE',  ( 72.27312669154171942, 72.08082049040204708, 3.221098087670088539 ) ) ;
#86313 = CARTESIAN_POINT ( 'NONE',  ( 56.72874666261028409, 196.8927522451418213, 10.00000000000009592 ) ) ;
#86312 = CARTESIAN_POINT ( 'NONE',  ( 8.974214183003985212, 13.38052372038638538, 10.00000000000000533 ) ) ;
#86314 = CARTESIAN_POINT ( 'NONE',  ( 8.129038565245441106, 16.64441083166258650, -10.00000000000000533 ) ) ;
#86315 = CARTESIAN_POINT ( 'NONE',  ( 182.1229068143135237, 256.9979893241743412, 1.317208241454887796 ) ) ;
#86316 = CARTESIAN_POINT ( 'NONE',  ( 157.0877926458200307, 258.5629572190321710, -17.40668770468195703 ) ) ;
#86317 = CARTESIAN_POINT ( 'NONE',  ( 162.2339947987030087, 251.8158834976649700, -12.96272347646762668 ) ) ;
#86318 = VERTEX_POINT ( 'NONE', #68684 ) ;
#86319 =( BOUNDED_CURVE ( )  B_SPLINE_CURVE ( 2, ( #99058, #29640, #61012, #7325, #44822, #91469, #84867, #54401, #60513 ),
 .UNSPECIFIED., .F., .T. ) 
 B_SPLINE_CURVE_WITH_KNOTS ( ( 3, 2, 2, 2, 3 ),
 ( 0.8185483870967742437, 0.8198924731182796188, 0.8225806451612903691, 0.8252688172043011194, 0.8266129032258064946 ),
 .UNSPECIFIED. ) 
 CURVE ( )  GEOMETRIC_REPRESENTATION_ITEM ( )  RATIONAL_B_SPLINE_CURVE ( ( 0.9330127018922194093, 0.9330127018922194093, 1.000000000000000000, 0.8660254037844387076, 1.000000000000000000, 0.8660254037844387076, 1.000000000000000000, 0.9330127018922194093, 0.9330127018922194093 ) ) 
 REPRESENTATION_ITEM ( '' )  );
#86320 = CARTESIAN_POINT ( 'NONE',  ( 19.14685258109593136, 191.8615022471903160, 5.000000000000046185 ) ) ;
#86321 = FACE_OUTER_BOUND ( 'NONE', #9484, .T. ) ;
#86322 = CARTESIAN_POINT ( 'NONE',  ( 208.3152833949211526, 269.8343404973242059, 2.763633873278860342 ) ) ;
#86323 = CARTESIAN_POINT ( 'NONE',  ( -18.01139699756907930, 172.6589784336661637, -6.496448406907675876E-16 ) ) ;
#86324 = CARTESIAN_POINT ( 'NONE',  ( 30.66313333631613247, 33.10171378149921395, 9.188101187500008038 ) ) ;
#86326 = CARTESIAN_POINT ( 'NONE',  ( 200.0499229738525457, 283.5835379334554887, 16.94138476260983239 ) ) ;
#86325 = CARTESIAN_POINT ( 'NONE',  ( 164.4515396538533309, 259.7753611418699506, -16.47110986934525556 ) ) ;
#86327 = CARTESIAN_POINT ( 'NONE',  ( 185.7051452101306381, 260.5437674537701014, 6.335629955934896529 ) ) ;
#86328 = CARTESIAN_POINT ( 'NONE',  ( 198.2505066714982149, 285.2670451491296149, 0.000000000000000000 ) ) ;
#86329 = CARTESIAN_POINT ( 'NONE',  ( 187.1546226255335625, 259.1615550454087042, -2.418851663009157882 ) ) ;
#86330 = CARTESIAN_POINT ( 'NONE',  ( 66.27754257038655794, 68.64336138396897979, 2.347787006359736139 ) ) ;
#86331 = ORIENTED_EDGE ( 'NONE', *, *, #29049, .T. ) ;
#86332 = CARTESIAN_POINT ( 'NONE',  ( 140.8234218128096131, 252.1115022471902591, 10.00000000000009592 ) ) ;
#86333 = SHAPE_REPRESENTATION_RELATIONSHIP ( 'NONE' , 'NONE' ,  #88422, #80385 ) ;
#86334 = CARTESIAN_POINT ( 'NONE',  ( 180.9635706913343824, 287.0861331774580094, 13.25109203236105060 ) ) ;
#86335 = CIRCLE ( 'NONE', #31239, 17.82106496071138935 ) ;
#86336 = CARTESIAN_POINT ( 'NONE',  ( 153.2920657472729715, 277.6580568772731112, -5.533179900162121356 ) ) ;
#86337 = CARTESIAN_POINT ( 'NONE',  ( 18.07869151248302941, 12.29860640527291338, -2.839279412974138328 ) ) ;
#86338 = CARTESIAN_POINT ( 'NONE',  ( 69.30415721694468800, 217.4865022471902876, -10.00000000000009592 ) ) ;
#86339 = EDGE_CURVE ( 'NONE', #55924, #3243, #52993, .T. ) ;
#86340 = CARTESIAN_POINT ( 'NONE',  ( 159.9894443651313338, 253.5371490153152081, -16.36035038356864391 ) ) ;
#86341 = AXIS2_PLACEMENT_3D ( 'NONE', #47360, #55445, #85417 ) ;
#86342 = LINE ( 'NONE', #96424, #35003 ) ;
#86343 = EDGE_CURVE ( 'NONE', #96192, #51310, #89250, .T. ) ;
#86345 = FACE_OUTER_BOUND ( 'NONE', #44550, .T. ) ;
#86344 =( BOUNDED_CURVE ( )  B_SPLINE_CURVE ( 2, ( #21702, #52587, #6509, #14606, #46478, #68291, #76419, #6991, #22706 ),
 .UNSPECIFIED., .F., .T. ) 
 B_SPLINE_CURVE_WITH_KNOTS ( ( 3, 2, 2, 2, 3 ),
 ( 0.7217741935483871218, 0.7231182795698924970, 0.7258064516129032473, 0.7284946236559139976, 0.7298387096774193727 ),
 .UNSPECIFIED. ) 
 CURVE ( )  GEOMETRIC_REPRESENTATION_ITEM ( )  RATIONAL_B_SPLINE_CURVE ( ( 0.9330127018922194093, 0.9330127018922194093, 1.000000000000000000, 0.8660254037844387076, 1.000000000000000000, 0.8660254037844387076, 1.000000000000000000, 0.9330127018922194093, 0.9330127018922194093 ) ) 
 REPRESENTATION_ITEM ( '' )  );
#86346 = LINE ( 'NONE', #61478, #19118 ) ;
#86347 = CARTESIAN_POINT ( 'NONE',  ( 71.94643353573425770, 71.53214566342799685, 5.625104812542567778 ) ) ;
#86348 = CARTESIAN_POINT ( 'NONE',  ( 163.4084407101100851, 247.6152736349200438, -10.68829614238923931 ) ) ;
#86349 = FACE_OUTER_BOUND ( 'NONE', #11911, .T. ) ;
#86350 = ORIENTED_EDGE ( 'NONE', *, *, #42979, .F. ) ;
#86351 = ORIENTED_EDGE ( 'NONE', *, *, #54968, .T. ) ;
#86352 = CARTESIAN_POINT ( 'NONE',  ( 157.2692844204907203, 277.2926557658657316, -9.947913950199314570 ) ) ;
#86353 = CIRCLE ( 'NONE', #65253, 0.1418229129680897982 ) ;
#86354 = CARTESIAN_POINT ( 'NONE',  ( 86.13128675074533191, 47.68336462356251815, 10.84980215260790182 ) ) ;
#86355 = EDGE_LOOP ( 'NONE', ( #19333, #99536, #86509, #48338 ) ) ;
#86356 = CARTESIAN_POINT ( 'NONE',  ( 70.51627874990606415, 69.09918821448661674, 8.581095468001166182 ) ) ;
#86357 = DIRECTION ( 'NONE',  ( 0.000000000000000000, 0.000000000000000000, 1.000000000000000000 ) ) ;
#86359 = EDGE_CURVE ( 'NONE', #56647, #44553, #97643, .T. ) ;
#86358 = VERTEX_POINT ( 'NONE', #83942 ) ;
#86360 = CARTESIAN_POINT ( 'NONE',  ( -22.42236680055709641, 157.8615022471902591, 0.000000000000000000 ) ) ;
#86361 = CARTESIAN_POINT ( 'NONE',  ( 41.47569090598248920, 209.1868197944957899, -18.47570218321542868 ) ) ;
#86362 = AXIS2_PLACEMENT_3D ( 'NONE', #22457, #53833, #53352 ) ;
#86363 = CARTESIAN_POINT ( 'NONE',  ( 14.21206617776240044, 23.90829794293879473, 10.00000000000000355 ) ) ;
#86364 = VERTEX_POINT ( 'NONE', #26104 ) ;
#86365 = CARTESIAN_POINT ( 'NONE',  ( 203.6224643629829529, 277.9625414913675172, 16.18209619002064414 ) ) ;
#86366 = CARTESIAN_POINT ( 'NONE',  ( 151.4281781455628675, 268.3656970847310390, 15.24742929158552585 ) ) ;
#86367 = CARTESIAN_POINT ( 'NONE',  ( 179.5196496019146650, 266.1175816663657656, 16.29367087753972498 ) ) ;
#86368 = B_SPLINE_SURFACE_WITH_KNOTS ( 'NONE', 3, 1, ( 
 ( #27721, #91046 ),
 ( #91535, #89562 ),
 ( #44886, #52007 ),
 ( #22099, #29702 ),
 ( #50996, #35304 ),
 ( #67707, #74339 ),
 ( #12525, #5415 ),
 ( #68191, #52493 ),
 ( #36795, #82950 ),
 ( #81452, #20620 ),
 ( #6413, #90048 ),
 ( #99120, #81947 ),
 ( #4408, #60579 ),
 ( #60083, #12024 ),
 ( #43396, #58589 ),
 ( #4928, #35807 ),
 ( #66701, #43895 ),
 ( #44391, #98634 ),
 ( #97636, #28201 ),
 ( #37294, #21130 ),
 ( #13523, #59077 ),
 ( #21613, #51504 ),
 ( #83441, #82471 ),
 ( #59585, #13033 ),
 ( #14008, #42880 ),
 ( #73816, #74835 ),
 ( #36298, #67201 ),
 ( #98123, #90561 ),
 ( #62573, #78312 ),
 ( #76796, #45872 ),
 ( #30704, #54987 ),
 ( #93021, #63091 ),
 ( #14985, #23577 ),
 ( #8400, #1306 ) ),
 .UNSPECIFIED., .T., .F., .F.,
 ( 4, 2, 2, 2, 2, 2, 2, 2, 2, 2, 2, 2, 2, 2, 2, 2, 4 ),
 ( 2, 2 ),
 ( 0.000000000000000000, 0.06250000000000000000, 0.1250000000000000000, 0.1875000000000000000, 0.2500000000000000000, 0.3125000000000000000, 0.3750000000000000000, 0.4375000000000000000, 0.5000000000000000000, 0.5625000000000000000, 0.6250000000000000000, 0.6875000000000000000, 0.7500000000000000000, 0.8125000000000000000, 0.8750000000000000000, 0.9375000000000000000, 1.000000000000000000 ),
 ( 0.000000000000000000, 1.000000000000000000 ),
 .UNSPECIFIED. ) ;
#86369 = VERTEX_POINT ( 'NONE', #78309 ) ;
#86370 = CARTESIAN_POINT ( 'NONE',  ( -37.33262083840143930, 163.6868197944959036, -37.49999999999995737 ) ) ;
#86371 = EDGE_CURVE ( 'NONE', #21644, #12155, #98736, .T. ) ;
#86372 = ORIENTED_EDGE ( 'NONE', *, *, #64947, .F. ) ;
#86373 = ADVANCED_FACE ( 'NONE', ( #94530 ), #55963, .T. ) ;
#86374 = ORIENTED_EDGE ( 'NONE', *, *, #11368, .F. ) ;
#86375 = CARTESIAN_POINT ( 'NONE',  ( 73.10630316137316242, 60.13848896484078210, 15.30670999211671024 ) ) ;
#86376 = VERTEX_POINT ( 'NONE', #9911 ) ;
#86377 = CARTESIAN_POINT ( 'NONE',  ( 67.34792581060418115, 67.11477767218006818, 7.860511789199255084 ) ) ;
#86378 = VERTEX_POINT ( 'NONE', #11912 ) ;
#86379 = CARTESIAN_POINT ( 'NONE',  ( 83.44125680345078422, 49.92309224034626425, 13.59759453135232299 ) ) ;
#86380 = CARTESIAN_POINT ( 'NONE',  ( 70.61396107802190159, 67.75272294984722521, 9.594151586959256406 ) ) ;
#86381 = CARTESIAN_POINT ( 'NONE',  ( 194.9455394410084921, 292.9914163096879065, -15.01116663483170655 ) ) ;
#86382 = LINE ( 'NONE', #78736, #9531 ) ;
#86383 = CYLINDRICAL_SURFACE ( 'NONE', #2998, 17.82106496071139645 ) ;
#86384 = LINE ( 'NONE', #226, #93298 ) ;
#86385 = CARTESIAN_POINT ( 'NONE',  ( 21.67811977205257890, 27.91421378149918553, 9.188101187500008038 ) ) ;
#86386 = CARTESIAN_POINT ( 'NONE',  ( 206.3505875407052486, 273.2372935382459787, 11.62318091048137880 ) ) ;
#86387 = FACE_OUTER_BOUND ( 'NONE', #80892, .T. ) ;
#86389 = ORIENTED_EDGE ( 'NONE', *, *, #37389, .F. ) ;
#86388 = CARTESIAN_POINT ( 'NONE',  ( 197.9002057575219453, 287.8737841300738296, 18.01270164875645818 ) ) ;
#86390 = CARTESIAN_POINT ( 'NONE',  ( 146.7742226592052361, 276.4265844432662220, -3.920976060369687932 ) ) ;
#86391 = EDGE_CURVE ( 'NONE', #77284, #53616, #11793, .T. ) ;
#86392 = DIRECTION ( 'NONE',  ( 0.8660254037844395958, 0.4999999999999985567, 0.000000000000000000 ) ) ;
#86393 = CARTESIAN_POINT ( 'NONE',  ( 159.2394649670193303, 254.8361514374751664, -16.43133403737800791 ) ) ;
#86394 = CARTESIAN_POINT ( 'NONE',  ( 27.88397166348279654, 69.57562948509108480, 59.99999999999999289 ) ) ;
#86395 = B_SPLINE_CURVE_WITH_KNOTS ( 'NONE', 3,
 ( #80457, #41901, #11529, #50008, #58101, #72840, #12018, #89083, #19632, #65207, #96148, #50492, #73807, #35298, #66210, #20118, #50989, #81939, #12517, #43389, #74332, #4920 ),
 .UNSPECIFIED., .F., .F.,
 ( 4, 2, 2, 2, 2, 2, 2, 2, 2, 2, 4 ),
 ( 0.005247342714528634502, 0.005571968392429927155, 0.005896594070331220676, 0.006221219748232513329, 0.006545845426133806849, 0.006870471104035099502, 0.007195096781936393023, 0.007844348137738960114, 0.009142850849344096031, 0.009792102205146660521, 0.01044135356094922501 ),
 .UNSPECIFIED. ) ;
#86396 = CARTESIAN_POINT ( 'NONE',  ( 137.2172943591538967, 238.4824982072973967, 3.021315404115420679E-15 ) ) ;
#86397 = CARTESIAN_POINT ( 'NONE',  ( 191.9661401536347114, 262.6107830541747035, -0.7521427156081436083 ) ) ;
#86399 = EDGE_CURVE ( 'NONE', #12659, #31705, #16606, .T. ) ;
#86398 = CARTESIAN_POINT ( 'NONE',  ( 193.8979767073725498, 294.8058481884610273, -15.36728096558731593 ) ) ;
#86400 = CYLINDRICAL_SURFACE ( 'NONE', #46301, 17.82106496071139645 ) ;
#86401 = CARTESIAN_POINT ( 'NONE',  ( 164.9586510554008782, 244.9302305544571823, -1.717556444319656039 ) ) ;
#86402 = CARTESIAN_POINT ( 'NONE',  ( 10.68506269473756909, 183.6427522451419634, -10.00000000000009415 ) ) ;
#86403 = CARTESIAN_POINT ( 'NONE',  ( 82.25819355828922141, 227.4869531367911293, 4.594050593750046652 ) ) ;
#86404 = B_SPLINE_CURVE_WITH_KNOTS ( 'NONE', 3,
 ( #7813, #38698, #61981, #92935 ),
 .UNSPECIFIED., .F., .F.,
 ( 4, 4 ),
 ( 0.01353903641422806066, 0.01992619949220648598 ),
 .UNSPECIFIED. ) ;
#86405 = CARTESIAN_POINT ( 'NONE',  ( 82.39390361753967795, 40.40531233075657980, -1.316817214398767089 ) ) ;
#86406 = ADVANCED_FACE ( 'NONE', ( #96043 ), #66986, .F. ) ;
#86407 = FACE_BOUND ( 'NONE', #34470, .T. ) ;
#86408 = CARTESIAN_POINT ( 'NONE',  ( 167.0544376998900589, 277.9796431053840138, -13.80256916416768931 ) ) ;
#86410 = CARTESIAN_POINT ( 'NONE',  ( 75.67360416972866233, 65.58707386806378281, 13.80094545836168685 ) ) ;
#86409 = CARTESIAN_POINT ( 'NONE',  ( 6.887527552763561545, 162.5327760586659736, 1.948934522072303157E-15 ) ) ;
#86411 = VECTOR ( 'NONE', #59729, 1000.000000000000114 ) ;
#86412 = ADVANCED_FACE ( 'NONE', ( #83320 ), #83822, .T. ) ;
#86413 = CARTESIAN_POINT ( 'NONE',  ( 161.3193951073452581, 251.2336067582368742, 13.01220207292984377 ) ) ;
#86414 = ORIENTED_EDGE ( 'NONE', *, *, #23905, .T. ) ;
#86415 = ORIENTED_EDGE ( 'NONE', *, *, #40532, .F. ) ;
#86416 = EDGE_CURVE ( 'NONE', #22170, #24654, #93991, .T. ) ;
#86417 = LINE ( 'NONE', #68914, #12874 ) ;
#86418 = CARTESIAN_POINT ( 'NONE',  ( 188.7890919132309762, 261.5044042730166893, -5.996600600795340519 ) ) ;
#86419 = CARTESIAN_POINT ( 'NONE',  ( 68.38173023771584269, 69.91662463375536163, 2.194006220653268890 ) ) ;
#86420 = CARTESIAN_POINT ( 'NONE',  ( -3.216670782107629911, 25.02209300385174373, -10.00000000000000000 ) ) ;
#86421 = VECTOR ( 'NONE', #87635, 1000.000000000000000 ) ;
#86422 = DIRECTION ( 'NONE',  ( -0.2126238682951524517, 0.9771341211068240717, 0.000000000000000000 ) ) ;
#86423 = CARTESIAN_POINT ( 'NONE',  ( 48.48788556946983874, 102.1758113618167982, -10.00000000000000000 ) ) ;
#86424 = CARTESIAN_POINT ( 'NONE',  ( 74.22019797964286170, 68.67351823779483766, -11.46693203622143820 ) ) ;
#86425 = CARTESIAN_POINT ( 'NONE',  ( 31.65035466828360100, 179.8923013555409796, 4.594050593750050204 ) ) ;
#86426 = CARTESIAN_POINT ( 'NONE',  ( 74.41009865654250177, 223.7677522451419350, -5.000000000000047962 ) ) ;
#86427 = CARTESIAN_POINT ( 'NONE',  ( 199.5527968932103704, 277.4168076600803374, 15.13942517218949213 ) ) ;
#86428 = VERTEX_POINT ( 'NONE', #37661 ) ;
#86429 = CARTESIAN_POINT ( 'NONE',  ( 26.50806851326365532, 196.1115022471903160, -5.000000000000047962 ) ) ;
#86430 = VECTOR ( 'NONE', #97280, 1000.000000000000000 ) ;
#86431 = DIRECTION ( 'NONE',  ( -0.8660254037844359321, -0.5000000000000051070, -0.000000000000000000 ) ) ;
#86432 = CARTESIAN_POINT ( 'NONE',  ( -16.14394294671762253, 170.6744531367911293, 4.594050593750047540 ) ) ;
#86433 = CARTESIAN_POINT ( 'NONE',  ( 195.7291850945597957, 291.6341022226063160, 17.08310330964873813 ) ) ;
#86434 = CARTESIAN_POINT ( 'NONE',  ( 155.5770330754656072, 261.1796695529068302, 18.26969263326161297 ) ) ;
#86435 = CARTESIAN_POINT ( 'NONE',  ( 179.4037581149374034, 257.9870511612666064, -10.76565914641300736 ) ) ;
#86436 = FACE_OUTER_BOUND ( 'NONE', #70320, .T. ) ;
#86437 = CARTESIAN_POINT ( 'NONE',  ( 147.9311236323648870, 274.4227731784279172, -7.799459659034405412 ) ) ;
#86438 = CARTESIAN_POINT ( 'NONE',  ( 189.4875514829830081, 262.4673988887644214, 8.218528321876050313 ) ) ;
#86439 = CARTESIAN_POINT ( 'NONE',  ( 204.7235752877335244, 276.0553614249301972, 14.82397698933823271 ) ) ;
#86440 = CARTESIAN_POINT ( 'NONE',  ( 192.5184197856564765, 265.2800136393148591, 8.105435529764278613 ) ) ;
#86441 = CARTESIAN_POINT ( 'NONE',  ( 146.5310397537613483, 276.8477895910274356, -0.2793038414862049068 ) ) ;
#86442 = CARTESIAN_POINT ( 'NONE',  ( 190.5674408456512765, 300.5745055173924811, -0.9151048603553563199 ) ) ;
#86443 = ORIENTED_EDGE ( 'NONE', *, *, #9515, .T. ) ;
#86444 = B_SPLINE_CURVE_WITH_KNOTS ( 'NONE', 3,
 ( #8480, #873, #7468, #31752 ),
 .UNSPECIFIED., .F., .F.,
 ( 4, 4 ),
 ( 0.01090216205137726352, 0.01663243029966742295 ),
 .UNSPECIFIED. ) ;
#86445 = CARTESIAN_POINT ( 'NONE',  ( 75.58214075417596689, 65.23491603964200181, 14.35294216029142333 ) ) ;
#86446 = CARTESIAN_POINT ( 'NONE',  ( 208.2175703429120688, 270.0035844679667889, 2.257951022351344150 ) ) ;
#86447 = CARTESIAN_POINT ( 'NONE',  ( 143.9908900580791169, 242.3932355074535394, -2.679491924311248496 ) ) ;
#86448 = CARTESIAN_POINT ( 'NONE',  ( 114.1121243109418799, 230.5643266524159856, -9.188101187500093303 ) ) ;
#86449 = CARTESIAN_POINT ( 'NONE',  ( 12.48623565965559479, 28.18502408145590721, 5.678558825948277544 ) ) ;
#86450 = CARTESIAN_POINT ( 'NONE',  ( -15.63054290230554955, 173.3297689869269504, -2.679491924311249385 ) ) ;
#86451 = DIRECTION ( 'NONE',  ( -0.9985601716053730259, 0.05364311403570636710, 0.000000000000000000 ) ) ;
#86453 = CARTESIAN_POINT ( 'NONE',  ( 191.7796050947615925, 276.9574050642111160, 17.17898019043861169 ) ) ;
#86452 = CARTESIAN_POINT ( 'NONE',  ( 176.9880447955025602, 255.7295297668954959, 9.707864002611934495 ) ) ;
#86454 = B_SPLINE_CURVE_WITH_KNOTS ( 'NONE', 3,
 ( #13583, #5971, #45454, #22675 ),
 .UNSPECIFIED., .F., .F.,
 ( 4, 4 ),
 ( 0.006529893551346395777, 0.01223971033066661822 ),
 .UNSPECIFIED. ) ;
#86455 = CARTESIAN_POINT ( 'NONE',  ( 190.9361477708944506, 299.9358863897686547, -8.027914178803371215 ) ) ;
#86456 = CARTESIAN_POINT ( 'NONE',  ( 189.6941666366152219, 261.1016796491359742, -4.547171728000958701 ) ) ;
#86457 = CARTESIAN_POINT ( 'NONE',  ( 149.2593905435863348, 272.1221474021800759, -12.98626158366800176 ) ) ;
#86458 = CARTESIAN_POINT ( 'NONE',  ( 91.02696109520442747, 213.3615022471902023, 5.000000000000051514 ) ) ;
#86459 = CARTESIAN_POINT ( 'NONE',  ( 175.3706562369355595, 291.2152232206044573, -1.076157994416038877 ) ) ;
#86460 = CARTESIAN_POINT ( 'NONE',  ( 85.85265132163429769, 47.44586991713102009, 10.77177032529229450 ) ) ;
#86461 = ORIENTED_EDGE ( 'NONE', *, *, #78353, .T. ) ;
#86462 = CARTESIAN_POINT ( 'NONE',  ( 131.5677753063154682, 256.7677522451419350, -5.000000000000047962 ) ) ;
#86463 = CARTESIAN_POINT ( 'NONE',  ( 30.79296800917359889, 109.3972131079642338, 59.99999999999999289 ) ) ;
#86464 = CARTESIAN_POINT ( 'NONE',  ( 200.5678471034125891, 269.1112160442550021, 9.133758541397122954 ) ) ;
#86465 = ORIENTED_EDGE ( 'NONE', *, *, #60812, .T. ) ;
#86466 = CARTESIAN_POINT ( 'NONE',  ( 71.97141114645215509, 72.59821799906346484, 1.534520970786815042 ) ) ;
#86467 = CARTESIAN_POINT ( 'NONE',  ( -23.56652710931154360, 99.64324603395651536, 45.19937630303415688 ) ) ;
#86468 = CARTESIAN_POINT ( 'NONE',  ( 39.80235952159635815, 84.99999999999998579, -10.00000000000000000 ) ) ;
#86469 = CYLINDRICAL_SURFACE ( 'NONE', #61439, 10.00000000000001066 ) ;
#86470 = CARTESIAN_POINT ( 'NONE',  ( 153.4477557824949940, 264.8676860077344486, 17.16010094972647693 ) ) ;
#86471 = EDGE_LOOP ( 'NONE', ( #81586, #37964, #52654, #53883 ) ) ;
#86472 = CARTESIAN_POINT ( 'NONE',  ( 191.1408708152463873, 280.4011667686116311, 16.85908246009275402 ) ) ;
#86473 = CARTESIAN_POINT ( 'NONE',  ( 41.71939737199939202, 29.80170272979930246, 7.433330006724137462 ) ) ;
#86474 = CARTESIAN_POINT ( 'NONE',  ( 72.84734729035820067, 70.28725029195504703, -8.119559778710620179 ) ) ;
#86475 = ORIENTED_EDGE ( 'NONE', *, *, #97239, .T. ) ;
#86476 = CARTESIAN_POINT ( 'NONE',  ( 166.4682810119589362, 280.3365465379465604, 11.69032492195255202 ) ) ;
#86477 = FACE_OUTER_BOUND ( 'NONE', #33668, .T. ) ;
#86478 = CARTESIAN_POINT ( 'NONE',  ( 85.03178579546401750, 43.95759251389035427, -7.567310116846363677 ) ) ;
#86480 = EDGE_CURVE ( 'NONE', #70676, #23520, #22965, .T. ) ;
#86479 = ORIENTED_EDGE ( 'NONE', *, *, #100231, .T. ) ;
#86481 = CARTESIAN_POINT ( 'NONE',  ( 86.17795171810620047, 46.97265431477908493, -10.08908967461300143 ) ) ;
#86482 = FACE_OUTER_BOUND ( 'NONE', #99035, .T. ) ;
#86483 = CARTESIAN_POINT ( 'NONE',  ( 204.8523313866422484, 275.8323493198358847, 14.65426965484541100 ) ) ;
#86484 = DIRECTION ( 'NONE',  ( -1.000000000000000000, 0.000000000000000000, -0.000000000000000000 ) ) ;
#86485 = CARTESIAN_POINT ( 'NONE',  ( 87.09656651665102345, 44.84278129179941885, -7.000152984404905965 ) ) ;
#86486 = CARTESIAN_POINT ( 'NONE',  ( 24.70930941448223450, 196.6199935810941213, 2.679491924311251605 ) ) ;
#86487 = VERTEX_POINT ( 'NONE', #29099 ) ;
#86488 = EDGE_CURVE ( 'NONE', #11929, #62608, #45511, .T. ) ;
#86489 = ORIENTED_EDGE ( 'NONE', *, *, #43812, .F. ) ;
#86490 = CARTESIAN_POINT ( 'NONE',  ( 162.7457592588995396, 249.1791651530724039, 10.37923698128102856 ) ) ;
#86491 = EDGE_CURVE ( 'NONE', #56024, #47030, #40823, .T. ) ;
#86492 = ORIENTED_EDGE ( 'NONE', *, *, #55939, .F. ) ;
#86493 = CARTESIAN_POINT ( 'NONE',  ( 77.14681100394483337, 49.55006509007303350, -14.96847495592216681 ) ) ;
#86494 = ORIENTED_EDGE ( 'NONE', *, *, #34864, .F. ) ;
#86495 = DIRECTION ( 'NONE',  ( -0.8660254037844387076, -0.4999999999999998890, -0.000000000000000000 ) ) ;
#86496 = CARTESIAN_POINT ( 'NONE',  ( 40.34888600819125060, 126.6204015641749834, -10.00000000000000000 ) ) ;
#86497 = ORIENTED_EDGE ( 'NONE', *, *, #72885, .T. ) ;
#86498 = CARTESIAN_POINT ( 'NONE',  ( 186.1746999497612762, 282.5091972200996224, -17.01259697921864245 ) ) ;
#86499 = CARTESIAN_POINT ( 'NONE',  ( 206.7156906810202770, 272.6049163492177740, -10.59685249612386571 ) ) ;
#86500 = CARTESIAN_POINT ( 'NONE',  ( 147.8139399455021135, 274.6257412778925300, -6.037782032743958638 ) ) ;
#86501 = CARTESIAN_POINT ( 'NONE',  ( 196.0478384692391671, 284.4236576599464001, -17.70377088038400615 ) ) ;
#86502 = DIRECTION ( 'NONE',  ( 0.4972609476841349796, -0.8612812260087746585, 0.1045284632676570652 ) ) ;
#86503 = CARTESIAN_POINT ( 'NONE',  ( 167.6519984660217517, 249.1525439965649298, -5.333742874422932267 ) ) ;
#86504 = CARTESIAN_POINT ( 'NONE',  ( 76.74023481339004604, 63.31925950119924096, -15.43993991125870124 ) ) ;
#86505 = VECTOR ( 'NONE', #59505, 1000.000000000000114 ) ;
#86506 = CARTESIAN_POINT ( 'NONE',  ( 157.9092491340927893, 281.1234455293418364, 2.649512146863262974 ) ) ;
#86507 = CARTESIAN_POINT ( 'NONE',  ( 128.5905526607566856, 254.2369531367911293, -4.594050593750048428 ) ) ;
#86508 = CARTESIAN_POINT ( 'NONE',  ( 186.6466061793297513, 262.7878478665138005, -9.097244108367178228 ) ) ;
#86509 = ORIENTED_EDGE ( 'NONE', *, *, #94019, .T. ) ;
#86511 = ORIENTED_EDGE ( 'NONE', *, *, #21292, .T. ) ;
#86510 = CARTESIAN_POINT ( 'NONE',  ( 85.70574795423719650, 48.48025216897318046, -12.24584271313005601 ) ) ;
#86512 = CARTESIAN_POINT ( 'NONE',  ( 200.6029011850095003, 274.3471715891406006, 13.46761961965223264 ) ) ;
#86513 = DIRECTION ( 'NONE',  ( 4.546899780356473057E-16, -0.000000000000000000, -1.000000000000000000 ) ) ;
#86514 = CARTESIAN_POINT ( 'NONE',  ( 174.3091936542869291, 290.3603755278153358, -4.810639208511179099 ) ) ;
#86515 = CARTESIAN_POINT ( 'NONE',  ( 147.0544566641476933, 275.9412049086974434, 4.176647824200751202 ) ) ;
#86516 = CARTESIAN_POINT ( 'NONE',  ( 72.99445915097255977, 65.45724384055469613, 12.87776796020878933 ) ) ;
#86517 = CARTESIAN_POINT ( 'NONE',  ( 77.93017357788673394, 184.0458036431182052, -21.50000000000000000 ) ) ;
#86518 = CARTESIAN_POINT ( 'NONE',  ( 79.17346404451581066, 56.03057509265897096, 16.54773837286879967 ) ) ;
#86519 = CARTESIAN_POINT ( 'NONE',  ( 174.9674570703506049, 282.3531941054687309, 14.48823916692557923 ) ) ;
#86520 = CARTESIAN_POINT ( 'NONE',  ( 43.63646518856938172, 66.22046553916848666, -10.00000000000000000 ) ) ;
#86521 = VERTEX_POINT ( 'NONE', #14869 ) ;
#86523 = ADVANCED_FACE ( 'NONE', ( #99498 ), #30078, .F. ) ;
#86522 = CARTESIAN_POINT ( 'NONE',  ( 194.3541845315608612, 294.0156730581561533, -14.67567721756631016 ) ) ;
#86524 = CARTESIAN_POINT ( 'NONE',  ( 151.8899205101083965, 272.8516340236540145, 11.76015270370216470 ) ) ;
#86525 = VERTEX_POINT ( 'NONE', #31063 ) ;
#86526 = CARTESIAN_POINT ( 'NONE',  ( 188.4443801593399144, 265.3218929820331482, -11.72523327534011806 ) ) ;
#86527 = EDGE_CURVE ( 'NONE', #7170, #57805, #75858, .T. ) ;
#86528 = CARTESIAN_POINT ( 'NONE',  ( 160.1932291396877588, 279.1613061217781819, 10.72099505396529473 ) ) ;
#86529 = CARTESIAN_POINT ( 'NONE',  ( 191.7401253710455364, 298.5433563381600948, -10.97067107967070143 ) ) ;
#86530 = LINE ( 'NONE', #94110, #44583 ) ;
#86531 = CARTESIAN_POINT ( 'NONE',  ( 87.74907107289486419, 44.16117455547063742, -4.521424286948807492 ) ) ;
#86533 = CARTESIAN_POINT ( 'NONE',  ( 153.2619048262327794, 276.0433244632241667, -8.635578536908909086 ) ) ;
#86532 = CARTESIAN_POINT ( 'NONE',  ( 161.4380241112732222, 281.4543506753062729, -6.652507061251734299 ) ) ;
#86534 = CARTESIAN_POINT ( 'NONE',  ( 200.2419102918539693, 267.3236120580114630, 6.328608526495528075 ) ) ;
#86535 = ORIENTED_EDGE ( 'NONE', *, *, #98017, .T. ) ;
#86536 = CARTESIAN_POINT ( 'NONE',  ( 204.8980137558721708, 272.5951782074533298, -9.440052061925650051 ) ) ;
#86537 = CARTESIAN_POINT ( 'NONE',  ( 186.8629439719893810, 262.8562446410389271, -9.020214349775766749 ) ) ;
#86538 = EDGE_CURVE ( 'NONE', #26620, #69871, #32721, .T. ) ;
#86539 = CARTESIAN_POINT ( 'NONE',  ( 190.4156752604778262, 274.6247770965693462, -15.68896343351512002 ) ) ;
#86540 = DIRECTION ( 'NONE',  ( -0.8660254037844359321, -0.5000000000000051070, -0.000000000000000000 ) ) ;
#86541 = CARTESIAN_POINT ( 'NONE',  ( 188.3939850883347162, 298.9566551310053342, -3.737861235791795522 ) ) ;
#86542 = CARTESIAN_POINT ( 'NONE',  ( 152.7618747630824885, 266.0556667813044101, 16.41480086888796919 ) ) ;
#86543 = CARTESIAN_POINT ( 'NONE',  ( -17.42236680055705023, 149.2012482093457777, 0.000000000000000000 ) ) ;
#86544 = CARTESIAN_POINT ( 'NONE',  ( 74.25054168435488577, 68.57848501580748746, 11.06803135282628325 ) ) ;
#86545 = CARTESIAN_POINT ( 'NONE',  ( 69.82525098749390224, 70.94647340042538985, -0.9569406247209537586 ) ) ;
#86546 = CARTESIAN_POINT ( 'NONE',  ( -11.38080322590321281, 173.4244531367911293, -4.594050593750046652 ) ) ;
#86547 = CARTESIAN_POINT ( 'NONE',  ( 85.37073267496330686, 220.0958772461660544, -9.188101187500095079 ) ) ;
#86548 = CARTESIAN_POINT ( 'NONE',  ( 155.5066938333533528, 261.3015006940112244, -18.40036130547566273 ) ) ;
#86549 = FACE_OUTER_BOUND ( 'NONE', #47171, .T. ) ;
#86550 = CARTESIAN_POINT ( 'NONE',  ( 147.7312888952508843, 275.3791301261515514, 3.813061375158469435 ) ) ;
#86551 = CARTESIAN_POINT ( 'NONE',  ( 202.9881971861223917, 279.0611244672630278, -15.16231470264511927 ) ) ;
#86552 = DIRECTION ( 'NONE',  ( 0.4999999999999992784, -0.8660254037844390407, 0.000000000000000000 ) ) ;
#86553 = CARTESIAN_POINT ( 'NONE',  ( 84.83525364562130733, 49.93448604028102267, -13.18857086666493217 ) ) ;
#86554 = CARTESIAN_POINT ( 'NONE',  ( 77.87908970151455890, 62.02332377074587555, 15.65384233240896350 ) ) ;
#86556 = CARTESIAN_POINT ( 'NONE',  ( 76.42510427590111988, 51.13649333467196811, 16.04694757192931931 ) ) ;
#86555 = CARTESIAN_POINT ( 'NONE',  ( 190.3036138866188196, 300.4162036267649682, -1.111846361930479254 ) ) ;
#86557 = CARTESIAN_POINT ( 'NONE',  ( 162.0307665587793338, 250.0014752612991913, 13.21085648779418698 ) ) ;
#86558 = CARTESIAN_POINT ( 'NONE',  ( 169.3360775606673485, 252.0299813709655439, -9.733642257039461398 ) ) ;
#86559 = CARTESIAN_POINT ( 'NONE',  ( 157.6286460899086137, 257.6261715744221306, 18.25526781158026779 ) ) ;
#86560 = CARTESIAN_POINT ( 'NONE',  ( 71.77313022743312843, 71.85913065286145240, 2.952583973247177251 ) ) ;
#86561 = COLOUR_RGB ( '',0.7921568627450980005, 0.8196078431372548767, 0.9333333333333333481 ) ;
#86562 = CARTESIAN_POINT ( 'NONE',  ( 161.5083988044524119, 250.9062427520286178, -14.53522982831775856 ) ) ;
#86563 = CARTESIAN_POINT ( 'NONE',  ( 36.49425040099653472, 198.0024278399160949, -9.188101187500093303 ) ) ;
#86564 = EDGE_CURVE ( 'NONE', #74259, #57797, #66144, .T. ) ;
#86565 = CARTESIAN_POINT ( 'NONE',  ( 62.47501251452968773, 213.0024278399160949, -9.188101187500093303 ) ) ;
#86566 = CARTESIAN_POINT ( 'NONE',  ( -29.48056340892364346, 35.96025339996432280, 59.99999999999999289 ) ) ;
#86568 = CARTESIAN_POINT ( 'NONE',  ( 88.33060278926279807, 43.77373715677852317, 0.1867717842524379002 ) ) ;
#86567 = AXIS2_PLACEMENT_3D ( 'NONE', #34451, #49161, #88713 ) ;
#86570 = FACE_OUTER_BOUND ( 'NONE', #51464, .T. ) ;
#86569 = CARTESIAN_POINT ( 'NONE',  ( 182.0338464029501040, 278.3680066549227945, 17.69288446120480174 ) ) ;
#86571 = CARTESIAN_POINT ( 'NONE',  ( 196.2376815664581500, 269.5000789340413689, -10.77412858023367370 ) ) ;
#86572 = CARTESIAN_POINT ( 'NONE',  ( 24.17276070933917609, 32.14336893147756768, 7.433330006724141015 ) ) ;
#86573 = CARTESIAN_POINT ( 'NONE',  ( 151.0388915836658725, 269.0399611886400635, -14.24896787280406585 ) ) ;
#86574 = CARTESIAN_POINT ( 'NONE',  ( 80.57150847499261204, 47.56777207323567325, -13.10156609182119958 ) ) ;
#86575 = CARTESIAN_POINT ( 'NONE',  ( 11.93836421708519779, 28.93396525600389069, 2.839279412974139660 ) ) ;
#86576 = CARTESIAN_POINT ( 'NONE',  ( 66.15596757637857195, 202.8768266524160140, 9.188101187500096856 ) ) ;
#86577 = CARTESIAN_POINT ( 'NONE',  ( 48.29091023345864642, 82.53782597618220507, -10.00000000000000000 ) ) ;
#86578 = DIRECTION ( 'NONE',  ( -0.5000000000000016653, 0.8660254037844377084, 0.000000000000000000 ) ) ;
#86579 = CARTESIAN_POINT ( 'NONE',  ( 197.9002057575219453, 287.8737841300738296, 18.01270164875645818 ) ) ;
#86580 = PLANE ( 'NONE',  #23151 ) ;
#86581 = CARTESIAN_POINT ( 'NONE',  ( 154.0911303478728769, 263.7533285722025767, 17.04017818173372945 ) ) ;
#86582 = B_SPLINE_CURVE_WITH_KNOTS ( 'NONE', 3,
 ( #32153, #63060, #94003, #92987, #47838, #54432, #63558, #94497, #85407, #2283, #18988, #95528, #19499, #11879, #96504, #49858, #66060, #97010, #48876, #17982, #64065, #81308, #26073, #10874, #40742, #79811, #65062, #10375, #87449, #50848, #88428, #87935, #49364, #4253, #27578, #34170, #88939, #42735, #50353, #80824, #96012, #80308, #41752, #41245, #11393, #71687, #65556, #73672 ),
 .UNSPECIFIED., .F., .F.,
 ( 4, 2, 2, 2, 2, 2, 2, 2, 2, 2, 2, 2, 2, 2, 2, 2, 2, 2, 2, 2, 2, 2, 2, 4 ),
 ( 0.0004679476576457052245, 0.0009134075131973231568, 0.001136137440973158334, 0.001247502404861099016, 0.001358867368749039697, 0.001470232332636980379, 0.001581597296524921061, 0.001804327224300763394, 0.002249787079852291066, 0.003140706790955346411, 0.004031626502058401756, 0.004922546213161457102, 0.005368006068713020336, 0.005590735996488724324, 0.005702100960376499557, 0.005757783442320386739, 0.005813465924264273922, 0.005869148406208161972, 0.005924830888152049155, 0.006036195852039825255, 0.006258925779815422558, 0.006704385635366572060, 0.007149845490917722431, 0.007595305346468871933 ),
 .UNSPECIFIED. ) ;
#86583 = CARTESIAN_POINT ( 'NONE',  ( 193.7599675174199660, 288.1895609423694964, 16.30602659942787369 ) ) ;
#86584 = CARTESIAN_POINT ( 'NONE',  ( 87.58100233665301459, 44.90480556695516867, -6.571228966301012164 ) ) ;
#86585 = CARTESIAN_POINT ( 'NONE',  ( 109.6465072765698210, 234.1115022471902307, 10.00000000000009592 ) ) ;
#86586 = DIRECTION ( 'NONE',  ( -1.000000000000000000, 0.000000000000000000, 0.000000000000000000 ) ) ;
#86587 = CARTESIAN_POINT ( 'NONE',  ( 207.2824254892180704, 271.6233028670009162, 6.274396967990798046 ) ) ;
#86588 = VERTEX_POINT ( 'NONE', #77698 ) ;
#86589 = CARTESIAN_POINT ( 'NONE',  ( 86.10640163849959094, 46.41140333115836114, 9.428975133176919599 ) ) ;
#86590 = CARTESIAN_POINT ( 'NONE',  ( 184.6787335681921718, 271.1592666014827842, 16.29185237002324982 ) ) ;
#86591 = ORIENTED_EDGE ( 'NONE', *, *, #40211, .T. ) ;
#86592 = CARTESIAN_POINT ( 'NONE',  ( 206.8313602288537538, 272.4045708154811791, -9.607337080360906612 ) ) ;
#86593 = DIRECTION ( 'NONE',  ( 0.4493970231495826861, -0.7783784768652872721, -0.4383711467890751834 ) ) ;
#86594 = CARTESIAN_POINT ( 'NONE',  ( 73.16639139570222028, 68.70606694088236566, -10.26624930846365125 ) ) ;
#86595 = EDGE_LOOP ( 'NONE', ( #49358, #26917, #91607, #52891 ) ) ;
#86596 = CARTESIAN_POINT ( 'NONE',  ( 176.9944672240674777, 253.3095680353166870, -0.2591140802082422812 ) ) ;
#86598 = ORIENTED_EDGE ( 'NONE', *, *, #1768, .F. ) ;
#86597 = B_SPLINE_CURVE_WITH_KNOTS ( 'NONE', 3,
 ( #23612, #92575, #83481, #6932, #61120, #75872, #6450, #68230, #99153, #29741, #79881, #9949, #71756, #32229, #79385, #24135, #70732, #87516, #86002, #87002, #57021, #8934, #40810, #63131, #46933, #32728, #2351, #18049, #70224, #39306, #40314, #94075, #33231, #55021, #1343, #48944, #16528, #17530, #16032, #24627, #93567, #55508, #77850, #63632, #64135, #10443 ),
 .UNSPECIFIED., .F., .F.,
 ( 4, 1, 2, 2, 1, 2, 2, 1, 1, 2, 2, 1, 1, 2, 2, 1, 1, 2, 2, 1, 1, 1, 2, 2, 1, 1, 1, 2, 2, 4 ),
 ( 0.000000000000000000, 0.06250000000000156819, 0.09375000000000216493, 0.1250000000000027756, 0.1875000000000044131, 0.2187500000000063283, 0.2500000000000082157, 0.3125000000000114908, 0.3437500000000141553, 0.3593750000000145439, 0.3750000000000149880, 0.4375000000000159317, 0.4687500000000164868, 0.4843750000000155431, 0.5000000000000145439, 0.5625000000000082157, 0.5937500000000061062, 0.6093750000000054401, 0.6250000000000046629, 0.6875000000000074385, 0.7187500000000093259, 0.7343750000000107692, 0.7421875000000118794, 0.7500000000000128786, 0.8125000000000160982, 0.8437500000000163203, 0.8593750000000163203, 0.8671875000000154321, 0.8750000000000145439, 1.000000000000000000 ),
 .UNSPECIFIED. ) ;
#86599 = CYLINDRICAL_SURFACE ( 'NONE', #89545, 10.00000000000001066 ) ;
#86600 = CARTESIAN_POINT ( 'NONE',  ( 51.48077938449444702, 188.9824982072973967, 3.021315404115420679E-15 ) ) ;
#86601 = CARTESIAN_POINT ( 'NONE',  ( 206.8532690132467451, 270.9563895460929643, -5.334349829856665615 ) ) ;
#86602 = ORIENTED_EDGE ( 'NONE', *, *, #61268, .T. ) ;
#86603 = AXIS2_PLACEMENT_3D ( 'NONE', #99629, #8903, #53984 ) ;
#86604 = CARTESIAN_POINT ( 'NONE',  ( 29.50362127723248662, 19.96004757982091604, -5.678558825948275768 ) ) ;
#86605 = CARTESIAN_POINT ( 'NONE',  ( 75.27101761674283864, 66.49390254752692897, -13.13272271682535930 ) ) ;
#86606 = CARTESIAN_POINT ( 'NONE',  ( 74.14312167556930433, 66.30466486950707861, 1.224646799147354045E-15 ) ) ;
#86607 = ORIENTED_EDGE ( 'NONE', *, *, #94761, .T. ) ;
#86609 = EDGE_CURVE ( 'NONE', #30332, #39213, #94413, .T. ) ;
#86608 = CARTESIAN_POINT ( 'NONE',  ( -62.95439910331221256, 68.06504152958493137, 60.00000000000000000 ) ) ;
#86610 = CARTESIAN_POINT ( 'NONE',  ( 206.3423291502491566, 273.2515974901050413, -10.76717883871977577 ) ) ;
#86611 = ADVANCED_FACE ( 'NONE', ( #2694 ), #71097, .T. ) ;
#86612 = ORIENTED_EDGE ( 'NONE', *, *, #54579, .T. ) ;
#86613 = CARTESIAN_POINT ( 'NONE',  ( 183.7135354246354666, 296.1227231308993169, 1.015274712648644106 ) ) ;
#86615 = CARTESIAN_POINT ( 'NONE',  ( 194.4826705584825390, 293.7931287314651740, -16.11258321617245315 ) ) ;
#86614 = CARTESIAN_POINT ( 'NONE',  ( 162.6361072964105006, 284.9137001060370835, -2.721021406022150479 ) ) ;
#86616 = CARTESIAN_POINT ( 'NONE',  ( 170.6178593158246315, 266.5408558992322696, -17.65857870869936974 ) ) ;
#86617 = CARTESIAN_POINT ( 'NONE',  ( 155.3738696901333469, 261.5315588585399951, 17.02116401938635804 ) ) ;
#86618 = CARTESIAN_POINT ( 'NONE',  ( 185.8238740079479214, 292.8821648394323915, -10.72204040993758234 ) ) ;
#86619 = CARTESIAN_POINT ( 'NONE',  ( 205.3943609285979051, 274.8935266139653777, -13.14270440534009943 ) ) ;
#86620 = CARTESIAN_POINT ( 'NONE',  ( 144.0260350180681712, 257.5444598644534153, -9.188101187500093303 ) ) ;
#86621 = CARTESIAN_POINT ( 'NONE',  ( 70.79942557690317528, 62.94285302112024993, -14.11492782255271017 ) ) ;
#86622 = CARTESIAN_POINT ( 'NONE',  ( 39.77289032284285497, 58.49985355908045648, -10.00000000000000000 ) ) ;
#86623 = CARTESIAN_POINT ( 'NONE',  ( 82.77265646360999085, 218.5958772461660544, -9.188101187500095079 ) ) ;
#86624 = ORIENTED_EDGE ( 'NONE', *, *, #38296, .F. ) ;
#86625 = CARTESIAN_POINT ( 'NONE',  ( 150.8888667059421209, 269.2998118992572927, 15.79021133717968617 ) ) ;
#86626 = CARTESIAN_POINT ( 'NONE',  ( 78.01756760496483878, 61.41364688087467272, -16.16017056289257425 ) ) ;
#86627 = ORIENTED_EDGE ( 'NONE', *, *, #89267, .T. ) ;
#86628 = CARTESIAN_POINT ( 'NONE',  ( 157.4810658944377906, 257.8817879711681940, -17.75031495925077962 ) ) ;
#86629 = ORIENTED_EDGE ( 'NONE', *, *, #44612, .T. ) ;
#86630 = FACE_OUTER_BOUND ( 'NONE', #39815, .T. ) ;
#86631 = CARTESIAN_POINT ( 'NONE',  ( 84.11911179316838627, 207.8262482093457777, 3.021315404115420679E-15 ) ) ;
#86632 = CARTESIAN_POINT ( 'NONE',  ( 146.5689048584090699, 276.7822053059436485, -0.4306668706573002492 ) ) ;
#86633 = CARTESIAN_POINT ( 'NONE',  ( 85.36737598551003714, 42.56170592440086153, 0.09984784679323620293 ) ) ;
#86634 = CARTESIAN_POINT ( 'NONE',  ( 86.12135434523638366, 46.98046262810483142, -10.13131473785488090 ) ) ;
#86635 = CARTESIAN_POINT ( 'NONE',  ( 162.7896496350696225, 248.6870512161599436, 11.81710663537990946 ) ) ;
#86636 = CARTESIAN_POINT ( 'NONE',  ( 82.06918437091763963, 212.0643266524160140, 9.188101187500095079 ) ) ;
#86637 = ORIENTED_EDGE ( 'NONE', *, *, #20531, .F. ) ;
#86638 = AXIS2_PLACEMENT_3D ( 'NONE', #72873, #81975, #58132 ) ;
#86639 = ORIENTED_EDGE ( 'NONE', *, *, #25039, .T. ) ;
#86640 = ADVANCED_FACE ( 'NONE', ( #64480 ), #79227, .T. ) ;
#86641 = CARTESIAN_POINT ( 'NONE',  ( 124.2269133023873025, 230.9824982072973683, 3.021315404115420679E-15 ) ) ;
#86642 = B_SPLINE_SURFACE_WITH_KNOTS ( 'NONE', 3, 1, ( 
 ( #42746, #96513 ),
 ( #57966, #73680 ),
 ( #41254, #22327 ),
 ( #68917, #38004 ),
 ( #8135, #92759 ),
 ( #38513, #90787 ),
 ( #99348, #53227 ),
 ( #69425, #46613 ),
 ( #45123, #14728 ),
 ( #30924, #23313 ),
 ( #39008, #45609 ),
 ( #28944, #59821 ),
 ( #77545, #29432 ),
 ( #84665, #99842 ),
 ( #97019, #38 ),
 ( #91761, #21338 ),
 ( #83673, #6130 ),
 ( #76541, #6639 ),
 ( #30426, #67935 ),
 ( #37026, #13731 ),
 ( #61809, #76060 ),
 ( #52715, #53708 ),
 ( #61315, #37514 ),
 ( #68421, #91265 ),
 ( #29927, #60802 ),
 ( #7119, #14237 ),
 ( #54200, #85168 ),
 ( #92278, #52223 ),
 ( #98856, #22825 ),
 ( #60308, #84179 ),
 ( #15208, #46103 ) ),
 .UNSPECIFIED., .F., .F., .F.,
 ( 4, 3, 3, 3, 3, 3, 3, 3, 3, 3, 4 ),
 ( 2, 2 ),
 ( 0.000000000000000000, 0.1333490885032285189, 0.3007194338854188853, 0.4699862290244924967, 0.5844252810809184018, 0.6686540514502693489, 0.7354980260655538116, 0.8028463152565737948, 0.8633854507757268149, 0.9437142632667515629, 1.000000000000000000 ),
 ( 0.000000000000000000, 1.000000000000000000 ),
 .UNSPECIFIED. ) ;
#86643 = CARTESIAN_POINT ( 'NONE',  ( 163.4139553296302267, 247.6057220337265505, -10.31482883765270842 ) ) ;
#86644 = ORIENTED_EDGE ( 'NONE', *, *, #73514, .F. ) ;
#86645 = AXIS2_PLACEMENT_3D ( 'NONE', #69188, #61081, #68685 ) ;
#86646 = CARTESIAN_POINT ( 'NONE',  ( 75.75917444283010127, 65.12044684595205979, -14.46054081031674876 ) ) ;
#86647 = CARTESIAN_POINT ( 'NONE',  ( 164.3400821678858392, 284.7095078879949028, 0.5037811400987294297 ) ) ;
#86648 = CARTESIAN_POINT ( 'NONE',  ( 47.92671612011950799, 80.40884667711614497, -10.00000000000000000 ) ) ;
#86649 = CARTESIAN_POINT ( 'NONE',  ( 87.84403297180379866, 44.29423158952226203, 4.754374079557551980 ) ) ;
#86650 = ORIENTED_EDGE ( 'NONE', *, *, #50936, .T. ) ;
#86651 = CARTESIAN_POINT ( 'NONE',  ( 83.03297025961435907, 43.66274663663242706, -7.959272922208247003 ) ) ;
#86652 = CARTESIAN_POINT ( 'NONE',  ( 186.0084645542806072, 259.0743807822461804, 6.274839502105399980 ) ) ;
#86653 = CARTESIAN_POINT ( 'NONE',  ( 159.2289198208967775, 254.8544161663325838, -15.88961297684315888 ) ) ;
#86654 = CARTESIAN_POINT ( 'NONE',  ( 147.7917198021585534, 275.6304213403500398, -3.790807063116589770 ) ) ;
#86655 = DIRECTION ( 'NONE',  ( 1.000000000000000000, 0.000000000000000000, 0.000000000000000000 ) ) ;
#86656 = CARTESIAN_POINT ( 'NONE',  ( 198.8472775862647666, 285.8620616674365920, -17.00592469681938823 ) ) ;
#86657 = CARTESIAN_POINT ( 'NONE',  ( 76.61888230025124358, 51.35972145274619294, 16.07233720520855158 ) ) ;
#86658 = VERTEX_POINT ( 'NONE', #2194 ) ;
#86659 = CARTESIAN_POINT ( 'NONE',  ( 203.4594108534527095, 277.8640620765348785, -14.42658014575316550 ) ) ;
#86660 = CARTESIAN_POINT ( 'NONE',  ( 200.4592688079413847, 283.4413569069752725, 18.39277739746426832 ) ) ;
#86661 = CARTESIAN_POINT ( 'NONE',  ( 85.85494225371405719, 44.84660830416275701, 7.405870140133522739 ) ) ;
#86662 = CARTESIAN_POINT ( 'NONE',  ( 187.8939482297251686, 266.1432077329668573, -11.85658473688042136 ) ) ;
#86663 = CARTESIAN_POINT ( 'NONE',  ( 83.98894966577088894, 51.79070771454841093, 14.82098776213804570 ) ) ;
#86664 = CARTESIAN_POINT ( 'NONE',  ( 175.6661633239287994, 291.2999147521263126, -6.611607887066273115 ) ) ;
#86665 = CARTESIAN_POINT ( 'NONE',  ( 156.6090548319399431, 272.6926376298130208, 14.76279018684578759 ) ) ;
#86666 = ORIENTED_EDGE ( 'NONE', *, *, #65844, .T. ) ;
#86667 = EDGE_CURVE ( 'NONE', #82593, #27025, #23967, .T. ) ;
#86668 = CARTESIAN_POINT ( 'NONE',  ( 72.77272354753068839, 64.36932843330238541, -13.45330500611205338 ) ) ;
#86670 = FACE_OUTER_BOUND ( 'NONE', #57174, .T. ) ;
#86669 = CARTESIAN_POINT ( 'NONE',  ( 180.5624607037953808, 267.1083404837390276, -14.97454804253810146 ) ) ;
#86671 = CARTESIAN_POINT ( 'NONE',  ( 176.1878285045740711, 285.1602639758941677, -12.77100825351733349 ) ) ;
#86672 = B_SPLINE_CURVE_WITH_KNOTS ( 'NONE', 3,
 ( #8722, #68518, #60401, #99440, #31504, #45702, #31012, #39593, #45215, #92363, #61902, #54811, #7718, #62399, #76154, #47212, #92852, #23405, #85264, #91865, #6729, #91357, #15809, #7212, #21921, #85788, #46714, #77642, #16320, #22910, #38096, #76626, #53797, #14815, #84760, #8226, #83766, #39095, #37606, #52809, #38610, #30017, #70008, #22422, #53313, #84269, #77113, #69007, #99937, #15297, #46197, #72549 ),
 .UNSPECIFIED., .F., .F.,
 ( 4, 2, 2, 2, 2, 2, 2, 2, 2, 2, 2, 2, 2, 2, 2, 2, 2, 2, 2, 2, 2, 2, 2, 2, 2, 4 ),
 ( 0.0001379551026079702870, 0.001154483995626299489, 0.001408616218880838055, 0.001662748442135376838, 0.001789814553762667480, 0.001916880665389957689, 0.002043946777017248331, 0.002171012888644538973, 0.002425145111899041327, 0.002679277335153543247, 0.003187541781662507623, 0.004204070674680569081, 0.005220599567698630539, 0.005728864014207661268, 0.005982996237462099437, 0.006110062349089359288, 0.006237128460716620006, 0.006300661516530249931, 0.006364194572343878989, 0.006491260683971138840, 0.006745392907225655939, 0.007253657353734690137, 0.007507789576989207236, 0.007761921800243724336, 0.008016054023498243170, 0.008270186246752759401 ),
 .UNSPECIFIED. ) ;
#86673 = CARTESIAN_POINT ( 'NONE',  ( 35.46999748293995225, 20.28848085856233396, 1.475505719884397138E-15 ) ) ;
#86674 = CARTESIAN_POINT ( 'NONE',  ( -34.42581292930597670, 25.91608375674935161, -10.00000000000000000 ) ) ;
#86675 = CARTESIAN_POINT ( 'NONE',  ( 179.7803990077309777, 275.4327082817983978, -17.81061729480618183 ) ) ;
#86676 = CARTESIAN_POINT ( 'NONE',  ( 192.2502979002084658, 262.0516754426723764, 3.027840789192269177 ) ) ;
#86677 = DIRECTION ( 'NONE',  ( 0.000000000000000000, 0.000000000000000000, 1.000000000000000000 ) ) ;
#86678 = B_SPLINE_CURVE_WITH_KNOTS ( 'NONE', 3,
 ( #9659, #40518, #71453, #41523 ),
 .UNSPECIFIED., .F., .F.,
 ( 4, 4 ),
 ( 0.01371562546018176634, 0.02009222533191522969 ),
 .UNSPECIFIED. ) ;
#86679 = CARTESIAN_POINT ( 'NONE',  ( -2.098180203030011182, 181.8464784336661353, 1.353441290958777327E-15 ) ) ;
#86680 = CARTESIAN_POINT ( 'NONE',  ( 81.84495297315717721, 46.76928670720106851, 12.06671785398880203 ) ) ;
#86681 = ORIENTED_EDGE ( 'NONE', *, *, #12845, .F. ) ;
#86682 = CARTESIAN_POINT ( 'NONE',  ( 175.7615011029471646, 255.7341681394030957, 8.240769549146955697 ) ) ;
#86683 = DIRECTION ( 'NONE',  ( 0.5000000000000001110, -0.8660254037844384856, -0.000000000000000000 ) ) ;
#86684 = DIRECTION ( 'NONE',  ( -0.4055404667435467125, 0.9140770918436946779, 0.000000000000000000 ) ) ;
#86685 = CARTESIAN_POINT ( 'NONE',  ( 22.50244069716294959, 192.9869531367911293, 4.594050593750046652 ) ) ;
#86686 = CARTESIAN_POINT ( 'NONE',  ( 58.10966550219803395, 178.3759306620403891, -17.47570218321534696 ) ) ;
#86687 = CARTESIAN_POINT ( 'NONE',  ( 37.50785463075374793, 23.78380873178790011, -6.180339887498949025 ) ) ;
#86688 = CARTESIAN_POINT ( 'NONE',  ( 178.3194579432817193, 291.9759310783170463, 5.627940545170020847 ) ) ;
#86689 = DIRECTION ( 'NONE',  ( -0.7715546603183375263, -0.6361630342459821952, 0.000000000000000000 ) ) ;
#86690 = AXIS2_PLACEMENT_3D ( 'NONE', #84215, #76572, #14762 ) ;
#86691 = CARTESIAN_POINT ( 'NONE',  ( 81.64869726432758057, 55.83996916651700815, 16.01049500238219636 ) ) ;
#86692 = CARTESIAN_POINT ( 'NONE',  ( 174.3697573357644899, 277.1653490889620457, -17.12727634137145571 ) ) ;
#86693 = CARTESIAN_POINT ( 'NONE',  ( 188.5128844555716796, 297.0448699536724462, -7.768193810651193409 ) ) ;
#86694 = CARTESIAN_POINT ( 'NONE',  ( 90.23310447506868570, 216.2365022471901739, -10.00000000000009237 ) ) ;
#86695 = AXIS2_PLACEMENT_3D ( 'NONE', #66248, #59110, #36329 ) ;
#86696 = CARTESIAN_POINT ( 'NONE',  ( 66.77824978924009258, 209.3615022471902591, -10.00000000000009592 ) ) ;
#86697 = CARTESIAN_POINT ( 'NONE',  ( 67.68514482100736984, 66.83340866827894899, -8.536435324610977204 ) ) ;
#86698 = CARTESIAN_POINT ( 'NONE',  ( 185.6563202890208970, 277.8056579403244086, -17.21583835310515553 ) ) ;
#86699 = CARTESIAN_POINT ( 'NONE',  ( 203.3753004216920885, 270.0891535218205490, 6.082445786454247383 ) ) ;
#86700 = CARTESIAN_POINT ( 'NONE',  ( 33.40920844789697952, 190.0958772461660544, -9.188101187500095079 ) ) ;
#86701 = CARTESIAN_POINT ( 'NONE',  ( 191.7788397968654408, 282.6077912147245570, 17.79992444728804202 ) ) ;
#86702 = CYLINDRICAL_SURFACE ( 'NONE', #75589, 10.00000000000001066 ) ;
#86703 = CARTESIAN_POINT ( 'NONE',  ( 151.1126408083691501, 268.9122237844355254, -15.82705194100464396 ) ) ;
#86704 = FACE_OUTER_BOUND ( 'NONE', #36854, .T. ) ;
#86705 = VERTEX_POINT ( 'NONE', #48792 ) ;
#86706 = CARTESIAN_POINT ( 'NONE',  ( -4.235833321083918079, 178.3615022471903160, 5.000000000000046185 ) ) ;
#86707 = CARTESIAN_POINT ( 'NONE',  ( -19.65312891409030271, 93.06504152958497400, 177.5919119679930134 ) ) ;
#86708 = LINE ( 'NONE', #17243, #46064 ) ;
#86709 = CARTESIAN_POINT ( 'NONE',  ( 23.46864935082055581, 158.3759306620404743, -22.49999999999984013 ) ) ;
#86710 = CARTESIAN_POINT ( 'NONE',  ( 19.72598728594001116, 34.49540643055188127, 3.479690158560446702E-15 ) ) ;
#86711 = CARTESIAN_POINT ( 'NONE',  ( 163.2442700311756596, 247.8996255919473697, 11.14021925110252020 ) ) ;
#86712 = CARTESIAN_POINT ( 'NONE',  ( 196.8435556370661459, 289.7039558245273838, -16.43899056939217118 ) ) ;
#86713 = CARTESIAN_POINT ( 'NONE',  ( 188.7651867339601210, 270.3529595027822552, -14.65709028123318802 ) ) ;
#86714 = ORIENTED_EDGE ( 'NONE', *, *, #74787, .F. ) ;
#86715 = CARTESIAN_POINT ( 'NONE',  ( 13.56875384759882941, 10.76004757982087945, 5.678558825948272215 ) ) ;
#86716 = B_SPLINE_CURVE_WITH_KNOTS ( 'NONE', 3,
 ( #55556, #87047, #77898, #48487, #23168, #16077 ),
 .UNSPECIFIED., .F., .F.,
 ( 4, 2, 4 ),
 ( 0.02242907851741109126, 0.02703286848893578578, 0.03163665846046048030 ),
 .UNSPECIFIED. ) ;
#86717 = CARTESIAN_POINT ( 'NONE',  ( 189.4969062498522305, 299.9520335943911391, 5.037320497423551480 ) ) ;
#86718 = CARTESIAN_POINT ( 'NONE',  ( 78.98302057781839380, 57.72790023617148591, -16.24074392209231377 ) ) ;
#86719 = CARTESIAN_POINT ( 'NONE',  ( 71.88488839165290756, 72.57896392602057745, -1.213109508826733407 ) ) ;
#86720 = ORIENTED_EDGE ( 'NONE', *, *, #63555, .T. ) ;
#86721 = CARTESIAN_POINT ( 'NONE',  ( -33.75225536883274913, 24.49963747467413810, -10.00000000000000000 ) ) ;
#86723 = EDGE_CURVE ( 'NONE', #10695, #56036, #34737, .T. ) ;
#86722 = DIRECTION ( 'NONE',  ( -0.9708212084269268738, 0.2398044646550215042, 0.000000000000000000 ) ) ;
#86724 = CARTESIAN_POINT ( 'NONE',  ( 85.05360768983020137, 48.89064580773020907, 12.39253331958761883 ) ) ;
#86725 = CARTESIAN_POINT ( 'NONE',  ( 82.81737761406506593, 40.62361263874299055, 0.9906565629087065172 ) ) ;
#86726 = FACE_OUTER_BOUND ( 'NONE', #13930, .T. ) ;
#86727 = EDGE_CURVE ( 'NONE', #57005, #29127, #16871, .T. ) ;
#86728 = ORIENTED_EDGE ( 'NONE', *, *, #18526, .T. ) ;
#86729 = VERTEX_POINT ( 'NONE', #32061 ) ;
#86731 = SURFACE_STYLE_FILL_AREA ( #55740 ) ;
#86730 = CARTESIAN_POINT ( 'NONE',  ( 189.6824569201680788, 274.2416051070018739, -15.66895928228713863 ) ) ;
#86732 = VERTEX_POINT ( 'NONE', #24967 ) ;
#86733 = CARTESIAN_POINT ( 'NONE',  ( 200.8251833487811666, 282.8075743310126882, -16.74393672780000131 ) ) ;
#86734 = EDGE_CURVE ( 'NONE', #22875, #94946, #85568, .T. ) ;
#86735 = CARTESIAN_POINT ( 'NONE',  ( 168.0462690533684338, 251.4142709888886884, 10.74789308012043954 ) ) ;
#86736 = CARTESIAN_POINT ( 'NONE',  ( 72.59376736060184498, 57.25557935749301208, -16.34525399114337674 ) ) ;
#86737 = CARTESIAN_POINT ( 'NONE',  ( 76.72979488479921883, 63.64413466080264214, 15.32332512078611053 ) ) ;
#86739 = EDGE_CURVE ( 'NONE', #38705, #57548, #74637, .T. ) ;
#86738 = CARTESIAN_POINT ( 'NONE',  ( 165.1533192291969954, 284.0593027945823792, 8.797467712081603608 ) ) ;
#86740 = CARTESIAN_POINT ( 'NONE',  ( 102.8537940617441819, 224.0643266524160140, 9.188101187500095079 ) ) ;
#86741 = CARTESIAN_POINT ( 'NONE',  ( 149.0203866098534888, 272.5361143586139860, -12.73049804737905255 ) ) ;
#86742 = CARTESIAN_POINT ( 'NONE',  ( 183.5196873229465950, 288.4008142763526621, -13.17049365496744784 ) ) ;
#86743 = AXIS2_PLACEMENT_3D ( 'NONE', #40467, #10591, #10092 ) ;
#86744 = ORIENTED_EDGE ( 'NONE', *, *, #45399, .F. ) ;
#86745 = CARTESIAN_POINT ( 'NONE',  ( 180.2261984326610218, 279.1782745765357276, -17.42438828499370729 ) ) ;
#86746 = ORIENTED_EDGE ( 'NONE', *, *, #87810, .F. ) ;
#86747 = CARTESIAN_POINT ( 'NONE',  ( 29.31959766232195008, 28.87878583063843152, -9.188101187500006262 ) ) ;
#86748 = CARTESIAN_POINT ( 'NONE',  ( 157.4313451293784851, 259.5368293376414499, 17.50557870161096830 ) ) ;
#86749 = CARTESIAN_POINT ( 'NONE',  ( 78.48406258408499525, 47.91922444745478771, -14.50189708698971636 ) ) ;
#86750 = CARTESIAN_POINT ( 'NONE',  ( 57.27886009182306282, 210.0024278399160949, -9.188101187500093303 ) ) ;
#86751 = CARTESIAN_POINT ( 'NONE',  ( 74.01669459151050035, 68.61891074470059948, 11.40943161386742943 ) ) ;
#86752 = DIRECTION ( 'NONE',  ( -0.8660254037844385966, -0.5000000000000001110, 0.000000000000000000 ) ) ;
#86753 = CARTESIAN_POINT ( 'NONE',  ( 198.0827002274358222, 287.5576944360828975, 17.17879237213074006 ) ) ;
#86754 = VECTOR ( 'NONE', #34521, 1000.000000000000114 ) ;
#86755 = CARTESIAN_POINT ( 'NONE',  ( 176.5315280144691599, 273.2242205654873146, 17.34008498547847665 ) ) ;
#86756 = ORIENTED_EDGE ( 'NONE', *, *, #60011, .T. ) ;
#86757 = CARTESIAN_POINT ( 'NONE',  ( 79.15788838581835307, 56.95875276203359050, -16.19999125909624382 ) ) ;
#86758 = CARTESIAN_POINT ( 'NONE',  ( 85.33874453257102743, 43.13968784339352425, -4.066132831716157803 ) ) ;
#86759 = CARTESIAN_POINT ( 'NONE',  ( 176.5752601597114335, 288.5842064133888130, 11.38490813771325350 ) ) ;
#86760 = CARTESIAN_POINT ( 'NONE',  ( 153.6596595523362794, 266.9882342533689439, 16.60685250298524807 ) ) ;
#86761 = ORIENTED_EDGE ( 'NONE', *, *, #21554, .F. ) ;
#86762 = CARTESIAN_POINT ( 'NONE',  ( 101.8522786425098445, 239.6115022471902876, -5.000000000000047962 ) ) ;
#86763 = CARTESIAN_POINT ( 'NONE',  ( 70.38949794949537875, 69.79236328211965201, -6.331911208559731108 ) ) ;
#86764 = CARTESIAN_POINT ( 'NONE',  ( 161.2977680094314223, 251.2710659906439616, -13.03191437619249982 ) ) ;
#86765 = CARTESIAN_POINT ( 'NONE',  ( 192.8607783413999073, 296.6023284558532396, -11.80574095728561446 ) ) ;
#86766 = CARTESIAN_POINT ( 'NONE',  ( 149.7166446726674565, 271.3301600186404698, 12.26048591517335495 ) ) ;
#86767 = CARTESIAN_POINT ( 'NONE',  ( 136.3105610988903607, 261.0530062829863027, -4.648177544792955347E-16 ) ) ;
#86768 = CARTESIAN_POINT ( 'NONE',  ( 206.2520115784021471, 273.4080321133600933, 11.69992874350409018 ) ) ;
#86769 = CARTESIAN_POINT ( 'NONE',  ( 46.80869107419874098, 110.6443039040113092, -10.00000000000000000 ) ) ;
#86770 = CARTESIAN_POINT ( 'NONE',  ( 154.2604299929738545, 264.1059117911821659, -16.74693418942497303 ) ) ;
#86771 = DIRECTION ( 'NONE',  ( 0.000000000000000000, 0.000000000000000000, 1.000000000000000000 ) ) ;
#86772 = CARTESIAN_POINT ( 'NONE',  ( 105.9656389868882513, 241.1744531367911577, 4.594050593750047540 ) ) ;
#86773 = ORIENTED_EDGE ( 'NONE', *, *, #72937, .F. ) ;
#86774 = AXIS2_PLACEMENT_3D ( 'NONE', #76397, #5979, #84026 ) ;
#86775 = CARTESIAN_POINT ( 'NONE',  ( 191.5893301551938350, 298.8045413135534432, -8.323356515452589477 ) ) ;
#86776 = CARTESIAN_POINT ( 'NONE',  ( 82.78931075109494486, 41.26378757911983541, -2.085430941142616845 ) ) ;
#86777 = CARTESIAN_POINT ( 'NONE',  ( 155.5211745099813356, 261.2764194263634749, -17.18163098020766810 ) ) ;
#86778 = CONICAL_SURFACE ( 'NONE', #83506, 17.82106496071138935, 0.7853981633974672638 ) ;
#86779 = CARTESIAN_POINT ( 'NONE',  ( 163.7010375032499212, 247.1084811230698506, 6.649922295230481950 ) ) ;
#86780 = CARTESIAN_POINT ( 'NONE',  ( 83.74759088628145776, 52.16275448854534602, -14.64583489767789359 ) ) ;
#86781 = CARTESIAN_POINT ( 'NONE',  ( 175.1529877741452026, 252.5256279684296885, 5.213479008607312615 ) ) ;
#86782 = VERTEX_POINT ( 'NONE', #48281 ) ;
#86783 = CARTESIAN_POINT ( 'NONE',  ( 80.54323102745749452, 57.15263273657545540, -16.22921413641979527 ) ) ;
#86784 = CARTESIAN_POINT ( 'NONE',  ( 154.6935981650651684, 273.3457612743501386, -13.11742276744757696 ) ) ;
#86785 = CARTESIAN_POINT ( 'NONE',  ( 182.0160447414319549, 260.4886594560794038, 9.565111796795191523 ) ) ;
#86786 = CARTESIAN_POINT ( 'NONE',  ( 206.1585898378126274, 271.5698433145930721, 8.212139725584252758 ) ) ;
#86787 = CARTESIAN_POINT ( 'NONE',  ( 124.3418758452630613, 242.5958772461660544, -9.188101187500095079 ) ) ;
#86788 = CARTESIAN_POINT ( 'NONE',  ( 151.0426280674448378, 269.0334894088936153, -15.84467774422408581 ) ) ;
#86789 = EDGE_CURVE ( 'NONE', #26239, #99548, #16375, .T. ) ;
#86790 = CARTESIAN_POINT ( 'NONE',  ( 190.3443929803903814, 298.9608357525441420, -8.219721500574586059 ) ) ;
#86791 = DIRECTION ( 'NONE',  ( 0.8660254037844382635, 0.5000000000000005551, 0.000000000000000000 ) ) ;
#86792 = CARTESIAN_POINT ( 'NONE',  ( 57.30635725539759306, 194.7048013555409796, 4.594050593750051981 ) ) ;
#86793 = EDGE_CURVE ( 'NONE', #2857, #56966, #56366, .T. ) ;
#86794 = CARTESIAN_POINT ( 'NONE',  ( 74.01261531380109204, 61.39505503205761272, -15.55988254646882041 ) ) ;
#86795 = CARTESIAN_POINT ( 'NONE',  ( 192.5672132233574700, 296.7161803602032819, 11.26440590052197521 ) ) ;
#86796 = CARTESIAN_POINT ( 'NONE',  ( 69.97056695745257571, 70.69477875497891262, -3.199289782720719177 ) ) ;
#86797 = CARTESIAN_POINT ( 'NONE',  ( 171.3265457834860399, 259.7800479426538800, 15.31382021385433490 ) ) ;
#86798 = CARTESIAN_POINT ( 'NONE',  ( 82.06139759189935035, 41.84807635679941029, -5.567411470978655075 ) ) ;
#86799 = CARTESIAN_POINT ( 'NONE',  ( 178.8786905444916897, 291.7200172712762765, -6.473733745693225572 ) ) ;
#86800 = ADVANCED_FACE ( 'NONE', ( #41157 ), #33585, .F. ) ;
#86801 = CARTESIAN_POINT ( 'NONE',  ( 155.6066474290145720, 261.1283759879266881, -18.16552045242181279 ) ) ;
#86802 = CARTESIAN_POINT ( 'NONE',  ( 153.6642320881653632, 269.2038616895226255, -15.45545102632714851 ) ) ;
#86803 = CARTESIAN_POINT ( 'NONE',  ( 119.8764323552255604, 240.0177522451418497, -10.00000000000009592 ) ) ;
#86804 = B_SPLINE_CURVE_WITH_KNOTS ( 'NONE', 3,
 ( #57992, #79841, #18510, #64096, #26604, #10911, #87479, #41786, #10407, #66094, #27610, #58476, #57479, #18014, #11426, #49896, #34688, #65589 ),
 .UNSPECIFIED., .F., .F.,
 ( 4, 2, 2, 2, 2, 2, 2, 2, 4 ),
 ( 0.000000000000000000, 0.0003050680724331772137, 0.0006101361448663544275, 0.0009152042172995316412, 0.001220272289732708855, 0.001525340362165886069, 0.001830408434599063282, 0.002135476507032240713, 0.002440544579465417710 ),
 .UNSPECIFIED. ) ;
#86805 = CARTESIAN_POINT ( 'NONE',  ( 22.23522817490527359, 21.03677371833801857, 10.00000000000000533 ) ) ;
#86806 = ORIENTED_EDGE ( 'NONE', *, *, #56222, .T. ) ;
#86807 = EDGE_CURVE ( 'NONE', #80416, #96457, #14682, .T. ) ;
#86808 = CARTESIAN_POINT ( 'NONE',  ( 202.9093905060991005, 279.1976216410395182, 16.97070083370504179 ) ) ;
#86809 = CARTESIAN_POINT ( 'NONE',  ( 87.63430470890591550, 44.67548875376495943, 5.011216075979657347 ) ) ;
#86810 = VECTOR ( 'NONE', #35963, 1000.000000000000114 ) ;
#86811 = CARTESIAN_POINT ( 'NONE',  ( 25.93973934025619599, 185.7833772461660544, -9.188101187500095079 ) ) ;
#86812 = CARTESIAN_POINT ( 'NONE',  ( 10.81481306776012019, 28.01751292744054922, 6.180339887498949913 ) ) ;
#86814 = AXIS2_PLACEMENT_3D ( 'NONE', #88401, #72156, #35124 ) ;
#86813 = CARTESIAN_POINT ( 'NONE',  ( 78.97208057699353390, 50.23458188978398908, -15.35366105675574389 ) ) ;
#86815 = DIRECTION ( 'NONE',  ( -0.000000000000000000, -0.000000000000000000, 1.000000000000000000 ) ) ;
#86816 = CARTESIAN_POINT ( 'NONE',  ( 73.92154985004793843, 55.00500715705026522, -16.60400407066505224 ) ) ;
#86818 = CARTESIAN_POINT ( 'NONE',  ( 54.92452707139267432, 202.5177522451418497, -10.00000000000009592 ) ) ;
#86817 = CARTESIAN_POINT ( 'NONE',  ( 198.2595496549591587, 277.4556135032432849, -15.39564098667653980 ) ) ;
#86819 = CARTESIAN_POINT ( 'NONE',  ( 174.5901894622132033, 289.1458820068615978, 7.757015802472061239 ) ) ;
#86820 = CARTESIAN_POINT ( 'NONE',  ( 181.3084254370976396, 256.5650938848051510, 1.317599750949192350 ) ) ;
#86821 = CARTESIAN_POINT ( 'NONE',  ( 205.2937235227012707, 275.0678357141204629, -12.80017165135291535 ) ) ;
#86822 = CARTESIAN_POINT ( 'NONE',  ( 66.50747487571916849, 68.84019554392912710, -4.400006582833474233 ) ) ;
#86823 = ORIENTED_EDGE ( 'NONE', *, *, #18517, .T. ) ;
#86824 = VECTOR ( 'NONE', #63259, 1000.000000000000000 ) ;
#86825 = CARTESIAN_POINT ( 'NONE',  ( 20.80673460501611771, 189.4865022471903160, 10.00000000000009237 ) ) ;
#86826 = CARTESIAN_POINT ( 'NONE',  ( 70.34454795188869980, 61.29844696716961749, 14.78467410895967760 ) ) ;
#86827 = FACE_OUTER_BOUND ( 'NONE', #19787, .T. ) ;
#86828 = CARTESIAN_POINT ( 'NONE',  ( -7.212535326543083158, 157.4548013555409796, -4.594050593750042211 ) ) ;
#86829 = CARTESIAN_POINT ( 'NONE',  ( 33.43441462842632461, 34.70171378149921537, -9.188101187500004485 ) ) ;
#86830 = B_SPLINE_CURVE_WITH_KNOTS ( 'NONE', 3,
 ( #22232, #53621, #98765, #29837 ),
 .UNSPECIFIED., .F., .F.,
 ( 4, 4 ),
 ( 2.797157557069881010E-17, 0.0005907011376378154327 ),
 .UNSPECIFIED. ) ;
#86832 = CARTESIAN_POINT ( 'NONE',  ( 200.1775782763787390, 283.4917191864510073, 16.85546934141439124 ) ) ;
#86831 = CARTESIAN_POINT ( 'NONE',  ( 80.41925082966935179, 57.89142005328343288, -16.24736989457703373 ) ) ;
#86833 = CARTESIAN_POINT ( 'NONE',  ( 152.6845319923753834, 266.1896283897672220, 17.20844521882669653 ) ) ;
#86834 = CARTESIAN_POINT ( 'NONE',  ( 32.17146729527596705, 24.28920272979928541, -7.433330006724141015 ) ) ;
#86835 = CARTESIAN_POINT ( 'NONE',  ( 164.3754245770190039, 245.9404084473339083, 1.667926061651832992 ) ) ;
#86836 = CARTESIAN_POINT ( 'NONE',  ( 184.7859038014685211, 258.6509473366765519, -2.313205586835159089 ) ) ;
#86837 = CARTESIAN_POINT ( 'NONE',  ( 66.30487963216988589, 69.19110079912826450, 2.493735217155242267 ) ) ;
#86838 = VERTEX_POINT ( 'NONE', #43653 ) ;
#86839 =( LENGTH_UNIT ( ) NAMED_UNIT ( * ) SI_UNIT ( .MILLI., .METRE. ) );
#86840 = CARTESIAN_POINT ( 'NONE',  ( 178.4072416225018287, 285.5359605631720683, 12.96076950543191408 ) ) ;
#86841 = CARTESIAN_POINT ( 'NONE',  ( 153.2956058496949936, 277.6605163919303436, -5.395659764655544421 ) ) ;
#86842 = CARTESIAN_POINT ( 'NONE',  ( 12.32384911305235420, 19.06628583063839955, -9.188101187500006262 ) ) ;
#86843 = CARTESIAN_POINT ( 'NONE',  ( 207.2758169296838560, 271.6347492278792402, 8.876423122295557633 ) ) ;
#86844 = AXIS2_PLACEMENT_3D ( 'NONE', #78917, #18097, #41375 ) ;
#86845 = CARTESIAN_POINT ( 'NONE',  ( 84.65536491870415148, 49.91664468313385328, -13.65730316586987669 ) ) ;
#86846 = CARTESIAN_POINT ( 'NONE',  ( 159.3451320108506764, 254.6531307488737355, -16.72997986213134425 ) ) ;
#86847 = EDGE_CURVE ( 'NONE', #7311, #28252, #72605, .T. ) ;
#86848 = CARTESIAN_POINT ( 'NONE',  ( 153.1164404339926080, 265.4415410246681972, 16.15325778160653414 ) ) ;
#86849 = CARTESIAN_POINT ( 'NONE',  ( 207.1601050488701503, 271.8351680844880889, 6.320235450527015075 ) ) ;
#86850 = VECTOR ( 'NONE', #60756, 1000.000000000000000 ) ;
#86851 = CARTESIAN_POINT ( 'NONE',  ( 96.15094473426229627, 232.9865022471903160, 10.00000000000009415 ) ) ;
#86852 = CARTESIAN_POINT ( 'NONE',  ( 87.65066030812953102, 45.32478036133853294, 6.436761220525266225 ) ) ;
#86853 = CARTESIAN_POINT ( 'NONE',  ( 155.4917600441137324, 261.3273667757233056, 17.14261720787171939 ) ) ;
#86854 = ORIENTED_EDGE ( 'NONE', *, *, #11288, .F. ) ;
#86855 = VERTEX_POINT ( 'NONE', #43142 ) ;
#86856 = CARTESIAN_POINT ( 'NONE',  ( 13.67211979723576931, 32.92651376809308772, -10.00000000000000000 ) ) ;
#86857 = CARTESIAN_POINT ( 'NONE',  ( 86.22850481619846619, 47.19188645326008924, 10.82438011396962096 ) ) ;
#86858 = ORIENTED_EDGE ( 'NONE', *, *, #58135, .F. ) ;
#86860 = EDGE_CURVE ( 'NONE', #88596, #64801, #20379, .T. ) ;
#86859 = CARTESIAN_POINT ( 'NONE',  ( 186.1370921618058674, 283.3846817430978149, 17.26256540491417368 ) ) ;
#86861 = CARTESIAN_POINT ( 'NONE',  ( 105.0000000000000000, 0.000000000000000000, 59.99999999999999289 ) ) ;
#86862 = VERTEX_POINT ( 'NONE', #96412 ) ;
#86864 = EDGE_CURVE ( 'NONE', #98279, #78709, #90856, .T. ) ;
#86863 = DIRECTION ( 'NONE',  ( -0.8660254037844387076, -0.4999999999999998890, -0.000000000000000000 ) ) ;
#86865 = CARTESIAN_POINT ( 'NONE',  ( 79.21589564954884111, 59.07845406483318129, -16.22212184578609495 ) ) ;
#86866 = CARTESIAN_POINT ( 'NONE',  ( 12.81113585708611957, 26.13478043621386959, 8.090169943749478065 ) ) ;
#86867 = VERTEX_POINT ( 'NONE', #88842 ) ;
#86868 = CARTESIAN_POINT ( 'NONE',  ( 174.8305575680244317, 267.7453695487130858, 17.43311389002270673 ) ) ;
#86869 = CARTESIAN_POINT ( 'NONE',  ( -32.95600942927097066, 94.73368306973679864, 43.91807046316925778 ) ) ;
#86870 = CARTESIAN_POINT ( 'NONE',  ( 191.3638605175971747, 299.1950661814348678, 7.382965314423603154 ) ) ;
#86871 = CARTESIAN_POINT ( 'NONE',  ( 151.4052515638881573, 274.9757893504045683, -8.619473620707406525 ) ) ;
#86872 = ORIENTED_EDGE ( 'NONE', *, *, #9504, .F. ) ;
#86873 = CARTESIAN_POINT ( 'NONE',  ( 171.2890091316600092, 255.9655340354736666, -11.60100004170818977 ) ) ;
#86874 = CARTESIAN_POINT ( 'NONE',  ( 163.1008115941903895, 248.1481028935802442, 11.25332017433677834 ) ) ;
#86875 = ORIENTED_EDGE ( 'NONE', *, *, #87671, .F. ) ;
#86876 = B_SPLINE_CURVE_WITH_KNOTS ( 'NONE', 3,
 ( #19044, #75223, #13426, #82367, #73232, #49917, #26623, #12937, #58012, #42788, #96561, #58496, #66112, #21033, #5318, #90464, #58978, #4828, #74243, #34221, #73723, #51916, #59482, #4305, #88993, #65116, #27632, #89470, #35710, #28600, #80873, #43796, #44295, #19546, #12427, #36194, #42299, #97536, #66609, #89948, #28105, #3824, #67100, #20028 ),
 .UNSPECIFIED., .F., .F.,
 ( 4, 2, 2, 2, 2, 2, 2, 2, 2, 2, 2, 2, 2, 2, 2, 2, 2, 2, 2, 2, 2, 4 ),
 ( 0.003413446297188858260, 0.003592890090865467987, 0.003682611987703821206, 0.003772333884542174425, 0.003862055781380527644, 0.003951777678218881297, 0.004131221471895593807, 0.004490109059249017959, 0.004848996646602442978, 0.005566771821309291282, 0.006284546996016138719, 0.007720097345429752060, 0.008078984932783212641, 0.008123845881202462760, 0.008168706829621709409, 0.008213567778040957792, 0.008258428726460206176, 0.008437872520137456450, 0.008617316313814708459, 0.008796760107491960468, 0.008976203901169210742, 0.009155647694846462750 ),
 .UNSPECIFIED. ) ;
#86877 = ORIENTED_EDGE ( 'NONE', *, *, #10419, .T. ) ;
#86878 = CARTESIAN_POINT ( 'NONE',  ( 74.23636598098558181, 65.21952277656190233, 13.49801994419013873 ) ) ;
#86879 = ORIENTED_EDGE ( 'NONE', *, *, #51234, .T. ) ;
#86880 = CARTESIAN_POINT ( 'NONE',  ( 161.1242728399023747, 271.1573432374348727, 16.29312882630539150 ) ) ;
#86881 = ORIENTED_EDGE ( 'NONE', *, *, #34742, .T. ) ;
#86882 = CARTESIAN_POINT ( 'NONE',  ( 44.98086946945896614, 119.9434018396067785, 10.00000000000000000 ) ) ;
#86883 = CARTESIAN_POINT ( 'NONE',  ( 72.29246316029069419, 70.94367127312519017, 6.361853069214371104 ) ) ;
#86884 = CARTESIAN_POINT ( 'NONE',  ( 194.3011251241114508, 294.1075746476782342, -14.76047579547631905 ) ) ;
#86885 = CARTESIAN_POINT ( 'NONE',  ( 82.75811122462442881, 53.31634770240417254, -15.29016885083995980 ) ) ;
#86886 = CYLINDRICAL_SURFACE ( 'NONE', #77376, 10.00000000000001066 ) ;
#86887 = ORIENTED_EDGE ( 'NONE', *, *, #52020, .T. ) ;
#86888 = DIRECTION ( 'NONE',  ( -0.4535245244745221282, 0.8912437970051507730, 0.000000000000000000 ) ) ;
#86889 = CARTESIAN_POINT ( 'NONE',  ( 27.42516030814984163, 18.76004757982090609, 5.678558825948272215 ) ) ;
#86890 = CIRCLE ( 'NONE', #5975, 3.300000000000010925 ) ;
#86891 = CARTESIAN_POINT ( 'NONE',  ( 205.8918578537579833, 274.0318366629789466, 11.52627491423194250 ) ) ;
#86892 = CARTESIAN_POINT ( 'NONE',  ( 205.8452707775803390, 274.1125278458945900, 11.42742867493066328 ) ) ;
#86894 = ORIENTED_EDGE ( 'NONE', *, *, #87563, .F. ) ;
#86893 = CARTESIAN_POINT ( 'NONE',  ( 206.9721564454444263, 271.1168479221515213, 4.971250805306120846 ) ) ;
#86895 = VECTOR ( 'NONE', #80505, 1000.000000000000000 ) ;
#86896 = CARTESIAN_POINT ( 'NONE',  ( 147.0973304052008928, 275.8669454108827495, -4.174482164748090085 ) ) ;
#86897 = CARTESIAN_POINT ( 'NONE',  ( 168.6951985533295044, 257.0048723434895805, -14.90311372616637264 ) ) ;
#86898 = CARTESIAN_POINT ( 'NONE',  ( 206.1405152101578437, 273.6011494880188479, -9.618815605734603480 ) ) ;
#86899 = CARTESIAN_POINT ( 'NONE',  ( -19.65312891409030271, 93.06504152958497400, 60.00000000000000000 ) ) ;
#86900 = AXIS2_PLACEMENT_3D ( 'NONE', #68753, #19334, #99180 ) ;
#86901 = CARTESIAN_POINT ( 'NONE',  ( 161.1027382213887336, 251.6088674925233022, 13.55451100897754557 ) ) ;
#86902 = CARTESIAN_POINT ( 'NONE',  ( 191.4231707742389688, 260.8644426583601330, -0.1720874273815105604 ) ) ;
#86903 = ORIENTED_EDGE ( 'NONE', *, *, #26582, .T. ) ;
#86904 = CARTESIAN_POINT ( 'NONE',  ( -22.42236680055709641, 157.8615022471902591, 0.000000000000000000 ) ) ;
#86905 = CARTESIAN_POINT ( 'NONE',  ( 14.26996179277632848, 9.208019796199270246, -3.090169943749474069 ) ) ;
#86906 = CARTESIAN_POINT ( 'NONE',  ( 75.04096107751730926, 66.95220489134598552, -13.17375343603499971 ) ) ;
#86907 = LINE ( 'NONE', #11379, #66136 ) ;
#86908 = CARTESIAN_POINT ( 'NONE',  ( 8.086986483384254853, 182.1427522451419350, -10.00000000000009415 ) ) ;
#86909 = CARTESIAN_POINT ( 'NONE',  ( 81.47361835793333285, 217.8458772461660544, 9.188101187500095079 ) ) ;
#86910 = CARTESIAN_POINT ( 'NONE',  ( 82.32772868565227498, 40.91284795898661031, -1.238209237945167018 ) ) ;
#86911 = CARTESIAN_POINT ( 'NONE',  ( 98.29796604426334738, 220.8927522451418213, 10.00000000000009948 ) ) ;
#86912 = CARTESIAN_POINT ( 'NONE',  ( 208.1303038335461224, 270.1547344959873840, 3.060743731163897863 ) ) ;
#86914 = LINE ( 'NONE', #79307, #60837 ) ;
#86913 = CARTESIAN_POINT ( 'NONE',  ( 13.57207436428344316, 169.4548013555409796, -4.594050593750042211 ) ) ;
#86915 = EDGE_CURVE ( 'NONE', #44311, #74402, #16386, .T. ) ;
#86916 = FACE_OUTER_BOUND ( 'NONE', #27023, .T. ) ;
#86917 = AXIS2_PLACEMENT_3D ( 'NONE', #67666, #60542, #92491 ) ;
#86918 = ORIENTED_EDGE ( 'NONE', *, *, #57486, .F. ) ;
#86919 = VECTOR ( 'NONE', #9214, 1000.000000000000114 ) ;
#86921 = ORIENTED_EDGE ( 'NONE', *, *, #69840, .T. ) ;
#86920 = PRODUCT_DEFINITION_CONTEXT ( 'detailed design', #5503, 'design' ) ;
#86922 = CARTESIAN_POINT ( 'NONE',  ( 200.8891374359296833, 267.7797059101260970, -2.891206998117599625 ) ) ;
#86923 =( REPRESENTATION_RELATIONSHIP ('NONE','NONE', #67038, #35972 ) REPRESENTATION_RELATIONSHIP_WITH_TRANSFORMATION ( #85192 )SHAPE_REPRESENTATION_RELATIONSHIP( ) );
#86924 = ADVANCED_FACE ( 'NONE', ( #49283 ), #57363, .F. ) ;
#86925 = CARTESIAN_POINT ( 'NONE',  ( 80.82015971479509631, 46.89095932202825878, -12.57338494565948217 ) ) ;
#86926 = CARTESIAN_POINT ( 'NONE',  ( 84.47342800902475801, 44.30953683796652598, 7.759599405057208799 ) ) ;
#86927 = CARTESIAN_POINT ( 'NONE',  ( 207.8792014703394671, 270.5896565469619759, -5.780233892547864905 ) ) ;
#86928 =( BOUNDED_CURVE ( )  B_SPLINE_CURVE ( 2, ( #55364, #1706, #47277, #86851, #56378, #48802, #9812, #71107, #56875 ),
 .UNSPECIFIED., .F., .T. ) 
 B_SPLINE_CURVE_WITH_KNOTS ( ( 3, 2, 2, 2, 3 ),
 ( 0.6975806451612903691, 0.6989247311827957443, 0.7016129032258064946, 0.7043010752688172449, 0.7056451612903226200 ),
 .UNSPECIFIED. ) 
 CURVE ( )  GEOMETRIC_REPRESENTATION_ITEM ( )  RATIONAL_B_SPLINE_CURVE ( ( 0.9330127018922194093, 0.9330127018922194093, 1.000000000000000000, 0.8660254037844387076, 1.000000000000000000, 0.8660254037844387076, 1.000000000000000000, 0.9330127018922194093, 0.9330127018922194093 ) ) 
 REPRESENTATION_ITEM ( '' )  );
#86929 = CARTESIAN_POINT ( 'NONE',  ( 82.92763370183318727, 43.61014228372319934, 7.996515586641524287 ) ) ;
#86930 = CARTESIAN_POINT ( 'NONE',  ( 74.23555041547366784, 68.49601928387086502, -11.11897725275786719 ) ) ;
#86931 = CARTESIAN_POINT ( 'NONE',  ( 27.59033994439653270, 195.9244531367911293, -4.594050593750046652 ) ) ;
#86932 = CARTESIAN_POINT ( 'NONE',  ( 75.78130554586785195, 227.8927522451419350, 2.944929066748280225E-16 ) ) ;
#86933 = CARTESIAN_POINT ( 'NONE',  ( 199.3290434049739304, 277.4687221132098784, 15.18886269640733389 ) ) ;
#86934 = ORIENTED_EDGE ( 'NONE', *, *, #82321, .F. ) ;
#86935 = EDGE_CURVE ( 'NONE', #84442, #80986, #90414, .T. ) ;
#86936 = CARTESIAN_POINT ( 'NONE',  ( 84.26780123106441067, 48.10812409167185422, 12.07091365660302884 ) ) ;
#86937 = CARTESIAN_POINT ( 'NONE',  ( 175.1939347090631145, 281.3215438300238134, -14.28959980792798667 ) ) ;
#86938 = CARTESIAN_POINT ( 'NONE',  ( -6.265406815095104776, 161.0643266524160140, 9.188101187500095079 ) ) ;
#86939 = CARTESIAN_POINT ( 'NONE',  ( 69.12672858200176051, 64.33651235087042153, -11.97836756590942642 ) ) ;
#86940 = CARTESIAN_POINT ( 'NONE',  ( 161.1093323826042933, 251.5974460702646809, -13.93502574894237078 ) ) ;
#86941 = LINE ( 'NONE', #49375, #88923 ) ;
#86942 = CARTESIAN_POINT ( 'NONE',  ( 194.5298665426430489, 293.7113828889860656, -16.13302716640051315 ) ) ;
#86943 = CARTESIAN_POINT ( 'NONE',  ( 183.8544464940034402, 258.0811408654732872, -7.110849303899298590 ) ) ;
#86944 = CARTESIAN_POINT ( 'NONE',  ( 171.5331681153915895, 279.9685107613297532, 15.23806245437180351 ) ) ;
#86945 = CARTESIAN_POINT ( 'NONE',  ( 146.5502055023624735, 276.8145935406849389, 0.3770461397900869427 ) ) ;
#86946 = CARTESIAN_POINT ( 'NONE',  ( 190.4744901378711290, 300.7355008658671522, 0.04566709859947504224 ) ) ;
#86947 = ADVANCED_FACE ( 'NONE', ( #21366 ), #5659, .F. ) ;
#86948 = ORIENTED_EDGE ( 'NONE', *, *, #17631, .F. ) ;
#86949 = CARTESIAN_POINT ( 'NONE',  ( 164.1821508476733698, 246.2751683663292397, -7.347745041495428175 ) ) ;
#86950 = CARTESIAN_POINT ( 'NONE',  ( 112.7044859340271472, 242.0024278399160949, 9.188101187500095079 ) ) ;
#86951 = CARTESIAN_POINT ( 'NONE',  ( 21.25954720759204974, 17.98920272979926338, 7.433330006724137462 ) ) ;
#86952 = CARTESIAN_POINT ( 'NONE',  ( 75.28739987566954994, 66.81623516066271407, 13.35525127813182245 ) ) ;
#86953 = PLANE ( 'NONE',  #32243 ) ;
#86955 = CARTESIAN_POINT ( 'NONE',  ( 185.5841049239575398, 288.2424334149885112, 15.16588072270419651 ) ) ;
#86954 = CARTESIAN_POINT ( 'NONE',  ( 157.2333142128019858, 258.3109064714224132, 16.87956768598436597 ) ) ;
#86956 = CARTESIAN_POINT ( 'NONE',  ( 150.6684462061087686, 269.6815914039983682, -13.71741525148136098 ) ) ;
#86957 = CARTESIAN_POINT ( 'NONE',  ( 192.6126025028360402, 263.6580856887314894, -4.343318140713091857 ) ) ;
#86958 = CARTESIAN_POINT ( 'NONE',  ( 148.9504735598738137, 272.6572073132907690, -11.88406006066344744 ) ) ;
#86959 = VECTOR ( 'NONE', #45376, 1000.000000000000114 ) ;
#86960 = CARTESIAN_POINT ( 'NONE',  ( 81.96605124766598749, 41.04055892413879292, -3.298067608424472219 ) ) ;
#86961 = CARTESIAN_POINT ( 'NONE',  ( 172.7262077320602316, 290.4534188193310911, -1.897623738731976983 ) ) ;
#86962 = CARTESIAN_POINT ( 'NONE',  ( 86.37884356567975885, 47.61826986380418703, 10.63568397185587067 ) ) ;
#86963 = ORIENTED_EDGE ( 'NONE', *, *, #67001, .F. ) ;
#86964 = CARTESIAN_POINT ( 'NONE',  ( 139.8153705705071843, 239.9824982072973967, 3.021315404115420679E-15 ) ) ;
#86965 = DIRECTION ( 'NONE',  ( 0.4999999999999998890, -0.8660254037844385966, 0.000000000000000000 ) ) ;
#86966 = AXIS2_PLACEMENT_3D ( 'NONE', #90435, #29578, #12909 ) ;
#86967 = LINE ( 'NONE', #41283, #527 ) ;
#86968 = EDGE_CURVE ( 'NONE', #16667, #15864, #29459, .T. ) ;
#86969 = ORIENTED_EDGE ( 'NONE', *, *, #41935, .T. ) ;
#86970 = B_SPLINE_SURFACE_WITH_KNOTS ( 'NONE', 3, 1, ( 
 ( #86166, #33402 ),
 ( #64303, #70396 ),
 ( #56182, #95254 ),
 ( #86660, #47592 ),
 ( #10107, #16700 ),
 ( #24792, #57185 ),
 ( #88164, #9626 ),
 ( #31886, #2007 ),
 ( #48094, #95758 ),
 ( #62791, #25822 ),
 ( #78520, #25296 ),
 ( #80043, #1521 ),
 ( #56698, #94734 ),
 ( #94240, #87679 ),
 ( #17192, #93748 ),
 ( #40972, #18214 ),
 ( #40487, #26310 ),
 ( #63800, #48613 ),
 ( #10610, #32401 ),
 ( #87176, #18712 ),
 ( #72431, #63298 ),
 ( #3034, #33925 ),
 ( #24307, #64810 ),
 ( #55673, #71918 ),
 ( #39978, #55183 ),
 ( #49594, #80548 ),
 ( #9105, #11125 ),
 ( #1008, #79035 ),
 ( #71417, #79552 ),
 ( #32893, #17712 ),
 ( #42967, #11618 ),
 ( #34401, #73909 ),
 ( #34885, #43973 ),
 ( #3522, #81055 ) ),
 .UNSPECIFIED., .T., .F., .F.,
 ( 4, 2, 2, 2, 2, 2, 2, 2, 2, 2, 2, 2, 2, 2, 2, 2, 4 ),
 ( 2, 2 ),
 ( 0.000000000000000000, 0.06250000000000000000, 0.1250000000000000000, 0.1875000000000000000, 0.2500000000000000000, 0.3125000000000000000, 0.3750000000000000000, 0.4375000000000000000, 0.5000000000000000000, 0.5625000000000000000, 0.6250000000000000000, 0.6875000000000000000, 0.7500000000000000000, 0.8125000000000000000, 0.8750000000000000000, 0.9375000000000000000, 1.000000000000000000 ),
 ( 0.000000000000000000, 1.000000000000000000 ),
 .UNSPECIFIED. ) ;
#86971 = CARTESIAN_POINT ( 'NONE',  ( 147.6095992045671323, 244.4824982072973967, 3.021315404115420679E-15 ) ) ;
#86972 = CARTESIAN_POINT ( 'NONE',  ( 180.2375854341549655, 256.9867171265678394, -8.836682230493849488 ) ) ;
#86973 = CARTESIAN_POINT ( 'NONE',  ( 10.03096235389214286, 7.350182197602630474, 1.163414459189986274E-15 ) ) ;
#86974 = CARTESIAN_POINT ( 'NONE',  ( 192.8132846206021611, 296.6845899933152850, 11.53748932578252351 ) ) ;
#86975 = EDGE_CURVE ( 'NONE', #82867, #93959, #25043, .T. ) ;
#86976 = AXIS2_PLACEMENT_3D ( 'NONE', #34258, #12470, #82413 ) ;
#86977 = ORIENTED_EDGE ( 'NONE', *, *, #77355, .T. ) ;
#86978 = CARTESIAN_POINT ( 'NONE',  ( 191.2386481741904163, 280.2331539523593733, 17.67023438497365362 ) ) ;
#86979 = CARTESIAN_POINT ( 'NONE',  ( 41.11799749075662191, 32.24335787977766898, -9.188101187500008038 ) ) ;
#86980 = CARTESIAN_POINT ( 'NONE',  ( 192.8969106881193909, 288.6213907137100705, -15.93263679494918605 ) ) ;
#86981 = EDGE_LOOP ( 'NONE', ( #38338, #1069, #6475, #70860 ) ) ;
#86982 = CARTESIAN_POINT ( 'NONE',  ( 167.6835809486661049, 280.9580889920492268, 11.68121032124829384 ) ) ;
#86983 = CARTESIAN_POINT ( 'NONE',  ( 164.3625597711517230, 265.6729452914248668, -17.82104740451561753 ) ) ;
#86984 = CARTESIAN_POINT ( 'NONE',  ( -11.26211276271270378, 158.5313752282679900, 0.000000000000000000 ) ) ;
#86985 = ORIENTED_EDGE ( 'NONE', *, *, #30962, .F. ) ;
#86987 = EDGE_CURVE ( 'NONE', #61860, #89587, #69938, .T. ) ;
#86986 = CARTESIAN_POINT ( 'NONE',  ( 86.15816146546031007, 46.97362167137357147, -10.10205920913481847 ) ) ;
#86988 = CARTESIAN_POINT ( 'NONE',  ( 188.8196614944561418, 293.5935099053481281, 12.74832926005498912 ) ) ;
#86989 = CARTESIAN_POINT ( 'NONE',  ( 17.00529913897481293, 33.43149683636510616, 177.5919119679930134 ) ) ;
#86990 = CARTESIAN_POINT ( 'NONE',  ( 78.08492915682273861, 51.99795259853134155, -15.56358649237862579 ) ) ;
#86991 = VECTOR ( 'NONE', #18826, 1000.000000000000000 ) ;
#86992 = CARTESIAN_POINT ( 'NONE',  ( 203.3041373168503299, 278.5139001086923827, -16.61929732091214973 ) ) ;
#86993 = ADVANCED_FACE ( 'NONE', ( #31437 ), #8652, .F. ) ;
#86994 = ORIENTED_EDGE ( 'NONE', *, *, #85455, .F. ) ;
#86995 = EDGE_CURVE ( 'NONE', #93568, #17251, #11634, .T. ) ;
#86996 = ORIENTED_EDGE ( 'NONE', *, *, #15466, .F. ) ;
#86997 = CARTESIAN_POINT ( 'NONE',  ( 57.60966550219794158, 179.2419560658248940, 18.47570218321542868 ) ) ;
#86998 = ORIENTED_EDGE ( 'NONE', *, *, #89456, .F. ) ;
#86999 = CARTESIAN_POINT ( 'NONE',  ( 77.20793521647205182, 49.23014827807851646, -14.84469579315973675 ) ) ;
#87000 = ORIENTED_EDGE ( 'NONE', *, *, #55958, .F. ) ;
#87001 = CARTESIAN_POINT ( 'NONE',  ( 74.30633198134589179, 55.67512901695737781, 16.11735991574911253 ) ) ;
#87002 = CARTESIAN_POINT ( 'NONE',  ( 79.23877006284985214, 53.37623035401563243, 15.75486908137112607 ) ) ;
#87003 = ORIENTED_EDGE ( 'NONE', *, *, #50508, .T. ) ;
#87004 = CARTESIAN_POINT ( 'NONE',  ( 185.7869666842954075, 282.3491821533310713, -17.27175951461987324 ) ) ;
#87005 = AXIS2_PLACEMENT_3D ( 'NONE', #39487, #41504, #80059 ) ;
#87006 = CARTESIAN_POINT ( 'NONE',  ( 205.9580306612148490, 273.9172219983844911, -10.82161348643986720 ) ) ;
#87007 = CARTESIAN_POINT ( 'NONE',  ( 147.4361307740465179, 275.2801259584190916, -5.848038935779946712 ) ) ;
#87008 = CARTESIAN_POINT ( 'NONE',  ( 42.33744422746376301, 122.7866300363639169, -10.00000000000000000 ) ) ;
#87009 = CARTESIAN_POINT ( 'NONE',  ( 146.7944005049231180, 276.3916353892955726, -4.243051111306586520 ) ) ;
#87010 = CARTESIAN_POINT ( 'NONE',  ( 153.3939648708017387, 264.9608545997728015, -16.49556533540763681 ) ) ;
#87011 = CARTESIAN_POINT ( 'NONE',  ( 46.78749671854927783, 204.4865022471903444, 10.00000000000009415 ) ) ;
#87012 = CARTESIAN_POINT ( 'NONE',  ( 157.8247281260298109, 280.9212376166452145, 2.089162359923931955 ) ) ;
#87013 = CARTESIAN_POINT ( 'NONE',  ( 127.9681836757279001, 250.8149278399160949, 9.188101187500093303 ) ) ;
#87014 = CARTESIAN_POINT ( 'NONE',  ( 75.50851089389813353, 54.04939035683948134, 16.08387913541453784 ) ) ;
#87015 = DIRECTION ( 'NONE',  ( -0.8660254037844359321, -0.5000000000000051070, -0.000000000000000000 ) ) ;
#87016 = CARTESIAN_POINT ( 'NONE',  ( 41.44275701717577221, 32.43085787977767609, -9.188101187500008038 ) ) ;
#87017 = ORIENTED_EDGE ( 'NONE', *, *, #87263, .T. ) ;
#87019 = ORIENTED_EDGE ( 'NONE', *, *, #52947, .T. ) ;
#87018 = CARTESIAN_POINT ( 'NONE',  ( 76.28872632190457637, 51.00282802105010660, -16.03419075268625349 ) ) ;
#87020 = CARTESIAN_POINT ( 'NONE',  ( 203.6239051785863410, 276.2879242122419328, 13.38875856211884319 ) ) ;
#87021 = CARTESIAN_POINT ( 'NONE',  ( 178.3662840243317760, 253.4271165972424171, 1.412557629060920750 ) ) ;
#87022 = CARTESIAN_POINT ( 'NONE',  ( 171.7394409073507120, 288.1570534852701257, -4.630247488080818208 ) ) ;
#87023 = DIRECTION ( 'NONE',  ( -0.9303772761487891785, -0.3666034970181814012, 0.000000000000000000 ) ) ;
#87024 = CARTESIAN_POINT ( 'NONE',  ( 72.70287041210059442, 64.35211551445759426, 13.43818951508896120 ) ) ;
#87025 = CARTESIAN_POINT ( 'NONE',  ( 201.0732166862245549, 282.3779679885897167, -18.18766936363638820 ) ) ;
#87026 = CARTESIAN_POINT ( 'NONE',  ( 175.9763040572248656, 288.1059871890528825, -9.332626666196993881 ) ) ;
#87027 = CARTESIAN_POINT ( 'NONE',  ( 193.8885253154310249, 293.1561265193603845, -14.44353267613299785 ) ) ;
#87028 = CARTESIAN_POINT ( 'NONE',  ( 194.9962653018843071, 291.7955338748228087, 15.77605307729832518 ) ) ;
#87029 = ORIENTED_EDGE ( 'NONE', *, *, #96274, .T. ) ;
#87030 = CARTESIAN_POINT ( 'NONE',  ( 194.8067605455144076, 293.2317884077015151, -16.00245909155922774 ) ) ;
#87031 = CARTESIAN_POINT ( 'NONE',  ( 152.8472162863966730, 273.6966317651701956, 11.99970075400534775 ) ) ;
#87032 = ORIENTED_EDGE ( 'NONE', *, *, #92565, .T. ) ;
#87033 = FACE_OUTER_BOUND ( 'NONE', #58874, .T. ) ;
#87034 = CARTESIAN_POINT ( 'NONE',  ( 160.2440860423037350, 278.9300554605163143, 10.54469911904840451 ) ) ;
#87035 = CARTESIAN_POINT ( 'NONE',  ( 152.3899997637754211, 266.6997731741686835, -15.63510712473265052 ) ) ;
#87036 = DIRECTION ( 'NONE',  ( 0.000000000000000000, 0.000000000000000000, 1.000000000000000000 ) ) ;
#87037 = CARTESIAN_POINT ( 'NONE',  ( 163.4260108471723640, 247.5848412648317662, 10.45113099391573108 ) ) ;
#87039 = CARTESIAN_POINT ( 'NONE',  ( 153.9180730477606573, 276.4901683324925443, -8.670461530457965083 ) ) ;
#87038 = CARTESIAN_POINT ( 'NONE',  ( 163.9578236787243100, 284.1347344607588070, -7.051233874980773919 ) ) ;
#87040 = CARTESIAN_POINT ( 'NONE',  ( 162.5076833207704965, 285.2105136841905164, -0.5237628275906566211 ) ) ;
#87041 = VERTEX_POINT ( 'NONE', #39030 ) ;
#87043 = CARTESIAN_POINT ( 'NONE',  ( 167.9126157730074169, 281.9481797483980472, -10.88728177065660851 ) ) ;
#87042 = AXIS2_PLACEMENT_3D ( 'NONE', #14025, #21149, #82968 ) ;
#87044 = CARTESIAN_POINT ( 'NONE',  ( 187.9582674523677213, 263.4472869081138242, -9.058670945028287846 ) ) ;
#87045 = DIRECTION ( 'NONE',  ( -0.000000000000000000, -0.000000000000000000, -1.000000000000000000 ) ) ;
#87046 = CARTESIAN_POINT ( 'NONE',  ( 82.70950877614343710, 211.8927522451418213, 10.00000000000009948 ) ) ;
#87047 = CARTESIAN_POINT ( 'NONE',  ( 169.0357847594885357, 288.9123690687650878, -1.452882998383906221 ) ) ;
#87048 = CARTESIAN_POINT ( 'NONE',  ( 152.6992418905140028, 266.1641500988167763, 17.27767170937316621 ) ) ;
#87049 = CARTESIAN_POINT ( 'NONE',  ( 14.52789699003380974, 30.16126292948894871, -6.180339887498951690 ) ) ;
#87050 = CARTESIAN_POINT ( 'NONE',  ( 73.77685717047434366, 68.42255065178834172, 10.96230068806748825 ) ) ;
#87051 = CARTESIAN_POINT ( 'NONE',  ( 67.69698224970645128, 69.54660018620847950, 2.034176490069760312 ) ) ;
#87052 = CARTESIAN_POINT ( 'NONE',  ( -15.08856125979659346, 174.3464784336661637, 1.353441290958777525E-15 ) ) ;
#87053 = CARTESIAN_POINT ( 'NONE',  ( 79.66011734693590540, 225.9869531367911293, 4.594050593750046652 ) ) ;
#87054 = CARTESIAN_POINT ( 'NONE',  ( -29.83289928091279464, 170.6969210143057580, 1.815056976409021644E-15 ) ) ;
#87055 = CARTESIAN_POINT ( 'NONE',  ( 146.8574506849497538, 276.2824292740633041, -4.888313306692038118 ) ) ;
#87056 = CARTESIAN_POINT ( 'NONE',  ( 182.7920823588448513, 294.2517127691644987, -7.995619123199669609 ) ) ;
#87057 = EDGE_CURVE ( 'NONE', #16332, #26607, #55355, .T. ) ;
#87058 = CARTESIAN_POINT ( 'NONE',  ( 78.99848661620951873, 60.24637179098722584, -16.44349368446545867 ) ) ;
#87059 = VECTOR ( 'NONE', #92569, 1000.000000000000000 ) ;
#87060 = DIRECTION ( 'NONE',  ( 0.4242989612870596283, -0.9055221650797523614, 0.000000000000000000 ) ) ;
#87061 = VECTOR ( 'NONE', #63016, 1000.000000000000114 ) ;
#87062 = B_SPLINE_CURVE_WITH_KNOTS ( 'NONE', 3,
 ( #71368, #47541, #92687, #70344 ),
 .UNSPECIFIED., .F., .F.,
 ( 4, 4 ),
 ( 0.009416156603928334604, 0.01493877551972221454 ),
 .UNSPECIFIED. ) ;
#87064 = CARTESIAN_POINT ( 'NONE',  ( -58.62427208439002158, 70.56504152958493137, 20.00000000000000355 ) ) ;
#87063 = DIRECTION ( 'NONE',  ( 0.5000000000000014433, -0.8660254037844378194, 0.000000000000000000 ) ) ;
#87065 = CARTESIAN_POINT ( 'NONE',  ( 207.9610911165470100, 270.4478195191170471, 5.492635222805117401 ) ) ;
#87066 = EDGE_CURVE ( 'NONE', #67601, #25811, #70971, .T. ) ;
#87067 = CARTESIAN_POINT ( 'NONE',  ( 169.1328200606558312, 252.0173167888393664, -8.779758093320142009 ) ) ;
#87068 =( NAMED_UNIT ( * ) SI_UNIT ( $, .STERADIAN. ) SOLID_ANGLE_UNIT ( ) );
#87069 = CARTESIAN_POINT ( 'NONE',  ( 28.46864935082048831, 149.7156766241961350, 22.50000000000001776 ) ) ;
#87070 = CARTESIAN_POINT ( 'NONE',  ( 74.49716087599449565, 188.9919560658248656, -17.97570218321539315 ) ) ;
#87071 = ADVANCED_FACE ( 'NONE', ( #47140 ), #32945, .F. ) ;
#87072 = CARTESIAN_POINT ( 'NONE',  ( 72.79244417080386143, 57.34122303501653306, -15.86467494005183099 ) ) ;
#87073 = DIRECTION ( 'NONE',  ( 1.000000000000000000, 0.000000000000000000, 0.000000000000000000 ) ) ;
#87074 = CARTESIAN_POINT ( 'NONE',  ( 41.36599039304901737, 188.5643266524159571, -9.188101187500093303 ) ) ;
#87075 = AXIS2_PLACEMENT_3D ( 'NONE', #60685, #83052, #29812 ) ;
#87076 = CARTESIAN_POINT ( 'NONE',  ( 76.93764771006534886, 63.33963654317832948, -15.47180374620822008 ) ) ;
#87077 = CARTESIAN_POINT ( 'NONE',  ( 66.48072710279772934, 203.0643266524160424, 9.188101187500095079 ) ) ;
#87078 = CARTESIAN_POINT ( 'NONE',  ( 64.25234236153551137, 201.2365022471902023, -10.00000000000009237 ) ) ;
#87079 = CARTESIAN_POINT ( 'NONE',  ( 88.37182738025107653, 44.19934082970731026, 0.1226661121921119174 ) ) ;
#87080 = CARTESIAN_POINT ( 'NONE',  ( 12.03141808487008824, 12.11029122506292488, -8.090169943749478065 ) ) ;
#87082 = CARTESIAN_POINT ( 'NONE',  ( 151.9298993999875904, 267.4966903808301026, 16.91367899156788468 ) ) ;
#87081 = DIRECTION ( 'NONE',  ( 0.4999999999999998890, -0.8660254037844385966, 0.000000000000000000 ) ) ;
#87083 = CARTESIAN_POINT ( 'NONE',  ( 20.35567970366385993, 175.8927522451418497, 10.00000000000009948 ) ) ;
#87084 = CARTESIAN_POINT ( 'NONE',  ( 26.18025557360336464, 27.06628583063842797, -9.188101187500006262 ) ) ;
#87085 = PLANE ( 'NONE',  #4621 ) ;
#87086 = CARTESIAN_POINT ( 'NONE',  ( 196.2878005184348353, 290.6665519265632724, -16.69183432842427806 ) ) ;
#87087 = ORIENTED_EDGE ( 'NONE', *, *, #17117, .T. ) ;
#87088 = CARTESIAN_POINT ( 'NONE',  ( 23.10163885443276754, 15.19860640527292261, 2.839279412974134775 ) ) ;
#87089 = CARTESIAN_POINT ( 'NONE',  ( 76.54827242179185021, 208.8768266524160140, 9.188101187500096856 ) ) ;
#87090 = CARTESIAN_POINT ( 'NONE',  ( 76.54295893941512929, 63.70811625220086682, 14.88924590245834345 ) ) ;
#87091 = CARTESIAN_POINT ( 'NONE',  ( 172.6820923522780049, 290.5181543830415762, -0.3406277123404243268 ) ) ;
#87092 = CARTESIAN_POINT ( 'NONE',  ( 73.64338300972052309, 65.35231775803438836, 13.17446611551941693 ) ) ;
#87093 = CARTESIAN_POINT ( 'NONE',  ( 202.0722854591110718, 280.6475301136950407, 16.68111299382005086 ) ) ;
#87094 = CARTESIAN_POINT ( 'NONE',  ( 86.72740319991413571, 46.97082492543196963, 10.28929863393111610 ) ) ;
#87095 = CARTESIAN_POINT ( 'NONE',  ( 193.6371173231629541, 288.3972668369637518, 16.12142398166468382 ) ) ;
#87096 = CARTESIAN_POINT ( 'NONE',  ( 87.54287973956584779, 45.08362754214010693, -6.108144277352557161 ) ) ;
#87097 = CARTESIAN_POINT ( 'NONE',  ( 126.4618338667176261, 250.4865022471902876, -10.00000000000009415 ) ) ;
#87098 = CARTESIAN_POINT ( 'NONE',  ( 19.85049821812295079, 172.2677522451417929, -5.000000000000041744 ) ) ;
#87099 = EDGE_CURVE ( 'NONE', #96593, #79260, #47637, .T. ) ;
#87100 = CARTESIAN_POINT ( 'NONE',  ( 164.7694554770609159, 245.2579269087094076, -3.003635650077957742 ) ) ;
#87101 = VERTEX_POINT ( 'NONE', #41031 ) ;
#87102 = VECTOR ( 'NONE', #4152, 1000.000000000000000 ) ;
#87103 = CARTESIAN_POINT ( 'NONE',  ( 188.5427288919736100, 272.8462714947278300, 15.72219057270026532 ) ) ;
#87104 = ORIENTED_EDGE ( 'NONE', *, *, #58748, .F. ) ;
#87105 = CARTESIAN_POINT ( 'NONE',  ( 203.0337691736598629, 278.9821914694464340, 16.08167820133810011 ) ) ;
#87106 = CARTESIAN_POINT ( 'NONE',  ( 65.82437655349816907, 69.12761348810168727, -0.3171013769033966812 ) ) ;
#87107 = FACE_OUTER_BOUND ( 'NONE', #57622, .T. ) ;
#87108 = EDGE_LOOP ( 'NONE', ( #18770, #43317, #76782, #5200, #50796 ) ) ;
#87110 = EDGE_CURVE ( 'NONE', #41680, #18235, #8366, .T. ) ;
#87109 = CARTESIAN_POINT ( 'NONE',  ( 176.1203811719671535, 253.1057001499724208, -0.2550088935518543543 ) ) ;
#87111 = VERTEX_POINT ( 'NONE', #24846 ) ;
#87113 = EDGE_CURVE ( 'NONE', #63065, #43398, #97568, .T. ) ;
#87112 = FACE_OUTER_BOUND ( 'NONE', #35435, .T. ) ;
#87114 = CARTESIAN_POINT ( 'NONE',  ( 170.6552073324595256, 250.4298647395600881, 3.342757437244376018 ) ) ;
#87115 = CARTESIAN_POINT ( 'NONE',  ( 148.4944702278734781, 274.4665431084056308, 7.703859803813626783 ) ) ;
#87116 = VECTOR ( 'NONE', #65426, 1000.000000000000000 ) ;
#87117 = ORIENTED_EDGE ( 'NONE', *, *, #69452, .T. ) ;
#87118 = AXIS2_PLACEMENT_3D ( 'NONE', #50797, #17930, #76125 ) ;
#87119 = EDGE_CURVE ( 'NONE', #6688, #97892, #25347, .T. ) ;
#87120 = CARTESIAN_POINT ( 'NONE',  ( 20.82173017108080515, 32.99752408145592142, 5.678558825948276656 ) ) ;
#87121 = CARTESIAN_POINT ( 'NONE',  ( 84.72527825293784076, 50.50787217764868586, -13.97547420692928277 ) ) ;
#87122 = CARTESIAN_POINT ( 'NONE',  ( 78.58789454043932210, 49.48878357515709325, -14.64335108961764753 ) ) ;
#87123 = EDGE_CURVE ( 'NONE', #76464, #72231, #16749, .T. ) ;
#87124 = EDGE_CURVE ( 'NONE', #36064, #14175, #61276, .T. ) ;
#87125 = CARTESIAN_POINT ( 'NONE',  ( 160.6526974584403149, 271.0904541309827778, -16.59201714530360050 ) ) ;
#87126 = FACE_OUTER_BOUND ( 'NONE', #64561, .T. ) ;
#87127 = ORIENTED_EDGE ( 'NONE', *, *, #48490, .F. ) ;
#87128 = VERTEX_POINT ( 'NONE', #40031 ) ;
#87129 = CARTESIAN_POINT ( 'NONE',  ( 186.0715527847238207, 298.7753624933060337, 1.084710433360843940 ) ) ;
#87130 = AXIS2_PLACEMENT_3D ( 'NONE', #72943, #2020, #63814 ) ;
#87132 = CARTESIAN_POINT ( 'NONE',  ( 147.8819534105757043, 274.5079385007862811, -9.338341377131436971 ) ) ;
#87131 = CARTESIAN_POINT ( 'NONE',  ( 68.01260680319232677, 65.70736637594835372, 10.87867279016386846 ) ) ;
#87133 = CARTESIAN_POINT ( 'NONE',  ( 34.81516168915606357, 51.10768172523390973, 10.00000000000000000 ) ) ;
#87134 = FACE_OUTER_BOUND ( 'NONE', #49431, .T. ) ;
#87135 = CARTESIAN_POINT ( 'NONE',  ( 34.21278864456112956, 38.49103043416551628, -8.090169943749479842 ) ) ;
#87136 = CARTESIAN_POINT ( 'NONE',  ( 157.8043799545718286, 257.3217915922150496, -17.97575562758749257 ) ) ;
#87137 = CARTESIAN_POINT ( 'NONE',  ( 207.5882819593617796, 271.0935439208888624, -5.111091721253596454 ) ) ;
#87138 = CARTESIAN_POINT ( 'NONE',  ( 76.62458508144393932, 61.22216847580316568, -16.02601530327725854 ) ) ;
#87139 = AXIS2_PLACEMENT_3D ( 'NONE', #99646, #53521, #61112 ) ;
#87140 = CARTESIAN_POINT ( 'NONE',  ( 83.00815485991435594, 53.30142267139500234, 15.60062745561815589 ) ) ;
#87141 = CARTESIAN_POINT ( 'NONE',  ( 76.62902843369037953, 224.2369531367911293, -4.594050593750048428 ) ) ;
#87142 = ORIENTED_EDGE ( 'NONE', *, *, #44572, .F. ) ;
#87143 = CARTESIAN_POINT ( 'NONE',  ( 191.4685399627163633, 299.0137560639802814, 7.545791216288330716 ) ) ;
#87144 = CARTESIAN_POINT ( 'NONE',  ( 177.7634369230092091, 252.8608366103077856, -4.270187854574569275E-12 ) ) ;
#87145 = ORIENTED_EDGE ( 'NONE', *, *, #60007, .F. ) ;
#87146 = CARTESIAN_POINT ( 'NONE',  ( 196.0264968210332768, 291.1191432066681841, -16.98183272759323614 ) ) ;
#87147 = VERTEX_POINT ( 'NONE', #54225 ) ;
#87148 = CARTESIAN_POINT ( 'NONE',  ( 80.07914371544711685, 44.88103632949623290, -11.28840885768255831 ) ) ;
#87149 = CARTESIAN_POINT ( 'NONE',  ( 66.61164111217610184, 67.57600878003083267, 6.268342412446013867 ) ) ;
#87150 = CARTESIAN_POINT ( 'NONE',  ( 146.5913834600193582, 276.7432712258716947, -0.4909717733184599253 ) ) ;
#87151 = CARTESIAN_POINT ( 'NONE',  ( 83.51043124159053832, 41.69464146566779306, -2.173292712442712826 ) ) ;
#87152 = CARTESIAN_POINT ( 'NONE',  ( 83.49336806191682570, 47.60227169604173270, -12.02527693348223359 ) ) ;
#87153 = CARTESIAN_POINT ( 'NONE',  ( 163.0959165854295065, 248.1565812974573930, 11.58894702640622754 ) ) ;
#87154 = CARTESIAN_POINT ( 'NONE',  ( 97.38683515247240052, 227.0333772461660544, 9.188101187500095079 ) ) ;
#87155 = EDGE_LOOP ( 'NONE', ( #96826, #59219, #98939, #66340 ) ) ;
#87156 = VECTOR ( 'NONE', #51524, 1000.000000000000000 ) ;
#87157 = ORIENTED_EDGE ( 'NONE', *, *, #40780, .T. ) ;
#87158 = CARTESIAN_POINT ( 'NONE',  ( 113.0439006004949931, 247.6199935810940929, 2.679491924311251605 ) ) ;
#87159 = CARTESIAN_POINT ( 'NONE',  ( 201.0579808891486380, 282.4043571632192311, -17.91925047041473107 ) ) ;
#87160 = ORIENTED_EDGE ( 'NONE', *, *, #74227, .F. ) ;
#87161 = EDGE_CURVE ( 'NONE', #92377, #5574, #20216, .T. ) ;
#87162 = CARTESIAN_POINT ( 'NONE',  ( 31.74858474661088081, 18.73415679381823651, -6.890680421881970419E-14 ) ) ;
#87163 = CARTESIAN_POINT ( 'NONE',  ( 69.81648863541811068, 69.35147540035858071, -6.558477812184903222 ) ) ;
#87164 = CARTESIAN_POINT ( 'NONE',  ( -8.295327404871391863, 176.0177522451419350, 5.000000000000046185 ) ) ;
#87165 = CARTESIAN_POINT ( 'NONE',  ( 88.04657803224654344, 44.71669033064829080, 4.399168146237476762 ) ) ;
#87166 = ORIENTED_EDGE ( 'NONE', *, *, #1377, .F. ) ;
#87167 = CARTESIAN_POINT ( 'NONE',  ( 86.58890667216479642, 43.96449127922488032, -4.508632658051355158 ) ) ;
#87168 = CARTESIAN_POINT ( 'NONE',  ( 156.8153509015677400, 274.0293242336268236, 13.38325589097203228 ) ) ;
#87169 = CARTESIAN_POINT ( 'NONE',  ( 206.0946696452135427, 273.6805563358039421, -10.19627505985792837 ) ) ;
#87170 = CARTESIAN_POINT ( 'NONE',  ( 147.7528226544125687, 275.1182078777800939, -4.309999617748870193 ) ) ;
#87171 = DIRECTION ( 'NONE',  ( 0.9598361373656965068, -0.2805612043866717031, 0.000000000000000000 ) ) ;
#87172 = CARTESIAN_POINT ( 'NONE',  ( 72.41389820116259557, 70.72247311216294463, 7.745007521649676541 ) ) ;
#87173 = DIRECTION ( 'NONE',  ( -1.000000000000000000, 0.000000000000000000, 0.000000000000000000 ) ) ;
#87174 = ORIENTED_EDGE ( 'NONE', *, *, #29293, .T. ) ;
#87175 = CARTESIAN_POINT ( 'NONE',  ( -19.65312891409030271, 93.06504152958497400, 177.5919119679930134 ) ) ;
#87176 = CARTESIAN_POINT ( 'NONE',  ( 200.5621507313343557, 283.2631601884785368, 16.81037192529623425 ) ) ;
#87177 = CARTESIAN_POINT ( 'NONE',  ( 84.30145135017787084, 42.73273955677608882, 4.648230990532672635 ) ) ;
#87178 = AXIS2_PLACEMENT_3D ( 'NONE', #79280, #65033, #48335 ) ;
#87179 = CARTESIAN_POINT ( 'NONE',  ( 171.6425804079232194, 251.4895661525248727, 7.246871942246497333 ) ) ;
#87180 = CARTESIAN_POINT ( 'NONE',  ( 83.19273697349305507, 52.30514367268771991, 14.84689007325454213 ) ) ;
#87181 = CARTESIAN_POINT ( 'NONE',  ( 175.0511171704688707, 290.6789393214584152, -6.519569310547577601 ) ) ;
#87182 = CARTESIAN_POINT ( 'NONE',  ( 153.5047258249362869, 270.3281759409417759, 14.02017829003231597 ) ) ;
#87183 = ORIENTED_EDGE ( 'NONE', *, *, #70159, .F. ) ;
#87184 = EDGE_CURVE ( 'NONE', #6168, #43553, #63198, .T. ) ;
#87185 = CIRCLE ( 'NONE', #64477, 70.00000000000001421 ) ;
#87186 = AXIS2_PLACEMENT_3D ( 'NONE', #29606, #66608, #21998 ) ;
#87187 = CARTESIAN_POINT ( 'NONE',  ( 76.90746743093833970, 62.93938289886319382, -15.23233999435670150 ) ) ;
#87189 = CARTESIAN_POINT ( 'NONE',  ( 74.30611599946955437, 55.28061810189145575, 16.60300916044171160 ) ) ;
#87188 = CARTESIAN_POINT ( 'NONE',  ( 58.36827475829091583, 216.0530062829863311, -4.648177544792955347E-16 ) ) ;
#87190 = CARTESIAN_POINT ( 'NONE',  ( 69.63353853914595959, 62.64057578429665796, -13.33088475737029732 ) ) ;
#87191 = EDGE_CURVE ( 'NONE', #79669, #56390, #28727, .T. ) ;
#87192 = CARTESIAN_POINT ( 'NONE',  ( 24.08934983677281494, 38.00034080476292075, -1.878358725466461243E-16 ) ) ;
#87193 = CARTESIAN_POINT ( 'NONE',  ( 98.02733310912860532, 220.7365022471901739, -10.00000000000009237 ) ) ;
#87194 = CARTESIAN_POINT ( 'NONE',  ( 172.2199326777433441, 275.1102788966048820, 16.82814706134498905 ) ) ;
#87195 = CARTESIAN_POINT ( 'NONE',  ( 72.46511837996447980, 71.56249752072032777, 6.234640293157904800 ) ) ;
#87196 = CARTESIAN_POINT ( 'NONE',  ( 72.02976470237955198, 59.30830629416842470, -15.33705471575644808 ) ) ;
#87197 = CARTESIAN_POINT ( 'NONE',  ( 189.4870307839178452, 261.4823983659626379, 2.871469372538022924 ) ) ;
#87198 = EDGE_CURVE ( 'NONE', #92094, #65643, #83457, .T. ) ;
#87199 = CARTESIAN_POINT ( 'NONE',  ( 207.5462191418491500, 271.1663988579299485, -5.239401497773396699 ) ) ;
#87200 = VECTOR ( 'NONE', #63715, 1000.000000000000114 ) ;
#87201 = CARTESIAN_POINT ( 'NONE',  ( 7.590999645455913658, 169.0643266524160140, -9.188101187500093303 ) ) ;
#87202 = CARTESIAN_POINT ( 'NONE',  ( 82.50577570618477807, 48.91507585382240109, 13.31341743689232082 ) ) ;
#87203 = VERTEX_POINT ( 'NONE', #43911 ) ;
#87204 = CARTESIAN_POINT ( 'NONE',  ( 160.3464284523794561, 253.3627658000544045, -14.66853605427253271 ) ) ;
#87205 = FACE_OUTER_BOUND ( 'NONE', #14562, .T. ) ;
#87206 = CARTESIAN_POINT ( 'NONE',  ( 84.89744547285587828, 41.79037650531964943, -3.168800655305855967E-06 ) ) ;
#87207 = CARTESIAN_POINT ( 'NONE',  ( 29.78290061743215134, 181.8768266524160424, 9.188101187500096856 ) ) ;
#87208 = LINE ( 'NONE', #41004, #60380 ) ;
#87209 = CARTESIAN_POINT ( 'NONE',  ( 36.11248442148217919, 32.80066082961424456, 10.00000000000000533 ) ) ;
#87210 = CARTESIAN_POINT ( 'NONE',  ( 181.4654272287283447, 294.5040635489617102, 6.489362936760144862 ) ) ;
#87211 = CARTESIAN_POINT ( 'NONE',  ( 191.8210230231139803, 298.4032374945642232, -8.800268167321144475 ) ) ;
#87212 = CARTESIAN_POINT ( 'NONE',  ( 197.0721673821830962, 289.3079886667778737, 16.89290144598883003 ) ) ;
#87213 = CARTESIAN_POINT ( 'NONE',  ( 81.30729757080379727, 56.16728312479073537, 16.09392928925141319 ) ) ;
#87214 = CARTESIAN_POINT ( 'NONE',  ( 5.030029564959478172, 25.83705186507751606, 3.090169943749475401 ) ) ;
#87215 = PRODUCT_DEFINITION_SHAPE ( 'NONE', 'NONE',  #77462 ) ;
#87216 = CARTESIAN_POINT ( 'NONE',  ( 188.9137685052497773, 297.3500637095433490, -7.801865818255394380 ) ) ;
#87217 = CARTESIAN_POINT ( 'NONE',  ( -58.62427208439001447, 70.56504152958493137, -20.00000000000000355 ) ) ;
#87218 = CARTESIAN_POINT ( 'NONE',  ( 83.16056367749570200, 225.4865022471902876, 10.00000000000009237 ) ) ;
#87219 = CARTESIAN_POINT ( 'NONE',  ( 68.57390157943029863, 66.83352816882218406, -9.225073082748975750 ) ) ;
#87220 = EDGE_CURVE ( 'NONE', #78035, #4325, #3376, .T. ) ;
#87221 = CARTESIAN_POINT ( 'NONE',  ( -19.65312891409030271, 93.06504152958497400, -10.00000000000000888 ) ) ;
#87222 = CARTESIAN_POINT ( 'NONE',  ( 41.04123086662985997, 188.3768266524159856, -9.188101187500091527 ) ) ;
#87223 = CARTESIAN_POINT ( 'NONE',  ( 50.51697681462041345, 96.61285555410614734, -10.00000000000000000 ) ) ;
#87224 = ORIENTED_EDGE ( 'NONE', *, *, #85806, .F. ) ;
#87225 = CARTESIAN_POINT ( 'NONE',  ( -6.979067178619878575, 83.87849322502869143, 13.57452325917756220 ) ) ;
#87226 = B_SPLINE_CURVE_WITH_KNOTS ( 'NONE', 3,
 ( #81529, #51072, #35880, #33916, #26303, #20202, #97226, #96735, #65293, #41989 ),
 .UNSPECIFIED., .F., .F.,
 ( 4, 2, 2, 2, 4 ),
 ( 0.000000000000000000, 0.0002622400424272822378, 0.0005244800848545644757, 0.0007867201272818467135, 0.001048960169709128951 ),
 .UNSPECIFIED. ) ;
#87227 = CARTESIAN_POINT ( 'NONE',  ( 198.5954523381739989, 286.6695817285962562, -18.45134152028667174 ) ) ;
#87228 = CARTESIAN_POINT ( 'NONE',  ( 24.17817230090144065, 55.16553699959921175, 59.99999999999999289 ) ) ;
#87229 = VERTEX_POINT ( 'NONE', #44903 ) ;
#87230 = CARTESIAN_POINT ( 'NONE',  ( 86.76900285993092155, 214.2365022471902023, 10.00000000000009948 ) ) ;
#87231 = FACE_OUTER_BOUND ( 'NONE', #50315, .T. ) ;
#87232 = CARTESIAN_POINT ( 'NONE',  ( -24.92236680055716036, 162.1916292661125283, 5.188172501216621122E-14 ) ) ;
#87233 = DIRECTION ( 'NONE',  ( 0.000000000000000000, 0.000000000000000000, 1.000000000000000000 ) ) ;
#87234 = CARTESIAN_POINT ( 'NONE',  ( 30.11465696128792757, 23.10170272979928541, -7.433330006724141015 ) ) ;
#87235 = CARTESIAN_POINT ( 'NONE',  ( 202.6551236945213361, 279.6380246773706517, 15.55476940527561425 ) ) ;
#87236 = CARTESIAN_POINT ( 'NONE',  ( 196.4808189786114951, 290.3322341467384717, -17.84817245450773271 ) ) ;
#87237 = CARTESIAN_POINT ( 'NONE',  ( 188.2366137343229866, 269.6014790893902955, -14.07889599767974431 ) ) ;
#87238 = VERTEX_POINT ( 'NONE', #36313 ) ;
#87239 = CARTESIAN_POINT ( 'NONE',  ( 4.512196379633642174, 24.64646525600387861, -2.839279412974133887 ) ) ;
#87240 = DIRECTION ( 'NONE',  ( 0.2938926261462335709, -0.5090369604551240323, 0.8090169943749504489 ) ) ;
#87241 = CARTESIAN_POINT ( 'NONE',  ( 156.6812872898450735, 261.2670451491295012, 0.000000000000000000 ) ) ;
#87242 = EDGE_CURVE ( 'NONE', #84611, #16883, #67389, .T. ) ;
#87243 = ORIENTED_EDGE ( 'NONE', *, *, #54652, .F. ) ;
#87244 = SHAPE_REPRESENTATION ( 'Upper Movable Jaw Swivel Body', ( #68784 ), #36458 ) ;
#87245 = CARTESIAN_POINT ( 'NONE',  ( 179.7389585068036979, 283.2694176073634935, 16.15404047216739514 ) ) ;
#87246 = CARTESIAN_POINT ( 'NONE',  ( 150.6571681785161445, 269.7011255207979730, 15.24894850018880454 ) ) ;
#87247 = CARTESIAN_POINT ( 'NONE',  ( 177.3670312401388571, 255.9174922417764435, -7.030267280083029924 ) ) ;
#87248 = CARTESIAN_POINT ( 'NONE',  ( 164.7396270603856294, 269.0037874151494179, 17.61975801440670608 ) ) ;
#87249 = ORIENTED_EDGE ( 'NONE', *, *, #85972, .F. ) ;
#87250 = ORIENTED_EDGE ( 'NONE', *, *, #22716, .T. ) ;
#87252 = CARTESIAN_POINT ( 'NONE',  ( 168.8785100482814698, 272.6966330010931756, 17.41127854651366391 ) ) ;
#87251 = CARTESIAN_POINT ( 'NONE',  ( 186.6626062937425843, 272.3587087772825726, -15.95341871095174291 ) ) ;
#87253 = ORIENTED_EDGE ( 'NONE', *, *, #58301, .T. ) ;
#87254 = CARTESIAN_POINT ( 'NONE',  ( 152.6692142062575499, 266.2161595735824449, -16.77985299603479419 ) ) ;
#87255 = AXIS2_PLACEMENT_3D ( 'NONE', #18079, #95116, #17057 ) ;
#87256 = FACE_OUTER_BOUND ( 'NONE', #62135, .T. ) ;
#87257 = CARTESIAN_POINT ( 'NONE',  ( 72.68761047489735461, 57.54079809338966101, -16.30797607761032353 ) ) ;
#87258 = CARTESIAN_POINT ( 'NONE',  ( 76.75190111695991391, 63.66135907976974551, 15.32171075625996259 ) ) ;
#87259 = CARTESIAN_POINT ( 'NONE',  ( 157.1850763439666139, 258.3944569110938687, -16.98181238659443437 ) ) ;
#87260 = CARTESIAN_POINT ( 'NONE',  ( 103.3675627755349353, 239.6744531367911577, 4.594050593750047540 ) ) ;
#87261 = VECTOR ( 'NONE', #192, 999.9999999999998863 ) ;
#87263 = EDGE_CURVE ( 'NONE', #41237, #42896, #32410, .T. ) ;
#87262 = VECTOR ( 'NONE', #81503, 1000.000000000000000 ) ;
#87264 = CARTESIAN_POINT ( 'NONE',  ( 87.40047971330916710, 211.2677522451417929, -5.000000000000041744 ) ) ;
#87265 = ORIENTED_EDGE ( 'NONE', *, *, #5644, .F. ) ;
#87266 = VECTOR ( 'NONE', #98529, 1000.000000000000000 ) ;
#87267 = CARTESIAN_POINT ( 'NONE',  ( 161.7691914441718382, 267.0751698082785310, 16.49970973976455113 ) ) ;
#87268 = ORIENTED_EDGE ( 'NONE', *, *, #5342, .F. ) ;
#87269 = CARTESIAN_POINT ( 'NONE',  ( 33.34238925418374322, 21.11110640527294180, -2.839279412974138328 ) ) ;
#87270 = CARTESIAN_POINT ( 'NONE',  ( 11.23059542939759936, 30.24628978557580794, 10.00000000000000000 ) ) ;
#87271 = CARTESIAN_POINT ( 'NONE',  ( 78.43208466135750712, 48.00925285049068947, -14.01282328640595232 ) ) ;
#87272 = CARTESIAN_POINT ( 'NONE',  ( 49.86334402403631572, 211.8464784336661637, 1.353441290958777525E-15 ) ) ;
#87273 = ORIENTED_EDGE ( 'NONE', *, *, #65292, .F. ) ;
#87274 = CARTESIAN_POINT ( 'NONE',  ( 73.77733668265750566, 68.41783923479601981, 11.46675506585085813 ) ) ;
#87275 = CARTESIAN_POINT ( 'NONE',  ( 150.7254409736883645, 269.5828735707850683, 14.54962197351449049 ) ) ;
#87276 = CARTESIAN_POINT ( 'NONE',  ( 35.43817338645655468, 49.87999306568065805, 10.00000000000000000 ) ) ;
#87277 = CARTESIAN_POINT ( 'NONE',  ( 172.9863964892439867, 271.2482479143764635, 16.42685820048345491 ) ) ;
#87278 = ORIENTED_EDGE ( 'NONE', *, *, #66147, .F. ) ;
#87279 = VECTOR ( 'NONE', #12289, 1000.000000000000114 ) ;
#87280 = CARTESIAN_POINT ( 'NONE',  ( 78.58888364635852497, 57.18144897753006006, -16.20312259563071677 ) ) ;
#87281 = CARTESIAN_POINT ( 'NONE',  ( 178.0447788114544210, 288.9018666865521823, 11.00351160062661826 ) ) ;
#87282 = CARTESIAN_POINT ( 'NONE',  ( 77.52183548858428708, 51.28834266016709620, 15.94339560165845171 ) ) ;
#87283 = ORIENTED_EDGE ( 'NONE', *, *, #287, .F. ) ;
#87284 = CARTESIAN_POINT ( 'NONE',  ( 171.8690269922494451, 259.0866485604661307, -13.74017874718136056 ) ) ;
#87285 = CARTESIAN_POINT ( 'NONE',  ( 174.2854763267832254, 277.2339634087840068, -15.62137160143660175 ) ) ;
#87286 = CARTESIAN_POINT ( 'NONE',  ( 207.1285138014047504, 271.8898857301724661, -5.752177443817618752 ) ) ;
#87287 = CARTESIAN_POINT ( 'NONE',  ( 193.0761489135300906, 296.2292956824684893, -11.99675185248219655 ) ) ;
#87288 = CARTESIAN_POINT ( 'NONE',  ( 50.69007152801540883, 211.6199935810940929, 2.679491924311251605 ) ) ;
#87289 = CARTESIAN_POINT ( 'NONE',  ( 177.3316242072715170, 269.5189898217483346, 16.09928397702987368 ) ) ;
#87290 = AXIS2_PLACEMENT_3D ( 'NONE', #21328, #13723, #37015 ) ;
#87291 = CARTESIAN_POINT ( 'NONE',  ( 206.4943150373521803, 272.9883502116088039, 11.34100825923693101 ) ) ;
#87292 = CARTESIAN_POINT ( 'NONE',  ( 67.28413888684362121, 66.89988542115362691, 9.018600864293709662 ) ) ;
#87293 = CARTESIAN_POINT ( 'NONE',  ( 167.5840822128345167, 256.4747449104621069, 13.66287527167402693 ) ) ;
#87294 = CARTESIAN_POINT ( 'NONE',  ( 131.1144086761837571, 258.0530062829863027, -4.648177544792955347E-16 ) ) ;
#87295 = CARTESIAN_POINT ( 'NONE',  ( 117.8198823448352499, 229.6423013555409796, -4.594050593750043987 ) ) ;
#87296 = ORIENTED_EDGE ( 'NONE', *, *, #88443, .T. ) ;
#87297 = CARTESIAN_POINT ( 'NONE',  ( 148.9673139787263381, 272.6280388522173439, -12.20954562941818722 ) ) ;
#87298 = CARTESIAN_POINT ( 'NONE',  ( 92.16361943412358926, 214.0177522451417929, 5.000000000000051514 ) ) ;
#87299 = DIRECTION ( 'NONE',  ( 0.000000000000000000, 0.000000000000000000, 1.000000000000000000 ) ) ;
#87300 = CARTESIAN_POINT ( 'NONE',  ( 191.8986733338516331, 296.2687432111309249, 12.49828825629462337 ) ) ;
#87301 = CARTESIAN_POINT ( 'NONE',  ( 83.48909022670937929, 51.62989903239390088, -14.87641496889664694 ) ) ;
#87302 = CARTESIAN_POINT ( 'NONE',  ( 76.47316661484272515, 51.61210842333346704, -15.65491330287230376 ) ) ;
#87303 = ORIENTED_EDGE ( 'NONE', *, *, #22835, .T. ) ;
#87304 = CARTESIAN_POINT ( 'NONE',  ( 80.46436188522254440, 57.84947393126303439, -16.24692113171143504 ) ) ;
#87305 = CARTESIAN_POINT ( 'NONE',  ( 156.6472780479514029, 274.0223492104835827, -12.66898415510409137 ) ) ;
#87307 = CARTESIAN_POINT ( 'NONE',  ( 184.6885808911535207, 260.6528513612950064, 10.31057805081157852 ) ) ;
#87306 = CARTESIAN_POINT ( 'NONE',  ( 72.73213343415878285, 70.95121167556251862, 7.670646158728279929 ) ) ;
#87308 = CARTESIAN_POINT ( 'NONE',  ( 206.3528985702396596, 273.2332907176744925, -9.687807306503337657 ) ) ;
#87309 = CARTESIAN_POINT ( 'NONE',  ( 146.6963301283313967, 249.3768266524160424, 9.188101187500096856 ) ) ;
#87310 = CARTESIAN_POINT ( 'NONE',  ( 189.7009002764073102, 294.6524816643598115, -12.56900444601840938 ) ) ;
#87311 = LINE ( 'NONE', #2647, #72457 ) ;
#87312 = LINE ( 'NONE', #55308, #4605 ) ;
#87313 = CARTESIAN_POINT ( 'NONE',  ( 70.29673831216418023, 202.2048013555409796, 4.594050593750051981 ) ) ;
#87314 = CARTESIAN_POINT ( 'NONE',  ( 85.58533047404948491, 48.36141062822003533, -12.20656690058575400 ) ) ;
#87315 = CARTESIAN_POINT ( 'NONE',  ( 157.8719920515997046, 257.2046840049564480, -17.69857783492101433 ) ) ;
#87316 = CARTESIAN_POINT ( 'NONE',  ( 87.92187120394066824, 44.49289898744115135, -3.958561838072920391 ) ) ;
#87317 = EDGE_CURVE ( 'NONE', #98946, #33229, #91646, .T. ) ;
#87318 = CARTESIAN_POINT ( 'NONE',  ( 80.01318412846774208, 44.36046053175815729, -11.54377855748506043 ) ) ;
#87319 = CARTESIAN_POINT ( 'NONE',  ( 171.0837707628333817, 259.8106783156040933, 15.05102682647995849 ) ) ;
#87320 = CARTESIAN_POINT ( 'NONE',  ( 81.76576923011752740, 41.62693581818646749, 5.446883335929131320 ) ) ;
#87321 = LINE ( 'NONE', #17853, #48333 ) ;
#87322 = LINE ( 'NONE', #17854, #10729 ) ;
#87323 = EDGE_CURVE ( 'NONE', #33698, #49174, #68644, .T. ) ;
#87324 = CARTESIAN_POINT ( 'NONE',  ( 194.1322773954189813, 288.8521459192547809, 16.09912479026312937 ) ) ;
#87325 = CARTESIAN_POINT ( 'NONE',  ( 123.7735466722555628, 242.2677522451418497, 10.00000000000009592 ) ) ;
#87326 = ADVANCED_FACE ( 'NONE', ( #70707 ), #63605, .T. ) ;
#87327 = CARTESIAN_POINT ( 'NONE',  ( 79.01371845142224970, 52.41748766984506602, -15.53612108484040100 ) ) ;
#87328 = ORIENTED_EDGE ( 'NONE', *, *, #29720, .T. ) ;
#87329 = EDGE_CURVE ( 'NONE', #54166, #94303, #67197, .T. ) ;
#87330 = VECTOR ( 'NONE', #49503, 1000.000000000000114 ) ;
#87331 = CARTESIAN_POINT ( 'NONE',  ( 190.3049670482083684, 301.0291234702190764, 0.2225066852051815758 ) ) ;
#87332 = CARTESIAN_POINT ( 'NONE',  ( 10.81481306776012019, 28.01751292744054922, 6.180339887498949913 ) ) ;
#87333 = CARTESIAN_POINT ( 'NONE',  ( 45.69611741197122257, 191.0643266524160140, 9.188101187500095079 ) ) ;
#87334 = CIRCLE ( 'NONE', #43569, 17.82106496071138224 ) ;
#87335 = CARTESIAN_POINT ( 'NONE',  ( 23.63615849558155446, 18.81029122506294726, 8.090169943749479842 ) ) ;
#87336 = DIRECTION ( 'NONE',  ( 0.5000000000000002220, -0.8660254037844384856, 0.000000000000000000 ) ) ;
#87337 = DIRECTION ( 'NONE',  ( -0.06958655048002569676, 0.1205274409548614395, -0.9902680687415721383 ) ) ;
#87338 = CARTESIAN_POINT ( 'NONE',  ( 147.3154503175461514, 275.4891506405583073, 3.671329888160011823 ) ) ;
#87339 = FACE_OUTER_BOUND ( 'NONE', #52143, .T. ) ;
#87341 = CARTESIAN_POINT ( 'NONE',  ( 49.65620586503731460, 206.1427522451419350, -10.00000000000009415 ) ) ;
#87340 = CARTESIAN_POINT ( 'NONE',  ( 198.0840284456224651, 277.7725242502040146, -15.93544264248174969 ) ) ;
#87342 = CARTESIAN_POINT ( 'NONE',  ( 123.9359264390130591, 242.3615022471902591, -10.00000000000009592 ) ) ;
#87343 = CARTESIAN_POINT ( 'NONE',  ( 181.2352160778011410, 256.5241942803364736, 1.318112620201692398 ) ) ;
#87344 = CARTESIAN_POINT ( 'NONE',  ( 205.3465787480556344, 274.9762877783610406, -13.79319041940166279 ) ) ;
#87345 = CARTESIAN_POINT ( 'NONE',  ( -62.95439910331221256, 68.06504152958493137, -40.00000000000000000 ) ) ;
#87346 = ORIENTED_EDGE ( 'NONE', *, *, #19358, .T. ) ;
#87347 = B_SPLINE_CURVE_WITH_KNOTS ( 'NONE', 3,
 ( #28024, #23399, #18699, #53792, #124, #69510, #92358, #25807, #77636, #54807, #49093, #2505, #7713, #84754, #77109, #80028, #70509, #33387, #22906, #85260, #11113, #64289, #85784, #10596, #41469, #56682, #23906, #15805, #72417, #15293, #62392 ),
 .UNSPECIFIED., .F., .F.,
 ( 4, 3, 3, 3, 3, 3, 3, 3, 3, 3, 4 ),
 ( 0.000000000000000000, 0.1333490885032282969, 0.3007194338854215498, 0.4699862290245004903, 0.5844252810809279497, 0.6686540514502673505, 0.7354980260655414881, 0.8028463152565613603, 0.8633854507757170449, 0.9437142632667081532, 1.000000000000000000 ),
 .UNSPECIFIED. ) ;
#87348 = AXIS2_PLACEMENT_3D ( 'NONE', #80422, #65660, #43354 ) ;
#87349 = CARTESIAN_POINT ( 'NONE',  ( 179.5139751590971287, 294.9444787810163007, 1.083326342264184117 ) ) ;
#87350 = CARTESIAN_POINT ( 'NONE',  ( 38.19941146435361645, 192.8615022471902591, -10.00000000000009592 ) ) ;
#87351 = CARTESIAN_POINT ( 'NONE',  ( 40.63510790894947888, 184.2677522451417929, -5.000000000000041744 ) ) ;
#87352 = CARTESIAN_POINT ( 'NONE',  ( 162.9796882977680639, 248.3578945969637743, 9.683801903336119565 ) ) ;
#87353 = CARTESIAN_POINT ( 'NONE',  ( 7.942909239684589728, 166.2048013555410080, 4.594050593750051981 ) ) ;
#87354 = CARTESIAN_POINT ( 'NONE',  ( 34.04545031248176912, 37.84336893147759184, -7.433330006724137462 ) ) ;
#87356 = CARTESIAN_POINT ( 'NONE',  ( -19.65312891409030271, 93.06504152958497400, 177.5919119679930134 ) ) ;
#87355 = CARTESIAN_POINT ( 'NONE',  ( 164.2304771159539314, 252.5565421600307729, 13.36745210293446107 ) ) ;
#87357 = CARTESIAN_POINT ( 'NONE',  ( 152.6656396574222754, 266.2223508737794759, 17.04346597795114349 ) ) ;
#87358 = CARTESIAN_POINT ( 'NONE',  ( 32.78250297933140445, 27.43085787977765477, -9.188101187500008038 ) ) ;
#87359 = CARTESIAN_POINT ( 'NONE',  ( 155.9941297720162368, 261.2689480174557843, -17.22357958794880517 ) ) ;
#87360 = LINE ( 'NONE', #56858, #22526 ) ;
#87361 = CARTESIAN_POINT ( 'NONE',  ( 66.08627282113103263, 68.62029620053424139, 1.806069293516707974 ) ) ;
#87362 = ORIENTED_EDGE ( 'NONE', *, *, #43183, .T. ) ;
#87363 = CARTESIAN_POINT ( 'NONE',  ( 42.70400705346037284, 26.78380873178790367, -6.180339887498949025 ) ) ;
#87364 = CARTESIAN_POINT ( 'NONE',  ( 183.6215648671697522, 257.5753772875778509, -6.308267261209747012 ) ) ;
#87365 = CARTESIAN_POINT ( 'NONE',  ( 0.000000000000000000, 0.000000000000000000, 0.000000000000000000 ) ) ;
#87366 = CARTESIAN_POINT ( 'NONE',  ( 4.795442299662375341, 20.95586893147752861, 7.433330006724141015 ) ) ;
#87367 = CARTESIAN_POINT ( 'NONE',  ( 168.6548331014163011, 287.6097714008884623, 0.5119831642859076215 ) ) ;
#87368 = CARTESIAN_POINT ( 'NONE',  ( 17.19404571121151903, 18.43085787977762280, -9.188101187500008038 ) ) ;
#87369 = CIRCLE ( 'NONE', #72706, 1.449999999999993072 ) ;
#87370 = DIRECTION ( 'NONE',  ( -0.000000000000000000, -0.000000000000000000, -1.000000000000000000 ) ) ;
#87371 = CARTESIAN_POINT ( 'NONE',  ( 84.72693717884534692, 49.96098312850357104, -13.65910992477957819 ) ) ;
#87372 = CARTESIAN_POINT ( 'NONE',  ( 206.8659638600981623, 272.3446355680395641, -10.26115277030573125 ) ) ;
#87373 = ORIENTED_EDGE ( 'NONE', *, *, #30664, .F. ) ;
#87374 = CARTESIAN_POINT ( 'NONE',  ( 32.92963059540232251, 19.41603393254328225, -1.583844403245396437 ) ) ;
#87375 = CARTESIAN_POINT ( 'NONE',  ( 206.8986117509267899, 272.2880877623646825, 6.975890063856878598 ) ) ;
#87376 = CARTESIAN_POINT ( 'NONE',  ( 66.25406239667182717, 68.20281254162030393, 4.159574302714934113 ) ) ;
#87377 = CARTESIAN_POINT ( 'NONE',  ( 87.29309660270801885, 45.46152261598134459, 7.123530500323841608 ) ) ;
#87378 = CARTESIAN_POINT ( 'NONE',  ( 155.5204415533959548, 261.2776889444089647, 17.19127227448963424 ) ) ;
#87379 = EDGE_LOOP ( 'NONE', ( #12596, #73771, #6800, #87249 ) ) ;
#87380 = VERTEX_POINT ( 'NONE', #72233 ) ;
#87381 = CARTESIAN_POINT ( 'NONE',  ( 155.9945892501227434, 277.4300987863958312, -10.50269384731501709 ) ) ;
#87382 = CARTESIAN_POINT ( 'NONE',  ( 85.88667062683153119, 47.52433287832054276, 10.83178577085193339 ) ) ;
#87383 = VERTEX_POINT ( 'NONE', #95059 ) ;
#87384 = CARTESIAN_POINT ( 'NONE',  ( 77.20308883393413169, 54.63758335188173731, 16.07556225031585484 ) ) ;
#87385 = CARTESIAN_POINT ( 'NONE',  ( -66.34925969370661392, 42.61035540433362456, -10.00000000000000000 ) ) ;
#87386 = EDGE_LOOP ( 'NONE', ( #87224, #100011, #27753, #80240, #60640, #56953, #84226, #68889 ) ) ;
#87387 = CARTESIAN_POINT ( 'NONE',  ( 78.39257131096576359, 61.24758009167359063, -15.88576424600291226 ) ) ;
#87388 = CYLINDRICAL_SURFACE ( 'NONE', #76677, 17.82106496071139645 ) ;
#87389 = EDGE_CURVE ( 'NONE', #33095, #15038, #46745, .T. ) ;
#87390 = CARTESIAN_POINT ( 'NONE',  ( 174.5814835802148650, 266.1494510194049781, 17.18910567408474677 ) ) ;
#87391 = ORIENTED_EDGE ( 'NONE', *, *, #13889, .T. ) ;
#87392 = CARTESIAN_POINT ( 'NONE',  ( 174.1881985213240682, 267.4147193431427354, 17.25901729942388485 ) ) ;
#87393 = CARTESIAN_POINT ( 'NONE',  ( 169.3620869378731300, 276.4508859477064675, -16.02936318750594324 ) ) ;
#87394 = CARTESIAN_POINT ( 'NONE',  ( 150.8888667059421209, 269.2998118992572927, 15.79021133717968617 ) ) ;
#87395 = CARTESIAN_POINT ( 'NONE',  ( 173.7623083844477208, 263.9770854346508600, 16.71843220567729915 ) ) ;
#87396 = ORIENTED_EDGE ( 'NONE', *, *, #38002, .T. ) ;
#87397 = CARTESIAN_POINT ( 'NONE',  ( 171.2113793187262729, 254.5338664307851957, -11.68439913917253392 ) ) ;
#87398 = CARTESIAN_POINT ( 'NONE',  ( 34.80818111321084274, 38.83478043621391151, -8.090169943749479842 ) ) ;
#87399 = EDGE_LOOP ( 'NONE', ( #39181, #67894, #9033, #6199 ) ) ;
#87400 = ORIENTED_EDGE ( 'NONE', *, *, #61020, .T. ) ;
#87401 = DIRECTION ( 'NONE',  ( 0.8660254037844395958, 0.4999999999999985567, 0.000000000000000000 ) ) ;
#87402 = ORIENTED_EDGE ( 'NONE', *, *, #38188, .F. ) ;
#87403 = PLANE ( 'NONE',  #80051 ) ;
#87404 = ORIENTED_EDGE ( 'NONE', *, *, #12283, .F. ) ;
#87405 = CARTESIAN_POINT ( 'NONE',  ( 5.968649350820469657, 188.6868197944958752, 37.50000000000000000 ) ) ;
#87406 = CARTESIAN_POINT ( 'NONE',  ( 168.7111818900347373, 272.8077130806378818, 15.97973317249935121 ) ) ;
#87407 = CARTESIAN_POINT ( 'NONE',  ( 193.9335844648177272, 294.7441737434225502, 14.74820358206551596 ) ) ;
#87408 = CARTESIAN_POINT ( 'NONE',  ( 177.3385562594880298, 288.8319590472722780, -9.367248622587959872 ) ) ;
#87410 = EDGE_CURVE ( 'NONE', #29964, #62095, #85373, .T. ) ;
#87409 = CARTESIAN_POINT ( 'NONE',  ( 69.44161659878608361, 65.07538059710674361, 11.53483947389128339 ) ) ;
#87411 = CARTESIAN_POINT ( 'NONE',  ( 200.4906113350036776, 281.3870700576555919, -17.24871243658977704 ) ) ;
#87413 = DIRECTION ( 'NONE',  ( -0.9879428538673719062, -0.1548189829846212673, 0.000000000000000000 ) ) ;
#87412 = VECTOR ( 'NONE', #81388, 1000.000000000000000 ) ;
#87414 = DIRECTION ( 'NONE',  ( 0.4999999999999998890, -0.8660254037844385966, 0.000000000000000000 ) ) ;
#87415 = ORIENTED_EDGE ( 'NONE', *, *, #84199, .T. ) ;
#87416 = CARTESIAN_POINT ( 'NONE',  ( 172.2831709724378868, 290.7678881282855059, 1.703707976439254201 ) ) ;
#87417 = CARTESIAN_POINT ( 'NONE',  ( 25.05680157815287146, 15.26216523072494624, -2.296566073217252530E-15 ) ) ;
#87418 = CARTESIAN_POINT ( 'NONE',  ( 164.6241018286200699, 245.5096868128744632, 3.031483545445131433 ) ) ;
#87419 = CARTESIAN_POINT ( 'NONE',  ( 206.3907062969896060, 273.1678058140250300, 11.56942460516550675 ) ) ;
#87421 = ORIENTED_EDGE ( 'NONE', *, *, #97788, .T. ) ;
#87420 = CARTESIAN_POINT ( 'NONE',  ( 159.3528137482544196, 254.6398255893999476, 16.73628156321660398 ) ) ;
#87422 = ORIENTED_EDGE ( 'NONE', *, *, #50988, .F. ) ;
#87423 = CARTESIAN_POINT ( 'NONE',  ( 190.3865446062718547, 300.8878269948957040, 5.596937249297124772 ) ) ;
#87424 = CARTESIAN_POINT ( 'NONE',  ( -14.22851846967002487, 105.1940860163543476, 43.89948692389422291 ) ) ;
#87425 = CARTESIAN_POINT ( 'NONE',  ( 86.78549426258130950, 45.83013854792883990, 8.849882187839872572 ) ) ;
#87426 = PLANE ( 'NONE',  #47314 ) ;
#87427 = CARTESIAN_POINT ( 'NONE',  ( 200.9110265982630779, 282.6588894614233141, 17.52479721249226685 ) ) ;
#87428 = VERTEX_POINT ( 'NONE', #56504 ) ;
#87429 = CARTESIAN_POINT ( 'NONE',  ( 79.14312167556931854, 57.64441083166269664, 0.000000000000000000 ) ) ;
#87430 = CARTESIAN_POINT ( 'NONE',  ( 192.6361035247282985, 294.0892689374524593, 14.43747539422717630 ) ) ;
#87431 = CARTESIAN_POINT ( 'NONE',  ( 50.20806676147353187, 85.59215312471712878, 10.00000000000000000 ) ) ;
#87432 = CARTESIAN_POINT ( 'NONE',  ( -8.638129123654803010, 172.4865022471903160, -10.00000000000009592 ) ) ;
#87433 = CARTESIAN_POINT ( 'NONE',  ( 8.231324050681633864, 188.8927522451419634, 2.944929066748280225E-16 ) ) ;
#87435 = CARTESIAN_POINT ( 'NONE',  ( 97.06207562605321471, 226.8458772461660544, 9.188101187500095079 ) ) ;
#87434 = B_SPLINE_CURVE_WITH_KNOTS ( 'NONE', 3,
 ( #8100, #70384, #69879, #99803, #493, #30389, #39962, #62775, #31380, #62265, #61280, #17178, #47578, #93220, #24293, #63284, #78506, #53673, #1505, #84627, #46068, #94227, #76981, #55660, #86647, #48079, #79020, #9609, #15168, #7584, #38475, #5, #69388, #42463, #41980, #80027, #87664, #26788, #65769, #40959, #1994, #56681, #32880, #96224, #10595, #56166 ),
 .UNSPECIFIED., .F., .F.,
 ( 4, 2, 2, 2, 2, 2, 2, 2, 2, 2, 2, 2, 2, 2, 2, 2, 2, 2, 2, 2, 2, 2, 4 ),
 ( 0.0001899055419981224681, 0.0006750962773007901071, 0.001160287012603457638, 0.001402882380254854341, 0.001645477747906250610, 0.001766775431732028976, 0.001888073115557807342, 0.002009370799383585707, 0.002130668483209364073, 0.002615859218512393836, 0.003101049953815423598, 0.004071431424421405494, 0.005041812895027385222, 0.005527003630330376387, 0.005769598997981835106, 0.006012194365633293826, 0.006072843207546120559, 0.006133492049458947291, 0.006254789733284562593, 0.006497385100935834830, 0.006982575836238381038, 0.007467766571540925512, 0.007952957306843470853 ),
 .UNSPECIFIED. ) ;
#87436 = CARTESIAN_POINT ( 'NONE',  ( 82.55952464939674940, 40.51136557279177453, -1.425512534736172565 ) ) ;
#87437 = DIRECTION ( 'NONE',  ( -0.8660254037844387076, -0.4999999999999998890, -0.000000000000000000 ) ) ;
#87438 = CARTESIAN_POINT ( 'NONE',  ( 166.8010608816141769, 278.4144572394360466, -14.76014027413921070 ) ) ;
#87439 = CARTESIAN_POINT ( 'NONE',  ( 22.85469738715664434, 177.8768266524160140, -9.188101187500091527 ) ) ;
#87440 = VECTOR ( 'NONE', #44777, 1000.000000000000114 ) ;
#87441 = CARTESIAN_POINT ( 'NONE',  ( 161.6673510627899191, 250.6309293646106653, 13.01175935005004192 ) ) ;
#87442 = ORIENTED_EDGE ( 'NONE', *, *, #53591, .F. ) ;
#87443 = EDGE_LOOP ( 'NONE', ( #59788, #75971, #85886, #28001 ) ) ;
#87444 = CARTESIAN_POINT ( 'NONE',  ( 197.7156036016341147, 265.5775033884078766, -2.905260353570674248 ) ) ;
#87445 = CARTESIAN_POINT ( 'NONE',  ( 68.00113622733728391, 69.59165091443878737, 2.730665754880787333 ) ) ;
#87446 = DIRECTION ( 'NONE',  ( 0.000000000000000000, -0.4385670422228005183, 0.8986984752829750844 ) ) ;
#87447 = CARTESIAN_POINT ( 'NONE',  ( 193.1380270375380803, 263.9472543795415049, -4.333440441786139630 ) ) ;
#87448 = CARTESIAN_POINT ( 'NONE',  ( 207.8984236726843164, 270.5563627158673512, -6.084369154771423815 ) ) ;
#87449 = CARTESIAN_POINT ( 'NONE',  ( 182.5715074166515990, 284.2755724526985546, 14.95694440675247527 ) ) ;
#87450 = CARTESIAN_POINT ( 'NONE',  ( 74.47004568639763988, 68.24076931554098735, -11.48438178457268855 ) ) ;
#87451 = CARTESIAN_POINT ( 'NONE',  ( 40.49996498926459054, 188.0643266524160140, 9.188101187500095079 ) ) ;
#87452 = CARTESIAN_POINT ( 'NONE',  ( 86.17361039128121547, 213.8927522451417929, -10.00000000000009059 ) ) ;
#87453 = EDGE_LOOP ( 'NONE', ( #48435, #24368, #55738, #18638, #19466 ) ) ;
#87454 = CARTESIAN_POINT ( 'NONE',  ( 84.02477065797984324, 47.37122689846454904, 11.56964593643152739 ) ) ;
#87455 = EDGE_CURVE ( 'NONE', #40778, #37845, #1822, .T. ) ;
#87456 = CARTESIAN_POINT ( 'NONE',  ( 179.4037581149374034, 257.9870511612666064, -10.76565914641300736 ) ) ;
#87457 = CARTESIAN_POINT ( 'NONE',  ( -1.691623377417284635, 160.6423013555410080, -4.594050593750043987 ) ) ;
#87458 = DIRECTION ( 'NONE',  ( -0.000000000000000000, -0.000000000000000000, -1.000000000000000000 ) ) ;
#87459 = CARTESIAN_POINT ( 'NONE',  ( 207.3874697692679945, 271.4413608369101780, -6.809237722377445401 ) ) ;
#87460 = CARTESIAN_POINT ( 'NONE',  ( -22.42236680055709641, 157.8615022471902591, 0.000000000000000000 ) ) ;
#87461 = CARTESIAN_POINT ( 'NONE',  ( 147.1603453755519695, 275.7578002805973370, -5.230822882238410187 ) ) ;
#87462 = CARTESIAN_POINT ( 'NONE',  ( 185.6713631041849055, 258.9584525764907426, -6.747383155299178092 ) ) ;
#87463 = CARTESIAN_POINT ( 'NONE',  ( 164.1259971043086239, 246.3724295028720519, 5.761669507629934905 ) ) ;
#87464 = CARTESIAN_POINT ( 'NONE',  ( 147.2180753513904961, 275.6578090293250511, 0.4909717733184589261 ) ) ;
#87465 = CARTESIAN_POINT ( 'NONE',  ( 189.8533352240220893, 301.8113727360248504, -0.2033756396389863053 ) ) ;
#87466 = VERTEX_POINT ( 'NONE', #1321 ) ;
#87467 = CARTESIAN_POINT ( 'NONE',  ( 181.4283053378885597, 267.7238133557910373, 16.48022347432943135 ) ) ;
#87468 = CARTESIAN_POINT ( 'NONE',  ( 106.6423081075360813, 238.5024278399160949, -9.188101187500093303 ) ) ;
#87469 = CARTESIAN_POINT ( 'NONE',  ( 17.24455747906367264, 28.14336893147755347, 7.433330006724141015 ) ) ;
#87470 = CARTESIAN_POINT ( 'NONE',  ( 75.22042510487506206, 66.98545636449729557, 12.77795336576078356 ) ) ;
#87471 = VECTOR ( 'NONE', #11042, 1000.000000000000000 ) ;
#87472 = CARTESIAN_POINT ( 'NONE',  ( 35.10161425989549855, 202.6199935810940929, 2.679491924311251605 ) ) ;
#87474 = CARTESIAN_POINT ( 'NONE',  ( 185.5154138499543990, 288.0851626838443735, 14.99196749104353366 ) ) ;
#87473 = CARTESIAN_POINT ( 'NONE',  ( 195.8627871995700502, 291.4026965887302936, 17.41145040657729481 ) ) ;
#87475 = CARTESIAN_POINT ( 'NONE',  ( 204.5925719030185803, 272.9227966449359997, -9.752334820156695727 ) ) ;
#87476 = VERTEX_POINT ( 'NONE', #18525 ) ;
#87477 = CARTESIAN_POINT ( 'NONE',  ( 189.6299445318082348, 261.2437137164477008, -4.504590422874706235 ) ) ;
#87478 = CARTESIAN_POINT ( 'NONE',  ( 196.9728329903666122, 289.4800408803428695, -17.53478045286815856 ) ) ;
#87479 = CARTESIAN_POINT ( 'NONE',  ( 190.3641678128861656, 300.0032373684350659, 4.431439196076422782 ) ) ;
#87480 = CARTESIAN_POINT ( 'NONE',  ( 175.9678860382099685, 292.6092798174653353, -1.135237467879147699 ) ) ;
#87481 = CARTESIAN_POINT ( 'NONE',  ( 81.54078422002766047, 55.47956193386177404, -16.32023236213573369 ) ) ;
#87482 = ORIENTED_EDGE ( 'NONE', *, *, #80161, .T. ) ;
#87483 = DIRECTION ( 'NONE',  ( 0.3103181967972123423, -0.9506327454577433445, 0.000000000000000000 ) ) ;
#87484 = CARTESIAN_POINT ( 'NONE',  ( 181.0697057238064644, 271.7990502603447567, 17.55876967510761233 ) ) ;
#87485 = CARTESIAN_POINT ( 'NONE',  ( 79.98829826350832661, 44.59498145193617802, 11.76229303994366049 ) ) ;
#87486 = CARTESIAN_POINT ( 'NONE',  ( 80.29398387428507533, 55.37432886148820188, 16.01591544229163944 ) ) ;
#87487 = CARTESIAN_POINT ( 'NONE',  ( 155.5311623832600958, 261.6886619413561448, 17.00987194985870943 ) ) ;
#87488 = CARTESIAN_POINT ( 'NONE',  ( 72.34691042023506213, 71.90931229659582868, -5.260778230539377098 ) ) ;
#87489 = VECTOR ( 'NONE', #27060, 1000.000000000000000 ) ;
#87490 = CARTESIAN_POINT ( 'NONE',  ( 179.5358833587677907, 289.0109454785418848, 12.61662917182883525 ) ) ;
#87491 = ORIENTED_EDGE ( 'NONE', *, *, #57998, .T. ) ;
#87492 = CARTESIAN_POINT ( 'NONE',  ( 85.04793144752864009, 49.76842598555754194, 13.42690168825989439 ) ) ;
#87493 = B_SPLINE_SURFACE_WITH_KNOTS ( 'NONE', 3, 1, ( 
 ( #28458, #23219 ),
 ( #36551, #5663 ),
 ( #8045, #90317 ),
 ( #98386, #67458 ),
 ( #90816, #51778 ),
 ( #28977, #46511 ),
 ( #97393, #82719 ),
 ( #77449, #51255 ),
 ( #69823, #52255 ),
 ( #83197, #54108 ),
 ( #13287, #38918 ),
 ( #75573, #66469 ),
 ( #7522, #82221 ),
 ( #31323, #12794 ),
 ( #38415, #20383 ),
 ( #69330, #43146 ),
 ( #44148, #89810 ),
 ( #434, #89337 ),
 ( #100251, #19889 ),
 ( #50760, #5174 ),
 ( #12286, #74087 ),
 ( #4679, #35569 ),
 ( #27961, #17641 ),
 ( #48539, #87611 ),
 ( #62210, #2450 ),
 ( #79478, #71348 ),
 ( #85590, #16131 ),
 ( #1939, #54607 ),
 ( #70837, #18139 ),
 ( #48021, #49039 ),
 ( #64229, #56628 ) ),
 .UNSPECIFIED., .F., .F., .F.,
 ( 4, 3, 3, 3, 3, 3, 3, 3, 3, 3, 4 ),
 ( 2, 2 ),
 ( 0.000000000000000000, 0.1333490885032384554, 0.3007194338854541904, 0.4699862290245523377, 0.5844252810809684728, 0.6686540514502963273, 0.7354980260655706870, 0.8028463152565942229, 0.8633854507757449115, 0.9437142632667596676, 1.000000000000000000 ),
 ( 0.000000000000000000, 1.000000000000000000 ),
 .UNSPECIFIED. ) ;
#87494 = CARTESIAN_POINT ( 'NONE',  ( 37.70440764347101492, 39.95586893147758900, 7.433330006724141015 ) ) ;
#87495 = CARTESIAN_POINT ( 'NONE',  ( 191.9702732701751984, 288.0542607666495201, -15.86116857044228290 ) ) ;
#87496 = ORIENTED_EDGE ( 'NONE', *, *, #34639, .F. ) ;
#87497 = CARTESIAN_POINT ( 'NONE',  ( 77.72205534048291042, 61.52847525230063042, 16.09962475150207339 ) ) ;
#87498 = CARTESIAN_POINT ( 'NONE',  ( 147.7785919239399846, 274.6869658471848652, -7.924750738206837397 ) ) ;
#87499 = CARTESIAN_POINT ( 'NONE',  ( -54.45295541630240166, 33.76759809053437777, -10.00000000000000000 ) ) ;
#87500 = ORIENTED_EDGE ( 'NONE', *, *, #69873, .F. ) ;
#87501 = CARTESIAN_POINT ( 'NONE',  ( 79.35100834308954632, 59.73271264539057057, 16.51943372556190326 ) ) ;
#87502 = DIRECTION ( 'NONE',  ( -0.8660254037844387076, -0.4999999999999998890, -0.000000000000000000 ) ) ;
#87503 = CARTESIAN_POINT ( 'NONE',  ( 151.3284628043366524, 268.5384091220288383, 14.49047510809488237 ) ) ;
#87504 = EDGE_CURVE ( 'NONE', #104, #45744, #90221, .T. ) ;
#87505 = PLANE ( 'NONE',  #46820 ) ;
#87506 = CARTESIAN_POINT ( 'NONE',  ( 80.32950597564698114, 44.91110509010904650, 11.18754419191202842 ) ) ;
#87507 = CARTESIAN_POINT ( 'NONE',  ( 189.4688130559096635, 300.2814762872015422, 3.283936888853890679 ) ) ;
#87508 = DIRECTION ( 'NONE',  ( 0.000000000000000000, 0.000000000000000000, -1.000000000000000000 ) ) ;
#87509 = ORIENTED_EDGE ( 'NONE', *, *, #10193, .T. ) ;
#87510 = ORIENTED_EDGE ( 'NONE', *, *, #25376, .F. ) ;
#87511 = CARTESIAN_POINT ( 'NONE',  ( 178.3793764524178016, 261.0518008416202633, 12.17990814227386842 ) ) ;
#87512 = ORIENTED_EDGE ( 'NONE', *, *, #4575, .T. ) ;
#87513 = CARTESIAN_POINT ( 'NONE',  ( 77.28211008475351207, 49.15284714648134923, -15.31460611935377614 ) ) ;
#87514 = EDGE_LOOP ( 'NONE', ( #9694, #78617, #45939, #99887 ) ) ;
#87515 = CARTESIAN_POINT ( 'NONE',  ( 74.52921011339299184, 56.62722107306336738, 16.07648648383083057 ) ) ;
#87516 = CARTESIAN_POINT ( 'NONE',  ( 79.35712722355306425, 54.04372616740326407, 15.87919829441960395 ) ) ;
#87517 = ORIENTED_EDGE ( 'NONE', *, *, #32054, .F. ) ;
#87518 = CARTESIAN_POINT ( 'NONE',  ( 186.1994311542131868, 282.5051706948743799, -16.93927830648238597 ) ) ;
#87519 = B_SPLINE_CURVE_WITH_KNOTS ( 'NONE', 3,
 ( #20491, #58940, #28067, #12900, #97985, #58459, #81816, #52358, #28563, #43756, #35168, #98493, #59950, #66079, #75680, #51362, #90921, #90425, #36654, #89433, #20998, #67062, #73686, #74202, #12392, #66573, #81323, #13385, #89911, #97499, #97025, #57973, #43257, #11895, #42752, #21471, #44255, #74700, #88957, #5279, #96520, #4792, #4270, #19512, #29085, #13867 ),
 .UNSPECIFIED., .F., .F.,
 ( 4, 1, 2, 2, 1, 2, 2, 1, 1, 2, 2, 1, 1, 2, 2, 1, 1, 2, 2, 1, 1, 1, 2, 2, 1, 1, 1, 2, 2, 4 ),
 ( 0.000000000000000000, 0.06249999999999743261, 0.09374999999999712730, 0.1249999999999968359, 0.1874999999999944766, 0.2187499999999914790, 0.2499999999999884814, 0.3124999999999819589, 0.3437499999999775735, 0.3593749999999752420, 0.3749999999999729661, 0.4374999999999674150, 0.4687499999999651390, 0.4843749999999640288, 0.4999999999999628630, 0.5624999999999517053, 0.5937499999999452660, 0.6093749999999420464, 0.6249999999999387157, 0.6874999999999311662, 0.7187499999999272804, 0.7343749999999259481, 0.7421874999999252820, 0.7499999999999247269, 0.8124999999999363842, 0.8437499999999431566, 0.8593749999999458211, 0.8671874999999463762, 0.8749999999999469313, 1.000000000000000000 ),
 .UNSPECIFIED. ) ;
#87520 = CARTESIAN_POINT ( 'NONE',  ( 81.93012584742906768, 41.13374663330952785, 3.753794840019959889 ) ) ;
#87521 = CARTESIAN_POINT ( 'NONE',  ( 147.8970867440366419, 274.4817267983439137, -7.002141163459742579 ) ) ;
#87522 = CARTESIAN_POINT ( 'NONE',  ( 194.8244254126244357, 266.5110688616923653, 10.33380443192758591 ) ) ;
#87523 = DIRECTION ( 'NONE',  ( -0.9607486656258008573, -0.2774202615135435979, 0.000000000000000000 ) ) ;
#87525 = EDGE_CURVE ( 'NONE', #1235, #62719, #48920, .T. ) ;
#87524 = CARTESIAN_POINT ( 'NONE',  ( 201.0468719883840265, 282.4235983437597497, -16.59631526626950659 ) ) ;
#87526 = DIRECTION ( 'NONE',  ( -0.8903844177683373218, -0.4552093898365224267, 0.000000000000000000 ) ) ;
#87527 = CARTESIAN_POINT ( 'NONE',  ( 153.8473343600284977, 279.7776813690406925, 2.204527152494932807 ) ) ;
#87528 = CARTESIAN_POINT ( 'NONE',  ( 117.0885659928033817, 250.6589784336661637, -6.496448406907675876E-16 ) ) ;
#87529 = ORIENTED_EDGE ( 'NONE', *, *, #78743, .T. ) ;
#87530 = FACE_OUTER_BOUND ( 'NONE', #53444, .T. ) ;
#87531 = ORIENTED_EDGE ( 'NONE', *, *, #72190, .T. ) ;
#87532 = ORIENTED_EDGE ( 'NONE', *, *, #66448, .T. ) ;
#87533 = CARTESIAN_POINT ( 'NONE',  ( 203.5754129385376530, 276.1909035769679690, 13.33079715167354884 ) ) ;
#87534 = CARTESIAN_POINT ( 'NONE',  ( 179.3580451049573981, 255.3422994520020950, 1.318133649256687745 ) ) ;
#87535 = DIRECTION ( 'NONE',  ( 0.5803476755362092510, 0.8143688203140632131, 0.000000000000000000 ) ) ;
#87536 = CARTESIAN_POINT ( 'NONE',  ( 147.1854439606469498, 275.7143282560145963, 4.140517173074471202 ) ) ;
#87537 = CARTESIAN_POINT ( 'NONE',  ( 157.3877702592915568, 280.2823303078274648, -7.027478506402013103 ) ) ;
#87538 = DIRECTION ( 'NONE',  ( 1.000000000000000000, 0.000000000000000000, 0.000000000000000000 ) ) ;
#87539 = DIRECTION ( 'NONE',  ( 0.000000000000000000, -0.000000000000000000, -1.000000000000000000 ) ) ;
#87540 = CARTESIAN_POINT ( 'NONE',  ( -112.5954152546897262, 74.04580364311806306, -21.50000000000000000 ) ) ;
#87541 = DIRECTION ( 'NONE',  ( -0.7696402260561131525, -0.6384778167143280170, 0.000000000000000000 ) ) ;
#87542 =( BOUNDED_CURVE ( )  B_SPLINE_CURVE ( 2, ( #42383, #10507, #65688, #27209, #64200, #79944, #41387, #65202, #72330 ),
 .UNSPECIFIED., .F., .T. ) 
 B_SPLINE_CURVE_WITH_KNOTS ( ( 3, 2, 2, 2, 3 ),
 ( 0.6088709677419354982, 0.6102150537634408733, 0.6129032258064516236, 0.6155913978494623739, 0.6169354838709677491 ),
 .UNSPECIFIED. ) 
 CURVE ( )  GEOMETRIC_REPRESENTATION_ITEM ( )  RATIONAL_B_SPLINE_CURVE ( ( 0.9330127018922194093, 0.9330127018922194093, 1.000000000000000000, 0.8660254037844387076, 1.000000000000000000, 0.8660254037844387076, 1.000000000000000000, 0.9330127018922194093, 0.9330127018922194093 ) ) 
 REPRESENTATION_ITEM ( '' )  );
#87543 = EDGE_LOOP ( 'NONE', ( #24423, #9783, #25156, #83511 ) ) ;
#87544 = CARTESIAN_POINT ( 'NONE',  ( 184.2680897726975786, 272.7852115255601007, -16.27692906205965073 ) ) ;
#87545 = CARTESIAN_POINT ( 'NONE',  ( 65.97972133490638669, 68.67132386035298452, -0.2592375539653856698 ) ) ;
#87546 = VERTEX_POINT ( 'NONE', #79856 ) ;
#87547 = CARTESIAN_POINT ( 'NONE',  ( 30.91722093456329645, 63.30801963086432949, 59.99999999999999289 ) ) ;
#87548 = CARTESIAN_POINT ( 'NONE',  ( 201.0208763613437952, 267.8406677295997156, -2.841550210549272037 ) ) ;
#87549 = CARTESIAN_POINT ( 'NONE',  ( 151.7688039545068364, 267.7757158772707839, -15.79694986370314069 ) ) ;
#87550 = DIRECTION ( 'NONE',  ( 0.5000000000000013323, -0.8660254037844378194, 0.000000000000000000 ) ) ;
#87551 = CARTESIAN_POINT ( 'NONE',  ( 163.1691520398773321, 248.0297337694385931, 11.21816141384514331 ) ) ;
#87553 = CARTESIAN_POINT ( 'NONE',  ( 151.5065022431975876, 275.0122692438795866, -8.642473134862484585 ) ) ;
#87552 = CARTESIAN_POINT ( 'NONE',  ( 153.3178590226085589, 270.2078922168774398, 14.03864727403227874 ) ) ;
#87554 = CYLINDRICAL_SURFACE ( 'NONE', #25239, 17.82106496071139645 ) ;
#87555 = ORIENTED_EDGE ( 'NONE', *, *, #31701, .T. ) ;
#87556 = ADVANCED_FACE ( 'NONE', ( #9927 ), #40788, .T. ) ;
#87557 = CARTESIAN_POINT ( 'NONE',  ( 74.91474539609477290, 61.54304851710285362, -15.22267036536665330 ) ) ;
#87558 = FACE_OUTER_BOUND ( 'NONE', #24608, .T. ) ;
#87559 = EDGE_CURVE ( 'NONE', #49074, #6076, #16453, .T. ) ;
#87560 = CARTESIAN_POINT ( 'NONE',  ( 74.43453170551926235, 65.24630961380456995, -13.55578908557625972 ) ) ;
#87561 = CARTESIAN_POINT ( 'NONE',  ( 152.8107382695299918, 265.9710327055011589, 16.32045346488711246 ) ) ;
#87562 = AXIS2_PLACEMENT_3D ( 'NONE', #58550, #19092, #27681 ) ;
#87563 = EDGE_CURVE ( 'NONE', #74702, #72615, #32215, .T. ) ;
#87564 = CARTESIAN_POINT ( 'NONE',  ( 80.62015840900424735, 43.33333764377209008, -9.369712834007803082 ) ) ;
#87565 = PLANE ( 'NONE',  #49863 ) ;
#87566 = CARTESIAN_POINT ( 'NONE',  ( -12.49048504844327390, 175.8464784336661637, 1.353441290958777525E-15 ) ) ;
#87567 = CARTESIAN_POINT ( 'NONE',  ( 95.60083130504949622, 219.8768266524159856, -9.188101187500091527 ) ) ;
#87568 = CARTESIAN_POINT ( 'NONE',  ( 155.6328838216860220, 261.0829332228125850, -17.51014940606912518 ) ) ;
#87569 = CARTESIAN_POINT ( 'NONE',  ( 88.07467786089314643, 44.31731248180877714, -4.422775558719206579 ) ) ;
#87570 = CARTESIAN_POINT ( 'NONE',  ( 147.7588084490480185, 275.1283837748432575, 4.327974371148282984 ) ) ;
#87571 = DIRECTION ( 'NONE',  ( -0.9909246428798921258, -0.1344185706417024839, 0.000000000000000000 ) ) ;
#87572 = EDGE_CURVE ( 'NONE', #30496, #48220, #72064, .T. ) ;
#87573 = LINE ( 'NONE', #85549, #50556 ) ;
#87574 = CARTESIAN_POINT ( 'NONE',  ( 19.39999966495784989, 36.48715600906564305, -10.00000000000000000 ) ) ;
#87575 = CARTESIAN_POINT ( 'NONE',  ( 164.1453682657562752, 284.0231398948004085, 5.767891135377496425 ) ) ;
#87577 = FACE_OUTER_BOUND ( 'NONE', #71022, .T. ) ;
#87576 = CARTESIAN_POINT ( 'NONE',  ( -22.42236680055709641, 157.8615022471902591, 0.000000000000000000 ) ) ;
#87578 = ADVANCED_FACE ( 'NONE', ( #46635 ), #85184, .F. ) ;
#87579 = CARTESIAN_POINT ( 'NONE',  ( 207.8744451524485441, 270.5978947312061678, 6.164818021356627042 ) ) ;
#87580 = EDGE_CURVE ( 'NONE', #69750, #32340, #62331, .T. ) ;
#87581 = SURFACE_SIDE_STYLE ('',( #94137 ) ) ;
#87582 = CARTESIAN_POINT ( 'NONE',  ( 190.0534303668326288, 269.9073674132432643, 15.26070177760127322 ) ) ;
#87583 = CARTESIAN_POINT ( 'NONE',  ( 81.01231947336798100, 53.36392349131256196, -15.94611761156046192 ) ) ;
#87584 = CARTESIAN_POINT ( 'NONE',  ( 66.48085443433819819, 68.27321713501613942, -4.336635036640815954 ) ) ;
#87585 = CARTESIAN_POINT ( 'NONE',  ( 44.66719160132967659, 208.8464784336661353, 1.353441290958777327E-15 ) ) ;
#87586 = CARTESIAN_POINT ( 'NONE',  ( 175.9190705534530252, 265.3157217463270285, -16.43460560943317361 ) ) ;
#87587 = CARTESIAN_POINT ( 'NONE',  ( 71.40607303893924040, 212.0333772461660544, 9.188101187500095079 ) ) ;
#87588 = CARTESIAN_POINT ( 'NONE',  ( 207.2167723318516153, 271.7370174712370954, -6.606038862010207957 ) ) ;
#87589 = FACE_OUTER_BOUND ( 'NONE', #28136, .T. ) ;
#87590 = DIRECTION ( 'NONE',  ( 0.5000000000000014433, -0.8660254037844378194, 0.000000000000000000 ) ) ;
#87592 = CARTESIAN_POINT ( 'NONE',  ( -3.019589773780833930, 24.80263534580897300, -10.00000000000000000 ) ) ;
#87591 = CARTESIAN_POINT ( 'NONE',  ( 198.7408816115379864, 285.9624092822338071, -17.04496721243561197 ) ) ;
#87593 = CARTESIAN_POINT ( 'NONE',  ( 22.01556172758404628, 173.5177522451417929, 5.000000000000051514 ) ) ;
#87594 = CARTESIAN_POINT ( 'NONE',  ( 30.44305165777243971, 40.68290643055189548, 3.479690158560446702E-15 ) ) ;
#87595 = CARTESIAN_POINT ( 'NONE',  ( -65.00000000000000000, 15.00000000000000000, 59.99999999999999289 ) ) ;
#87596 = CARTESIAN_POINT ( 'NONE',  ( -3.099174982164758951, 179.0177522451419350, 5.000000000000046185 ) ) ;
#87597 = ORIENTED_EDGE ( 'NONE', *, *, #68711, .F. ) ;
#87598 = CARTESIAN_POINT ( 'NONE',  ( 18.31506083472495661, 16.28920272979926054, -7.433330006724141015 ) ) ;
#87599 = CARTESIAN_POINT ( 'NONE',  ( 83.72013207082297015, 209.9548013555409796, -4.594050593750042211 ) ) ;
#87600 = CARTESIAN_POINT ( 'NONE',  ( 76.51987890029035100, 63.61070592637643983, 14.91914813192732403 ) ) ;
#87601 = FACE_OUTER_BOUND ( 'NONE', #55118, .T. ) ;
#87602 = LINE ( 'NONE', #42885, #44196 ) ;
#87603 = CARTESIAN_POINT ( 'NONE',  ( 201.9081421151641962, 280.9318347251351611, 16.34854216200801247 ) ) ;
#87604 = EDGE_LOOP ( 'NONE', ( #55131, #41840, #41437, #42447 ) ) ;
#87605 = CARTESIAN_POINT ( 'NONE',  ( 86.10659305072458380, 47.03284479452093336, 10.73441527774546245 ) ) ;
#87606 = CARTESIAN_POINT ( 'NONE',  ( 124.7815979145579632, 254.3967562850346553, -4.648177544792955347E-16 ) ) ;
#87607 = CARTESIAN_POINT ( 'NONE',  ( 124.0080952226617086, 255.7365022471903444, 2.944929066748280225E-16 ) ) ;
#87608 = CARTESIAN_POINT ( 'NONE',  ( 204.6470611188870521, 276.1878878528713130, -13.02652554726987866 ) ) ;
#87609 = CARTESIAN_POINT ( 'NONE',  ( 74.90174054662361414, 53.21786585885936915, 16.51862851041579461 ) ) ;
#87610 = EDGE_LOOP ( 'NONE', ( #88379, #84800, #38951, #13051 ) ) ;
#87611 = CARTESIAN_POINT ( 'NONE',  ( 82.14148480337546232, 54.17133474984891706, 15.63111399271332047 ) ) ;
#87612 = EDGE_LOOP ( 'NONE', ( #105, #49574, #96803, #98913 ) ) ;
#87613 = CARTESIAN_POINT ( 'NONE',  ( 202.4323889586180201, 280.0238125565655878, 15.69595176008160919 ) ) ;
#87614 = CARTESIAN_POINT ( 'NONE',  ( 150.5438776023515004, 278.3016033182416322, -9.804454847755098641E-05 ) ) ;
#87615 = CARTESIAN_POINT ( 'NONE',  ( -11.40312891409031693, 78.77562236714182120, 52.49999999999999289 ) ) ;
#87616 = ORIENTED_EDGE ( 'NONE', *, *, #71819, .T. ) ;
#87617 = DIRECTION ( 'NONE',  ( -0.000000000000000000, -0.000000000000000000, -1.000000000000000000 ) ) ;
#87618 = VERTEX_POINT ( 'NONE', #39515 ) ;
#87619 = CARTESIAN_POINT ( 'NONE',  ( 189.3598067383799730, 290.0015115173640083, 14.41535925276077812 ) ) ;
#87620 = CARTESIAN_POINT ( 'NONE',  ( 167.4563744213245684, 247.8076185277009529, 3.554669314528694724 ) ) ;
#87621 = DIRECTION ( 'NONE',  ( 0.1237105541964824001, -0.9923183454821336014, 0.000000000000000000 ) ) ;
#87622 = VERTEX_POINT ( 'NONE', #8149 ) ;
#87623 = EDGE_CURVE ( 'NONE', #51674, #69479, #75648, .T. ) ;
#87624 = CARTESIAN_POINT ( 'NONE',  ( 33.10965510200716722, 34.51421378149920827, -9.188101187500004485 ) ) ;
#87625 = CARTESIAN_POINT ( 'NONE',  ( 84.86548878997092515, 50.26520129761993871, -13.37165312599878320 ) ) ;
#87626 = CARTESIAN_POINT ( 'NONE',  ( 86.00921005490911853, 47.65307992534832948, -10.85841856809923378 ) ) ;
#87627 = EDGE_CURVE ( 'NONE', #28084, #47657, #57510, .T. ) ;
#87628 = DIRECTION ( 'NONE',  ( -0.000000000000000000, 0.000000000000000000, -1.000000000000000000 ) ) ;
#87629 = CARTESIAN_POINT ( 'NONE',  ( -78.24550368024017644, 54.29179893118896416, 10.00000000000000000 ) ) ;
#87630 = ORIENTED_EDGE ( 'NONE', *, *, #98347, .F. ) ;
#87631 = VECTOR ( 'NONE', #10285, 1000.000000000000000 ) ;
#87632 = ORIENTED_EDGE ( 'NONE', *, *, #85117, .F. ) ;
#87633 = CARTESIAN_POINT ( 'NONE',  ( 183.1481327660158342, 295.7621509781383793, 0.9827986306915983405 ) ) ;
#87635 = DIRECTION ( 'NONE',  ( -0.6625377181876236365, -0.7490285521785781109, 0.000000000000000000 ) ) ;
#87634 = CARTESIAN_POINT ( 'NONE',  ( 164.2712161151136172, 246.1209027979328710, 7.276091357954241445 ) ) ;
#87636 = CARTESIAN_POINT ( 'NONE',  ( 81.65607015944604541, 55.82719893760320673, -16.00789492171315942 ) ) ;
#87637 = CARTESIAN_POINT ( 'NONE',  ( 154.9683083969241011, 262.2340116239618055, 18.33261662430134109 ) ) ;
#87638 = CARTESIAN_POINT ( 'NONE',  ( 185.4446033158241960, 292.4306437117321025, -11.14656972876700003 ) ) ;
#87639 = CARTESIAN_POINT ( 'NONE',  ( 70.63617790867836277, 60.90204785445763491, 15.02499658488835443 ) ) ;
#87641 = EDGE_CURVE ( 'NONE', #50852, #81157, #6656, .T. ) ;
#87640 = CARTESIAN_POINT ( 'NONE',  ( 164.1706088557112935, 246.2951596828278298, 5.725034427997321984 ) ) ;
#87642 = CARTESIAN_POINT ( 'NONE',  ( 203.8566748796650359, 269.0194278887698260, 2.458571758291232978 ) ) ;
#87643 = DIRECTION ( 'NONE',  ( -0.8660254037844379305, -0.5000000000000011102, -0.000000000000000000 ) ) ;
#87644 = CARTESIAN_POINT ( 'NONE',  ( 90.56688509766992468, 223.0958772461660260, -9.188101187500095079 ) ) ;
#87645 = ORIENTED_EDGE ( 'NONE', *, *, #54776, .F. ) ;
#87646 = DIRECTION ( 'NONE',  ( -0.6139877827364832452, 0.7893155279419866721, 0.000000000000000000 ) ) ;
#87647 = CARTESIAN_POINT ( 'NONE',  ( 77.77867966053455007, 61.43039905302717330, -16.12786080876372807 ) ) ;
#87648 = ORIENTED_EDGE ( 'NONE', *, *, #50620, .F. ) ;
#87649 = CARTESIAN_POINT ( 'NONE',  ( 195.9058436374999701, 291.3281206506429726, -17.17388571147666809 ) ) ;
#87650 = VERTEX_POINT ( 'NONE', #70440 ) ;
#87651 = CARTESIAN_POINT ( 'NONE',  ( 80.01822028430966327, 44.43016943383536699, -11.60302980327384859 ) ) ;
#87652 = EDGE_CURVE ( 'NONE', #70323, #82431, #76080, .T. ) ;
#87653 = CARTESIAN_POINT ( 'NONE',  ( 191.0933613939813540, 299.6635844069401173, -8.689828987424775164 ) ) ;
#87654 = DIRECTION ( 'NONE',  ( -0.8660254037844359321, -0.5000000000000051070, -0.000000000000000000 ) ) ;
#87655 = CARTESIAN_POINT ( 'NONE',  ( 206.3018347371251195, 273.3217358710584790, -9.309724106897926177 ) ) ;
#87656 = CARTESIAN_POINT ( 'NONE',  ( 162.4777017143181581, 249.2273608642169904, 10.60452504456504919 ) ) ;
#87657 = EDGE_CURVE ( 'NONE', #93313, #63730, #23775, .T. ) ;
#87658 = CARTESIAN_POINT ( 'NONE',  ( 88.45577462806285496, 228.0024278399160664, -9.188101187500093303 ) ) ;
#87659 = ORIENTED_EDGE ( 'NONE', *, *, #99968, .T. ) ;
#87660 = ORIENTED_EDGE ( 'NONE', *, *, #97129, .T. ) ;
#87661 = CARTESIAN_POINT ( 'NONE',  ( 163.2256942281324541, 247.9317998266098471, -9.780520296312531059 ) ) ;
#87662 = VERTEX_POINT ( 'NONE', #56739 ) ;
#87663 = CARTESIAN_POINT ( 'NONE',  ( 75.87525401958798454, 64.72722897157592570, -14.29033900848947525 ) ) ;
#87664 = CARTESIAN_POINT ( 'NONE',  ( 165.5828704949435064, 285.3748741401371376, 0.6646079123997954419 ) ) ;
#87665 = CARTESIAN_POINT ( 'NONE',  ( 186.0348036264326481, 259.0250182415348945, 6.435743254585703177 ) ) ;
#87666 = CARTESIAN_POINT ( 'NONE',  ( 147.4771206202524354, 275.6046823160672830, -0.001107820683494442279 ) ) ;
#87667 = CARTESIAN_POINT ( 'NONE',  ( 87.86423278622298483, 44.30858544867225390, 4.762156274856222282 ) ) ;
#87668 = ORIENTED_EDGE ( 'NONE', *, *, #30604, .F. ) ;
#87669 = CARTESIAN_POINT ( 'NONE',  ( 86.65373920060009993, 43.97555830415484479, -4.434315822418210651 ) ) ;
#87670 = CARTESIAN_POINT ( 'NONE',  ( 157.0019680973974801, 274.0489577305648368, 13.29051776178687838 ) ) ;
#87671 = EDGE_CURVE ( 'NONE', #81514, #97599, #16742, .T. ) ;
#87672 = CARTESIAN_POINT ( 'NONE',  ( 82.01519968974108110, 40.98639441602998801, -2.953312919879617304 ) ) ;
#87673 = DIRECTION ( 'NONE',  ( 0.000000000000000000, 0.000000000000000000, 1.000000000000000000 ) ) ;
#87674 = CARTESIAN_POINT ( 'NONE',  ( 174.9037822226496814, 284.1633774455944490, 13.90002592669620185 ) ) ;
#87675 = LINE ( 'NONE', #18210, #44932 ) ;
#87676 = ORIENTED_EDGE ( 'NONE', *, *, #49300, .T. ) ;
#87677 = CARTESIAN_POINT ( 'NONE',  ( 149.0769653949221549, 274.3756200000332797, 9.020936583412852983 ) ) ;
#87678 = EDGE_CURVE ( 'NONE', #96454, #36629, #35803, .T. ) ;
#87679 = CARTESIAN_POINT ( 'NONE',  ( 161.3193951073452581, 251.2336067582368742, 13.01220207292984377 ) ) ;
#87680 = CARTESIAN_POINT ( 'NONE',  ( 85.35261164803672784, 44.05229582933603183, 6.432725872221583430 ) ) ;
#87681 = CARTESIAN_POINT ( 'NONE',  ( 167.6497685817575700, 249.8759886161104475, 7.693690790770736143 ) ) ;
#87682 = CARTESIAN_POINT ( 'NONE',  ( 77.79577372677249514, 62.02059634206501926, 15.64361606394993842 ) ) ;
#87683 = CARTESIAN_POINT ( 'NONE',  ( -33.66737166714137430, 24.21715323669988607, -10.00000000000000000 ) ) ;
#87684 = CARTESIAN_POINT ( 'NONE',  ( 202.7344253759264916, 279.5006701360513830, -16.45903677349620864 ) ) ;
#87685 = EDGE_CURVE ( 'NONE', #10543, #36817, #25339, .T. ) ;
#87686 = ORIENTED_EDGE ( 'NONE', *, *, #30362, .F. ) ;
#87687 = CARTESIAN_POINT ( 'NONE',  ( 27.17098259457989684, 39.18528772668521043, -1.583844403245329602 ) ) ;
#87688 = ADVANCED_FACE ( 'NONE', ( #9668 ), #9148, .F. ) ;
#87689 = ADVANCED_FACE ( 'NONE', ( #2563 ), #57229, .F. ) ;
#87690 = CARTESIAN_POINT ( 'NONE',  ( 207.5338226493333025, 271.1878702128032614, 6.432541580693135863 ) ) ;
#87691 = CARTESIAN_POINT ( 'NONE',  ( 183.0285049134369899, 264.2983816328642774, 14.23074442033831488 ) ) ;
#87692 = CARTESIAN_POINT ( 'NONE',  ( 86.98925081226386169, 46.40596221211884398, -8.809588356812493970 ) ) ;
#87693 = CARTESIAN_POINT ( 'NONE',  ( 38.34546801798370552, 23.10801979619931501, 3.090169943749476733 ) ) ;
#87694 = CARTESIAN_POINT ( 'NONE',  ( 91.00660716696484087, 234.8967562850347122, -4.648177544792955347E-16 ) ) ;
#87695 = CARTESIAN_POINT ( 'NONE',  ( 180.7904606653500821, 273.2281357677318852, 16.74012675949395756 ) ) ;
#87696 = CARTESIAN_POINT ( 'NONE',  ( 161.0980924722764769, 273.3945384687940532, -15.29422357739410110 ) ) ;
#87697 = CARTESIAN_POINT ( 'NONE',  ( 84.81921465843747399, 43.36599167773228203, -5.564511731166422948 ) ) ;
#87698 = CARTESIAN_POINT ( 'NONE',  ( 186.1577919818338387, 274.1963684029099682, -17.47416603093387621 ) ) ;
#87699 = CARTESIAN_POINT ( 'NONE',  ( 9.323050453024791295, 170.0643266524160140, 9.188101187500095079 ) ) ;
#87700 = DIRECTION ( 'NONE',  ( -0.000000000000000000, -0.000000000000000000, -1.000000000000000000 ) ) ;
#87701 = ORIENTED_EDGE ( 'NONE', *, *, #72707, .T. ) ;
#87702 = CARTESIAN_POINT ( 'NONE',  ( 87.10409928669704982, 46.39511029792537045, 8.719520416454489720 ) ) ;
#87703 = DIRECTION ( 'NONE',  ( 0.5000000000000003331, -0.8660254037844383745, 0.000000000000000000 ) ) ;
#87704 = CARTESIAN_POINT ( 'NONE',  ( 204.1986089961618234, 275.4461207950287189, -12.65196423004078419 ) ) ;
#87705 = CARTESIAN_POINT ( 'NONE',  ( 82.10990542498430500, 41.84899041517287088, 5.504228460268151046 ) ) ;
#87706 = CARTESIAN_POINT ( 'NONE',  ( 28.75397480679061601, 199.6589784336661353, -6.496448406907676862E-16 ) ) ;
#87707 = DIRECTION ( 'NONE',  ( 0.4999999999999992784, -0.8660254037844390407, 0.000000000000000000 ) ) ;
#87708 = CARTESIAN_POINT ( 'NONE',  ( 48.87252615048947035, 107.3561085985703016, 10.00000000000000000 ) ) ;
#87709 = CARTESIAN_POINT ( 'NONE',  ( 42.70400705346036574, 26.78380873178790367, -6.180339887498949025 ) ) ;
#87710 = CARTESIAN_POINT ( 'NONE',  ( 199.7952696689775109, 267.3031272996356620, -6.755464101794886211 ) ) ;
#87711 = CARTESIAN_POINT ( 'NONE',  ( 107.6178230991326927, 221.3932355074535678, -2.679491924311248496 ) ) ;
#87712 = CARTESIAN_POINT ( 'NONE',  ( 149.7104618599964851, 271.3408689643206344, 11.89409965450183293 ) ) ;
#87713 = CARTESIAN_POINT ( 'NONE',  ( 182.5845504737252725, 280.2578898108608882, -16.09494218299740353 ) ) ;
#87714 = CARTESIAN_POINT ( 'NONE',  ( 15.56473500984127512, 9.390406791769814632, -7.779800476318352071E-15 ) ) ;
#87715 = CARTESIAN_POINT ( 'NONE',  ( 87.13594473370017113, 46.33577775587144032, -8.608104698120229159 ) ) ;
#87716 = CARTESIAN_POINT ( 'NONE',  ( 84.89261448506458407, 226.4865022471902876, -10.00000000000009592 ) ) ;
#87717 = CARTESIAN_POINT ( 'NONE',  ( 83.66574516303663245, 229.1115022471903160, -5.000000000000047962 ) ) ;
#87718 = CARTESIAN_POINT ( 'NONE',  ( 69.46904662810460707, 66.79780009071521363, -9.892305524425870189 ) ) ;
#87719 = CARTESIAN_POINT ( 'NONE',  ( 39.48212635690286021, 23.76426979415093044, 3.090169943749476733 ) ) ;
#87720 = CARTESIAN_POINT ( 'NONE',  ( 45.88512659934279014, 206.4869531367911009, 4.594050593750046652 ) ) ;
#87721 = DIRECTION ( 'NONE',  ( -0.5169068966820244970, 0.8560416229147732592, 0.000000000000000000 ) ) ;
#87722 = EDGE_LOOP ( 'NONE', ( #73402, #30599, #48330, #65275 ) ) ;
#87723 = CARTESIAN_POINT ( 'NONE',  ( -17.28329050831346692, 82.11986129481219621, 14.61049846789633300 ) ) ;
#87724 = CARTESIAN_POINT ( 'NONE',  ( 190.9498149295421570, 299.9122141765958531, -5.138500224925297566 ) ) ;
#87725 = DIRECTION ( 'NONE',  ( -0.9414334852479518956, -0.3371987438498165734, 0.000000000000000000 ) ) ;
#87726 = ORIENTED_EDGE ( 'NONE', *, *, #93833, .F. ) ;
#87727 = CARTESIAN_POINT ( 'NONE',  ( 167.3994242795659488, 285.0697971307098442, 7.791926321083453288 ) ) ;
#87728 = CARTESIAN_POINT ( 'NONE',  ( -5.676897265278508797, 155.9824982072973683, -6.972266317189433020E-16 ) ) ;
#87729 = CARTESIAN_POINT ( 'NONE',  ( 193.2871234453870386, 295.8638770741889061, 14.00693169951743755 ) ) ;
#87730 = CARTESIAN_POINT ( 'NONE',  ( 72.73830096649396637, 70.17554807097293690, 8.869713815284775649 ) ) ;
#87731 = CARTESIAN_POINT ( 'NONE',  ( 27.26159103020561147, 24.24335787977764767, -9.188101187500008038 ) ) ;
#87732 = CARTESIAN_POINT ( 'NONE',  ( 163.3706531435203146, 247.6807236201477735, 10.06957846017757241 ) ) ;
#87733 = CARTESIAN_POINT ( 'NONE',  ( 196.7491951525289835, 289.8673929779723721, -16.35352603081977207 ) ) ;
#87734 = CARTESIAN_POINT ( 'NONE',  ( 44.08135397534552169, 118.8355609772188188, 10.00000000000000000 ) ) ;
#87735 = ORIENTED_EDGE ( 'NONE', *, *, #21436, .T. ) ;
#87736 = CARTESIAN_POINT ( 'NONE',  ( 12.16147613323643029, 27.99752408145590721, 5.678558825948276656 ) ) ;
#87737 = CARTESIAN_POINT ( 'NONE',  ( 15.54637163393425148, 191.3297689869269504, -2.679491924311252493 ) ) ;
#87738 = CARTESIAN_POINT ( 'NONE',  ( 87.78081971166569986, 44.10618430004836910, 2.676874261813567468 ) ) ;
#87739 = ORIENTED_EDGE ( 'NONE', *, *, #3345, .T. ) ;
#87740 = CARTESIAN_POINT ( 'NONE',  ( 178.6316378771798554, 282.3279298503816221, 15.59256888213965198 ) ) ;
#87741 = CARTESIAN_POINT ( 'NONE',  ( 77.93017357788673394, 184.0458036431182052, -21.50000000000000000 ) ) ;
#87742 = CARTESIAN_POINT ( 'NONE',  ( 79.14312167556931854, 57.64441083166269664, 0.000000000000000000 ) ) ;
#87743 = CARTESIAN_POINT ( 'NONE',  ( 76.32984284614508397, 63.49129372016874839, -15.29838449762297614 ) ) ;
#87744 = ORIENTED_EDGE ( 'NONE', *, *, #10851, .T. ) ;
#87745 = ORIENTED_EDGE ( 'NONE', *, *, #24516, .F. ) ;
#87747 = CARTESIAN_POINT ( 'NONE',  ( 151.1448005994188577, 269.3082076351089995, -13.99603974239249737 ) ) ;
#87746 = CARTESIAN_POINT ( 'NONE',  ( 187.0452942487604275, 272.6200080864273332, -15.85002353977101386 ) ) ;
#87748 = CARTESIAN_POINT ( 'NONE',  ( 16.72324493992723049, 11.78380873178785748, -6.180339887498949025 ) ) ;
#87749 = EDGE_LOOP ( 'NONE', ( #35473, #16638, #36688, #52755 ) ) ;
#87750 = CARTESIAN_POINT ( 'NONE',  ( -71.61465314115659453, 63.06504152958490295, 203.6502102582797420 ) ) ;
#87751 = CARTESIAN_POINT ( 'NONE',  ( 72.09461912472968947, 72.35512880999853280, -3.358616764072534178 ) ) ;
#87752 = CARTESIAN_POINT ( 'NONE',  ( 72.72402067594053676, 57.21056264940069269, -15.87973078800185966 ) ) ;
#87753 = CARTESIAN_POINT ( 'NONE',  ( 78.26014935871903333, 61.04899649461657418, -15.91113552180851620 ) ) ;
#87754 = CARTESIAN_POINT ( 'NONE',  ( 204.7242223814549504, 276.0542406257275161, -13.93608974681376189 ) ) ;
#87756 = ADVANCED_FACE ( 'NONE', ( #43405 ), #55222, .T. ) ;
#87755 = CARTESIAN_POINT ( 'NONE',  ( 108.1307024963493149, 242.4244531367911293, -4.594050593750046652 ) ) ;
#87757 = CARTESIAN_POINT ( 'NONE',  ( 196.2630260332681189, 290.7094625936034049, -17.43112004684450866 ) ) ;
#87758 = CARTESIAN_POINT ( 'NONE',  ( 184.1488128701229812, 288.7864932478067885, -13.16340755393728834 ) ) ;
#87759 = ORIENTED_EDGE ( 'NONE', *, *, #56731, .F. ) ;
#87760 = CARTESIAN_POINT ( 'NONE',  ( 208.2939409893161553, 269.8713066281881083, 2.523744790997269227 ) ) ;
#87761 = ORIENTED_EDGE ( 'NONE', *, *, #13845, .F. ) ;
#87762 = CARTESIAN_POINT ( 'NONE',  ( 40.27059248445925732, 25.11110640527295601, -2.839279412974138328 ) ) ;
#87763 = CARTESIAN_POINT ( 'NONE',  ( 197.8977219949227049, 287.8780861330898801, 17.48564646125164046 ) ) ;
#87764 = CARTESIAN_POINT ( 'NONE',  ( 204.6748560047368244, 275.6941871888094511, -12.57733492443129464 ) ) ;
#87765 = CARTESIAN_POINT ( 'NONE',  ( 60.66220569506229765, 196.6423013555410080, -4.594050593750043987 ) ) ;
#87766 = ADVANCED_FACE ( 'NONE', ( #47631 ), #5531, .F. ) ;
#87767 = CARTESIAN_POINT ( 'NONE',  ( 74.41176536287696308, 68.30213538679808494, 11.38880159922067747 ) ) ;
#87768 = LINE ( 'NONE', #34486, #32067 ) ;
#87769 = CARTESIAN_POINT ( 'NONE',  ( 98.24615118885414233, 215.9824982072973683, 3.021315404115420679E-15 ) ) ;
#87770 = CARTESIAN_POINT ( 'NONE',  ( 172.9450931783573537, 271.2952670478148320, 16.43454517436645546 ) ) ;
#87771 = EDGE_CURVE ( 'NONE', #58503, #58533, #30210, .T. ) ;
#87772 = VERTEX_POINT ( 'NONE', #6425 ) ;
#87773 = CARTESIAN_POINT ( 'NONE',  ( 76.57256817690921480, 57.91657040172975712, -16.10350934941853041 ) ) ;
#87774 = CARTESIAN_POINT ( 'NONE',  ( 83.57479903228094997, 42.82924647053130229, -5.872390686928415704 ) ) ;
#87775 = CARTESIAN_POINT ( 'NONE',  ( 176.8722193823187183, 288.7079821761982430, 11.35092617276139393 ) ) ;
#87776 = CARTESIAN_POINT ( 'NONE',  ( 184.5457051153594534, 294.3635293766698169, 10.03055039675435367 ) ) ;
#87777 = ORIENTED_EDGE ( 'NONE', *, *, #91424, .T. ) ;
#87778 = CARTESIAN_POINT ( 'NONE',  ( 171.9484922859593041, 258.9508083473583042, -13.76153770011480937 ) ) ;
#87779 = CARTESIAN_POINT ( 'NONE',  ( 68.22269823808483125, 69.38605919497339869, -4.074953496159504418 ) ) ;
#87780 = CARTESIAN_POINT ( 'NONE',  ( 160.4646087359858484, 258.1587684244410070, -17.17204240885691746 ) ) ;
#87781 = CARTESIAN_POINT ( 'NONE',  ( 206.5103405372297232, 270.6423507306794249, 2.445296693522686748 ) ) ;
#87782 = CARTESIAN_POINT ( 'NONE',  ( 149.3833831332874240, 271.9073859370555510, 11.40518020539810173 ) ) ;
#87783 = CARTESIAN_POINT ( 'NONE',  ( 33.79711566178269777, 196.9865022471903444, 10.00000000000009415 ) ) ;
#87784 = CARTESIAN_POINT ( 'NONE',  ( 164.2545401858843945, 246.1497863546213978, 2.275217130759496609 ) ) ;
#87785 = CARTESIAN_POINT ( 'NONE',  ( 75.51323141522172477, 65.35427051582675517, 13.87231131232226744 ) ) ;
#87786 = CARTESIAN_POINT ( 'NONE',  ( 168.1601509168907569, 255.5064425537701993, 14.08313907349351446 ) ) ;
#87787 = CARTESIAN_POINT ( 'NONE',  ( 164.4578252119609090, 245.7976863610386999, -6.211333091911165560 ) ) ;
#87788 = CARTESIAN_POINT ( 'NONE',  ( 122.0685591603289026, 241.2833772461660544, -9.188101187500095079 ) ) ;
#87789 = EDGE_LOOP ( 'NONE', ( #95700, #31091, #27646, #95028 ) ) ;
#87790 = CARTESIAN_POINT ( 'NONE',  ( 84.35801967554498049, 44.16480482089680493, -7.626279337594716878 ) ) ;
#87791 = DIRECTION ( 'NONE',  ( 0.5000000000000014433, -0.8660254037844378194, 0.000000000000000000 ) ) ;
#87792 = DIRECTION ( 'NONE',  ( -0.000000000000000000, -0.000000000000000000, -1.000000000000000000 ) ) ;
#87793 = CARTESIAN_POINT ( 'NONE',  ( 40.34888600819125770, 126.6204015641749834, -10.00000000000000000 ) ) ;
#87794 = CARTESIAN_POINT ( 'NONE',  ( 74.90473642350332284, 61.75549325437163617, 15.17546568179592725 ) ) ;
#87795 = CARTESIAN_POINT ( 'NONE',  ( 174.9640303183041112, 252.5332431885451854, 5.182172288090916012 ) ) ;
#87796 = ORIENTED_EDGE ( 'NONE', *, *, #80492, .T. ) ;
#87797 = CARTESIAN_POINT ( 'NONE',  ( 80.31886729598942054, 57.42767889257750369, -16.58902572440456780 ) ) ;
#87798 = EDGE_CURVE ( 'NONE', #94453, #73260, #28212, .T. ) ;
#87799 = CARTESIAN_POINT ( 'NONE',  ( 158.5026241661040558, 275.0849458030947972, -12.46164233742350902 ) ) ;
#87800 = CARTESIAN_POINT ( 'NONE',  ( 72.07793231134587586, 71.39460431499534820, 5.116661974763394127 ) ) ;
#87801 = CARTESIAN_POINT ( 'NONE',  ( 205.9334673742153257, 273.9597668594684023, -10.28447216160094158 ) ) ;
#87802 = CARTESIAN_POINT ( 'NONE',  ( 71.50240432004942193, 72.40933122983058468, 5.654570818603106787E-06 ) ) ;
#87803 = CARTESIAN_POINT ( 'NONE',  ( -32.57773935851065517, 93.92637809958223727, 43.89948692389421581 ) ) ;
#87804 = EDGE_CURVE ( 'NONE', #14885, #40695, #87925, .T. ) ;
#87805 = CARTESIAN_POINT ( 'NONE',  ( 67.74046153704668427, 68.49183975612825748, 5.712584250058917235 ) ) ;
#87806 = CARTESIAN_POINT ( 'NONE',  ( 54.73473692032377613, 214.6589784336661637, -6.496448406907675876E-16 ) ) ;
#87807 = AXIS2_PLACEMENT_3D ( 'NONE', #17255, #79102, #9686 ) ;
#87808 = B_SPLINE_CURVE_WITH_KNOTS ( 'NONE', 3,
 ( #25720, #79452, #79947, #88071, #15715, #32800, #72835, #78935, #3428, #64715, #46617, #95664, #10511, #10016, #40879, #9522, #41390, #40384, #1915, #46107, #87076, #33302, #72333, #71323, #56081, #41894, #77021, #71826, #64203, #33825, #2937 ),
 .UNSPECIFIED., .F., .F.,
 ( 4, 3, 3, 3, 3, 3, 3, 3, 3, 3, 4 ),
 ( 0.000000000000000000, 0.1333490885032290463, 0.3007194338854137228, 0.4699862290245038765, 0.5844252810809251741, 0.6686540514502686827, 0.7354980260655517021, 0.8028463152565618044, 0.8633854507757415808, 0.9437142632667480102, 1.000000000000000000 ),
 .UNSPECIFIED. ) ;
#87809 = CARTESIAN_POINT ( 'NONE',  ( 173.6395413452840728, 251.9775273180457873, 3.447188466571927457 ) ) ;
#87810 = EDGE_CURVE ( 'NONE', #27127, #81475, #15328, .T. ) ;
#87811 = B_SPLINE_SURFACE_WITH_KNOTS ( 'NONE', 3, 1, ( 
 ( #86483, #35083 ),
 ( #96436, #27000 ),
 ( #19428, #9424 ),
 ( #57884, #50284 ),
 ( #81237, #40299 ),
 ( #81727, #85988 ),
 ( #11811, #4182 ),
 ( #71241, #35588 ),
 ( #50777, #1834 ),
 ( #65987, #19905 ),
 ( #58376, #55010 ),
 ( #89352, #74104 ),
 ( #16516, #47411 ),
 ( #70717, #1332 ),
 ( #32214, #97410 ),
 ( #29972, #98898 ),
 ( #84225, #74617 ),
 ( #75101, #58857 ),
 ( #36072, #89826 ),
 ( #82237, #59356 ),
 ( #43675, #21872 ),
 ( #5679, #90834 ),
 ( #13778, #44656 ),
 ( #37074, #97900 ),
 ( #36568, #60849 ),
 ( #60353, #7163 ),
 ( #29480, #5190 ),
 ( #22372, #90332 ),
 ( #44165, #13306 ),
 ( #67475, #91312 ),
 ( #37557, #12813 ),
 ( #52758, #20402 ),
 ( #66973, #51271 ),
 ( #28475, #20909 ) ),
 .UNSPECIFIED., .T., .F., .F.,
 ( 4, 2, 2, 2, 2, 2, 2, 2, 2, 2, 2, 2, 2, 2, 2, 2, 4 ),
 ( 2, 2 ),
 ( 0.000000000000000000, 0.06250000000000000000, 0.1250000000000000000, 0.1875000000000000000, 0.2500000000000000000, 0.3125000000000000000, 0.3750000000000000000, 0.4375000000000000000, 0.5000000000000000000, 0.5625000000000000000, 0.6250000000000000000, 0.6875000000000000000, 0.7500000000000000000, 0.8125000000000000000, 0.8750000000000000000, 0.9375000000000000000, 1.000000000000000000 ),
 ( 0.000000000000000000, 1.000000000000000000 ),
 .UNSPECIFIED. ) ;
#87812 = CARTESIAN_POINT ( 'NONE',  ( 172.0338011489890278, 260.6545490261862597, 14.59499001995644640 ) ) ;
#87813 = CARTESIAN_POINT ( 'NONE',  ( 155.4155621527535800, 279.6985967190125848, -1.505547091306592478 ) ) ;
#87814 = CARTESIAN_POINT ( 'NONE',  ( 170.8463542321686077, 287.4393069310528972, -8.645854640182026429 ) ) ;
#87815 = CARTESIAN_POINT ( 'NONE',  ( 202.9881971861223917, 279.0611244672630278, -15.16231470264511927 ) ) ;
#87816 = CARTESIAN_POINT ( 'NONE',  ( 157.5084939801577093, 271.0392582902702543, -14.68761352887457861 ) ) ;
#87817 = CARTESIAN_POINT ( 'NONE',  ( 127.6706609892855369, 244.5177522451418497, -10.00000000000009592 ) ) ;
#87818 = CYLINDRICAL_SURFACE ( 'NONE', #14357, 16.60714546451156792 ) ;
#87819 = VERTEX_POINT ( 'NONE', #77311 ) ;
#87820 = CARTESIAN_POINT ( 'NONE',  ( 160.4170979800060479, 258.1363065642061088, -17.22270422867546102 ) ) ;
#87821 = CARTESIAN_POINT ( 'NONE',  ( -7.212535326543083158, 157.4548013555409796, -4.594050593750042211 ) ) ;
#87822 = CARTESIAN_POINT ( 'NONE',  ( 42.06911538997637479, 207.3464784336661353, 1.353441290958777327E-15 ) ) ;
#87823 = CARTESIAN_POINT ( 'NONE',  ( 23.65144817020273393, 15.78380873178787347, -6.180339887498949025 ) ) ;
#87824 = CARTESIAN_POINT ( 'NONE',  ( 85.68485941944548756, 48.66523437743575187, 11.91861461389293808 ) ) ;
#87825 = CARTESIAN_POINT ( 'NONE',  ( 66.04572084532792076, 69.25630126843506673, 0.2739672973347200835 ) ) ;
#87826 = CARTESIAN_POINT ( 'NONE',  ( 189.9211050898329347, 290.8589279105092942, -14.43444364813599634 ) ) ;
#87827 = CARTESIAN_POINT ( 'NONE',  ( 147.1249913145849177, 275.8190353104462815, 3.637773609013635223 ) ) ;
#87828 = CARTESIAN_POINT ( 'NONE',  ( 66.54213899643076502, 67.99313125863469054, -6.545993785947124444 ) ) ;
#87829 = CARTESIAN_POINT ( 'NONE',  ( 50.52223126882174853, 206.6427522451419065, 10.00000000000009237 ) ) ;
#87830 = CARTESIAN_POINT ( 'NONE',  ( 172.8951663193395234, 288.9549776225803157, 8.104654168245465584 ) ) ;
#87831 = CARTESIAN_POINT ( 'NONE',  ( 180.9259186355868394, 256.3478317398164563, 1.329846375023655547 ) ) ;
#87832 = DIRECTION ( 'NONE',  ( 0.000000000000000000, -1.000000000000000000, 0.000000000000000000 ) ) ;
#87833 = CARTESIAN_POINT ( 'NONE',  ( 73.27328646083023500, 70.16270934360544231, -9.274526489422589393 ) ) ;
#87834 =( BOUNDED_CURVE ( )  B_SPLINE_CURVE ( 2, ( #70128, #69641, #31129, #92973, #39713, #70641, #85394, #55420, #46845, #77767, #8352, #16938, #47824 ),
 .UNSPECIFIED., .F., .T. ) 
 B_SPLINE_CURVE_WITH_KNOTS ( ( 3, 2, 2, 2, 2, 2, 3 ),
 ( 0.1375000000000000111, 0.1400000000000000133, 0.1449999999999999900, 0.1499999999999999944, 0.1549999999999999989, 0.1600000000000000033, 0.1625000000000000056 ),
 .UNSPECIFIED. ) 
 CURVE ( )  GEOMETRIC_REPRESENTATION_ITEM ( )  RATIONAL_B_SPLINE_CURVE ( ( 0.9755282581475768211, 0.9755282581475768211, 1.000000000000000000, 0.9510565162951535312, 1.000000000000000000, 0.9510565162951535312, 1.000000000000000000, 0.9510565162951535312, 1.000000000000000000, 0.9510565162951535312, 1.000000000000000000, 0.9755282581475768211, 0.9755282581475768211 ) ) 
 REPRESENTATION_ITEM ( '' )  );
#87835 = ADVANCED_FACE ( 'NONE', ( #85974 ), #55976, .T. ) ;
#87836 = CARTESIAN_POINT ( 'NONE',  ( 37.33338606056913989, 202.3615022471903160, 5.000000000000046185 ) ) ;
#87837 = CARTESIAN_POINT ( 'NONE',  ( 185.0922654080720235, 294.3675542256470408, 9.847061582960922266 ) ) ;
#87838 = DIRECTION ( 'NONE',  ( 0.000000000000000000, 0.000000000000000000, 1.000000000000000000 ) ) ;
#87839 = CARTESIAN_POINT ( 'NONE',  ( -6.509410329615746171, 176.2369531367911293, -4.594050593750048428 ) ) ;
#87840 = CARTESIAN_POINT ( 'NONE',  ( 32.39518414388500389, 34.10171378149920685, 9.188101187500008038 ) ) ;
#87841 = EDGE_CURVE ( 'NONE', #85448, #80622, #74594, .T. ) ;
#87842 = CARTESIAN_POINT ( 'NONE',  ( 152.6615646578087819, 266.2294089801508221, 16.94722993326405813 ) ) ;
#87843 = CARTESIAN_POINT ( 'NONE',  ( 37.97865540203802937, 30.43085787977766188, -9.188101187500008038 ) ) ;
#87844 = CARTESIAN_POINT ( 'NONE',  ( 206.5479446040613141, 272.8954610772809133, 10.74757481123993230 ) ) ;
#87845 = FACE_OUTER_BOUND ( 'NONE', #85107, .T. ) ;
#87846 = CARTESIAN_POINT ( 'NONE',  ( 66.30954113569532637, 68.28728378170326607, 3.992301261007330737 ) ) ;
#87847 = CARTESIAN_POINT ( 'NONE',  ( 148.9322735291567597, 272.6887306911919495, -12.40988026045598858 ) ) ;
#87848 = CARTESIAN_POINT ( 'NONE',  ( 177.8071669554300058, 260.6696581013277410, -13.92674055003218747 ) ) ;
#87849 = CARTESIAN_POINT ( 'NONE',  ( 7.976297994771393896, 26.64646525600388571, -2.839279412974133887 ) ) ;
#87850 = CARTESIAN_POINT ( 'NONE',  ( 167.9901924881250181, 286.9604587259559594, 0.5049872151095315953 ) ) ;
#87851 = CARTESIAN_POINT ( 'NONE',  ( 17.79544559245429625, 15.98920272979925628, 7.433330006724137462 ) ) ;
#87852 = CARTESIAN_POINT ( 'NONE',  ( 207.1328285129854976, 271.8824124304944689, 9.368303624280315489 ) ) ;
#87853 = CARTESIAN_POINT ( 'NONE',  ( 152.8910811562359413, 278.3431035384439269, -4.654733895217889383 ) ) ;
#87854 = LINE ( 'NONE', #45880, #43702 ) ;
#87855 = CARTESIAN_POINT ( 'NONE',  ( 88.20990559483804816, 44.21161532246393477, -1.798209583089680041 ) ) ;
#87856 = ORIENTED_EDGE ( 'NONE', *, *, #71324, .T. ) ;
#87857 = CARTESIAN_POINT ( 'NONE',  ( 152.5564169041443847, 266.8265214178677525, 15.57863003859133499 ) ) ;
#87858 = CARTESIAN_POINT ( 'NONE',  ( 164.9971748156432056, 244.8635054444190757, -1.825016704039769788 ) ) ;
#87859 = LINE ( 'NONE', #64996, #63903 ) ;
#87860 = CARTESIAN_POINT ( 'NONE',  ( 87.34977546134365411, 44.90968568749347867, 6.842696035241847774 ) ) ;
#87861 = CARTESIAN_POINT ( 'NONE',  ( 155.4186054393023255, 261.4540742680644598, 17.05753227160644769 ) ) ;
#87862 = ORIENTED_EDGE ( 'NONE', *, *, #25590, .T. ) ;
#87863 = VERTEX_POINT ( 'NONE', #86971 ) ;
#87864 = CARTESIAN_POINT ( 'NONE',  ( 138.7947376353724849, 239.3932355074535963, -2.679491924311248496 ) ) ;
#87865 = CARTESIAN_POINT ( 'NONE',  ( 86.07940076415255248, 47.67293344237150166, 10.86953268328462308 ) ) ;
#87866 = ORIENTED_EDGE ( 'NONE', *, *, #94384, .T. ) ;
#87867 = CARTESIAN_POINT ( 'NONE',  ( 76.78470638831343820, 52.79280447672221044, 15.85451643790141141 ) ) ;
#87868 = DIRECTION ( 'NONE',  ( -0.000000000000000000, -0.000000000000000000, 1.000000000000000000 ) ) ;
#87869 = EDGE_LOOP ( 'NONE', ( #35067, #80885, #68608, #19659 ) ) ;
#87870 = CARTESIAN_POINT ( 'NONE',  ( 78.27822849507501246, 61.67779232024188474, -15.77509627637905432 ) ) ;
#87871 = DIRECTION ( 'NONE',  ( 0.4999999999999998890, -0.8660254037844385966, 0.000000000000000000 ) ) ;
#87873 = AXIS2_PLACEMENT_3D ( 'NONE', #48133, #1043, #85699 ) ;
#87872 = CARTESIAN_POINT ( 'NONE',  ( 16.78929260308981952, 21.64441083166260427, -10.00000000000000533 ) ) ;
#87874 = ORIENTED_EDGE ( 'NONE', *, *, #38388, .F. ) ;
#87875 = CARTESIAN_POINT ( 'NONE',  ( 173.6846226408814573, 267.2224573121649769, 16.82899224521884207 ) ) ;
#87876 = CARTESIAN_POINT ( 'NONE',  ( 169.1248369069356841, 276.0452466230211712, -15.48103994540444717 ) ) ;
#87877 = CARTESIAN_POINT ( 'NONE',  ( 151.3635996277190827, 275.1454279078836862, -8.423308477353403489 ) ) ;
#87878 = VERTEX_POINT ( 'NONE', #7920 ) ;
#87879 = CARTESIAN_POINT ( 'NONE',  ( 170.7362026651413203, 255.3656839902395177, -11.44183947388228084 ) ) ;
#87880 = VECTOR ( 'NONE', #44523, 1000.000000000000227 ) ;
#87881 = VERTEX_POINT ( 'NONE', #86467 ) ;
#87882 = EDGE_CURVE ( 'NONE', #85116, #43189, #69715, .T. ) ;
#87883 = EDGE_LOOP ( 'NONE', ( #79530, #27286, #25864, #92011 ) ) ;
#87884 = CARTESIAN_POINT ( 'NONE',  ( 157.0081533241564102, 266.1116096007127112, -16.83218197677382122 ) ) ;
#87885 = ORIENTED_EDGE ( 'NONE', *, *, #77903, .T. ) ;
#87886 = EDGE_CURVE ( 'NONE', #76398, #7306, #41906, .T. ) ;
#87887 = CARTESIAN_POINT ( 'NONE',  ( 162.1151829103941964, 273.8406652419924967, -15.84115298045961673 ) ) ;
#87888 = ORIENTED_EDGE ( 'NONE', *, *, #98974, .F. ) ;
#87889 = CARTESIAN_POINT ( 'NONE',  ( 78.01622611019826081, 227.3967562850346837, -4.648177544792955347E-16 ) ) ;
#87890 = EDGE_CURVE ( 'NONE', #53400, #18010, #96053, .T. ) ;
#87891 = CARTESIAN_POINT ( 'NONE',  ( 147.3528235038055811, 275.4244183831162900, 5.914741335832481184 ) ) ;
#87892 = CARTESIAN_POINT ( 'NONE',  ( 180.5791919176537874, 291.4317077338294553, -9.732688088917043956 ) ) ;
#87893 = DIRECTION ( 'NONE',  ( -0.000000000000000000, -0.000000000000000000, 1.000000000000000000 ) ) ;
#87894 = CARTESIAN_POINT ( 'NONE',  ( 152.8107382695299918, 265.9710327055011589, 16.32045346488711246 ) ) ;
#87895 = CARTESIAN_POINT ( 'NONE',  ( 48.92549481379852949, 97.87922363803308201, -10.00000000000000000 ) ) ;
#87896 = FACE_OUTER_BOUND ( 'NONE', #37978, .T. ) ;
#87897 = VECTOR ( 'NONE', #40210, 1000.000000000000000 ) ;
#87898 = ORIENTED_EDGE ( 'NONE', *, *, #17857, .T. ) ;
#87899 = DIRECTION ( 'NONE',  ( -1.000000000000000000, 0.000000000000000000, 0.000000000000000000 ) ) ;
#87900 = CARTESIAN_POINT ( 'NONE',  ( 16.63655203261577498, 31.64646525600389637, -2.839279412974133887 ) ) ;
#87901 = CARTESIAN_POINT ( 'NONE',  ( 164.8616299252405213, 245.0982760813026857, 1.544363874765093625 ) ) ;
#87902 = B_SPLINE_CURVE_WITH_KNOTS ( 'NONE', 3,
 ( #83437, #14504, #44387, #91042 ),
 .UNSPECIFIED., .F., .F.,
 ( 4, 4 ),
 ( 7.881068500304280180E-17, 0.004334768247277024505 ),
 .UNSPECIFIED. ) ;
#87904 = CARTESIAN_POINT ( 'NONE',  ( -19.65312891409030271, 93.06504152958497400, 10.00000000000000888 ) ) ;
#87903 = CARTESIAN_POINT ( 'NONE',  ( 77.54655217216907204, 49.73132247284985397, -15.46410396994591530 ) ) ;
#87906 = ORIENTED_EDGE ( 'NONE', *, *, #91374, .T. ) ;
#87905 = CARTESIAN_POINT ( 'NONE',  ( 16.73070718246250621, 56.29032694264133596, 59.99999999999999289 ) ) ;
#87907 = VERTEX_POINT ( 'NONE', #11435 ) ;
#87908 = CARTESIAN_POINT ( 'NONE',  ( 186.6673878995319455, 276.5074556901925007, 17.73048906045012529 ) ) ;
#87909 = CARTESIAN_POINT ( 'NONE',  ( 171.4605843149748523, 259.7787113614812142, -14.34284248236907722 ) ) ;
#87910 = CARTESIAN_POINT ( 'NONE',  ( 35.87562414229657293, 44.21091486745863364, 7.012934429366973338E-14 ) ) ;
#87911 = CARTESIAN_POINT ( 'NONE',  ( 179.0976092565113902, 278.1804918307850585, -17.48872506936735505 ) ) ;
#87912 = B_SPLINE_CURVE_WITH_KNOTS ( 'NONE', 3,
 ( #14318, #56297, #71532, #63411 ),
 .UNSPECIFIED., .F., .F.,
 ( 4, 4 ),
 ( 0.008452089677209189203, 0.01483908248598288238 ),
 .UNSPECIFIED. ) ;
#87913 = CARTESIAN_POINT ( 'NONE',  ( 160.5146108177758890, 252.6275340369041942, -16.06237538655383545 ) ) ;
#87914 = CARTESIAN_POINT ( 'NONE',  ( 190.7994525848730234, 261.9583232506778927, -0.5433290425362596876 ) ) ;
#87915 = ORIENTED_EDGE ( 'NONE', *, *, #82821, .T. ) ;
#87916 = CARTESIAN_POINT ( 'NONE',  ( 177.6785493476784552, 271.3070803369324153, -17.73189896442177016 ) ) ;
#87917 = EDGE_CURVE ( 'NONE', #16332, #19447, #818, .T. ) ;
#87918 = CARTESIAN_POINT ( 'NONE',  ( 164.3274319858398087, 246.0235340536434592, -1.770631424362269168 ) ) ;
#87919 = CARTESIAN_POINT ( 'NONE',  ( 19.85049821812290816, 182.2677522451418497, 10.00000000000009592 ) ) ;
#87920 = CARTESIAN_POINT ( 'NONE',  ( 105.6144235841895664, 219.5327760586659451, 1.948934522072302763E-15 ) ) ;
#87921 = CARTESIAN_POINT ( 'NONE',  ( 82.56903123641447451, 41.04314473016881237, -1.144421423674383265 ) ) ;
#87922 = B_SPLINE_CURVE_WITH_KNOTS ( 'NONE', 3,
 ( #48346, #94986, #87916, #10355, #3269, #80798 ),
 .UNSPECIFIED., .F., .F.,
 ( 4, 2, 4 ),
 ( 0.02063947560780285406, 0.02520718459488528046, 0.02977489358196770339 ),
 .UNSPECIFIED. ) ;
#87923 = CARTESIAN_POINT ( 'NONE',  ( 100.7282019964230244, 217.4155109091896065, 2.679491924311254714 ) ) ;
#87924 = CARTESIAN_POINT ( 'NONE',  ( 207.8616498235123231, 270.6200568910230118, 3.132900500943239130 ) ) ;
#87925 = B_SPLINE_CURVE_WITH_KNOTS ( 'NONE', 3,
 ( #74844, #52502, #82958, #59087, #83451, #14018, #68202, #92063, #90061, #20630, #99129, #14520, #45402, #61092, #5424, #76332, #6905, #44400, #46902, #16500, #62583, #55480, #23585, #39280, #24099, #54478, #9407, #25093, #8901, #69700, #308 ),
 .UNSPECIFIED., .F., .F.,
 ( 4, 3, 3, 3, 3, 3, 3, 3, 3, 3, 4 ),
 ( 0.000000000000000000, 0.1333490885032302675, 0.3007194338854343174, 0.4699862290245060414, 0.5844252810809307253, 0.6686540514502736787, 0.7354980260655518132, 0.8028463152565562533, 0.8633854507757269259, 0.9437142632667357978, 1.000000000000000000 ),
 .UNSPECIFIED. ) ;
#87926 = CARTESIAN_POINT ( 'NONE',  ( 22.06942799527072907, 192.7369531367911293, -4.594050593750048428 ) ) ;
#87927 = CARTESIAN_POINT ( 'NONE',  ( -27.42236680055714260, 166.5217562850347406, 1.224646799147364892E-15 ) ) ;
#87928 = ORIENTED_EDGE ( 'NONE', *, *, #34307, .T. ) ;
#87929 = ORIENTED_EDGE ( 'NONE', *, *, #74715, .T. ) ;
#87930 = CARTESIAN_POINT ( 'NONE',  ( 74.39670515357231295, 68.40078795844485171, -11.29786485497992921 ) ) ;
#87931 = CARTESIAN_POINT ( 'NONE',  ( 179.0484917649878298, 259.9789987921100192, 12.89662402083353854 ) ) ;
#87932 = CARTESIAN_POINT ( 'NONE',  ( 82.99579283926775020, 42.25164479318972610, 5.310766221622300165 ) ) ;
#87933 = CYLINDRICAL_SURFACE ( 'NONE', #53084, 10.00000000000010658 ) ;
#87934 = CARTESIAN_POINT ( 'NONE',  ( 207.8570869662935365, 270.6279599915536664, -5.669188455878507504 ) ) ;
#87935 = CARTESIAN_POINT ( 'NONE',  ( 182.4691726830119194, 284.2328283816569865, 14.94772914765149530 ) ) ;
#87936 = CARTESIAN_POINT ( 'NONE',  ( 6.599962460801562791, 15.76159833115048770, -9.594050593750004907 ) ) ;
#87937 = CARTESIAN_POINT ( 'NONE',  ( 46.18343024948246978, 185.2202760586659451, -5.415160957724236172E-17 ) ) ;
#87938 = CARTESIAN_POINT ( 'NONE',  ( 81.69914580506156199, 224.6427522451419065, 10.00000000000009237 ) ) ;
#87939 = VERTEX_POINT ( 'NONE', #44775 ) ;
#87940 = CARTESIAN_POINT ( 'NONE',  ( 81.65310433048475147, 42.64019311979919280, 7.560891536010023728 ) ) ;
#87941 = DIRECTION ( 'NONE',  ( 0.4999999999999992784, -0.8660254037844390407, 0.000000000000000000 ) ) ;
#87942 = EDGE_CURVE ( 'NONE', #46058, #32613, #92722, .T. ) ;
#87943 = CARTESIAN_POINT ( 'NONE',  ( -2.098180203030011182, 181.8464784336661353, 1.353441290958777327E-15 ) ) ;
#87944 = CARTESIAN_POINT ( 'NONE',  ( 71.94941146435354540, 134.4047874917408478, 22.50000000000001776 ) ) ;
#87945 = CARTESIAN_POINT ( 'NONE',  ( 151.4188942279983223, 268.3817773016460251, -14.77302265413830895 ) ) ;
#87946 = CARTESIAN_POINT ( 'NONE',  ( 186.4826759020093334, 282.7967963076828823, 16.16522040270928784 ) ) ;
#87947 = CARTESIAN_POINT ( 'NONE',  ( 192.8301672656986341, 296.6553483942417415, -13.40355799340913556 ) ) ;
#87948 = DIRECTION ( 'NONE',  ( 0.8660254037844395958, 0.4999999999999985567, 0.000000000000000000 ) ) ;
#87949 = CARTESIAN_POINT ( 'NONE',  ( 163.8040269124969939, 246.9300982336122559, 6.025552750865228013 ) ) ;
#87950 = CARTESIAN_POINT ( 'NONE',  ( 146.5046981847821428, 276.8934145268504494, 0.02269072295920678689 ) ) ;
#87951 = CARTESIAN_POINT ( 'NONE',  ( 207.6477529416552557, 270.9905371579805546, 7.447146952410988341 ) ) ;
#87952 = ORIENTED_EDGE ( 'NONE', *, *, #31778, .T. ) ;
#87953 = CARTESIAN_POINT ( 'NONE',  ( -8.638129123654804786, 172.4865022471903160, -10.00000000000009415 ) ) ;
#87954 = CARTESIAN_POINT ( 'NONE',  ( 16.68515570176661811, 168.8932355074535678, -2.679491924311248496 ) ) ;
#87955 = CARTESIAN_POINT ( 'NONE',  ( 119.4704829489755724, 239.7833772461660544, -9.188101187500095079 ) ) ;
#87956 = CARTESIAN_POINT ( 'NONE',  ( 15.22926075146606273, 30.83396525600389637, -2.839279412974133887 ) ) ;
#87957 = CARTESIAN_POINT ( 'NONE',  ( 75.15861105040980306, 67.07800672539922004, 12.69370984594314322 ) ) ;
#87958 = CARTESIAN_POINT ( 'NONE',  ( -3.019589773780833930, 24.80263534580897300, 10.00000000000000000 ) ) ;
#87959 = VECTOR ( 'NONE', #90944, 1000.000000000000114 ) ;
#87961 = CARTESIAN_POINT ( 'NONE',  ( 185.7606924044570462, 288.4259988650926516, 15.28553487407920386 ) ) ;
#87960 = CARTESIAN_POINT ( 'NONE',  ( 157.0848929289108469, 258.5679796760466047, 17.57466231005294688 ) ) ;
#87962 = CARTESIAN_POINT ( 'NONE',  ( -52.31886624268647523, 30.86069821571189919, 10.00000000000000000 ) ) ;
#87963 = ORIENTED_EDGE ( 'NONE', *, *, #43324, .T. ) ;
#87964 = CARTESIAN_POINT ( 'NONE',  ( 189.9217467546592104, 261.7193677635744962, -4.432260095178574666 ) ) ;
#87965 = CARTESIAN_POINT ( 'NONE',  ( 149.5390997184345281, 271.6376768999995761, -11.52989534384373016 ) ) ;
#87966 = FACE_OUTER_BOUND ( 'NONE', #5049, .T. ) ;
#87967 = CARTESIAN_POINT ( 'NONE',  ( 176.0908325915940793, 292.6123105786978726, -1.131283208944192431 ) ) ;
#87968 = CARTESIAN_POINT ( 'NONE',  ( 81.76698870106028494, 55.35579676949175365, -15.92943682233255132 ) ) ;
#87969 = ORIENTED_EDGE ( 'NONE', *, *, #75424, .T. ) ;
#87970 = CARTESIAN_POINT ( 'NONE',  ( 189.1378126190901980, 265.5228191422445434, 11.86773559132568323 ) ) ;
#87971 = CARTESIAN_POINT ( 'NONE',  ( 175.6080711066265110, 278.5854651567873930, 15.44675607434413855 ) ) ;
#87972 = CARTESIAN_POINT ( 'NONE',  ( 168.7748138323674709, 271.7814369042428098, -16.73069365461695668 ) ) ;
#87973 = CARTESIAN_POINT ( 'NONE',  ( 196.8684470336377501, 271.1649120511164028, 12.04039631205532679 ) ) ;
#87974 = CARTESIAN_POINT ( 'NONE',  ( 83.70712025649116583, 51.47757175601724811, -14.37168843583688194 ) ) ;
#87975 = CARTESIAN_POINT ( 'NONE',  ( 72.27803260052462520, 71.63036165027699553, -5.844549976855538453 ) ) ;
#87976 = CARTESIAN_POINT ( 'NONE',  ( 192.2943420783192323, 297.5834248427583475, 12.53393473147773562 ) ) ;
#87977 = ORIENTED_EDGE ( 'NONE', *, *, #40844, .F. ) ;
#87978 = DIRECTION ( 'NONE',  ( 0.000000000000000000, 0.000000000000000000, 1.000000000000000000 ) ) ;
#87979 = CARTESIAN_POINT ( 'NONE',  ( 11.39908531360041088, 14.78052372038638929, -10.00000000000000355 ) ) ;
#87980 = CARTESIAN_POINT ( 'NONE',  ( 174.0334219321320575, 272.1732822737818083, -16.75381009008792788 ) ) ;
#87981 = EDGE_LOOP ( 'NONE', ( #39336, #86598, #95590, #66858 ) ) ;
#87982 = CARTESIAN_POINT ( 'NONE',  ( 163.8309440367553975, 279.3941924811222179, 12.19413334027601081 ) ) ;
#87983 = CARTESIAN_POINT ( 'NONE',  ( 148.2352135776142177, 273.8960739431854563, -9.245976304249309052 ) ) ;
#87984 = CARTESIAN_POINT ( 'NONE',  ( 86.33534873861279380, 44.01410524257547507, -6.217298191315958178 ) ) ;
#87985 = ORIENTED_EDGE ( 'NONE', *, *, #39011, .F. ) ;
#87986 = CARTESIAN_POINT ( 'NONE',  ( 78.71329144889060103, 59.90182516230142795, 16.12092670603864875 ) ) ;
#87987 = PLANE ( 'NONE',  #54021 ) ;
#87988 = CARTESIAN_POINT ( 'NONE',  ( 191.0816511748900268, 299.6838671013740623, 7.311127128005925790 ) ) ;
#87989 = CARTESIAN_POINT ( 'NONE',  ( 80.18538372971539729, 51.32048852683736584, -15.03707885865879135 ) ) ;
#87990 = CARTESIAN_POINT ( 'NONE',  ( 73.43921776615482599, 70.07059797397528200, -9.512040028895288657 ) ) ;
#87991 = CARTESIAN_POINT ( 'NONE',  ( 189.6420494643790278, 300.2261056104030104, 3.258464925664200429 ) ) ;
#87992 = CARTESIAN_POINT ( 'NONE',  ( 203.5477091018662748, 278.0920214017542662, -16.09930363698006062 ) ) ;
#87993 = ORIENTED_EDGE ( 'NONE', *, *, #20478, .T. ) ;
#87994 = ORIENTED_EDGE ( 'NONE', *, *, #8879, .F. ) ;
#87995 = EDGE_CURVE ( 'NONE', #43017, #19180, #36560, .T. ) ;
#87996 = CARTESIAN_POINT ( 'NONE',  ( -22.42236680055709641, 157.8615022471902591, 0.000000000000000000 ) ) ;
#87997 = ORIENTED_EDGE ( 'NONE', *, *, #12012, .T. ) ;
#87998 = DIRECTION ( 'NONE',  ( -0.5000000000000006661, 0.8660254037844382635, -1.877843081442121204E-16 ) ) ;
#87999 = ORIENTED_EDGE ( 'NONE', *, *, #93507, .T. ) ;
#88000 = ADVANCED_FACE ( 'NONE', ( #91937, #68088 ), #36680, .T. ) ;
#88001 = LINE ( 'NONE', #17022, #2362 ) ;
#88002 = CARTESIAN_POINT ( 'NONE',  ( 202.9881971861223917, 279.0611244672630278, -15.16231470264511927 ) ) ;
#88003 = ORIENTED_EDGE ( 'NONE', *, *, #14715, .F. ) ;
#88004 = CARTESIAN_POINT ( 'NONE',  ( 186.1755760447797456, 282.4646021076670195, -16.83160945059842462 ) ) ;
#88005 = CARTESIAN_POINT ( 'NONE',  ( 81.98366634404946751, 41.07155685126597433, 3.381361522722056367 ) ) ;
#88006 = CARTESIAN_POINT ( 'NONE',  ( 160.5948787015109360, 254.3126484189558880, -15.26349502958301585 ) ) ;
#88007 = CARTESIAN_POINT ( 'NONE',  ( 158.6960675524883584, 274.7800521535589269, -12.92120065756460079 ) ) ;
#88008 = CARTESIAN_POINT ( 'NONE',  ( 192.9633865298379476, 296.4246058602058156, -11.85717392250713864 ) ) ;
#88009 = CARTESIAN_POINT ( 'NONE',  ( -11.40312891409031693, 78.77562236714182120, 59.97499999999998721 ) ) ;
#88010 = EDGE_CURVE ( 'NONE', #28615, #94399, #67589, .T. ) ;
#88011 = DIRECTION ( 'NONE',  ( 2.816764622163176999E-16, 1.626259812849726452E-16, -1.000000000000000000 ) ) ;
#88012 = CARTESIAN_POINT ( 'NONE',  ( 154.3430704429289619, 279.5595050419421455, 2.149449913245343069 ) ) ;
#88013 = CARTESIAN_POINT ( 'NONE',  ( 140.0925393287100178, 257.8149278399160949, -9.188101187500095079 ) ) ;
#88014 = CARTESIAN_POINT ( 'NONE',  ( 70.86275222855024936, 61.11972120349191329, -14.45886437636409916 ) ) ;
#88015 = CARTESIAN_POINT ( 'NONE',  ( 6.802937163926562114, 15.87878583063839066, -9.188101187500006262 ) ) ;
#88016 = ORIENTED_EDGE ( 'NONE', *, *, #34513, .T. ) ;
#88018 = ORIENTED_EDGE ( 'NONE', *, *, #92136, .F. ) ;
#88017 = CARTESIAN_POINT ( 'NONE',  ( 85.61207876059154387, 48.93336676014416753, -12.63415981529851173 ) ) ;
#88019 = CARTESIAN_POINT ( 'NONE',  ( -16.45508872280957036, 105.1413016814280894, 12.14368461262158583 ) ) ;
#88020 = FACE_OUTER_BOUND ( 'NONE', #55249, .T. ) ;
#88021 = CARTESIAN_POINT ( 'NONE',  ( 186.8123841630082040, 258.3999256946553942, 3.104652050626591553 ) ) ;
#88022 = CARTESIAN_POINT ( 'NONE',  ( 192.1545761101252481, 297.8255066008389349, 12.36758039018573108 ) ) ;
#88023 = CARTESIAN_POINT ( 'NONE',  ( 153.0319512166365712, 277.3779982626183482, 6.711626137538481807 ) ) ;
#88024 = CARTESIAN_POINT ( 'NONE',  ( -19.65312891409030271, 93.06504152958497400, 10.00000000000000888 ) ) ;
#88025 = CARTESIAN_POINT ( 'NONE',  ( 176.9795757823318638, 289.3634148552241641, -8.962721485982672931 ) ) ;
#88026 = CARTESIAN_POINT ( 'NONE',  ( 171.3220061097250948, 280.3562742204175038, 13.76436716405364891 ) ) ;
#88027 = CARTESIAN_POINT ( 'NONE',  ( 16.89228056887236917, 28.49103043416548786, -8.090169943749479842 ) ) ;
#88028 = CARTESIAN_POINT ( 'NONE',  ( 176.6970911207717165, 255.7224310037160535, -7.285259763286168422 ) ) ;
#88029 = ORIENTED_EDGE ( 'NONE', *, *, #73314, .F. ) ;
#88030 = CARTESIAN_POINT ( 'NONE',  ( 194.2154056360670040, 294.2560451561701029, -15.66696967429384557 ) ) ;
#88031 = CARTESIAN_POINT ( 'NONE',  ( 66.03170575037515277, 68.70116307984658022, -0.02812428434925291418 ) ) ;
#88032 = VECTOR ( 'NONE', #93534, 1000.000000000000000 ) ;
#88033 = ORIENTED_EDGE ( 'NONE', *, *, #73320, .T. ) ;
#88034 = CARTESIAN_POINT ( 'NONE',  ( 163.9104742396420704, 278.2281419285811239, 13.48933418416708996 ) ) ;
#88035 = VECTOR ( 'NONE', #13738, 1000.000000000000114 ) ;
#88036 = CARTESIAN_POINT ( 'NONE',  ( 200.9679874475659460, 267.7110922426995785, -2.589691348594355791 ) ) ;
#88037 = CARTESIAN_POINT ( 'NONE',  ( 192.0613504677270384, 297.9869781500409545, -10.79912279808309350 ) ) ;
#88038 = CARTESIAN_POINT ( 'NONE',  ( -11.87431992379006296, 23.49859753039504895, 10.00000000000000000 ) ) ;
#88039 = CARTESIAN_POINT ( 'NONE',  ( 162.9466247808429102, 248.4151622881552441, 11.25765811906727443 ) ) ;
#88041 = CARTESIAN_POINT ( 'NONE',  ( 87.94262069806690363, 44.22295065580315310, 2.813175635398602825 ) ) ;
#88040 = DIRECTION ( 'NONE',  ( 0.3715724127386967335, -0.6435822975543782354, -0.6691306063588567943 ) ) ;
#88042 = DIRECTION ( 'NONE',  ( 1.000000000000000000, 0.000000000000000000, 0.000000000000000000 ) ) ;
#88043 = ORIENTED_EDGE ( 'NONE', *, *, #35208, .F. ) ;
#88044 = B_SPLINE_SURFACE_WITH_KNOTS ( 'NONE', 3, 1, ( 
 ( #64512, #81741 ),
 ( #33615, #95470 ),
 ( #26023, #97423 ),
 ( #29982, #13315 ),
 ( #89841, #52282 ),
 ( #14783, #44176 ),
 ( #82747, #20414 ),
 ( #90846, #6691 ),
 ( #75113, #51282 ),
 ( #60861, #27992 ),
 ( #36082, #74119 ),
 ( #45179, #58871 ),
 ( #68475, #21398 ),
 ( #37084, #13789 ),
 ( #82251, #44665 ),
 ( #12824, #5689 ),
 ( #4713, #67485 ),
 ( #75601, #99404 ),
 ( #91824, #83223 ),
 ( #67988, #6188 ),
 ( #84234, #98908 ),
 ( #29489, #36579 ),
 ( #60364, #28485 ),
 ( #29007, #59367 ),
 ( #22384, #91323 ),
 ( #5201, #35599 ),
 ( #21883, #66984 ),
 ( #52769, #43686 ),
 ( #74627, #83729 ),
 ( #76118, #98415 ),
 ( #53282, #97911 ),
 ( #66497, #90343 ),
 ( #20922, #14292 ),
 ( #37568, #51805 ) ),
 .UNSPECIFIED., .T., .F., .F.,
 ( 4, 2, 2, 2, 2, 2, 2, 2, 2, 2, 2, 2, 2, 2, 2, 2, 4 ),
 ( 2, 2 ),
 ( 0.000000000000000000, 0.06250000000000000000, 0.1250000000000000000, 0.1875000000000000000, 0.2500000000000000000, 0.3125000000000000000, 0.3750000000000000000, 0.4375000000000000000, 0.5000000000000000000, 0.5625000000000000000, 0.6250000000000000000, 0.6875000000000000000, 0.7500000000000000000, 0.8125000000000000000, 0.8750000000000000000, 0.9375000000000000000, 1.000000000000000000 ),
 ( 0.000000000000000000, 1.000000000000000000 ),
 .UNSPECIFIED. ) ;
#88045 = CARTESIAN_POINT ( 'NONE',  ( 71.02243149778057330, 62.59254995015435696, -13.81378205064200415 ) ) ;
#88046 = CARTESIAN_POINT ( 'NONE',  ( 80.52088211617494551, 57.79340230469777850, 16.24652106404656138 ) ) ;
#88047 = DIRECTION ( 'NONE',  ( 0.000000000000000000, 0.000000000000000000, 1.000000000000000000 ) ) ;
#88048 = DIRECTION ( 'NONE',  ( -0.07193265315672570104, 0.9974094913373514615, 0.000000000000000000 ) ) ;
#88049 = CARTESIAN_POINT ( 'NONE',  ( 80.75062256945429340, 43.57525148357456857, -9.564875268673995734 ) ) ;
#88050 = DIRECTION ( 'NONE',  ( -0.000000000000000000, -0.000000000000000000, -1.000000000000000000 ) ) ;
#88051 = CARTESIAN_POINT ( 'NONE',  ( 202.3421728196210552, 280.1800714929709670, 16.85915999540957344 ) ) ;
#88052 = CARTESIAN_POINT ( 'NONE',  ( -13.97887943725652882, 171.9244531367911293, -4.594050593750046652 ) ) ;
#88053 = CARTESIAN_POINT ( 'NONE',  ( 102.6097905472235539, 239.2369531367911009, -4.594050593750048428 ) ) ;
#88054 = CARTESIAN_POINT ( 'NONE',  ( 88.18084728802688232, 44.43898297010869669, -4.607830584147581732 ) ) ;
#88055 = CARTESIAN_POINT ( 'NONE',  ( 2.966658798487924908, 25.21091486745858035, 1.000260061240931054E-15 ) ) ;
#88056 = CARTESIAN_POINT ( 'NONE',  ( 183.3634088509504352, 284.6525016221286251, -16.42631288611494256 ) ) ;
#88057 = EDGE_CURVE ( 'NONE', #69571, #14857, #96319, .T. ) ;
#88058 = CARTESIAN_POINT ( 'NONE',  ( 77.29821696115968166, 51.33252059662452638, 15.49558435715045945 ) ) ;
#88059 = CARTESIAN_POINT ( 'NONE',  ( 164.1651990362067011, 284.0577512603656487, 5.775159962432079297 ) ) ;
#88061 = FACE_OUTER_BOUND ( 'NONE', #76146, .T. ) ;
#88060 = DIRECTION ( 'NONE',  ( 0.6833540297821638632, -0.7300871660154544251, 0.000000000000000000 ) ) ;
#88062 = CARTESIAN_POINT ( 'NONE',  ( 161.7554271570718356, 250.4783770943820969, 12.69314527299759909 ) ) ;
#88063 = DIRECTION ( 'NONE',  ( -0.8660254037844378194, -0.5000000000000013323, -0.000000000000000000 ) ) ;
#88064 =( NAMED_UNIT ( * ) PLANE_ANGLE_UNIT ( ) SI_UNIT ( $, .RADIAN. ) );
#88065 = CARTESIAN_POINT ( 'NONE',  ( 81.58661138081841102, 53.69171030639404307, -15.56960227015292197 ) ) ;
#88066 = CARTESIAN_POINT ( 'NONE',  ( 79.25417529428960961, 46.14802681996067690, -13.25003384320201683 ) ) ;
#88067 = EDGE_CURVE ( 'NONE', #87383, #47538, #34260, .T. ) ;
#88068 = CARTESIAN_POINT ( 'NONE',  ( 73.34110816220993456, 69.83660377678546638, 9.135763230745686414 ) ) ;
#88069 = CARTESIAN_POINT ( 'NONE',  ( 47.75258065019424691, 204.5024278399160949, 9.188101187500095079 ) ) ;
#88070 = B_SPLINE_CURVE_WITH_KNOTS ( 'NONE', 3,
 ( #29584, #44276, #83824, #91926, #74221, #35692, #5783, #36671, #39148, #15355, #32063, #679, #47268, #99998, #70061, #7780, #16377, #85849, #86334, #55845, #40158, #16872, #38153, #31560, #46776, #62451, #77699, #47757, #94415, #63478, #92907, #93418, #46251, #78696, #71099, #62974, #86840, #23969, #78190, #70569, #9283, #23459, #53854, #8778, #84817, #54349, #85322, #1187, #92417, #77175 ),
 .UNSPECIFIED., .F., .F.,
 ( 4, 2, 2, 2, 2, 2, 2, 2, 2, 2, 2, 2, 2, 2, 2, 2, 2, 2, 2, 2, 2, 2, 2, 2, 4 ),
 ( 0.0002857323352533271284, 0.0007593487685542560112, 0.001232965201855184840, 0.001469773418505610114, 0.001588177526830845520, 0.001706581635156080492, 0.001943389851806547400, 0.002180198068457014308, 0.002653814501757891312, 0.003127430935058769183, 0.004074663801660423877, 0.005021896668262079873, 0.005495513101562916544, 0.005732321318213334446, 0.005850725426538501764, 0.005909927480701086290, 0.005969129534863669949, 0.006028331589026254475, 0.006087533643188839001, 0.006205937751514171118, 0.006442745968164699175, 0.006916362401465711920, 0.007153170618116217426, 0.007389978834766722064, 0.007863595268067727004 ),
 .UNSPECIFIED. ) ;
#88071 = CARTESIAN_POINT ( 'NONE',  ( 76.90757676121016573, 64.01000647765765450, -15.22607040013521029 ) ) ;
#88072 = EDGE_CURVE ( 'NONE', #90334, #38467, #97526, .T. ) ;
#88073 = CARTESIAN_POINT ( 'NONE',  ( 86.64296780859545777, 211.6423013555409796, -4.594050593750043987 ) ) ;
#88074 = CARTESIAN_POINT ( 'NONE',  ( 161.7767236248226084, 250.4414905302161287, -13.15904643207033153 ) ) ;
#88075 = CARTESIAN_POINT ( 'NONE',  ( 82.28500086614531028, 51.41804074472770480, -15.07771380314018295 ) ) ;
#88076 = FACE_OUTER_BOUND ( 'NONE', #22673, .T. ) ;
#88078 = DIRECTION ( 'NONE',  ( -0.6681572590663601430, 0.7440200784635646603, 0.000000000000000000 ) ) ;
#88077 = CARTESIAN_POINT ( 'NONE',  ( 41.19957572438558913, 58.46810036157969392, 10.00000000000000000 ) ) ;
#88079 = LINE ( 'NONE', #32808, #41228 ) ;
#88080 = CARTESIAN_POINT ( 'NONE',  ( 85.71737152317884068, 47.69513843210439319, -11.59802438570544858 ) ) ;
#88081 = VERTEX_POINT ( 'NONE', #52884 ) ;
#88082 = CARTESIAN_POINT ( 'NONE',  ( 22.55376741186237055, 15.94754757982089544, 5.678558825948272215 ) ) ;
#88083 = CARTESIAN_POINT ( 'NONE',  ( 75.51934661115031133, 226.6589784336661637, -6.496448406907676862E-16 ) ) ;
#88084 = CARTESIAN_POINT ( 'NONE',  ( 76.52245355297571905, 63.63306135144966902, 14.91177216842233477 ) ) ;
#88085 = B_SPLINE_CURVE_WITH_KNOTS ( 'NONE', 3,
 ( #72874, #64755, #19170, #18658, #4956, #43427, #35835, #3943, #26251, #50528 ),
 .UNSPECIFIED., .F., .F.,
 ( 4, 2, 2, 2, 4 ),
 ( 2.752498918913566419E-15, 0.0004302583884043699046, 0.0008605167768059872367, 0.001290775165207604623, 0.001721033553609222118 ),
 .UNSPECIFIED. ) ;
#88086 = DIRECTION ( 'NONE',  ( 0.000000000000000000, 0.000000000000000000, -1.000000000000000000 ) ) ;
#88087 = CARTESIAN_POINT ( 'NONE',  ( -30.09721120228516966, 94.48592239574253426, 12.47173656650774731 ) ) ;
#88088 = CARTESIAN_POINT ( 'NONE',  ( 201.7463482373744910, 281.2120699418204595, 16.24774024092229396 ) ) ;
#88089 = CARTESIAN_POINT ( 'NONE',  ( -28.04097607764120781, 24.82386083235215679, -10.00000000000000000 ) ) ;
#88090 = AXIS2_PLACEMENT_3D ( 'NONE', #2815, #49388, #71715 ) ;
#88091 = CARTESIAN_POINT ( 'NONE',  ( -19.65312891409034179, 93.06504152958504505, 0.000000000000000000 ) ) ;
#88092 = CARTESIAN_POINT ( 'NONE',  ( 72.54789201874723403, 71.57418066018787783, 5.334923225846505801 ) ) ;
#88093 = CARTESIAN_POINT ( 'NONE',  ( 127.8330407560430757, 234.6115022471901739, -5.000000000000041744 ) ) ;
#88094 = CARTESIAN_POINT ( 'NONE',  ( 157.2104826425669728, 258.3504519110855995, -16.92635148710569482 ) ) ;
#88095 = CARTESIAN_POINT ( 'NONE',  ( -19.65312891409030271, 93.06504152958497400, 10.00000000000000888 ) ) ;
#88096 = ORIENTED_EDGE ( 'NONE', *, *, #23354, .T. ) ;
#88097 = CARTESIAN_POINT ( 'NONE',  ( 85.33078790130267066, 46.00342033433972233, 9.479200480945582541 ) ) ;
#88098 = ORIENTED_EDGE ( 'NONE', *, *, #38040, .T. ) ;
#88099 = CARTESIAN_POINT ( 'NONE',  ( 202.6070187115982719, 279.7213449518906145, 15.56322169823762280 ) ) ;
#88100 = CARTESIAN_POINT ( 'NONE',  ( 207.4437983686434848, 270.9555910830893026, -0.9151573623704182259 ) ) ;
#88101 = CARTESIAN_POINT ( 'NONE',  ( -14.95575157760114671, 40.24948350530962671, 59.99999999999999289 ) ) ;
#88102 = ORIENTED_EDGE ( 'NONE', *, *, #38452, .F. ) ;
#88103 = CARTESIAN_POINT ( 'NONE',  ( -34.42581292930597670, 25.91608375674935161, 10.00000000000000000 ) ) ;
#88104 = ORIENTED_EDGE ( 'NONE', *, *, #6609, .T. ) ;
#88105 = DIRECTION ( 'NONE',  ( 0.6361630342459738685, -0.7715546603183444097, 0.000000000000000000 ) ) ;
#88106 = CARTESIAN_POINT ( 'NONE',  ( 169.7479376959777824, 249.8559926079458933, 3.422520443736486673 ) ) ;
#88107 = LINE ( 'NONE', #26742, #70374 ) ;
#88108 = CARTESIAN_POINT ( 'NONE',  ( 153.4495116231415750, 264.8646448025247082, -16.73555355292144498 ) ) ;
#88109 = ORIENTED_EDGE ( 'NONE', *, *, #40794, .F. ) ;
#88110 = CARTESIAN_POINT ( 'NONE',  ( 35.07444006175263240, 22.11110640527294535, -2.839279412974138328 ) ) ;
#88111 = CARTESIAN_POINT ( 'NONE',  ( 77.75401164654779507, 49.70357266593546797, -14.90152202399484160 ) ) ;
#88112 = EDGE_CURVE ( 'NONE', #98201, #64385, #43783, .T. ) ;
#88113 = CARTESIAN_POINT ( 'NONE',  ( -27.42236680055714260, 166.5217562850347406, 1.224646799147364892E-15 ) ) ;
#88114 = CARTESIAN_POINT ( 'NONE',  ( 28.46864935082050252, 149.7156766241961350, -37.49999999999994316 ) ) ;
#88115 = ORIENTED_EDGE ( 'NONE', *, *, #83453, .F. ) ;
#88116 = ORIENTED_EDGE ( 'NONE', *, *, #92565, .F. ) ;
#88117 = CARTESIAN_POINT ( 'NONE',  ( 184.3226795282388650, 274.5458599865910969, 17.66928848808302988 ) ) ;
#88118 =( BOUNDED_CURVE ( )  B_SPLINE_CURVE ( 2, ( #58404, #66512, #96463, #4211, #57913, #50310, #35108, #89377, #20939 ),
 .UNSPECIFIED., .F., .T. ) 
 B_SPLINE_CURVE_WITH_KNOTS ( ( 3, 2, 2, 2, 3 ),
 ( 0.9395161290322581182, 0.9408602150537634934, 0.9435483870967742437, 0.9462365591397849940, 0.9475806451612903691 ),
 .UNSPECIFIED. ) 
 CURVE ( )  GEOMETRIC_REPRESENTATION_ITEM ( )  RATIONAL_B_SPLINE_CURVE ( ( 0.9330127018922194093, 0.9330127018922194093, 1.000000000000000000, 0.8660254037844387076, 1.000000000000000000, 0.8660254037844387076, 1.000000000000000000, 0.9330127018922194093, 0.9330127018922194093 ) ) 
 REPRESENTATION_ITEM ( '' )  );
#88120 = CARTESIAN_POINT ( 'NONE',  ( 194.5298665426430489, 293.7113828889860656, -16.13302716640051315 ) ) ;
#88119 = CARTESIAN_POINT ( 'NONE',  ( 204.1780753366177237, 277.0001950557890495, 14.05599973203924158 ) ) ;
#88121 = DIRECTION ( 'NONE',  ( 0.000000000000000000, -1.000000000000000000, 0.000000000000000000 ) ) ;
#88122 = CARTESIAN_POINT ( 'NONE',  ( 154.8838596469624349, 262.3802811495310152, 18.07457254681616021 ) ) ;
#88123 = CARTESIAN_POINT ( 'NONE',  ( 48.32408078245681793, 82.80331927372955647, -10.00000000000000000 ) ) ;
#88124 = CARTESIAN_POINT ( 'NONE',  ( 187.4334564798314489, 291.4426959843206077, -14.06091351875603479 ) ) ;
#88125 = ADVANCED_FACE ( 'NONE', ( #83834 ), #36183, .T. ) ;
#88126 = CARTESIAN_POINT ( 'NONE',  ( 208.1496619281015512, 270.1212052926800880, -4.495150198885598414 ) ) ;
#88127 = EDGE_CURVE ( 'NONE', #50908, #26854, #15364, .T. ) ;
#88128 = CARTESIAN_POINT ( 'NONE',  ( -48.71813016832984289, 30.75580926756359901, -10.00000000000000000 ) ) ;
#88129 = CARTESIAN_POINT ( 'NONE',  ( 31.12960416526798824, 44.88710030135629836, 10.00000000000000000 ) ) ;
#88130 = CARTESIAN_POINT ( 'NONE',  ( 97.33288211261837830, 220.8768266524160140, 9.188101187500098632 ) ) ;
#88131 = ORIENTED_EDGE ( 'NONE', *, *, #4972, .T. ) ;
#88132 = CARTESIAN_POINT ( 'NONE',  ( -40.14225747417106760, 26.13077817479420872, 10.00000000000000000 ) ) ;
#88133 = CARTESIAN_POINT ( 'NONE',  ( 163.1014196328097512, 276.5356776938393750, -13.94729885495409860 ) ) ;
#88134 = ORIENTED_EDGE ( 'NONE', *, *, #10502, .T. ) ;
#88135 = ORIENTED_EDGE ( 'NONE', *, *, #33579, .T. ) ;
#88136 = CARTESIAN_POINT ( 'NONE',  ( 79.95079703291114015, 44.75747180391820024, -11.24531851929095083 ) ) ;
#88137 = DIRECTION ( 'NONE',  ( 0.4458072818673325943, 0.8951289669282637140, 0.000000000000000000 ) ) ;
#88138 = CARTESIAN_POINT ( 'NONE',  ( 82.70475790854101206, 41.40672355988375841, -3.064047408685779406 ) ) ;
#88139 = CARTESIAN_POINT ( 'NONE',  ( 206.8791291248445532, 272.3218326606039454, -10.16823074922856840 ) ) ;
#88140 = CARTESIAN_POINT ( 'NONE',  ( 207.1811052634604380, 270.9586164604430678, -3.621044357883208775 ) ) ;
#88141 = CARTESIAN_POINT ( 'NONE',  ( 89.59260651841245249, 222.5333772461660544, 9.188101187500095079 ) ) ;
#88142 = ORIENTED_EDGE ( 'NONE', *, *, #75275, .F. ) ;
#88143 = ORIENTED_EDGE ( 'NONE', *, *, #28918, .F. ) ;
#88144 = CARTESIAN_POINT ( 'NONE',  ( 20.94141239725287917, 35.71947554534623492, 10.00000000000000000 ) ) ;
#88145 = DIRECTION ( 'NONE',  ( -0.9756173257765569096, -0.2194785493951510180, 0.000000000000000000 ) ) ;
#88146 = ORIENTED_EDGE ( 'NONE', *, *, #30909, .T. ) ;
#88147 = CARTESIAN_POINT ( 'NONE',  ( 185.9608592076092464, 288.5956984647530703, 15.36535719480430018 ) ) ;
#88148 = CARTESIAN_POINT ( 'NONE',  ( 21.81709757609801770, 176.7365022471902307, 10.00000000000009948 ) ) ;
#88149 = CARTESIAN_POINT ( 'NONE',  ( 73.30483403957811106, 69.17932697374328654, -9.895411455429695025 ) ) ;
#88151 = LINE ( 'NONE', #38604, #85199 ) ;
#88150 = CARTESIAN_POINT ( 'NONE',  ( 138.2797325092426490, 241.4548013555409796, -4.594050593750042211 ) ) ;
#88152 = CARTESIAN_POINT ( 'NONE',  ( -0.9341114727035790821, 160.2677522451418213, -5.000000000000041744 ) ) ;
#88153 = CARTESIAN_POINT ( 'NONE',  ( 88.05492707984328149, 44.74075123808635368, 4.463746458969096054 ) ) ;
#88154 = ORIENTED_EDGE ( 'NONE', *, *, #23401, .T. ) ;
#88155 = CARTESIAN_POINT ( 'NONE',  ( 157.0482715255472215, 258.6314098073167997, 18.43444315619183271 ) ) ;
#88156 = CARTESIAN_POINT ( 'NONE',  ( 160.6010507955586490, 275.6504566167214989, 12.84439325828979861 ) ) ;
#88157 = CARTESIAN_POINT ( 'NONE',  ( 82.03757150437812129, 40.99183643444361991, -2.920132542340025950 ) ) ;
#88158 = CARTESIAN_POINT ( 'NONE',  ( 188.9774666975129662, 269.5299829227286068, 14.91052322670039132 ) ) ;
#88159 = CARTESIAN_POINT ( 'NONE',  ( 175.1187049791955701, 283.7737228748806615, 13.32334552399349548 ) ) ;
#88160 = CARTESIAN_POINT ( 'NONE',  ( 72.46511837996449401, 71.56249752072032777, 6.234640293157917235 ) ) ;
#88161 = VECTOR ( 'NONE', #48897, 1000.000000000000000 ) ;
#88162 = CARTESIAN_POINT ( 'NONE',  ( 198.8382651030371449, 282.3441860183548329, -16.97453155116460977 ) ) ;
#88163 = DIRECTION ( 'NONE',  ( -1.000000000000000000, 0.000000000000000000, 0.000000000000000000 ) ) ;
#88164 = CARTESIAN_POINT ( 'NONE',  ( 200.2631011806900005, 283.7811292041749311, 18.23377125296567058 ) ) ;
#88165 = CARTESIAN_POINT ( 'NONE',  ( 82.89553795050942142, 41.40690226224887738, 2.584278410276873217 ) ) ;
#88166 = CARTESIAN_POINT ( 'NONE',  ( 167.6693233113157646, 249.9456431551184039, 6.971576484633508208 ) ) ;
#88167 = CARTESIAN_POINT ( 'NONE',  ( 83.37296956034946049, 51.74080471427828343, 14.95189368521468154 ) ) ;
#88168 = CARTESIAN_POINT ( 'NONE',  ( 177.9794308749766856, 291.2700001626445214, -6.136377113293979058 ) ) ;
#88169 = B_SPLINE_CURVE_WITH_KNOTS ( 'NONE', 3,
 ( #92929, #93441, #15893, #16399, #6312, #63998, #47782, #72119, #57391, #78216, #25502, #17918, #95953, #80246, #70596, #48816 ),
 .UNSPECIFIED., .F., .F.,
 ( 4, 1, 2, 2, 2, 1, 2, 2, 4 ),
 ( 0.000000000000000000, 0.1249999999999958367, 0.1874999999999937550, 0.2499999999999916733, 0.4999999999999926725, 0.6249999999999928946, 0.6874999999999948930, 0.7499999999999967804, 1.000000000000000000 ),
 .UNSPECIFIED. ) ;
#88170 = CARTESIAN_POINT ( 'NONE',  ( 198.3697893717576051, 274.2502983357130120, 15.02126222074246797 ) ) ;
#88171 = AXIS2_PLACEMENT_3D ( 'NONE', #66738, #75870, #6449 ) ;
#88172 = EDGE_CURVE ( 'NONE', #61860, #6163, #92427, .T. ) ;
#88173 = CARTESIAN_POINT ( 'NONE',  ( 73.78779888375932217, 64.08313911669114304, -13.94799677262989768 ) ) ;
#88174 = CARTESIAN_POINT ( 'NONE',  ( 74.22098529628976848, 55.36760511359434389, 16.12280093334807063 ) ) ;
#88175 = DIRECTION ( 'NONE',  ( 0.2649596321166021728, -0.4589235447807153423, -0.8480480961564252906 ) ) ;
#88176 = EDGE_CURVE ( 'NONE', #18677, #69383, #42474, .T. ) ;
#88177 = CARTESIAN_POINT ( 'NONE',  ( 33.26462506102002692, 34.90829794293883026, 10.00000000000000355 ) ) ;
#88178 = CARTESIAN_POINT ( 'NONE',  ( 78.07878065217096264, 47.77350909806117585, 13.99880554328534110 ) ) ;
#88179 = CARTESIAN_POINT ( 'NONE',  ( 183.1223740192843081, 274.6153891519672356, 16.37435194274504369 ) ) ;
#88180 = CARTESIAN_POINT ( 'NONE',  ( 84.89744547285587828, 41.79037650531964943, -3.168800655305855967E-06 ) ) ;
#88181 = CARTESIAN_POINT ( 'NONE',  ( 87.56744345830549037, 43.91593491218741718, -2.248609772235193649 ) ) ;
#88182 = CARTESIAN_POINT ( 'NONE',  ( 20.58138070222249638, 176.5643266524160140, -9.188101187500093303 ) ) ;
#88183 = CARTESIAN_POINT ( 'NONE',  ( 82.98570375819691947, 51.14804373459350728, 14.38639528083483832 ) ) ;
#88184 = ORIENTED_EDGE ( 'NONE', *, *, #87995, .T. ) ;
#88185 = ADVANCED_FACE ( 'NONE', ( #62459 ), #24978, .T. ) ;
#88186 = CARTESIAN_POINT ( 'NONE',  ( 86.67787608365236451, 46.41355258656824390, 9.087135552152110662 ) ) ;
#88187 = CARTESIAN_POINT ( 'NONE',  ( 24.18060153781336297, 14.36477965099640564, 1.583844403245364907 ) ) ;
#88188 = CARTESIAN_POINT ( 'NONE',  ( 38.06444208900335013, 180.5327760586659736, 1.948934522072302763E-15 ) ) ;
#88189 = CARTESIAN_POINT ( 'NONE',  ( 87.29394575703194903, 46.02912284201620707, 8.718719511823859847 ) ) ;
#88190 = CARTESIAN_POINT ( 'NONE',  ( 147.4963928429778264, 275.1757489932608109, 4.929816573182678852 ) ) ;
#88191 = CARTESIAN_POINT ( 'NONE',  ( 32.15421140596747307, 42.65659080271453263, -1.878358725466461243E-16 ) ) ;
#88192 = CARTESIAN_POINT ( 'NONE',  ( 199.6026874660839781, 267.3423861812402720, -6.701379308517451783 ) ) ;
#88193 = CARTESIAN_POINT ( 'NONE',  ( 146.7434471017767521, 276.4798892723637209, 0.7354350123930684102 ) ) ;
#88194 = CARTESIAN_POINT ( 'NONE',  ( 149.0223506047763635, 272.5327126196219183, 12.70178612879041502 ) ) ;
#88195 = CARTESIAN_POINT ( 'NONE',  ( 182.5027709831066431, 280.4898292648059055, -16.09026386679935783 ) ) ;
#88196 = CARTESIAN_POINT ( 'NONE',  ( 169.9836960595253572, 273.3332435997890570, -17.42200768236145336 ) ) ;
#88197 = CARTESIAN_POINT ( 'NONE',  ( 86.80242440116035141, 45.86160641078058831, -8.224216122728513767 ) ) ;
#88198 = EDGE_CURVE ( 'NONE', #41047, #95263, #86346, .T. ) ;
#88199 = LINE ( 'NONE', #80586, #67731 ) ;
#88200 = EDGE_CURVE ( 'NONE', #4089, #100289, #4404, .T. ) ;
#88201 = CARTESIAN_POINT ( 'NONE',  ( 82.43887584100865240, 231.7365022471903160, 2.944929066748280225E-16 ) ) ;
#88202 = CARTESIAN_POINT ( 'NONE',  ( 75.24955243259913118, 53.08423708156048093, 16.48597916460597901 ) ) ;
#88203 = DIRECTION ( 'NONE',  ( -0.7911563084720435457, -0.6116140086401625764, 0.000000000000000000 ) ) ;
#88204 = CARTESIAN_POINT ( 'NONE',  ( 39.90439897628026955, 193.8458772461660544, 9.188101187500095079 ) ) ;
#88205 = CARTESIAN_POINT ( 'NONE',  ( 198.2114954873088948, 287.3346145022089786, 18.52864136173620935 ) ) ;
#88206 = VERTEX_POINT ( 'NONE', #14878 ) ;
#88207 = CARTESIAN_POINT ( 'NONE',  ( -18.15312891409030627, 78.77562236714182120, 13.81405534229504894 ) ) ;
#88208 = CARTESIAN_POINT ( 'NONE',  ( 190.5653282632609091, 300.5781646174276602, -5.775635208185608604 ) ) ;
#88209 = DIRECTION ( 'NONE',  ( -0.8660254037844387076, -0.4999999999999998890, -0.000000000000000000 ) ) ;
#88210 = EDGE_LOOP ( 'NONE', ( #90968, #78269, #87296, #28227 ) ) ;
#88211 = CARTESIAN_POINT ( 'NONE',  ( 171.3427733889341482, 286.5388357190055331, 7.606204075628364869 ) ) ;
#88212 = CARTESIAN_POINT ( 'NONE',  ( 206.9878665138179770, 272.1334939782196329, 6.566295309274049252 ) ) ;
#88213 = CARTESIAN_POINT ( 'NONE',  ( 147.1448590109090162, 275.7846234509833607, 6.573501232734778377 ) ) ;
#88214 = CARTESIAN_POINT ( 'NONE',  ( 33.34238925418374322, 21.11110640527294180, -2.839279412974138328 ) ) ;
#88215 = CARTESIAN_POINT ( 'NONE',  ( 188.3608790720148534, 265.1764494128112233, 10.74626820104000302 ) ) ;
#88216 = PLANE ( 'NONE',  #24666 ) ;
#88217 = CARTESIAN_POINT ( 'NONE',  ( 171.4196486961773189, 255.6818549069291748, 11.25747882315595305 ) ) ;
#88218 = EDGE_LOOP ( 'NONE', ( #25801, #88258, #29121 ) ) ;
#88219 = CARTESIAN_POINT ( 'NONE',  ( 18.76490627030545610, 13.76004757982088655, 5.678558825948272215 ) ) ;
#88220 = LINE ( 'NONE', #56755, #38728 ) ;
#88221 = CARTESIAN_POINT ( 'NONE',  ( 79.99999999999998579, 20.00000000000000000, -2.622423327744133559 ) ) ;
#88222 = EDGE_CURVE ( 'NONE', #93711, #17411, #85330, .T. ) ;
#88223 = ORIENTED_EDGE ( 'NONE', *, *, #90442, .F. ) ;
#88224 = CARTESIAN_POINT ( 'NONE',  ( 175.8939073520130592, 252.7054158260212375, 5.280091837693253964 ) ) ;
#88225 = CARTESIAN_POINT ( 'NONE',  ( 166.8902351030177726, 261.4103272712569606, 16.60908148647677862 ) ) ;
#88226 = CARTESIAN_POINT ( 'NONE',  ( 177.4659907304532851, 255.7405978883358557, -6.896888922040105285 ) ) ;
#88227 = CARTESIAN_POINT ( 'NONE',  ( 48.83428215874786815, 87.09189275153327969, -10.00000000000000000 ) ) ;
#88228 = VECTOR ( 'NONE', #23275, 1000.000000000000000 ) ;
#88229 = VERTEX_POINT ( 'NONE', #8785 ) ;
#88230 = ORIENTED_EDGE ( 'NONE', *, *, #540, .F. ) ;
#88231 = EDGE_CURVE ( 'NONE', #60917, #33333, #14235, .T. ) ;
#88233 = CYLINDRICAL_SURFACE ( 'NONE', #58853, 17.82106496071139645 ) ;
#88232 = CARTESIAN_POINT ( 'NONE',  ( 161.1061647010182583, 251.6029326557136585, -13.56144933775657613 ) ) ;
#88234 = CARTESIAN_POINT ( 'NONE',  ( 69.88883377749583303, 71.12950566994834389, -3.160072888935177460 ) ) ;
#88235 = VERTEX_POINT ( 'NONE', #55363 ) ;
#88236 = CARTESIAN_POINT ( 'NONE',  ( 35.65891684237409720, 42.36126292948898708, 6.180339887498949913 ) ) ;
#88237 = CARTESIAN_POINT ( 'NONE',  ( 175.4039180538638050, 286.4985578832265105, -12.71199677751706503 ) ) ;
#88238 = CARTESIAN_POINT ( 'NONE',  ( 72.74315697103594403, 57.58733809446825092, -16.30555998160541264 ) ) ;
#88239 = CARTESIAN_POINT ( 'NONE',  ( 77.91028351001615704, 61.39461664896379034, -16.15133184208620420 ) ) ;
#88240 = CARTESIAN_POINT ( 'NONE',  ( 157.8696211474012330, 257.2087905314882619, -17.27527248276125604 ) ) ;
#88242 = CARTESIAN_POINT ( 'NONE',  ( 113.7334117446687287, 224.2202760586659167, -5.415160957724236172E-17 ) ) ;
#88241 = VECTOR ( 'NONE', #64221, 1000.000000000000000 ) ;
#88243 = EDGE_CURVE ( 'NONE', #91866, #91566, #39157, .T. ) ;
#88244 = DIRECTION ( 'NONE',  ( 1.000000000000000000, 0.000000000000000000, 0.000000000000000000 ) ) ;
#88245 = EDGE_CURVE ( 'NONE', #85740, #73648, #30592, .T. ) ;
#88246 = CARTESIAN_POINT ( 'NONE',  ( 207.6172352878830907, 271.0433952848413810, 3.316653249540578496 ) ) ;
#88247 = ORIENTED_EDGE ( 'NONE', *, *, #73082, .T. ) ;
#88248 = EDGE_CURVE ( 'NONE', #73611, #28264, #40632, .T. ) ;
#88249 = CARTESIAN_POINT ( 'NONE',  ( 35.92184506804998279, 29.24335787977765477, -9.188101187500008038 ) ) ;
#88250 = FACE_BOUND ( 'NONE', #7986, .T. ) ;
#88251 = CARTESIAN_POINT ( 'NONE',  ( 71.76089672477446868, 70.71256120569563564, -7.122520486804837958 ) ) ;
#88252 = EDGE_CURVE ( 'NONE', #9589, #78857, #85857, .T. ) ;
#88253 = CARTESIAN_POINT ( 'NONE',  ( 74.00414925029257063, 213.5333772461660544, 9.188101187500095079 ) ) ;
#88254 = CARTESIAN_POINT ( 'NONE',  ( 73.77070425341645432, 68.39923094797843817, 10.98015304846415141 ) ) ;
#88255 = CARTESIAN_POINT ( 'NONE',  ( 151.2057546125658973, 268.7509459446807227, 15.78031848731319187 ) ) ;
#88256 = CARTESIAN_POINT ( 'NONE',  ( 198.3452313965520375, 287.1029771126029573, 18.55943827821351988 ) ) ;
#88257 = PLANE ( 'NONE',  #52770 ) ;
#88258 = ORIENTED_EDGE ( 'NONE', *, *, #1692, .T. ) ;
#88259 = CARTESIAN_POINT ( 'NONE',  ( 73.16301214023302180, 58.99354537464945025, -15.59469135662974537 ) ) ;
#88260 = CARTESIAN_POINT ( 'NONE',  ( 78.83027756516089823, 59.16041374580647272, 16.54524128708894537 ) ) ;
#88261 = ORIENTED_EDGE ( 'NONE', *, *, #69967, .T. ) ;
#88262 = CARTESIAN_POINT ( 'NONE',  ( 153.6323727466833873, 269.3172676078306154, -15.66543061290010641 ) ) ;
#88263 = CARTESIAN_POINT ( 'NONE',  ( 174.2197551875393629, 277.1311307515431395, -15.63619229037431069 ) ) ;
#88264 = CARTESIAN_POINT ( 'NONE',  ( 207.2167723318516153, 271.7370174712370954, -6.606038862010207957 ) ) ;
#88265 = LINE ( 'NONE', #34498, #35130 ) ;
#88266 = CARTESIAN_POINT ( 'NONE',  ( 180.4366689915419784, 271.0272158672133855, 17.24581807274774548 ) ) ;
#88267 = VECTOR ( 'NONE', #2206, 1000.000000000000114 ) ;
#88268 = PLANE ( 'NONE',  #69302 ) ;
#88269 = CARTESIAN_POINT ( 'NONE',  ( 75.52043138733441197, 65.40259152114373364, 13.85004969525200380 ) ) ;
#88270 = DIRECTION ( 'NONE',  ( -0.7646402761590023189, -0.6444573283588951318, 0.000000000000000000 ) ) ;
#88271 = ORIENTED_EDGE ( 'NONE', *, *, #35650, .F. ) ;
#88272 = CARTESIAN_POINT ( 'NONE',  ( 163.8947349411736525, 246.7729873192901664, -5.868803394723933309 ) ) ;
#88273 = CARTESIAN_POINT ( 'NONE',  ( 123.0160347675418677, 232.6423013555409796, -4.594050593750043987 ) ) ;
#88274 = ORIENTED_EDGE ( 'NONE', *, *, #59808, .F. ) ;
#88275 = CARTESIAN_POINT ( 'NONE',  ( 83.46551755975433196, 44.18061934712438443, -8.403307044377809731 ) ) ;
#88276 = CARTESIAN_POINT ( 'NONE',  ( 165.4781454232152953, 246.0304399151612245, -2.837517270351797016 ) ) ;
#88277 = CARTESIAN_POINT ( 'NONE',  ( 166.2786698706664765, 279.3007919285489606, -14.16120680810289301 ) ) ;
#88278 = CARTESIAN_POINT ( 'NONE',  ( 164.2851776226980860, 246.0967207574460929, 5.847738044744511754 ) ) ;
#88279 = CARTESIAN_POINT ( 'NONE',  ( 0.9806730298622799991, 159.8262482093458061, 3.021315404115420679E-15 ) ) ;
#88280 = CARTESIAN_POINT ( 'NONE',  ( 178.0312528307557898, 255.3900881702813024, 4.808504629698181709 ) ) ;
#88281 = VERTEX_POINT ( 'NONE', #23467 ) ;
#88282 = CARTESIAN_POINT ( 'NONE',  ( 80.21108484470566680, 57.40951183915923650, -16.59077246605596301 ) ) ;
#88283 = CARTESIAN_POINT ( 'NONE',  ( 158.2340186899420189, 275.5716318946143701, -12.34771995126616417 ) ) ;
#88285 = CARTESIAN_POINT ( 'NONE',  ( 72.05642296158499960, 71.36845324389531697, 5.149965714867518862 ) ) ;
#88284 = CYLINDRICAL_SURFACE ( 'NONE', #71069, 10.00000000000010658 ) ;
#88286 = CARTESIAN_POINT ( 'NONE',  ( 206.0316325540811704, 273.7897397804065918, -11.04223638802967322 ) ) ;
#88288 = CARTESIAN_POINT ( 'NONE',  ( 144.5855667544892924, 242.0327760586659451, 1.948934522072302763E-15 ) ) ;
#88287 = B_SPLINE_CURVE_WITH_KNOTS ( 'NONE', 3,
 ( #61806, #47115, #78034, #1029 ),
 .UNSPECIFIED., .F., .F.,
 ( 4, 4 ),
 ( 2.129127682876557597E-15, 0.004546946768845585782 ),
 .UNSPECIFIED. ) ;
#88289 = DIRECTION ( 'NONE',  ( -0.7715546603183375263, -0.6361630342459821952, 0.000000000000000000 ) ) ;
#88290 = CARTESIAN_POINT ( 'NONE',  ( -22.42236680055709641, 157.8615022471902591, 0.000000000000000000 ) ) ;
#88291 = CARTESIAN_POINT ( 'NONE',  ( 67.70493856312646130, 68.44720612190054965, 5.765748310548177713 ) ) ;
#88292 = CARTESIAN_POINT ( 'NONE',  ( 73.32782722540972031, 203.9548013555409796, -4.594050593750042211 ) ) ;
#88293 = CARTESIAN_POINT ( 'NONE',  ( 205.2937235227012707, 275.0678357141204629, -12.80017165135291535 ) ) ;
#88294 = CARTESIAN_POINT ( 'NONE',  ( 181.4632975752175525, 255.1188003790442167, 1.936479460681336695 ) ) ;
#88295 = CARTESIAN_POINT ( 'NONE',  ( 15.25129666230372827, 24.50829794293880326, -10.00000000000000355 ) ) ;
#88296 = CARTESIAN_POINT ( 'NONE',  ( 190.8138402884741254, 300.1477291634665789, 4.037153726988762514 ) ) ;
#88297 = CARTESIAN_POINT ( 'NONE',  ( 155.4093994093388176, 279.7353005465348019, -1.380077325180699921 ) ) ;
#88298 = CARTESIAN_POINT ( 'NONE',  ( 172.6200275220975300, 287.6579637919017500, -8.258093202231311381 ) ) ;
#88299 = VECTOR ( 'NONE', #16777, 1000.000000000000227 ) ;
#88300 = CARTESIAN_POINT ( 'NONE',  ( 202.7602807045765019, 279.4558873931827065, -15.90558713185497020 ) ) ;
#88301 = CARTESIAN_POINT ( 'NONE',  ( 193.5548866660658121, 288.5596665684437312, 16.05153972607462975 ) ) ;
#88302 = CARTESIAN_POINT ( 'NONE',  ( 143.1869494737568118, 240.1427522451417644, 1.119607411625061291E-15 ) ) ;
#88303 = CARTESIAN_POINT ( 'NONE',  ( 83.93867512875034720, 50.77184042243444395, -13.93002038390009467 ) ) ;
#88304 = VERTEX_POINT ( 'NONE', #54358 ) ;
#88306 = ADVANCED_FACE ( 'NONE', ( #15875 ), #34602, .F. ) ;
#88305 = CIRCLE ( 'NONE', #78566, 9.999999999999998224 ) ;
#88307 = CARTESIAN_POINT ( 'NONE',  ( 66.48112308386458835, 67.80287055615345082, -6.850275035659466383 ) ) ;
#88308 = CARTESIAN_POINT ( 'NONE',  ( 160.5099781893591455, 258.1706592185460067, -17.21824937912870013 ) ) ;
#88309 = CARTESIAN_POINT ( 'NONE',  ( -13.19395714113563045, 169.3149278399160949, -9.188101187500095079 ) ) ;
#88310 = CARTESIAN_POINT ( 'NONE',  ( 32.78649236710315762, 198.9244531367911293, -4.594050593750046652 ) ) ;
#88311 = CARTESIAN_POINT ( 'NONE',  ( 178.6233049832252107, 259.3218917414808971, -11.04666618235884279 ) ) ;
#88312 = CARTESIAN_POINT ( 'NONE',  ( 25.03708881625783889, 16.58380873178787240, 6.180339887498953466 ) ) ;
#88313 = CARTESIAN_POINT ( 'NONE',  ( 38.03703169759612734, 192.7677522451418781, 10.00000000000009592 ) ) ;
#88314 = CARTESIAN_POINT ( 'NONE',  ( 157.2104826425669728, 258.3504519110855995, -16.92635148710569482 ) ) ;
#88315 = CARTESIAN_POINT ( 'NONE',  ( 192.0881900057259486, 293.2991038262234156, -14.57190693698760775 ) ) ;
#88316 = CARTESIAN_POINT ( 'NONE',  ( 190.2648877593310317, 301.0985428348857340, -4.426259207433023590 ) ) ;
#88317 = CARTESIAN_POINT ( 'NONE',  ( 74.02679248361786790, 55.63944272452155815, -16.58679916994908865 ) ) ;
#88319 = CARTESIAN_POINT ( 'NONE',  ( 62.71875570545262946, 207.0177522451418497, -10.00000000000009592 ) ) ;
#88318 = CARTESIAN_POINT ( 'NONE',  ( 66.16250339235085676, 220.5530062829863027, -4.648177544792955347E-16 ) ) ;
#88320 = CARTESIAN_POINT ( 'NONE',  ( 180.8696061126360348, 256.1446004347802159, 1.863214197090637958 ) ) ;
#88321 = EDGE_CURVE ( 'NONE', #64907, #89705, #25026, .T. ) ;
#88322 = CARTESIAN_POINT ( 'NONE',  ( 204.6713671561005299, 276.1457885614869951, -12.94307097876490431 ) ) ;
#88323 = DIRECTION ( 'NONE',  ( 0.000000000000000000, -0.5247752241695049502, -0.8512408378936280329 ) ) ;
#88324 = B_SPLINE_CURVE_WITH_KNOTS ( 'NONE', 3,
 ( #39066, #18307, #48706, #78104 ),
 .UNSPECIFIED., .F., .F.,
 ( 4, 4 ),
 ( 0.005060962031092128451, 0.01063827492794387417 ),
 .UNSPECIFIED. ) ;
#88325 = EDGE_CURVE ( 'NONE', #28883, #42203, #28428, .T. ) ;
#88326 = CARTESIAN_POINT ( 'NONE',  ( 33.79711566178269777, 196.9865022471903160, 10.00000000000009237 ) ) ;
#88327 = FACE_OUTER_BOUND ( 'NONE', #3342, .T. ) ;
#88328 = CARTESIAN_POINT ( 'NONE',  ( 149.8050492866161392, 271.5723974896224604, -11.69608657949948061 ) ) ;
#88329 = CARTESIAN_POINT ( 'NONE',  ( -1.664820405372784862, 169.8458772461660544, 9.188101187500095079 ) ) ;
#88330 = CARTESIAN_POINT ( 'NONE',  ( 42.15419773769040290, 26.19860640527295814, 2.839279412974134775 ) ) ;
#88331 = CARTESIAN_POINT ( 'NONE',  ( 162.5088600558392500, 251.8859699354127883, 13.03670156802715674 ) ) ;
#88332 = CARTESIAN_POINT ( 'NONE',  ( 192.6470966816805230, 296.9724359471326807, 11.11268290051284424 ) ) ;
#88333 = CARTESIAN_POINT ( 'NONE',  ( 37.28583507901048932, 30.03085787977765975, 9.188101187500006262 ) ) ;
#88334 = CARTESIAN_POINT ( 'NONE',  ( 17.15438521794160920, 32.83705186507754092, 3.090169943749475401 ) ) ;
#88335 = CARTESIAN_POINT ( 'NONE',  ( 207.4826643481121664, 271.2764789897469768, 7.783310782367018454 ) ) ;
#88336 = CARTESIAN_POINT ( 'NONE',  ( 152.7043854946215049, 268.1552411151685078, 15.94764448997051964 ) ) ;
#88337 = CARTESIAN_POINT ( 'NONE',  ( 176.9081908142109398, 260.3210854900437425, -13.74092692686856587 ) ) ;
#88338 =( LENGTH_UNIT ( ) NAMED_UNIT ( * ) SI_UNIT ( .MILLI., .METRE. ) );
#88339 = CARTESIAN_POINT ( 'NONE',  ( 12.93244592517074487, 8.262165230724926701, -2.296566073217252530E-15 ) ) ;
#88340 = CARTESIAN_POINT ( 'NONE',  ( 153.2681147270651252, 277.6995928556744389, -5.735428835157149408 ) ) ;
#88341 = CARTESIAN_POINT ( 'NONE',  ( 19.81074232005190794, 13.29860640527291693, -2.839279412974138328 ) ) ;
#88342 = CARTESIAN_POINT ( 'NONE',  ( 157.9207213236967675, 258.7415897385611743, 16.78933168291549194 ) ) ;
#88343 = VECTOR ( 'NONE', #5610, 1000.000000000000000 ) ;
#88344 = CARTESIAN_POINT ( 'NONE',  ( 153.1373638848023120, 277.6226180988243755, -5.202466352909343783 ) ) ;
#88345 = CARTESIAN_POINT ( 'NONE',  ( 161.5515493166768977, 252.8315038724842623, 14.92355679770252053 ) ) ;
#88346 = CARTESIAN_POINT ( 'NONE',  ( 206.2313482792274328, 273.4438219973828268, -9.403385562213845361 ) ) ;
#88347 = ORIENTED_EDGE ( 'NONE', *, *, #7207, .T. ) ;
#88348 = CARTESIAN_POINT ( 'NONE',  ( 192.3401793061076717, 297.5040324353506094, 12.56432540404525611 ) ) ;
#88349 = CARTESIAN_POINT ( 'NONE',  ( 207.4826643481121664, 271.2764789897469768, 7.783310782367018454 ) ) ;
#88350 = VECTOR ( 'NONE', #23896, 1000.000000000000114 ) ;
#88351 = CARTESIAN_POINT ( 'NONE',  ( 45.34926676561319425, 66.39822172987334170, 10.00000000000000000 ) ) ;
#88352 = CARTESIAN_POINT ( 'NONE',  ( 87.11797949770195260, 45.31116807351030218, 7.029999331949805530 ) ) ;
#88353 = ORIENTED_EDGE ( 'NONE', *, *, #95552, .F. ) ;
#88354 = ORIENTED_EDGE ( 'NONE', *, *, #91521, .T. ) ;
#88355 = EDGE_CURVE ( 'NONE', #99043, #28862, #28468, .T. ) ;
#88357 = DIRECTION ( 'NONE',  ( 1.000000000000000000, 0.000000000000000000, 0.000000000000000000 ) ) ;
#88356 = CARTESIAN_POINT ( 'NONE',  ( -89.11465314115667979, 93.37593066204033221, -30.52142883766496695 ) ) ;
#88358 = CARTESIAN_POINT ( 'NONE',  ( 86.40526999274889874, 47.59822202186899176, 10.59880268136866555 ) ) ;
#88359 = VERTEX_POINT ( 'NONE', #27500 ) ;
#88360 = CARTESIAN_POINT ( 'NONE',  ( 77.55915319031737454, 56.41274902163431904, 16.17439937459049659 ) ) ;
#88361 = CARTESIAN_POINT ( 'NONE',  ( 174.6066048939933921, 262.0940252294753918, 15.79829227059981278 ) ) ;
#88362 = ORIENTED_EDGE ( 'NONE', *, *, #73932, .T. ) ;
#88363 = CARTESIAN_POINT ( 'NONE',  ( 68.81024624021658553, 64.23859217638603525, -11.91047422207082462 ) ) ;
#88364 = CARTESIAN_POINT ( 'NONE',  ( 88.49889760693197616, 43.86969135779091999, -0.01036396331279294640 ) ) ;
#88365 = EDGE_CURVE ( 'NONE', #5700, #93568, #74611, .T. ) ;
#88366 = ADVANCED_FACE ( 'NONE', ( #52752 ), #21379, .F. ) ;
#88367 = CARTESIAN_POINT ( 'NONE',  ( 80.48551130740291626, 43.60439347182430225, 9.783031566464561735 ) ) ;
#88368 = ORIENTED_EDGE ( 'NONE', *, *, #86915, .F. ) ;
#88369 = CARTESIAN_POINT ( 'NONE',  ( 174.4001821373126404, 267.7328157961984516, 16.40384357689936934 ) ) ;
#88370 = CARTESIAN_POINT ( 'NONE',  ( 166.2445671850063889, 273.7634225484549688, -16.23583275697997053 ) ) ;
#88371 = VECTOR ( 'NONE', #50838, 1000.000000000000000 ) ;
#88372 = CARTESIAN_POINT ( 'NONE',  ( -22.42236680055709641, 157.8615022471902591, 0.000000000000000000 ) ) ;
#88373 = B_SPLINE_CURVE_WITH_KNOTS ( 'NONE', 3,
 ( #43947, #13086, #50554, #72903 ),
 .UNSPECIFIED., .F., .F.,
 ( 4, 4 ),
 ( 0.04183888476990187816, 0.04887120950165264183 ),
 .UNSPECIFIED. ) ;
#88374 = ORIENTED_EDGE ( 'NONE', *, *, #47648, .F. ) ;
#88375 = EDGE_CURVE ( 'NONE', #48247, #68558, #82231, .T. ) ;
#88376 = CARTESIAN_POINT ( 'NONE',  ( -22.42236680055709641, 157.8615022471902591, 0.000000000000000000 ) ) ;
#88377 = CARTESIAN_POINT ( 'NONE',  ( 163.3706531435203146, 247.6807236201477735, 10.06957846017757241 ) ) ;
#88378 = EDGE_CURVE ( 'NONE', #47529, #2005, #52655, .T. ) ;
#88379 = ORIENTED_EDGE ( 'NONE', *, *, #16964, .F. ) ;
#88380 = CARTESIAN_POINT ( 'NONE',  ( 157.0111464366968619, 266.1057930065318260, -17.09359609089053222 ) ) ;
#88381 = AXIS2_PLACEMENT_3D ( 'NONE', #70213, #47415, #72250 ) ;
#88382 = ORIENTED_EDGE ( 'NONE', *, *, #54455, .T. ) ;
#88383 = CARTESIAN_POINT ( 'NONE',  ( 158.2450265141656018, 269.1956154815484297, 15.62383266220220968 ) ) ;
#88384 = ORIENTED_EDGE ( 'NONE', *, *, #63337, .T. ) ;
#88385 = CARTESIAN_POINT ( 'NONE',  ( 168.7684621475002302, 272.8101242616207855, 15.98675317345763958 ) ) ;
#88386 = CARTESIAN_POINT ( 'NONE',  ( 147.9364826856482864, 274.4134910258607079, 6.769466817982260132 ) ) ;
#88387 = CARTESIAN_POINT ( 'NONE',  ( -22.42236680055709641, 157.8615022471902591, 0.000000000000000000 ) ) ;
#88388 = CARTESIAN_POINT ( 'NONE',  ( -22.42236680055709641, 157.8615022471902591, 0.000000000000000000 ) ) ;
#88389 = CARTESIAN_POINT ( 'NONE',  ( 150.5287101026835330, 271.9236214347867531, -12.89083132144543775 ) ) ;
#88390 = CARTESIAN_POINT ( 'NONE',  ( 178.5528122206513046, 291.5498836112694221, 6.349106513625528692 ) ) ;
#88391 = CARTESIAN_POINT ( 'NONE',  ( 196.9892929991941912, 289.4515313087606501, -17.86022972575499068 ) ) ;
#88392 = ORIENTED_EDGE ( 'NONE', *, *, #29594, .T. ) ;
#88393 = CARTESIAN_POINT ( 'NONE',  ( 92.14326550588401687, 235.5530062829863027, -4.648177544792955347E-16 ) ) ;
#88394 = CARTESIAN_POINT ( 'NONE',  ( 29.15721111571870594, 19.76004757982090965, 5.678558825948272215 ) ) ;
#88395 = CARTESIAN_POINT ( 'NONE',  ( 164.7297297678022403, 245.3267338555121455, 3.020078936458732599 ) ) ;
#88396 = CARTESIAN_POINT ( 'NONE',  ( 48.74043828842092552, 100.0309547576005258, -10.00000000000000000 ) ) ;
#88397 = ORIENTED_EDGE ( 'NONE', *, *, #79289, .T. ) ;
#88398 = ORIENTED_EDGE ( 'NONE', *, *, #21839, .F. ) ;
#88399 = CARTESIAN_POINT ( 'NONE',  ( 190.4665781587570734, 300.7492048156811393, 6.617184385853465578 ) ) ;
#88400 = CARTESIAN_POINT ( 'NONE',  ( 69.46922245526401696, 62.68787098779524314, 13.82297688367849808 ) ) ;
#88401 = CARTESIAN_POINT ( 'NONE',  ( -22.42236680055709641, 157.8615022471902591, 0.000000000000000000 ) ) ;
#88402 = CARTESIAN_POINT ( 'NONE',  ( 122.4745085665788906, 241.5177522451418497, -10.00000000000009592 ) ) ;
#88403 = EDGE_CURVE ( 'NONE', #26239, #60221, #58850, .T. ) ;
#88404 = CARTESIAN_POINT ( 'NONE',  ( 199.2279464128285724, 285.5740698558083182, -17.12749070589345024 ) ) ;
#88405 = CARTESIAN_POINT ( 'NONE',  ( 190.4340612255839460, 300.8055257960429003, -1.331319038338205196 ) ) ;
#88406 = ORIENTED_EDGE ( 'NONE', *, *, #20350, .T. ) ;
#88407 = DIRECTION ( 'NONE',  ( 0.4999999999999998890, -0.8660254037844385966, 0.000000000000000000 ) ) ;
#88408 = DIRECTION ( 'NONE',  ( -0.000000000000000000, 0.000000000000000000, -1.000000000000000000 ) ) ;
#88410 = EDGE_CURVE ( 'NONE', #99877, #35455, #23572, .T. ) ;
#88409 = DIRECTION ( 'NONE',  ( -0.9008877160804935613, -0.4340522123146846045, 0.000000000000000000 ) ) ;
#88411 = CARTESIAN_POINT ( 'NONE',  ( 25.04665064082949755, 195.2677522451419350, -5.000000000000047962 ) ) ;
#88412 = CARTESIAN_POINT ( 'NONE',  ( 106.1553423657898492, 232.0958772461660260, -9.188101187500095079 ) ) ;
#88413 = CARTESIAN_POINT ( 'NONE',  ( 172.0728039219370658, 285.9831811572526021, 11.38650458882361427 ) ) ;
#88414 = CARTESIAN_POINT ( 'NONE',  ( -16.10531488956837975, 22.89493580087430402, 10.00000000000000000 ) ) ;
#88415 = CARTESIAN_POINT ( 'NONE',  ( 162.4777017143181581, 249.2273608642169904, 10.60452504456504919 ) ) ;
#88416 = CARTESIAN_POINT ( 'NONE',  ( 30.27021345494340565, 176.0327760586659736, 1.948934522072303157E-15 ) ) ;
#88417 = VECTOR ( 'NONE', #75915, 999.9999999999998863 ) ;
#88418 = CARTESIAN_POINT ( 'NONE',  ( 161.4726291907278721, 250.9681975403669867, 14.52346149734912117 ) ) ;
#88419 = ORIENTED_EDGE ( 'NONE', *, *, #16284, .F. ) ;
#88420 = ORIENTED_EDGE ( 'NONE', *, *, #51502, .T. ) ;
#88421 = CARTESIAN_POINT ( 'NONE',  ( 186.4151829245328429, 260.6633168624404675, -5.822087422882750829 ) ) ;
#88422 = SHAPE_REPRESENTATION ( 'Lead Screw Acme Drive Shaft', ( #68784 ), #59069 ) ;
#88423 = CARTESIAN_POINT ( 'NONE',  ( 87.88902802526534686, 43.91876200309240375, 0.4180276961671919311 ) ) ;
#88424 = AXIS2_PLACEMENT_3D ( 'NONE', #75616, #36098, #75130 ) ;
#88425 = CARTESIAN_POINT ( 'NONE',  ( 75.96002837510272343, 51.45078221087327108, 16.17316520771503008 ) ) ;
#88426 = DIRECTION ( 'NONE',  ( 1.000000000000000000, 0.000000000000000000, 0.000000000000000000 ) ) ;
#88427 = CARTESIAN_POINT ( 'NONE',  ( 207.5785076975260779, 271.1104734389944042, -6.824813054587777650 ) ) ;
#88428 = CARTESIAN_POINT ( 'NONE',  ( 182.5044606565503784, 284.2441587155593652, 14.95203780250641046 ) ) ;
#88429 = CARTESIAN_POINT ( 'NONE',  ( 166.6595125297302502, 251.3695113782756323, 10.25274148534845864 ) ) ;
#88430 = CARTESIAN_POINT ( 'NONE',  ( 39.47103917862304456, 205.8464784336661637, 1.353441290958777525E-15 ) ) ;
#88431 = CARTESIAN_POINT ( 'NONE',  ( 86.10144160763246646, 220.5177522451418497, -10.00000000000009592 ) ) ;
#88432 = ORIENTED_EDGE ( 'NONE', *, *, #4915, .T. ) ;
#88433 = CARTESIAN_POINT ( 'NONE',  ( 83.52367447683917590, 46.08189511659875848, 10.61866891795677681 ) ) ;
#88434 = EDGE_CURVE ( 'NONE', #1543, #43165, #23853, .T. ) ;
#88435 = CARTESIAN_POINT ( 'NONE',  ( -70.92467617367975663, 45.40763453331954480, 10.00000000000000000 ) ) ;
#88436 = CARTESIAN_POINT ( 'NONE',  ( 68.66220828135105592, 64.65574856808412108, -12.15835882835606618 ) ) ;
#88437 = CARTESIAN_POINT ( 'NONE',  ( 151.3999564459286375, 268.4145785023736153, -15.40574304386609050 ) ) ;
#88438 = AXIS2_PLACEMENT_3D ( 'NONE', #90874, #41342, #2887 ) ;
#88439 = CARTESIAN_POINT ( 'NONE',  ( 79.62821684406628719, 47.63998313237675575, 14.03196863946704909 ) ) ;
#88440 = CARTESIAN_POINT ( 'NONE',  ( 193.2140586456748679, 295.9904290195353269, -12.67640480829088823 ) ) ;
#88441 = CARTESIAN_POINT ( 'NONE',  ( -110.0000000000000000, 15.00000000000000000, 59.99999999999999289 ) ) ;
#88442 = CARTESIAN_POINT ( 'NONE',  ( 204.7986527064648214, 275.9253235211867263, 14.74587861556245905 ) ) ;
#88443 = EDGE_CURVE ( 'NONE', #18151, #10695, #17492, .T. ) ;
#88444 = CARTESIAN_POINT ( 'NONE',  ( 191.7247331938518187, 298.5700163710982338, -9.650650827884682315 ) ) ;
#88445 = CARTESIAN_POINT ( 'NONE',  ( 207.6727254509676186, 270.9472835030587703, 7.315149605389819953 ) ) ;
#88446 = ORIENTED_EDGE ( 'NONE', *, *, #96175, .F. ) ;
#88447 = AXIS2_PLACEMENT_3D ( 'NONE', #17208, #55197, #9123 ) ;
#88448 = ADVANCED_FACE ( 'NONE', ( #77583 ), #33802, .T. ) ;
#88449 = CARTESIAN_POINT ( 'NONE',  ( 207.8060684685902686, 270.7163266217015689, 2.015725026008670540 ) ) ;
#88450 = CARTESIAN_POINT ( 'NONE',  ( -3.297639133650789756, 182.2365022471903444, 2.944929066748280225E-16 ) ) ;
#88451 = CARTESIAN_POINT ( 'NONE',  ( 81.87359138893998534, 41.32955797152818889, 5.976920566253458134 ) ) ;
#88452 = CARTESIAN_POINT ( 'NONE',  ( 121.9063529450018137, 235.0643266524159856, -9.188101187500093303 ) ) ;
#88453 = CARTESIAN_POINT ( 'NONE',  ( 21.16812676580727270, 15.14754757982089650, -5.678558825948276656 ) ) ;
#88454 = CARTESIAN_POINT ( 'NONE',  ( 74.86089102438639031, 67.20426264302339803, 12.49187069351280499 ) ) ;
#88455 = CARTESIAN_POINT ( 'NONE',  ( 46.16860155800336685, 185.9155109091895781, 2.679491924311254714 ) ) ;
#88457 = CARTESIAN_POINT ( 'NONE',  ( 185.6554113515731217, 288.0628275752804370, 14.84040072038121139 ) ) ;
#88456 = CARTESIAN_POINT ( 'NONE',  ( 81.74030608389443842, 41.67103928136101842, -5.586802174944530464 ) ) ;
#88458 = LINE ( 'NONE', #87962, #51348 ) ;
#88459 = ORIENTED_EDGE ( 'NONE', *, *, #48506, .T. ) ;
#88460 = CARTESIAN_POINT ( 'NONE',  ( 190.9061255863007318, 299.9878863388391892, 7.497146773253707153 ) ) ;
#88461 = CARTESIAN_POINT ( 'NONE',  ( 149.4171629335945681, 271.8488776066536730, -11.42564036194071520 ) ) ;
#88462 = CARTESIAN_POINT ( 'NONE',  ( 183.7496303464618279, 290.0633936972313904, 13.69834534244574442 ) ) ;
#88463 = CARTESIAN_POINT ( 'NONE',  ( 176.3202518409931656, 292.2088383860199770, -1.100976535451413385 ) ) ;
#88464 = CARTESIAN_POINT ( 'NONE',  ( 81.76809963683952276, 55.60016907699685618, -15.96690463567013474 ) ) ;
#88465 = VERTEX_POINT ( 'NONE', #40549 ) ;
#88466 = CARTESIAN_POINT ( 'NONE',  ( 74.50030574182822818, 64.90152822149880762, -14.20405048683398874 ) ) ;
#88467 = FACE_OUTER_BOUND ( 'NONE', #88218, .T. ) ;
#88468 = CARTESIAN_POINT ( 'NONE',  ( 39.00902500372484383, 91.81115952553612658, 59.99999999999999289 ) ) ;
#88469 = CARTESIAN_POINT ( 'NONE',  ( 83.69031307077386828, 42.59536443435012387, 5.155235521226168238 ) ) ;
#88470 = CARTESIAN_POINT ( 'NONE',  ( 79.53253147591188110, 51.45198067062761993, 15.17816704916131521 ) ) ;
#88471 = CARTESIAN_POINT ( 'NONE',  ( 179.4408063581041688, 277.4340371255875652, 17.62723233342114071 ) ) ;
#88472 = DIRECTION ( 'NONE',  ( 0.4386133837897754351, 0.6599160945941884293, 0.6100238090894790632 ) ) ;
#88473 = CARTESIAN_POINT ( 'NONE',  ( 192.2185419806677942, 297.7147144631093170, 12.45868041609393728 ) ) ;
#88474 = ORIENTED_EDGE ( 'NONE', *, *, #73488, .F. ) ;
#88475 = ADVANCED_FACE ( 'NONE', ( #2079 ), #41043, .T. ) ;
#88476 = CARTESIAN_POINT ( 'NONE',  ( 190.9415060515185587, 280.7361723716825850, 16.66172594339581181 ) ) ;
#88477 = CARTESIAN_POINT ( 'NONE',  ( 5.452216952852307230, 26.08080186712590631, -3.090169943749475845 ) ) ;
#88478 = CARTESIAN_POINT ( 'NONE',  ( 174.0797739608361780, 272.0896664596502887, -17.07181625714556361 ) ) ;
#88479 = ORIENTED_EDGE ( 'NONE', *, *, #51905, .F. ) ;
#88480 = CARTESIAN_POINT ( 'NONE',  ( 163.9610465543719329, 279.7500988940785192, 12.43876487773592920 ) ) ;
#88481 = CARTESIAN_POINT ( 'NONE',  ( 147.7467138384290308, 274.7421803109381813, -9.190172068879620682 ) ) ;
#88482 = PLANE ( 'NONE',  #46760 ) ;
#88483 = ORIENTED_EDGE ( 'NONE', *, *, #73774, .F. ) ;
#88484 = CARTESIAN_POINT ( 'NONE',  ( 78.92848498041493599, 59.73641368792644357, 16.49589861780994227 ) ) ;
#88485 = CARTESIAN_POINT ( 'NONE',  ( 185.4400636248849139, 291.0517812546900700, 12.13220115290137358 ) ) ;
#88486 = AXIS2_PLACEMENT_3D ( 'NONE', #99778, #61253, #30370 ) ;
#88487 = ORIENTED_EDGE ( 'NONE', *, *, #42310, .F. ) ;
#88488 = CARTESIAN_POINT ( 'NONE',  ( 76.84355992005671965, 52.38483315033376186, -15.78702513624113557 ) ) ;
#88489 = AXIS2_PLACEMENT_3D ( 'NONE', #8953, #87535, #78372 ) ;
#88490 = CARTESIAN_POINT ( 'NONE',  ( 183.5502601116926940, 258.9811193475696314, -5.834672144206265010 ) ) ;
#88491 = ORIENTED_EDGE ( 'NONE', *, *, #93410, .T. ) ;
#88492 = ORIENTED_EDGE ( 'NONE', *, *, #98473, .T. ) ;
#88493 = CARTESIAN_POINT ( 'NONE',  ( 176.9703162662242164, 260.2192451074442374, 12.27184398422452993 ) ) ;
#88494 = ORIENTED_EDGE ( 'NONE', *, *, #86987, .T. ) ;
#88495 = CARTESIAN_POINT ( 'NONE',  ( -19.65312891409030271, 93.06504152958497400, 177.5919119679930134 ) ) ;
#88496 = ORIENTED_EDGE ( 'NONE', *, *, #57578, .F. ) ;
#88497 = CARTESIAN_POINT ( 'NONE',  ( 28.29029450517493061, 115.7140298976778325, 59.99999999999999289 ) ) ;
#88498 = CARTESIAN_POINT ( 'NONE',  ( 202.7602807045765019, 279.4558873931827065, -15.90558713185497020 ) ) ;
#88499 = ORIENTED_EDGE ( 'NONE', *, *, #23936, .F. ) ;
#88500 = CARTESIAN_POINT ( 'NONE',  ( 182.8485886489254426, 280.3539150357451604, -16.11020329633530679 ) ) ;
#88501 = CARTESIAN_POINT ( 'NONE',  ( 82.03343428350656552, 41.08618529242319539, 3.321173257777776389 ) ) ;
#88502 = CARTESIAN_POINT ( 'NONE',  ( 162.9152754634673101, 255.8478433609669480, -14.94487196607794566 ) ) ;
#88503 = DIRECTION ( 'NONE',  ( 0.4999999999999998890, -0.8660254037844385966, 0.000000000000000000 ) ) ;
#88504 = CARTESIAN_POINT ( 'NONE',  ( 193.1569697810063531, 296.0893098336876506, -13.02398914535779539 ) ) ;
#88505 = CARTESIAN_POINT ( 'NONE',  ( 152.6692142062575499, 266.2161595735824449, -16.77985299603479419 ) ) ;
#88506 = CARTESIAN_POINT ( 'NONE',  ( 38.65784837781280459, 56.65029301956751340, -10.00000000000000000 ) ) ;
#88507 = CARTESIAN_POINT ( 'NONE',  ( 18.59950357648009955, 34.23654200823202842, 1.583844403245363353 ) ) ;
#88508 = CARTESIAN_POINT ( 'NONE',  ( 139.4158702080621879, 260.4869531367911009, 4.594050593750046652 ) ) ;
#88509 = ORIENTED_EDGE ( 'NONE', *, *, #10509, .T. ) ;
#88510 = CARTESIAN_POINT ( 'NONE',  ( 70.47390418687882629, 61.30276010542613108, -14.81569727497708833 ) ) ;
#88511 = EDGE_CURVE ( 'NONE', #28623, #27644, #46542, .T. ) ;
#88512 = ORIENTED_EDGE ( 'NONE', *, *, #42459, .F. ) ;
#88513 = VECTOR ( 'NONE', #66798, 1000.000000000000114 ) ;
#88515 = ORIENTED_EDGE ( 'NONE', *, *, #41602, .T. ) ;
#88514 = CARTESIAN_POINT ( 'NONE',  ( 199.9111308183154279, 270.2641321296042065, 9.500731247801665447 ) ) ;
#88516 = AXIS2_PLACEMENT_3D ( 'NONE', #82143, #36477, #53545 ) ;
#88517 = CARTESIAN_POINT ( 'NONE',  ( 46.88368875251780565, 110.3874725885333135, -10.00000000000000000 ) ) ;
#88518 = CARTESIAN_POINT ( 'NONE',  ( -8.295327404871391863, 176.0177522451419350, 5.000000000000046185 ) ) ;
#88519 = DIRECTION ( 'NONE',  ( 0.5000000000000048850, -0.8660254037844358210, 0.000000000000000000 ) ) ;
#88520 = CARTESIAN_POINT ( 'NONE',  ( 157.3938364985311011, 279.9930687026446776, -6.917094818336486206 ) ) ;
#88521 = CARTESIAN_POINT ( 'NONE',  ( 81.38451658133408273, 39.76220097505215989, 0.000000000000000000 ) ) ;
#88522 = CIRCLE ( 'NONE', #85236, 14.99999999999967848 ) ;
#88523 = CARTESIAN_POINT ( 'NONE',  ( 43.53831125515428369, 65.97156238185917232, 10.00000000000000000 ) ) ;
#88524 = CARTESIAN_POINT ( 'NONE',  ( 76.44099679799769831, 51.64620055149545408, -16.15625289873146286 ) ) ;
#88525 = CARTESIAN_POINT ( 'NONE',  ( 88.28491662655248717, 43.90562524633402575, -2.137378875048265403 ) ) ;
#88526 = ORIENTED_EDGE ( 'NONE', *, *, #21938, .F. ) ;
#88527 = CARTESIAN_POINT ( 'NONE',  ( 185.1132493422790617, 273.1213101841942148, -16.83739034747381069 ) ) ;
#88528 = CARTESIAN_POINT ( 'NONE',  ( 66.28466101247255438, 68.84525821111240873, 0.1138578521233850477 ) ) ;
#88529 = VERTEX_POINT ( 'NONE', #88224 ) ;
#88530 = CARTESIAN_POINT ( 'NONE',  ( 163.7274143833883784, 277.7048757494857227, 13.04941950082464430 ) ) ;
#88531 = CARTESIAN_POINT ( 'NONE',  ( 201.3079779175387500, 267.1163987143520444, -2.193808737881617787 ) ) ;
#88532 = CARTESIAN_POINT ( 'NONE',  ( 204.2538229384546469, 276.8689963608560447, -15.05174826659082221 ) ) ;
#88533 = CARTESIAN_POINT ( 'NONE',  ( 190.6094661480870798, 300.5017155583701083, 4.598210453186021951 ) ) ;
#88534 = CARTESIAN_POINT ( 'NONE',  ( 203.0507839702407580, 278.9527209772879814, 16.21318481136342626 ) ) ;
#88536 = CARTESIAN_POINT ( 'NONE',  ( 88.33437046889027044, 43.98075787490867583, 2.428164790499226733 ) ) ;
#88535 = CARTESIAN_POINT ( 'NONE',  ( 82.35285118013293015, 53.50770157854819331, -15.77620284334257938 ) ) ;
#88537 = CARTESIAN_POINT ( 'NONE',  ( 167.1864846243946658, 248.1417588236094787, 6.437963532893948404 ) ) ;
#88538 = VERTEX_POINT ( 'NONE', #3098 ) ;
#88539 = CARTESIAN_POINT ( 'NONE',  ( 74.52678402073020436, 61.66496649313184975, -15.10502237438445228 ) ) ;
#88540 = CARTESIAN_POINT ( 'NONE',  ( 80.39194534802405201, 57.98788175658641109, 16.25790314543759152 ) ) ;
#88541 = CARTESIAN_POINT ( 'NONE',  ( 73.65091262424760998, 65.48395239458849915, -13.12340454139720514 ) ) ;
#88542 = CARTESIAN_POINT ( 'NONE',  ( 82.29734961797254300, 53.60383310410945512, 15.81226994477781211 ) ) ;
#88543 = CARTESIAN_POINT ( 'NONE',  ( 80.80860232633280305, 43.61757695342358687, -9.575079427039360880 ) ) ;
#88544 = LINE ( 'NONE', #43367, #98405 ) ;
#88545 = CARTESIAN_POINT ( 'NONE',  ( -15.35952475613307655, 102.2482863741581980, 44.42918405269885795 ) ) ;
#88546 = CARTESIAN_POINT ( 'NONE',  ( 5.696048431029936410, 186.3464784336661637, 1.353441290958777525E-15 ) ) ;
#88547 = CARTESIAN_POINT ( 'NONE',  ( 105.9931361504627603, 225.8768266524159856, -9.188101187500091527 ) ) ;
#88548 = CARTESIAN_POINT ( 'NONE',  ( 154.8579861482817535, 262.4250953638155011, -17.69813260923097786 ) ) ;
#88549 = CARTESIAN_POINT ( 'NONE',  ( 88.16744270275496831, 44.54586846255803323, -4.939063992914634937 ) ) ;
#88550 = CARTESIAN_POINT ( 'NONE',  ( 182.6933049510233218, 257.5106189887609958, -2.311194929639305951 ) ) ;
#88551 = DIRECTION ( 'NONE',  ( 0.000000000000000000, 0.000000000000000000, 1.000000000000000000 ) ) ;
#88552 = AXIS2_PLACEMENT_3D ( 'NONE', #98431, #66511, #35612 ) ;
#88553 = CYLINDRICAL_SURFACE ( 'NONE', #66824, 16.60714546451156792 ) ;
#88554 = AXIS2_PLACEMENT_3D ( 'NONE', #31133, #54422, #85 ) ;
#88555 = LINE ( 'NONE', #19121, #53347 ) ;
#88556 = CARTESIAN_POINT ( 'NONE',  ( 148.2670916631250861, 273.8408594794321971, -7.980554973576580835 ) ) ;
#88557 = CARTESIAN_POINT ( 'NONE',  ( 181.6650930950966085, 291.4988380269174968, 9.336250461819773250 ) ) ;
#88558 = B_SPLINE_CURVE_WITH_KNOTS ( 'NONE', 3,
 ( #57809, #11251, #96364, #3641 ),
 .UNSPECIFIED., .F., .F.,
 ( 4, 4 ),
 ( 1.014933693205114626E-16, 0.0002129429434441837334 ),
 .UNSPECIFIED. ) ;
#88559 = CARTESIAN_POINT ( 'NONE',  ( 89.87110602656373715, 45.06299687293669365, 0.3596699001693225983 ) ) ;
#88560 = CARTESIAN_POINT ( 'NONE',  ( 164.2092127378751059, 246.2282957975508282, -5.762401283578112654 ) ) ;
#88561 = CARTESIAN_POINT ( 'NONE',  ( 0.2927578493243047641, 177.6427522451419350, -10.00000000000009592 ) ) ;
#88562 = EDGE_CURVE ( 'NONE', #77615, #55413, #71978, .T. ) ;
#88563 = CARTESIAN_POINT ( 'NONE',  ( 75.51089968197061353, 55.97360561932201506, -16.15470048074736198 ) ) ;
#88564 = DIRECTION ( 'NONE',  ( 0.5000000000000014433, -0.8660254037844378194, 0.000000000000000000 ) ) ;
#88565 = EDGE_CURVE ( 'NONE', #734, #62639, #99683, .T. ) ;
#88566 = VECTOR ( 'NONE', #58670, 1000.000000000000114 ) ;
#88568 = EDGE_CURVE ( 'NONE', #51782, #97333, #28863, .T. ) ;
#88567 = CYLINDRICAL_SURFACE ( 'NONE', #82403, 70.00000000000002842 ) ;
#88569 = EDGE_CURVE ( 'NONE', #90851, #84918, #59741, .T. ) ;
#88570 = CARTESIAN_POINT ( 'NONE',  ( 82.93520977470207356, 212.5643266524159856, -9.188101187500093303 ) ) ;
#88571 = CARTESIAN_POINT ( 'NONE',  ( 207.2337123599961899, 271.7076764818092443, -5.443417788256701861 ) ) ;
#88572 = CARTESIAN_POINT ( 'NONE',  ( 73.11370943405387379, 57.30880053450761125, 15.89862119264240370 ) ) ;
#88573 = FACE_OUTER_BOUND ( 'NONE', #21745, .T. ) ;
#88575 = CARTESIAN_POINT ( 'NONE',  ( 199.7269368322551202, 284.7097930968712376, 17.25965714184168931 ) ) ;
#88574 = CARTESIAN_POINT ( 'NONE',  ( 84.59307794881090103, 43.06915618060124729, -6.352897038551593489 ) ) ;
#88576 = CARTESIAN_POINT ( 'NONE',  ( 75.58531661750802755, 65.25623013732912625, 14.34312269817976215 ) ) ;
#88577 = CARTESIAN_POINT ( 'NONE',  ( 175.5673309417393568, 269.5851035110758289, -16.45774993793282448 ) ) ;
#88578 = CARTESIAN_POINT ( 'NONE',  ( 27.35361640444819287, 37.83396525600391413, -2.839279412974133887 ) ) ;
#88579 = CARTESIAN_POINT ( 'NONE',  ( 44.85937643310610667, 116.8208962945185050, -10.00000000000000000 ) ) ;
#88580 = CARTESIAN_POINT ( 'NONE',  ( 74.86122976112790184, 57.66712160362105521, 16.46677789332469999 ) ) ;
#88581 = EDGE_LOOP ( 'NONE', ( #45326, #49966, #14546, #88931 ) ) ;
#88582 = CARTESIAN_POINT ( 'NONE',  ( 14.99289142922413021, 26.84336893147755276, -7.433330006724137462 ) ) ;
#88583 = CARTESIAN_POINT ( 'NONE',  ( 69.94448162217048548, 217.3149278399160664, -9.188101187500095079 ) ) ;
#88584 = VECTOR ( 'NONE', #12690, 1000.000000000000114 ) ;
#88585 = CARTESIAN_POINT ( 'NONE',  ( 169.2047444088227053, 288.5477631478519243, -1.125125296904627925 ) ) ;
#88586 = DIRECTION ( 'NONE',  ( 1.000000000000000000, 0.000000000000000000, 0.000000000000000000 ) ) ;
#88587 = CARTESIAN_POINT ( 'NONE',  ( 191.6956933185365131, 288.0999053561845926, -15.81058546843402191 ) ) ;
#88588 = CARTESIAN_POINT ( 'NONE',  ( 86.70421956006907749, 47.09494090442339598, 10.43848816880117525 ) ) ;
#88589 = CARTESIAN_POINT ( 'NONE',  ( 193.4121261747727942, 288.4174338016593424, 16.05890728405906032 ) ) ;
#88590 = CARTESIAN_POINT ( 'NONE',  ( 175.4967466201937611, 291.2628096033125189, 6.560984766252938805 ) ) ;
#88591 = CARTESIAN_POINT ( 'NONE',  ( 131.6579862894243433, 233.4865022471901455, 1.119607411625061291E-15 ) ) ;
#88592 = CARTESIAN_POINT ( 'NONE',  ( 204.8385597977314490, 275.8562024115307167, -12.64672659107585240 ) ) ;
#88593 = CARTESIAN_POINT ( 'NONE',  ( 75.03955294907601115, 53.26399608549274234, 16.03606609946628581 ) ) ;
#88594 = EDGE_LOOP ( 'NONE', ( #79236, #99938, #6562, #7451 ) ) ;
#88595 = CARTESIAN_POINT ( 'NONE',  ( 85.73923958617189101, 47.08247690321802281, 10.46103602312257586 ) ) ;
#88596 = VERTEX_POINT ( 'NONE', #43031 ) ;
#88597 = CARTESIAN_POINT ( 'NONE',  ( 202.8211298556536804, 279.3504935719197988, 17.07914446815911447 ) ) ;
#88598 = CARTESIAN_POINT ( 'NONE',  ( 32.30839531297598910, 123.0650415295850593, 60.00000000000000000 ) ) ;
#88599 = LINE ( 'NONE', #21505, #80807 ) ;
#88600 = ORIENTED_EDGE ( 'NONE', *, *, #75168, .T. ) ;
#88601 = CARTESIAN_POINT ( 'NONE',  ( 77.27195188805879411, 63.42260127183214991, -15.13583386105102058 ) ) ;
#88602 = ORIENTED_EDGE ( 'NONE', *, *, #61502, .F. ) ;
#88603 = CARTESIAN_POINT ( 'NONE',  ( 192.1581366030953859, 291.7909651536984370, 14.80011484029171953 ) ) ;
#88604 = CARTESIAN_POINT ( 'NONE',  ( 167.5369157106011073, 247.4367840998064310, 3.630136079718237152 ) ) ;
#88605 = CARTESIAN_POINT ( 'NONE',  ( 152.7045549149684405, 246.7202760586659736, -5.415160957724236172E-17 ) ) ;
#88606 = CARTESIAN_POINT ( 'NONE',  ( 153.2283961777204695, 265.2476279883323400, -17.66880461074566000 ) ) ;
#88607 = ORIENTED_EDGE ( 'NONE', *, *, #25559, .T. ) ;
#88608 = CARTESIAN_POINT ( 'NONE',  ( 29.64555348686940661, 32.51421378149921537, -9.188101187500004485 ) ) ;
#88609 = CARTESIAN_POINT ( 'NONE',  ( 73.61114153562050433, 60.42089198535372674, -15.30486817249622256 ) ) ;
#88610 = CARTESIAN_POINT ( 'NONE',  ( 164.5588179998277383, 274.5918845762219576, 14.68862726419591169 ) ) ;
#88611 = DIRECTION ( 'NONE',  ( 0.4999999999999992784, -0.8660254037844390407, 0.000000000000000000 ) ) ;
#88612 = ORIENTED_EDGE ( 'NONE', *, *, #82386, .T. ) ;
#88613 = ORIENTED_EDGE ( 'NONE', *, *, #95791, .T. ) ;
#88614 = CARTESIAN_POINT ( 'NONE',  ( -115.0954152546898257, 78.37593066204033221, -30.52142883766496695 ) ) ;
#88616 = CARTESIAN_POINT ( 'NONE',  ( 148.3253847707240141, 273.7398928553401447, -9.074433450356286457 ) ) ;
#88615 = CARTESIAN_POINT ( 'NONE',  ( 164.1259971043086239, 246.3724295028720519, 5.761669507629934905 ) ) ;
#88617 = CARTESIAN_POINT ( 'NONE',  ( 85.76129479494518648, 48.67511999704337455, -11.90588009047172235 ) ) ;
#88618 = CARTESIAN_POINT ( 'NONE',  ( 169.9469112398214747, 250.9785751410766750, -8.718312767540300712 ) ) ;
#88619 = CARTESIAN_POINT ( 'NONE',  ( 45.11483101423404918, 69.99284853207299761, -10.00000000000000000 ) ) ;
#88620 = LINE ( 'NONE', #97195, #33923 ) ;
#88621 = CARTESIAN_POINT ( 'NONE',  ( 207.4789536975254691, 271.2829060250925295, -4.960982614616589181 ) ) ;
#88622 = CARTESIAN_POINT ( 'NONE',  ( 166.5034556664195691, 265.5931899439500512, 16.54637507192525447 ) ) ;
#88623 = CARTESIAN_POINT ( 'NONE',  ( 180.9962514683335257, 255.6518059654043782, 5.281628127585873855 ) ) ;
#88624 = CARTESIAN_POINT ( 'NONE',  ( 99.30858933894288043, 218.9548013555409511, -4.594050593750042211 ) ) ;
#88625 = VERTEX_POINT ( 'NONE', #52636 ) ;
#88626 = DIRECTION ( 'NONE',  ( -1.000000000000000000, 0.000000000000000000, 0.000000000000000000 ) ) ;
#88627 = CARTESIAN_POINT ( 'NONE',  ( 93.96857342517719758, 15.00000000000000000, 0.000000000000000000 ) ) ;
#88628 = CARTESIAN_POINT ( 'NONE',  ( 119.1467862834650902, 228.0494855054051584, -2.679491924311248496 ) ) ;
#88629 = ADVANCED_FACE ( 'NONE', ( #5067 ), #34948, .T. ) ;
#88630 = EDGE_LOOP ( 'NONE', ( #22886, #79760, #86879, #70476, #19159, #16898, #98045, #58245, #54669, #78970, #61605, #25784, #86591, #74635, #1710, #86881, #33224, #53405, #7809, #41825, #75192, #63741 ) ) ;
#88631 = AXIS2_PLACEMENT_3D ( 'NONE', #36332, #75360, #4442 ) ;
#88632 = ORIENTED_EDGE ( 'NONE', *, *, #63428, .T. ) ;
#88633 = ORIENTED_EDGE ( 'NONE', *, *, #76944, .F. ) ;
#88634 = CARTESIAN_POINT ( 'NONE',  ( 87.14099742722598307, 46.04774061545423081, -8.211005622168064733 ) ) ;
#88636 = B_SPLINE_SURFACE_WITH_KNOTS ( 'NONE', 3, 1, ( 
 ( #32645, #2266 ),
 ( #740, #31624 ),
 ( #8842, #63541 ),
 ( #10362, #16441 ),
 ( #9349, #9872 ),
 ( #47336, #63043 ),
 ( #39712, #33663 ),
 ( #70640, #25554 ),
 ( #46844, #48353 ),
 ( #93988, #48864 ),
 ( #78762, #8350 ),
 ( #62522, #1254 ),
 ( #32135, #24539 ),
 ( #86405, #94992 ),
 ( #24039, #16937 ),
 ( #64553, #47823 ),
 ( #1765, #56442 ),
 ( #94482, #25038 ),
 ( #26060, #55917 ),
 ( #87436, #86910 ),
 ( #17447, #40729 ),
 ( #41230, #33148 ),
 ( #72169, #77766 ),
 ( #2774, #95514 ),
 ( #56936, #15939 ),
 ( #58429, #72681 ),
 ( #3761, #11382 ),
 ( #50339, #27058 ),
 ( #58911, #19956 ),
 ( #50833, #87921 ),
 ( #42720, #49352 ) ),
 .UNSPECIFIED., .F., .F., .F.,
 ( 4, 3, 3, 3, 3, 3, 3, 3, 3, 3, 4 ),
 ( 2, 2 ),
 ( 0.000000000000000000, 0.1122669598086781934, 0.2243161639709670419, 0.3396355846219092367, 0.4553962076585101326, 0.5677860799922354040, 0.6749047109689589874, 0.7773884377078243979, 0.8775581155834022429, 0.9782364162377785721, 1.000000000000000000 ),
 ( 0.000000000000000000, 1.000000000000000000 ),
 .UNSPECIFIED. ) ;
#88635 = CARTESIAN_POINT ( 'NONE',  ( 177.3755417603144338, 293.4917590415172413, -2.831906106862874584 ) ) ;
#88637 = CARTESIAN_POINT ( 'NONE',  ( 68.35453417343931903, 65.67399229982113695, 10.37910612949749911 ) ) ;
#88638 = CARTESIAN_POINT ( 'NONE',  ( 7.070540392147681708, 27.58029201028040234, 1.583844403245363353 ) ) ;
#88639 = CARTESIAN_POINT ( 'NONE',  ( 207.1917959879256728, 271.3993813902129659, -4.219514555173214276 ) ) ;
#88640 = CARTESIAN_POINT ( 'NONE',  ( 95.54687826519547400, 213.7202760586659167, -5.415160957724236172E-17 ) ) ;
#88641 = ORIENTED_EDGE ( 'NONE', *, *, #14398, .T. ) ;
#88642 = AXIS2_PLACEMENT_3D ( 'NONE', #35896, #52586, #75929 ) ;
#88643 = EDGE_LOOP ( 'NONE', ( #72420, #26768, #27237, #3576 ) ) ;
#88644 = LINE ( 'NONE', #19209, #7418 ) ;
#88645 = VERTEX_POINT ( 'NONE', #82614 ) ;
#88646 = EDGE_CURVE ( 'NONE', #73177, #47570, #35619, .T. ) ;
#88647 = CARTESIAN_POINT ( 'NONE',  ( 193.4694029979582979, 265.6208689502353764, -7.753311972763973436 ) ) ;
#88648 = CARTESIAN_POINT ( 'NONE',  ( 72.28450659106211162, 69.33006679800452332, -8.955401149264922367 ) ) ;
#88650 = CARTESIAN_POINT ( 'NONE',  ( 69.72987185967514279, 62.73297604805756578, -13.30854282143535094 ) ) ;
#88649 = CARTESIAN_POINT ( 'NONE',  ( 123.8274129399422918, 251.4869531367911577, 4.594050593750046652 ) ) ;
#88651 = CARTESIAN_POINT ( 'NONE',  ( -2.160980794731546695, 162.8927522451418213, -10.00000000000009059 ) ) ;
#88652 = CARTESIAN_POINT ( 'NONE',  ( 172.9698904924519240, 250.6642211707864476, -4.168778760986519671 ) ) ;
#88653 = ORIENTED_EDGE ( 'NONE', *, *, #27895, .F. ) ;
#88654 = VECTOR ( 'NONE', #10445, 1000.000000000000114 ) ;
#88655 = CARTESIAN_POINT ( 'NONE',  ( 204.4814917997891541, 276.4746623257233296, 13.21872368206963877 ) ) ;
#88656 = CARTESIAN_POINT ( 'NONE',  ( 157.3881051607127119, 274.1628151507284201, 13.17500510233437261 ) ) ;
#88657 = FACE_OUTER_BOUND ( 'NONE', #86131, .T. ) ;
#88658 = CYLINDRICAL_SURFACE ( 'NONE', #77220, 70.00000000000002842 ) ;
#88659 = CARTESIAN_POINT ( 'NONE',  ( 114.3892930691446850, 248.3967562850347122, -4.648177544792955347E-16 ) ) ;
#88660 = DIRECTION ( 'NONE',  ( -1.000000000000000000, 0.000000000000000000, 0.000000000000000000 ) ) ;
#88661 = CARTESIAN_POINT ( 'NONE',  ( 199.0763421850443251, 281.8631602056879615, -16.59742191502687092 ) ) ;
#88662 = LINE ( 'NONE', #9104, #93142 ) ;
#88663 = CARTESIAN_POINT ( 'NONE',  ( 153.5960728533304405, 266.9358381153638788, 16.61214075660420519 ) ) ;
#88664 = VECTOR ( 'NONE', #59692, 1000.000000000000000 ) ;
#88665 = DIRECTION ( 'NONE',  ( 0.8660254037844385966, 0.5000000000000002220, 7.511572993685832627E-16 ) ) ;
#88666 = CARTESIAN_POINT ( 'NONE',  ( 159.9788992190088948, 253.5554137441726255, -15.81862932303382330 ) ) ;
#88667 = CARTESIAN_POINT ( 'NONE',  ( 77.95413687424900218, 62.00520656085893734, 15.66750427035592708 ) ) ;
#88668 = CARTESIAN_POINT ( 'NONE',  ( 208.3790849386676598, 269.7238329819538762, -1.525282248498321946 ) ) ;
#88669 = DIRECTION ( 'NONE',  ( -0.8660254037844378194, -0.5000000000000013323, -0.000000000000000000 ) ) ;
#88670 = CARTESIAN_POINT ( 'NONE',  ( 70.43471136582493841, 64.87908352274641288, -12.18040581727293414 ) ) ;
#88671 = CARTESIAN_POINT ( 'NONE',  ( 182.1706919099075037, 264.0156754124984673, 13.98243676683973824 ) ) ;
#88672 = CARTESIAN_POINT ( 'NONE',  ( 5.338489584578805847, 26.58029201028039878, 1.583844403245363353 ) ) ;
#88673 = ADVANCED_FACE ( 'NONE', ( #28347 ), #90201, .T. ) ;
#88674 = CARTESIAN_POINT ( 'NONE',  ( 39.48888774545857672, 24.92755873383629250, 6.180339887498953466 ) ) ;
#88675 = CARTESIAN_POINT ( 'NONE',  ( -65.03992292888628413, 39.77302590755693501, -10.00000000000000000 ) ) ;
#88676 = CARTESIAN_POINT ( 'NONE',  ( 75.48012123268173923, 53.33211347945791658, 16.49774674168797617 ) ) ;
#88677 = CARTESIAN_POINT ( 'NONE',  ( 157.6561448699392827, 271.0329277901845444, -14.72207385342193220 ) ) ;
#88678 = CARTESIAN_POINT ( 'NONE',  ( 87.83899792242847582, 44.00541668311378629, -1.848955303085625390 ) ) ;
#88679 = CARTESIAN_POINT ( 'NONE',  ( 19.17374232530777078, 188.0024278399161233, 9.188101187500095079 ) ) ;
#88680 = CARTESIAN_POINT ( 'NONE',  ( 80.51198428680065433, 43.68793065238016737, 9.861687463089015893 ) ) ;
#88681 = VERTEX_POINT ( 'NONE', #6052 ) ;
#88682 = AXIS2_PLACEMENT_3D ( 'NONE', #57089, #25197, #18620 ) ;
#88683 = EDGE_CURVE ( 'NONE', #36246, #58741, #36947, .T. ) ;
#88684 = CARTESIAN_POINT ( 'NONE',  ( 86.77687789830739007, 46.46486760889777656, 9.079242751187690530 ) ) ;
#88685 = CARTESIAN_POINT ( 'NONE',  ( 23.30503800868897102, 15.58380873178786707, 6.180339887498953466 ) ) ;
#88686 = CARTESIAN_POINT ( 'NONE',  ( 208.1415148974628266, 270.1353163636768500, 3.453641150550738725 ) ) ;
#88687 = CARTESIAN_POINT ( 'NONE',  ( 72.04834849415196629, 72.28436413801229321, -0.8995985284803085236 ) ) ;
#88688 = CARTESIAN_POINT ( 'NONE',  ( 35.05980905203730913, 200.2369531367911293, -4.594050593750048428 ) ) ;
#88689 = AXIS2_PLACEMENT_3D ( 'NONE', #97700, #5481, #36363 ) ;
#88690 = CARTESIAN_POINT ( 'NONE',  ( 86.89976093607516816, 45.97909969559822940, 8.962991326411129833 ) ) ;
#88691 = CARTESIAN_POINT ( 'NONE',  ( 147.5177358149801421, 275.1387818813681179, 4.867883209065928085 ) ) ;
#88692 = CARTESIAN_POINT ( 'NONE',  ( 39.74423100597210379, 28.11029122506297639, -8.090169943749478065 ) ) ;
#88693 = CARTESIAN_POINT ( 'NONE',  ( 178.4130537636820009, 291.8182790410380676, 5.746090763460109940 ) ) ;
#88694 = CARTESIAN_POINT ( 'NONE',  ( 191.7741832257749195, 298.4843664033717801, -8.615487418695501276 ) ) ;
#88695 = DIRECTION ( 'NONE',  ( 0.000000000000000000, 0.000000000000000000, -1.000000000000000000 ) ) ;
#88696 = CARTESIAN_POINT ( 'NONE',  ( 116.4844995237365453, 231.3927522451418497, 10.00000000000009948 ) ) ;
#88697 = CARTESIAN_POINT ( 'NONE',  ( -0.7215821717578424499, 65.74988880085649612, -10.00000000000000000 ) ) ;
#88699 = FACE_OUTER_BOUND ( 'NONE', #91167, .T. ) ;
#88698 = CIRCLE ( 'NONE', #35277, 70.00000000000001421 ) ;
#88701 =( BOUNDED_SURFACE ( )  B_SPLINE_SURFACE ( 1, 2, ( 
 ( #61469, #22967, #93922, #24476, #55357, #80732, #81219, #10788, #87366, #3692, #72607, #18896, #71599, #41662, #79724, #88339, #57365, #57865, #27488, #11795, #72095, #88844, #9802, #3209, #18389, #34094, #49284, #19407, #65968, #35061, #64482, #64984, #17896, #50266, #42650, #34571, #58357, #95928, #49775, #42164, #73584, #10286, #73100, #96920, #48793, #65472, #96414, #11306, #4164, #17375, #48284, #41158, #26488, #40662, #56369, #2695, #25477, #79229, #26981, #25994, #33586, #2195, #95442, #56865, #87849, #33078, #80220, #63971, #94914, #36549, #75080, #36051, #6664, #66954, #67456, #98384, #28975, #59850, #90814, #90315, #58839, #21367, #45151, #97883, #97391, #20887, #21857, #76090, #51253, #5661, #68447, #52253, #27959, #83195, #29460, #82219, #13285, #52739, #28456, #12792, #5172, #29954, #83701, #89808, #20381, #43655, #74597, #37541, #82717, #59335, #12284, #43144, #51776, #13758, #81711, #14260, #44146, #99375, #44637, #75571, #89335, #66467, #91292, #19887, #6159, #4677, #37055, #50758, #74086, #35567, #67962, #98880, #60335, #38542, #68941, #62333, #99868, #69449, #7651, #16251, #7144, #30452, #60830, #61837, #61342, #53252, #65, #38031, #62842, #31937, #93797, #92784, #84207, #39031, #91790, #47141, #78066, #30948, #92301, #15737, #23339, #557, #15234, #8653, #31439, #93284, #54227, #22850, #85193, #53734, #23840, #46645, #77570, #22355, #69940, #46130, #39524, #24358, #70449, #8158, #40032, #54733, #55229, #84693, #14753, #1058, #85716, #77043, #86212, #45635, #1574, #16750, #76563, #47638, #78572, #9156, #70972, #94293, #88714, #94789, #3571, #18269, #63850, #17768, #18766, #86710, #41032, #33457, #32946, #73465, #19283, #34452, #63354, #71969, #42532, #95317, #3088, #25348, #48151, #87731, #65350, #72486, #24847, #2573, #64353, #55722, #25874, #80099, #56749, #17246, #56241, #71473, #32457, #72980, #49163, #49643, #41541, #50151, #87234, #96289, #10665, #48669, #79602, #80601, #79094, #33979, #64863, #10165, #9678, #81103, #26858, #40539, #95810, #2066, #26364, #57239, #88214, #11179, #42046, #57734, #11670, #65833, #43538, #35937, #96799, #74479, #51653, #28337, #27358, #27848, #43021, #4048, #45888, #66840, #22621, #13168, #73960, #58240, #89220, #82097, #44022, #19768, #38298, #12670, #61601, #4545, #90189, #30720, #81590, #7406, #100134, #82602, #50637, #20765, #84949, #46395, #12159, #5057, #34938, #35446, #97767, #66348, #6912, #97281, #59215, #51135, #61099, #58726, #89701, #20261, #76339, #37800, #68708, #99634, #30216, #69208, #76812, #92553, #92071, #53506, #84460, #15000, #23099, #53990, #15494, #8414, #32204, #47402, #17001, #31686, #32707, #47890, #9415, #85980, #46910, #78329, #70196, #78832, #8909, #39777, #38800, #55487, #62593, #55982, #48415, #63606, #16507, #56505, #70708, #79364, #54486, #314, #94546, #1322, #806, #93548, #31202, #18028, #40289, #62091, #63109, #94053, #71232, #77320, #69706, #24109, #55002, #93037, #7927, #1824, #23593, #24606, #86473, #25101, #85465, #16010, #33211, #39286, #9928, #86979, #17510, #40790, #71736, #77831, #2329, #64109, #95061, #25621, #87494, #20023, #79858, #57497, #58973, #11441, #19541, #80357, #64620, #3819, #50898, #88987, #10421 ),
 ( #50402, #81357, #89465, #89943, #43290, #3340, #81847, #41294, #34701, #49911, #73227, #80868, #12421, #97531, #66604, #96059, #65602, #18527, #74237, #4823, #35204, #48921, #96555, #11927, #73717, #35706, #41800, #4300, #28100, #10928, #66107, #97055, #42783, #72234, #2840, #33730, #72747, #42294, #95575, #87979, #34216, #56997, #26120, #27125, #88477, #65111, #27626, #49410, #26618, #19039, #58007, #58491, #45288, #44289, #83336, #21508, #75218, #30097, #5801, #13900, #44781, #75717, #6301, #37192, #67595, #28595, #68094, #68590, #36686, #67095, #98525, #76222, #99513, #90458, #52393, #91944, #99016, #98019, #29602, #83841, #21028, #22495, #60979, #14406, #51399, #29114, #20520, #90952, #60475, #51911, #59477, #91433, #6798, #21994, #43791, #59982, #52889, #74734, #37678, #82362, #12931, #82851, #5313, #13421, #36189, #51211, #73541, #27921, #19847, #80685, #34052, #64942, #88799, #50715, #3167, #43615, #19366, #66915, #11260, #96876, #36014, #88295, #12752, #5132, #89293, #26448, #27444, #90275, #51738, #95887, #81180, #41621, #72563, #50225, #18850, #12242, #49732, #11747, #57820, #66427, #57323, #42123, #10745, #42610, #73054, #3649, #4124, #34529, #74555, #82178, #97845, #35018, #65429, #81669, #96370, #97355, #58804, #65920, #26936, #58318, #43101, #74044, #4632, #89768, #35526, #20339, #28414, #59294, #20846, #75533, #84169, #52703, #83663, #44104, #60789, #37014, #61306, #53697, #37994, #91253, #61800, #14226, #84653, #59809, #5619, #68906, #21818, #6118, #67922, #36513, #23302, #22315, #67414, #6627, #76047, #14716, #82680, #75043, #38501, #44598, #15198, #68411, #13722, #98845, #99832, #98342, #45113, #37504, #83157, #30416, #92268, #60296, #29422, #99338, #29917, #53218, #91752, #22816, #45599, #76533, #7110, #52210, #46094, #77007, #7612, #69416, #28, #28933, #30913, #92748, #13246, #90776, #21327, #62805, #33415, #24319, #56196, #31407, #77534, #9639, #93762, #78028, #47107, #8126, #95272, #94254, #38999, #78533, #47605, #55685, #54192, #15703, #10120, #16215, #25308, #39989, #85677, #39486, #40498, #69905, #55195, #86178, #54694, #85156, #40984, #87192, #46601, #16712, #64315, #9118, #24807, #8620, #519, #70930, #17725, #86673, #62293, #1535, #32417, #93250, #63311, #17205, #48108, #23805, #70412, #1020, #31901, #94746, #79050, #71430, #2019, #32905, #63813, #48627, #79562, #71929, #2533, #58685, #34411, #82057, #26324, #11629, #51090, #3048, #27810, #20221, #4013, #41501, #42490, #5019, #66800, #10624, #96252, #56710, #87693, #3535, #33935, #27321, #64822, #65312, #72942, #81548, #72442, #95768, #25835, #26816, #57197, #18225, #57697, #88177, #89659, #97244, #12626, #88674, #49121, #34895, #80056, #43496, #18723, #74438, #35900, #65796, #49607, #73424, #80559, #11137, #42009, #19247, #50112, #81066, #96754, #58205, #89182, #19730, #50597, #12117, #42981, #73919, #4504, #35404, #66312, #67298, #90146, #44489, #43984, #99714, #68789, #30302, #29313, #20723, #75934, #97727, #53096, #84052, #75419, #28807, #52589, #67807, #37390, #52098, #14610, #68294, #29802, #6004, #98225, #98734, #90661, #99217, #60178, #91142, #59172, #6512, #83043, #76423, #61188, #45487, #36897, #76890, #21704, #92156, #74926 ) ),
 .UNSPECIFIED., .F., .F., .T. ) 
 B_SPLINE_SURFACE_WITH_KNOTS ( ( 2, 2 ),
 ( 3, 2, 2, 2, 2, 2, 2, 2, 2, 2, 2, 2, 2, 2, 2, 2, 2, 2, 2, 2, 2, 2, 2, 2, 2, 2, 2, 2, 2, 2, 2, 2, 2, 2, 2, 2, 2, 2, 2, 2, 2, 2, 2, 2, 2, 2, 2, 2, 2, 2, 2, 2, 2, 2, 2, 2, 2, 2, 2, 2, 2, 2, 2, 2, 2, 2, 2, 2, 2, 2, 2, 2, 2, 2, 2, 2, 2, 2, 2, 2, 2, 2, 2, 2, 2, 2, 2, 2, 2, 2, 2, 2, 2, 2, 2, 2, 2, 2, 2, 2, 2, 2, 2, 2, 2, 2, 2, 2, 2, 2, 2, 2, 2, 2, 2, 2, 2, 2, 2, 2, 2, 2, 2, 2, 2, 2, 2, 2, 2, 2, 2, 2, 2, 2, 2, 2, 2, 2, 2, 2, 2, 2, 2, 2, 2, 2, 2, 2, 2, 2, 2, 2, 2, 2, 2, 2, 2, 2, 2, 2, 2, 2, 2, 2, 2, 2, 2, 2, 2, 2, 2, 2, 2, 2, 2, 2, 2, 2, 2, 2, 2, 2, 2, 2, 2, 2, 2, 2, 2, 2, 2, 2, 2, 2, 2, 2, 2, 2, 2, 2, 3 ),
 ( 0.000000000000000000, 1.000000000000000000 ),
 ( 0.000000000000000000, 0.005000000000000000104, 0.01000000000000000021, 0.01499999999999999944, 0.02000000000000000042, 0.02500000000000000139, 0.02999999999999999889, 0.03500000000000000333, 0.04000000000000000083, 0.04499999999999999833, 0.05000000000000000278, 0.05500000000000000028, 0.05999999999999999778, 0.06500000000000000222, 0.07000000000000000666, 0.07499999999999999722, 0.08000000000000000167, 0.08500000000000000611, 0.08999999999999999667, 0.09500000000000000111, 0.1000000000000000056, 0.1049999999999999961, 0.1100000000000000006, 0.1150000000000000050, 0.1199999999999999956, 0.1250000000000000000, 0.1300000000000000044, 0.1350000000000000089, 0.1400000000000000133, 0.1449999999999999900, 0.1499999999999999944, 0.1549999999999999989, 0.1600000000000000033, 0.1650000000000000078, 0.1700000000000000122, 0.1749999999999999889, 0.1799999999999999933, 0.1849999999999999978, 0.1900000000000000022, 0.1950000000000000067, 0.2000000000000000111, 0.2049999999999999878, 0.2099999999999999922, 0.2149999999999999967, 0.2200000000000000011, 0.2250000000000000056, 0.2300000000000000100, 0.2349999999999999867, 0.2399999999999999911, 0.2449999999999999956, 0.2500000000000000000, 0.2550000000000000044, 0.2600000000000000089, 0.2650000000000000133, 0.2700000000000000178, 0.2750000000000000222, 0.2800000000000000266, 0.2849999999999999756, 0.2899999999999999800, 0.2949999999999999845, 0.2999999999999999889, 0.3049999999999999933, 0.3099999999999999978, 0.3150000000000000022, 0.3200000000000000067, 0.3250000000000000111, 0.3300000000000000155, 0.3350000000000000200, 0.3400000000000000244, 0.3449999999999999734, 0.3499999999999999778, 0.3549999999999999822, 0.3599999999999999867, 0.3649999999999999911, 0.3699999999999999956, 0.3750000000000000000, 0.3800000000000000044, 0.3850000000000000089, 0.3900000000000000133, 0.3950000000000000178, 0.4000000000000000222, 0.4050000000000000266, 0.4099999999999999756, 0.4149999999999999800, 0.4199999999999999845, 0.4249999999999999889, 0.4299999999999999933, 0.4349999999999999978, 0.4400000000000000022, 0.4450000000000000067, 0.4500000000000000111, 0.4550000000000000155, 0.4600000000000000200, 0.4650000000000000244, 0.4699999999999999734, 0.4749999999999999778, 0.4799999999999999822, 0.4849999999999999867, 0.4899999999999999911, 0.4949999999999999956, 0.5000000000000000000, 0.5050000000000000044, 0.5100000000000000089, 0.5150000000000000133, 0.5200000000000000178, 0.5250000000000000222, 0.5300000000000000266, 0.5350000000000000311, 0.5400000000000000355, 0.5450000000000000400, 0.5500000000000000444, 0.5550000000000000488, 0.5600000000000000533, 0.5649999999999999467, 0.5699999999999999512, 0.5749999999999999556, 0.5799999999999999600, 0.5849999999999999645, 0.5899999999999999689, 0.5949999999999999734, 0.5999999999999999778, 0.6049999999999999822, 0.6099999999999999867, 0.6149999999999999911, 0.6199999999999999956, 0.6250000000000000000, 0.6300000000000000044, 0.6350000000000000089, 0.6400000000000000133, 0.6450000000000000178, 0.6500000000000000222, 0.6550000000000000266, 0.6600000000000000311, 0.6650000000000000355, 0.6700000000000000400, 0.6750000000000000444, 0.6800000000000000488, 0.6850000000000000533, 0.6899999999999999467, 0.6949999999999999512, 0.6999999999999999556, 0.7049999999999999600, 0.7099999999999999645, 0.7149999999999999689, 0.7199999999999999734, 0.7249999999999999778, 0.7299999999999999822, 0.7349999999999999867, 0.7399999999999999911, 0.7449999999999999956, 0.7500000000000000000, 0.7550000000000000044, 0.7600000000000000089, 0.7650000000000000133, 0.7700000000000000178, 0.7750000000000000222, 0.7800000000000000266, 0.7850000000000000311, 0.7900000000000000355, 0.7950000000000000400, 0.8000000000000000444, 0.8050000000000000488, 0.8100000000000000533, 0.8149999999999999467, 0.8199999999999999512, 0.8249999999999999556, 0.8299999999999999600, 0.8349999999999999645, 0.8399999999999999689, 0.8449999999999999734, 0.8499999999999999778, 0.8549999999999999822, 0.8599999999999999867, 0.8649999999999999911, 0.8699999999999999956, 0.8750000000000000000, 0.8800000000000000044, 0.8850000000000000089, 0.8900000000000000133, 0.8950000000000000178, 0.9000000000000000222, 0.9050000000000000266, 0.9100000000000000311, 0.9150000000000000355, 0.9200000000000000400, 0.9250000000000000444, 0.9300000000000000488, 0.9350000000000000533, 0.9399999999999999467, 0.9449999999999999512, 0.9499999999999999556, 0.9549999999999999600, 0.9599999999999999645, 0.9649999999999999689, 0.9699999999999999734, 0.9749999999999999778, 0.9799999999999999822, 0.9849999999999999867, 0.9899999999999999911, 0.9949999999999999956, 1.000000000000000000 ),
 .UNSPECIFIED. ) 
 GEOMETRIC_REPRESENTATION_ITEM ( )  RATIONAL_B_SPLINE_SURFACE ( (
 ( 1.000000000000000000, 0.9510565162951535312, 1.000000000000000000, 0.9510565162951535312, 1.000000000000000000, 0.9510565162951535312, 1.000000000000000000, 0.9510565162951535312, 1.000000000000000000, 0.9510565162951535312, 1.000000000000000000, 0.9510565162951535312, 1.000000000000000000, 0.9510565162951535312, 1.000000000000000000, 0.9510565162951535312, 1.000000000000000000, 0.9510565162951535312, 1.000000000000000000, 0.9510565162951535312, 1.000000000000000000, 0.9510565162951535312, 1.000000000000000000, 0.9510565162951535312, 1.000000000000000000, 0.9510565162951535312, 1.000000000000000000, 0.9510565162951535312, 1.000000000000000000, 0.9510565162951535312, 1.000000000000000000, 0.9510565162951535312, 1.000000000000000000, 0.9510565162951535312, 1.000000000000000000, 0.9510565162951535312, 1.000000000000000000, 0.9510565162951535312, 1.000000000000000000, 0.9510565162951535312, 1.000000000000000000, 0.9510565162951535312, 1.000000000000000000, 0.9510565162951535312, 1.000000000000000000, 0.9510565162951535312, 1.000000000000000000, 0.9510565162951535312, 1.000000000000000000, 0.9510565162951535312, 1.000000000000000000, 0.9510565162951535312, 1.000000000000000000, 0.9510565162951535312, 1.000000000000000000, 0.9510565162951535312, 1.000000000000000000, 0.9510565162951535312, 1.000000000000000000, 0.9510565162951535312, 1.000000000000000000, 0.9510565162951535312, 1.000000000000000000, 0.9510565162951535312, 1.000000000000000000, 0.9510565162951535312, 1.000000000000000000, 0.9510565162951535312, 1.000000000000000000, 0.9510565162951535312, 1.000000000000000000, 0.9510565162951535312, 1.000000000000000000, 0.9510565162951535312, 1.000000000000000000, 0.9510565162951535312, 1.000000000000000000, 0.9510565162951535312, 1.000000000000000000, 0.9510565162951535312, 1.000000000000000000, 0.9510565162951535312, 1.000000000000000000, 0.9510565162951535312, 1.000000000000000000, 0.9510565162951535312, 1.000000000000000000, 0.9510565162951535312, 1.000000000000000000, 0.9510565162951535312, 1.000000000000000000, 0.9510565162951535312, 1.000000000000000000, 0.9510565162951535312, 1.000000000000000000, 0.9510565162951535312, 1.000000000000000000, 0.9510565162951535312, 1.000000000000000000, 0.9510565162951535312, 1.000000000000000000, 0.9510565162951535312, 1.000000000000000000, 0.9510565162951535312, 1.000000000000000000, 0.9510565162951535312, 1.000000000000000000, 0.9510565162951535312, 1.000000000000000000, 0.9510565162951535312, 1.000000000000000000, 0.9510565162951535312, 1.000000000000000000, 0.9510565162951535312, 1.000000000000000000, 0.9510565162951535312, 1.000000000000000000, 0.9510565162951535312, 1.000000000000000000, 0.9510565162951535312, 1.000000000000000000, 0.9510565162951535312, 1.000000000000000000, 0.9510565162951535312, 1.000000000000000000, 0.9510565162951535312, 1.000000000000000000, 0.9510565162951535312, 1.000000000000000000, 0.9510565162951535312, 1.000000000000000000, 0.9510565162951535312, 1.000000000000000000, 0.9510565162951535312, 1.000000000000000000, 0.9510565162951535312, 1.000000000000000000, 0.9510565162951535312, 1.000000000000000000, 0.9510565162951535312, 1.000000000000000000, 0.9510565162951535312, 1.000000000000000000, 0.9510565162951535312, 1.000000000000000000, 0.9510565162951535312, 1.000000000000000000, 0.9510565162951535312, 1.000000000000000000, 0.9510565162951535312, 1.000000000000000000, 0.9510565162951535312, 1.000000000000000000, 0.9510565162951535312, 1.000000000000000000, 0.9510565162951535312, 1.000000000000000000, 0.9510565162951535312, 1.000000000000000000, 0.9510565162951535312, 1.000000000000000000, 0.9510565162951535312, 1.000000000000000000, 0.9510565162951535312, 1.000000000000000000, 0.9510565162951535312, 1.000000000000000000, 0.9510565162951535312, 1.000000000000000000, 0.9510565162951535312, 1.000000000000000000, 0.9510565162951535312, 1.000000000000000000, 0.9510565162951535312, 1.000000000000000000, 0.9510565162951535312, 1.000000000000000000, 0.9510565162951535312, 1.000000000000000000, 0.9510565162951535312, 1.000000000000000000, 0.9510565162951535312, 1.000000000000000000, 0.9510565162951535312, 1.000000000000000000, 0.9510565162951535312, 1.000000000000000000, 0.9510565162951535312, 1.000000000000000000, 0.9510565162951535312, 1.000000000000000000, 0.9510565162951535312, 1.000000000000000000, 0.9510565162951535312, 1.000000000000000000, 0.9510565162951535312, 1.000000000000000000, 0.9510565162951535312, 1.000000000000000000, 0.9510565162951535312, 1.000000000000000000, 0.9510565162951535312, 1.000000000000000000, 0.9510565162951535312, 1.000000000000000000, 0.9510565162951535312, 1.000000000000000000, 0.9510565162951535312, 1.000000000000000000, 0.9510565162951535312, 1.000000000000000000, 0.9510565162951535312, 1.000000000000000000, 0.9510565162951535312, 1.000000000000000000, 0.9510565162951535312, 1.000000000000000000, 0.9510565162951535312, 1.000000000000000000, 0.9510565162951535312, 1.000000000000000000, 0.9510565162951535312, 1.000000000000000000, 0.9510565162951535312, 1.000000000000000000, 0.9510565162951535312, 1.000000000000000000, 0.9510565162951535312, 1.000000000000000000, 0.9510565162951535312, 1.000000000000000000, 0.9510565162951535312, 1.000000000000000000, 0.9510565162951535312, 1.000000000000000000, 0.9510565162951535312, 1.000000000000000000, 0.9510565162951535312, 1.000000000000000000, 0.9510565162951535312, 1.000000000000000000, 0.9510565162951535312, 1.000000000000000000, 0.9510565162951535312, 1.000000000000000000, 0.9510565162951535312, 1.000000000000000000, 0.9510565162951535312, 1.000000000000000000, 0.9510565162951535312, 1.000000000000000000, 0.9510565162951535312, 1.000000000000000000, 0.9510565162951535312, 1.000000000000000000, 0.9510565162951535312, 1.000000000000000000, 0.9510565162951535312, 1.000000000000000000, 0.9510565162951535312, 1.000000000000000000, 0.9510565162951535312, 1.000000000000000000, 0.9510565162951535312, 1.000000000000000000, 0.9510565162951535312, 1.000000000000000000, 0.9510565162951535312, 1.000000000000000000, 0.9510565162951535312, 1.000000000000000000, 0.9510565162951535312, 1.000000000000000000, 0.9510565162951535312, 1.000000000000000000, 0.9510565162951535312, 1.000000000000000000, 0.9510565162951535312, 1.000000000000000000, 0.9510565162951535312, 1.000000000000000000, 0.9510565162951535312, 1.000000000000000000, 0.9510565162951535312, 1.000000000000000000, 0.9510565162951535312, 1.000000000000000000, 0.9510565162951535312, 1.000000000000000000, 0.9510565162951535312, 1.000000000000000000, 0.9510565162951535312, 1.000000000000000000, 0.9510565162951535312, 1.000000000000000000, 0.9510565162951535312, 1.000000000000000000, 0.9510565162951535312, 1.000000000000000000, 0.9510565162951535312, 1.000000000000000000, 0.9510565162951535312, 1.000000000000000000, 0.9510565162951535312, 1.000000000000000000, 0.9510565162951535312, 1.000000000000000000, 0.9510565162951535312, 1.000000000000000000, 0.9510565162951535312, 1.000000000000000000, 0.9510565162951535312, 1.000000000000000000, 0.9510565162951535312, 1.000000000000000000, 0.9510565162951535312, 1.000000000000000000, 0.9510565162951535312, 1.000000000000000000, 0.9510565162951535312, 1.000000000000000000, 0.9510565162951535312, 1.000000000000000000, 0.9510565162951535312, 1.000000000000000000, 0.9510565162951535312, 1.000000000000000000, 0.9510565162951535312, 1.000000000000000000, 0.9510565162951535312, 1.000000000000000000, 0.9510565162951535312, 1.000000000000000000, 0.9510565162951535312, 1.000000000000000000, 0.9510565162951535312, 1.000000000000000000, 0.9510565162951535312, 1.000000000000000000, 0.9510565162951535312, 1.000000000000000000, 0.9510565162951535312, 1.000000000000000000, 0.9510565162951535312, 1.000000000000000000, 0.9510565162951535312, 1.000000000000000000, 0.9510565162951535312, 1.000000000000000000, 0.9510565162951535312, 1.000000000000000000, 0.9510565162951535312, 1.000000000000000000, 0.9510565162951535312, 1.000000000000000000, 0.9510565162951535312, 1.000000000000000000, 0.9510565162951535312, 1.000000000000000000, 0.9510565162951535312, 1.000000000000000000, 0.9510565162951535312, 1.000000000000000000, 0.9510565162951535312, 1.000000000000000000, 0.9510565162951535312, 1.000000000000000000, 0.9510565162951535312, 1.000000000000000000, 0.9510565162951535312, 1.000000000000000000, 0.9510565162951535312, 1.000000000000000000, 0.9510565162951535312, 1.000000000000000000, 0.9510565162951535312, 1.000000000000000000, 0.9510565162951535312, 1.000000000000000000, 0.9510565162951535312, 1.000000000000000000, 0.9510565162951535312, 1.000000000000000000, 0.9510565162951535312, 1.000000000000000000, 0.9510565162951535312, 1.000000000000000000, 0.9510565162951535312, 1.000000000000000000, 0.9510565162951535312, 1.000000000000000000, 0.9510565162951535312, 1.000000000000000000, 0.9510565162951535312, 1.000000000000000000, 0.9510565162951535312, 1.000000000000000000, 0.9510565162951535312, 1.000000000000000000, 0.9510565162951535312, 1.000000000000000000),
 ( 1.000000000000000000, 0.9510565162951535312, 1.000000000000000000, 0.9510565162951535312, 1.000000000000000000, 0.9510565162951535312, 1.000000000000000000, 0.9510565162951535312, 1.000000000000000000, 0.9510565162951535312, 1.000000000000000000, 0.9510565162951535312, 1.000000000000000000, 0.9510565162951535312, 1.000000000000000000, 0.9510565162951535312, 1.000000000000000000, 0.9510565162951535312, 1.000000000000000000, 0.9510565162951535312, 1.000000000000000000, 0.9510565162951535312, 1.000000000000000000, 0.9510565162951535312, 1.000000000000000000, 0.9510565162951535312, 1.000000000000000000, 0.9510565162951535312, 1.000000000000000000, 0.9510565162951535312, 1.000000000000000000, 0.9510565162951535312, 1.000000000000000000, 0.9510565162951535312, 1.000000000000000000, 0.9510565162951535312, 1.000000000000000000, 0.9510565162951535312, 1.000000000000000000, 0.9510565162951535312, 1.000000000000000000, 0.9510565162951535312, 1.000000000000000000, 0.9510565162951535312, 1.000000000000000000, 0.9510565162951535312, 1.000000000000000000, 0.9510565162951535312, 1.000000000000000000, 0.9510565162951535312, 1.000000000000000000, 0.9510565162951535312, 1.000000000000000000, 0.9510565162951535312, 1.000000000000000000, 0.9510565162951535312, 1.000000000000000000, 0.9510565162951535312, 1.000000000000000000, 0.9510565162951535312, 1.000000000000000000, 0.9510565162951535312, 1.000000000000000000, 0.9510565162951535312, 1.000000000000000000, 0.9510565162951535312, 1.000000000000000000, 0.9510565162951535312, 1.000000000000000000, 0.9510565162951535312, 1.000000000000000000, 0.9510565162951535312, 1.000000000000000000, 0.9510565162951535312, 1.000000000000000000, 0.9510565162951535312, 1.000000000000000000, 0.9510565162951535312, 1.000000000000000000, 0.9510565162951535312, 1.000000000000000000, 0.9510565162951535312, 1.000000000000000000, 0.9510565162951535312, 1.000000000000000000, 0.9510565162951535312, 1.000000000000000000, 0.9510565162951535312, 1.000000000000000000, 0.9510565162951535312, 1.000000000000000000, 0.9510565162951535312, 1.000000000000000000, 0.9510565162951535312, 1.000000000000000000, 0.9510565162951535312, 1.000000000000000000, 0.9510565162951535312, 1.000000000000000000, 0.9510565162951535312, 1.000000000000000000, 0.9510565162951535312, 1.000000000000000000, 0.9510565162951535312, 1.000000000000000000, 0.9510565162951535312, 1.000000000000000000, 0.9510565162951535312, 1.000000000000000000, 0.9510565162951535312, 1.000000000000000000, 0.9510565162951535312, 1.000000000000000000, 0.9510565162951535312, 1.000000000000000000, 0.9510565162951535312, 1.000000000000000000, 0.9510565162951535312, 1.000000000000000000, 0.9510565162951535312, 1.000000000000000000, 0.9510565162951535312, 1.000000000000000000, 0.9510565162951535312, 1.000000000000000000, 0.9510565162951535312, 1.000000000000000000, 0.9510565162951535312, 1.000000000000000000, 0.9510565162951535312, 1.000000000000000000, 0.9510565162951535312, 1.000000000000000000, 0.9510565162951535312, 1.000000000000000000, 0.9510565162951535312, 1.000000000000000000, 0.9510565162951535312, 1.000000000000000000, 0.9510565162951535312, 1.000000000000000000, 0.9510565162951535312, 1.000000000000000000, 0.9510565162951535312, 1.000000000000000000, 0.9510565162951535312, 1.000000000000000000, 0.9510565162951535312, 1.000000000000000000, 0.9510565162951535312, 1.000000000000000000, 0.9510565162951535312, 1.000000000000000000, 0.9510565162951535312, 1.000000000000000000, 0.9510565162951535312, 1.000000000000000000, 0.9510565162951535312, 1.000000000000000000, 0.9510565162951535312, 1.000000000000000000, 0.9510565162951535312, 1.000000000000000000, 0.9510565162951535312, 1.000000000000000000, 0.9510565162951535312, 1.000000000000000000, 0.9510565162951535312, 1.000000000000000000, 0.9510565162951535312, 1.000000000000000000, 0.9510565162951535312, 1.000000000000000000, 0.9510565162951535312, 1.000000000000000000, 0.9510565162951535312, 1.000000000000000000, 0.9510565162951535312, 1.000000000000000000, 0.9510565162951535312, 1.000000000000000000, 0.9510565162951535312, 1.000000000000000000, 0.9510565162951535312, 1.000000000000000000, 0.9510565162951535312, 1.000000000000000000, 0.9510565162951535312, 1.000000000000000000, 0.9510565162951535312, 1.000000000000000000, 0.9510565162951535312, 1.000000000000000000, 0.9510565162951535312, 1.000000000000000000, 0.9510565162951535312, 1.000000000000000000, 0.9510565162951535312, 1.000000000000000000, 0.9510565162951535312, 1.000000000000000000, 0.9510565162951535312, 1.000000000000000000, 0.9510565162951535312, 1.000000000000000000, 0.9510565162951535312, 1.000000000000000000, 0.9510565162951535312, 1.000000000000000000, 0.9510565162951535312, 1.000000000000000000, 0.9510565162951535312, 1.000000000000000000, 0.9510565162951535312, 1.000000000000000000, 0.9510565162951535312, 1.000000000000000000, 0.9510565162951535312, 1.000000000000000000, 0.9510565162951535312, 1.000000000000000000, 0.9510565162951535312, 1.000000000000000000, 0.9510565162951535312, 1.000000000000000000, 0.9510565162951535312, 1.000000000000000000, 0.9510565162951535312, 1.000000000000000000, 0.9510565162951535312, 1.000000000000000000, 0.9510565162951535312, 1.000000000000000000, 0.9510565162951535312, 1.000000000000000000, 0.9510565162951535312, 1.000000000000000000, 0.9510565162951535312, 1.000000000000000000, 0.9510565162951535312, 1.000000000000000000, 0.9510565162951535312, 1.000000000000000000, 0.9510565162951535312, 1.000000000000000000, 0.9510565162951535312, 1.000000000000000000, 0.9510565162951535312, 1.000000000000000000, 0.9510565162951535312, 1.000000000000000000, 0.9510565162951535312, 1.000000000000000000, 0.9510565162951535312, 1.000000000000000000, 0.9510565162951535312, 1.000000000000000000, 0.9510565162951535312, 1.000000000000000000, 0.9510565162951535312, 1.000000000000000000, 0.9510565162951535312, 1.000000000000000000, 0.9510565162951535312, 1.000000000000000000, 0.9510565162951535312, 1.000000000000000000, 0.9510565162951535312, 1.000000000000000000, 0.9510565162951535312, 1.000000000000000000, 0.9510565162951535312, 1.000000000000000000, 0.9510565162951535312, 1.000000000000000000, 0.9510565162951535312, 1.000000000000000000, 0.9510565162951535312, 1.000000000000000000, 0.9510565162951535312, 1.000000000000000000, 0.9510565162951535312, 1.000000000000000000, 0.9510565162951535312, 1.000000000000000000, 0.9510565162951535312, 1.000000000000000000, 0.9510565162951535312, 1.000000000000000000, 0.9510565162951535312, 1.000000000000000000, 0.9510565162951535312, 1.000000000000000000, 0.9510565162951535312, 1.000000000000000000, 0.9510565162951535312, 1.000000000000000000, 0.9510565162951535312, 1.000000000000000000, 0.9510565162951535312, 1.000000000000000000, 0.9510565162951535312, 1.000000000000000000, 0.9510565162951535312, 1.000000000000000000, 0.9510565162951535312, 1.000000000000000000, 0.9510565162951535312, 1.000000000000000000, 0.9510565162951535312, 1.000000000000000000, 0.9510565162951535312, 1.000000000000000000, 0.9510565162951535312, 1.000000000000000000, 0.9510565162951535312, 1.000000000000000000, 0.9510565162951535312, 1.000000000000000000, 0.9510565162951535312, 1.000000000000000000, 0.9510565162951535312, 1.000000000000000000, 0.9510565162951535312, 1.000000000000000000, 0.9510565162951535312, 1.000000000000000000, 0.9510565162951535312, 1.000000000000000000, 0.9510565162951535312, 1.000000000000000000, 0.9510565162951535312, 1.000000000000000000, 0.9510565162951535312, 1.000000000000000000, 0.9510565162951535312, 1.000000000000000000, 0.9510565162951535312, 1.000000000000000000, 0.9510565162951535312, 1.000000000000000000, 0.9510565162951535312, 1.000000000000000000, 0.9510565162951535312, 1.000000000000000000, 0.9510565162951535312, 1.000000000000000000, 0.9510565162951535312, 1.000000000000000000, 0.9510565162951535312, 1.000000000000000000, 0.9510565162951535312, 1.000000000000000000, 0.9510565162951535312, 1.000000000000000000, 0.9510565162951535312, 1.000000000000000000, 0.9510565162951535312, 1.000000000000000000, 0.9510565162951535312, 1.000000000000000000, 0.9510565162951535312, 1.000000000000000000, 0.9510565162951535312, 1.000000000000000000, 0.9510565162951535312, 1.000000000000000000, 0.9510565162951535312, 1.000000000000000000, 0.9510565162951535312, 1.000000000000000000, 0.9510565162951535312, 1.000000000000000000, 0.9510565162951535312, 1.000000000000000000, 0.9510565162951535312, 1.000000000000000000, 0.9510565162951535312, 1.000000000000000000, 0.9510565162951535312, 1.000000000000000000, 0.9510565162951535312, 1.000000000000000000, 0.9510565162951535312, 1.000000000000000000, 0.9510565162951535312, 1.000000000000000000, 0.9510565162951535312, 1.000000000000000000, 0.9510565162951535312, 1.000000000000000000, 0.9510565162951535312, 1.000000000000000000, 0.9510565162951535312, 1.000000000000000000, 0.9510565162951535312, 1.000000000000000000, 0.9510565162951535312, 1.000000000000000000, 0.9510565162951535312, 1.000000000000000000) ) ) 
 REPRESENTATION_ITEM ( '' )  SURFACE ( )  );
#88700 = CARTESIAN_POINT ( 'NONE',  ( 81.57285043722427531, 211.2365022471902023, 10.00000000000009592 ) ) ;
#88702 = CARTESIAN_POINT ( 'NONE',  ( 75.99750771566300500, 65.44421971917601866, -13.95497799904430458 ) ) ;
#88703 = CARTESIAN_POINT ( 'NONE',  ( 175.1378461883211912, 279.3152656845848583, 16.63146252814350134 ) ) ;
#88704 = CARTESIAN_POINT ( 'NONE',  ( 46.39958950466356669, 197.5958772461660544, -9.188101187500095079 ) ) ;
#88705 = ORIENTED_EDGE ( 'NONE', *, *, #18310, .F. ) ;
#88706 = CARTESIAN_POINT ( 'NONE',  ( -16.51533461259688806, 83.20563776615510676, 14.84223041658741060 ) ) ;
#88707 = CARTESIAN_POINT ( 'NONE',  ( 198.6363782946250183, 286.5986958926748116, -18.50260615857378355 ) ) ;
#88708 = CARTESIAN_POINT ( 'NONE',  ( 67.47994349727724739, 66.77496821803354976, -8.450748656079085208 ) ) ;
#88709 = ORIENTED_EDGE ( 'NONE', *, *, #61906, .F. ) ;
#88710 = VECTOR ( 'NONE', #46529, 1000.000000000000000 ) ;
#88711 = CARTESIAN_POINT ( 'NONE',  ( 167.4364575273616822, 285.0497252248627547, 7.773533576968246983 ) ) ;
#88712 = CARTESIAN_POINT ( 'NONE',  ( 207.6477529416552557, 270.9905371579805546, 7.447146952410988341 ) ) ;
#88713 = DIRECTION ( 'NONE',  ( 0.5000000000000009992, -0.8660254037844380415, 0.000000000000000000 ) ) ;
#88714 = CARTESIAN_POINT ( 'NONE',  ( 26.65055534615017763, 21.10170272979927830, -7.433330006724141015 ) ) ;
#88715 = CARTESIAN_POINT ( 'NONE',  ( 187.5114625740205270, 264.6447095084205330, 10.77906233194030250 ) ) ;
#88716 = CARTESIAN_POINT ( 'NONE',  ( 190.9474291326297930, 266.7645650087163745, -12.82661358031884546 ) ) ;
#88717 = CARTESIAN_POINT ( 'NONE',  ( 171.5429889697022645, 255.3861488387996701, 12.49561417135016406 ) ) ;
#88718 = EDGE_LOOP ( 'NONE', ( #47667, #65765, #80041, #6054 ) ) ;
#88719 = CARTESIAN_POINT ( 'NONE',  ( 11.81506597172265316, 27.79752408145591502, -5.678558825948271327 ) ) ;
#88720 = CARTESIAN_POINT ( 'NONE',  ( 76.03876470936320686, 60.18435193765323987, 15.76689522733356164 ) ) ;
#88721 = CARTESIAN_POINT ( 'NONE',  ( 173.1828068919900829, 254.0980817964978371, 8.310286840905920513 ) ) ;
#88722 = CARTESIAN_POINT ( 'NONE',  ( 10.91961124514380366, 177.1115022471902307, 10.00000000000009592 ) ) ;
#88723 = ORIENTED_EDGE ( 'NONE', *, *, #21506, .F. ) ;
#88724 = CARTESIAN_POINT ( 'NONE',  ( 178.6961944256588879, 282.3096576696289048, 15.48889775239164024 ) ) ;
#88725 = CARTESIAN_POINT ( 'NONE',  ( 167.1103609241472157, 261.4346035182707055, 16.90549041653298445 ) ) ;
#88726 = CARTESIAN_POINT ( 'NONE',  ( 32.38751264475774860, 201.0530062829863027, -4.648177544792955347E-16 ) ) ;
#88727 = CARTESIAN_POINT ( 'NONE',  ( 75.27341285390555470, 63.90702616464435692, -14.88884485943207459 ) ) ;
#88728 = ORIENTED_EDGE ( 'NONE', *, *, #49180, .T. ) ;
#88729 = VERTEX_POINT ( 'NONE', #62732 ) ;
#88730 = CIRCLE ( 'NONE', #32027, 16.82106496071145685 ) ;
#88732 = FACE_OUTER_BOUND ( 'NONE', #61104, .T. ) ;
#88731 = CARTESIAN_POINT ( 'NONE',  ( 161.6755750489535046, 250.6166850027345276, -13.01404233079112061 ) ) ;
#88733 = CARTESIAN_POINT ( 'NONE',  ( 149.1429535397850827, 272.3238222086447990, -12.91457852089092384 ) ) ;
#88734 = VERTEX_POINT ( 'NONE', #99761 ) ;
#88735 = CARTESIAN_POINT ( 'NONE',  ( 206.7893622945242385, 272.4773133715531230, -10.52881283832460291 ) ) ;
#88736 = CARTESIAN_POINT ( 'NONE',  ( 159.2511875226268216, 254.8158473755685520, 15.75855490706745599 ) ) ;
#88737 = CARTESIAN_POINT ( 'NONE',  ( 72.74966122630479504, 56.93859335219654838, -15.92450643838010471 ) ) ;
#88738 = CARTESIAN_POINT ( 'NONE',  ( 77.86555730066851311, 62.20866292688850763, -15.95979438352862090 ) ) ;
#88739 = CARTESIAN_POINT ( 'NONE',  ( 205.2414727015710412, 275.1583367910551488, -12.71338796362297963 ) ) ;
#88740 = CARTESIAN_POINT ( 'NONE',  ( 123.0160347675418677, 232.6423013555409796, -4.594050593750043987 ) ) ;
#88741 = CARTESIAN_POINT ( 'NONE',  ( 106.7110898388691851, 243.9637435831425307, 2.679491924311251605 ) ) ;
#88742 = ADVANCED_FACE ( 'NONE', ( #30849 ), #76465, .T. ) ;
#88743 = ORIENTED_EDGE ( 'NONE', *, *, #40629, .T. ) ;
#88744 = CARTESIAN_POINT ( 'NONE',  ( 208.3152833949211526, 269.8343404973242059, 2.763633873278860342 ) ) ;
#88745 = ORIENTED_EDGE ( 'NONE', *, *, #44500, .F. ) ;
#88746 = CARTESIAN_POINT ( 'NONE',  ( 38.25529575686164208, 27.80170272979929535, 7.433330006724137462 ) ) ;
#88747 = CARTESIAN_POINT ( 'NONE',  ( 159.6978881494930249, 254.0421391940632532, 15.34888828951022610 ) ) ;
#88748 = CARTESIAN_POINT ( 'NONE',  ( 74.96244436416358781, 66.36905339528264847, -13.09731569639688509 ) ) ;
#88749 = EDGE_CURVE ( 'NONE', #46305, #68766, #70343, .T. ) ;
#88750 = CARTESIAN_POINT ( 'NONE',  ( 75.30318735596920021, 214.2833772461660544, -9.188101187500095079 ) ) ;
#88751 = EDGE_LOOP ( 'NONE', ( #88135, #93565, #78296, #24002 ) ) ;
#88752 = CARTESIAN_POINT ( 'NONE',  ( -73.83803415018344651, 50.74234351129840093, 10.00000000000000000 ) ) ;
#88753 = CARTESIAN_POINT ( 'NONE',  ( 191.2729698983822288, 299.3524933518466469, 8.871011392605806734 ) ) ;
#88754 = CARTESIAN_POINT ( 'NONE',  ( 193.9204722154232741, 294.7668848255750049, 15.43855698596013859 ) ) ;
#88755 = CARTESIAN_POINT ( 'NONE',  ( 171.8605515403996833, 276.6437741024603838, 16.15068646528671437 ) ) ;
#88756 = VERTEX_POINT ( 'NONE', #60721 ) ;
#88757 = CARTESIAN_POINT ( 'NONE',  ( 73.23650963592969276, 58.97240520736598768, -15.60991212256156402 ) ) ;
#88758 = DIRECTION ( 'NONE',  ( -0.000000000000000000, 1.000000000000000000, -0.000000000000000000 ) ) ;
#88759 = VECTOR ( 'NONE', #88203, 1000.000000000000000 ) ;
#88760 = ORIENTED_EDGE ( 'NONE', *, *, #86995, .T. ) ;
#88761 = CARTESIAN_POINT ( 'NONE',  ( 148.0169957629716464, 274.2740382852624634, 9.106122941397371662 ) ) ;
#88762 = CARTESIAN_POINT ( 'NONE',  ( 69.50635844379594630, 69.67114699658039001, -5.427956398610904287 ) ) ;
#88763 = EDGE_CURVE ( 'NONE', #82127, #73330, #36869, .T. ) ;
#88764 = CARTESIAN_POINT ( 'NONE',  ( 207.3874697692679945, 271.4413608369101780, -6.809237722377445401 ) ) ;
#88765 = DIRECTION ( 'NONE',  ( 0.9522021074858112444, 0.3054687324417666994, 0.000000000000000000 ) ) ;
#88766 = VECTOR ( 'NONE', #57846, 1000.000000000000000 ) ;
#88767 = CARTESIAN_POINT ( 'NONE',  ( 80.31808946940563487, 54.04802570103038306, 16.19007400800021301 ) ) ;
#88768 = VECTOR ( 'NONE', #86791, 1000.000000000000114 ) ;
#88769 = CARTESIAN_POINT ( 'NONE',  ( 164.2813349609167517, 246.1033764428878214, 1.949810150281061638 ) ) ;
#88770 = CARTESIAN_POINT ( 'NONE',  ( 206.1215120922853146, 273.6340638536760821, 10.12238414215620885 ) ) ;
#88771 = DIRECTION ( 'NONE',  ( 0.4999999999999998890, -0.8660254037844385966, 0.000000000000000000 ) ) ;
#88772 = CARTESIAN_POINT ( 'NONE',  ( 164.1998033881670551, 254.1351517766089501, 14.29502161760787438 ) ) ;
#88773 = ORIENTED_EDGE ( 'NONE', *, *, #85678, .T. ) ;
#88774 = CARTESIAN_POINT ( 'NONE',  ( 208.3132655666949233, 269.8378354783333180, 2.688523655043302707 ) ) ;
#88775 = AXIS2_PLACEMENT_3D ( 'NONE', #14790, #91330, #52290 ) ;
#88776 = CARTESIAN_POINT ( 'NONE',  ( 120.7695210546522446, 240.5333772461660544, 9.188101187500095079 ) ) ;
#88777 = ORIENTED_EDGE ( 'NONE', *, *, #73695, .F. ) ;
#88778 = CARTESIAN_POINT ( 'NONE',  ( 146.5095091551180815, 276.8850816817948726, 0.1418322875769769398 ) ) ;
#88779 = CARTESIAN_POINT ( 'NONE',  ( 87.40047971330913867, 221.2677522451418497, 10.00000000000009592 ) ) ;
#88780 = ADVANCED_FACE ( 'NONE', ( #37926 ), #92686, .T. ) ;
#88781 = FACE_BOUND ( 'NONE', #44113, .T. ) ;
#88782 = CARTESIAN_POINT ( 'NONE',  ( 74.53493183439029224, 59.86322019391595717, 15.61592258559468505 ) ) ;
#88783 = CYLINDRICAL_SURFACE ( 'NONE', #55067, 70.00000000000002842 ) ;
#88784 = ORIENTED_EDGE ( 'NONE', *, *, #64364, .F. ) ;
#88785 = CARTESIAN_POINT ( 'NONE',  ( 80.47734257382147405, 57.78184453145892263, -16.59809864164601478 ) ) ;
#88786 = VECTOR ( 'NONE', #49508, 1000.000000000000000 ) ;
#88787 = CARTESIAN_POINT ( 'NONE',  ( 71.94586788039056557, 72.25955706396953815, 0.6154238980746699061 ) ) ;
#88788 = CARTESIAN_POINT ( 'NONE',  ( -22.42236680055709641, 157.8615022471902591, 0.000000000000000000 ) ) ;
#88789 = CARTESIAN_POINT ( 'NONE',  ( 206.7044739906782809, 272.6243442267827959, -10.28926534613781030 ) ) ;
#88790 = CARTESIAN_POINT ( 'NONE',  ( 48.60927726968589013, 109.6985806698937012, -10.00000000000000000 ) ) ;
#88791 = CIRCLE ( 'NONE', #17488, 70.00000000000001421 ) ;
#88792 = DIRECTION ( 'NONE',  ( -0.8660254037844387076, -0.4999999999999998890, -0.000000000000000000 ) ) ;
#88793 = CARTESIAN_POINT ( 'NONE',  ( 152.7980788416505220, 279.6030702425718459, 0.5086631364502993691 ) ) ;
#88794 = B_SPLINE_CURVE_WITH_KNOTS ( 'NONE', 3,
 ( #89298, #3172, #34058, #4637, #64948, #87324, #65926, #95892, #96882, #81185, #73060, #3655, #26453, #4130, #57328, #88301, #18856, #79689, #34535, #57826, #19852, #88804, #50720, #81674, #17856, #50231, #43106, #2657, #10250, #41121 ),
 .UNSPECIFIED., .F., .F.,
 ( 4, 2, 2, 2, 2, 2, 2, 2, 2, 2, 2, 2, 2, 2, 4 ),
 ( 0.0004150180397800705846, 0.001518865485007307205, 0.002622712930234544042, 0.003174636652848163328, 0.003312617583501567715, 0.003381608048828311543, 0.003416103281491683456, 0.003450598514155055370, 0.003519588979481798330, 0.003588579444808541290, 0.003726560375461841594, 0.004002522236768397967, 0.004278484098074954341, 0.004554445959381510714, 0.004830407820688066220 ),
 .UNSPECIFIED. ) ;
#88795 = B_SPLINE_CURVE_WITH_KNOTS ( 'NONE', 3,
 ( #75942, #98739, #29318, #60185 ),
 .UNSPECIFIED., .F., .F.,
 ( 4, 4 ),
 ( 0.01394906585337539820, 0.02027515528328900640 ),
 .UNSPECIFIED. ) ;
#88796 = CARTESIAN_POINT ( 'NONE',  ( 157.8043799545718286, 257.3217915922150496, -17.97575562758749257 ) ) ;
#88797 = CARTESIAN_POINT ( 'NONE',  ( 174.6137999045392064, 252.0957045990745939, 3.527324166098372515 ) ) ;
#88798 = EDGE_CURVE ( 'NONE', #10180, #2192, #53635, .T. ) ;
#88799 = CARTESIAN_POINT ( 'NONE',  ( 19.03539854152464628, 16.15404122711133184, 8.090169943749479842 ) ) ;
#88800 = CARTESIAN_POINT ( 'NONE',  ( 148.9228818358559749, 272.7049975811580680, 12.13823097167056275 ) ) ;
#88801 = DIRECTION ( 'NONE',  ( 0.9995565931350004485, 0.02977611660964677234, 0.000000000000000000 ) ) ;
#88802 = CARTESIAN_POINT ( 'NONE',  ( 169.5047115304352872, 285.2286671053543614, -7.972866365725085558 ) ) ;
#88803 = CARTESIAN_POINT ( 'NONE',  ( 154.8786460229866577, 262.3893114111486398, -18.06164891362396929 ) ) ;
#88804 = CARTESIAN_POINT ( 'NONE',  ( 193.3797031396337047, 288.8503464183884262, 16.03552877166950452 ) ) ;
#88805 = EDGE_CURVE ( 'NONE', #82637, #23731, #93690, .T. ) ;
#88806 = CARTESIAN_POINT ( 'NONE',  ( 145.0633378486230072, 247.8927522451418213, 10.00000000000009592 ) ) ;
#88807 = CARTESIAN_POINT ( 'NONE',  ( 25.91265234538223439, 15.36477965099640919, 1.583844403245364907 ) ) ;
#88808 = ORIENTED_EDGE ( 'NONE', *, *, #70203, .F. ) ;
#88809 = EDGE_CURVE ( 'NONE', #36428, #40233, #28891, .T. ) ;
#88810 = CARTESIAN_POINT ( 'NONE',  ( 157.4656258344471098, 257.9085309395441641, 18.30485740784190796 ) ) ;
#88811 = CARTESIAN_POINT ( 'NONE',  ( 190.6071113721798156, 300.5057941498820924, -0.4754021072632813594 ) ) ;
#88812 = CARTESIAN_POINT ( 'NONE',  ( -6.590166341514275494, 160.8768266524160140, 9.188101187500096856 ) ) ;
#88813 = CIRCLE ( 'NONE', #11110, 14.21260523776213347 ) ;
#88814 = CARTESIAN_POINT ( 'NONE',  ( 40.58072100116311276, 203.4244531367911293, -4.594050593750046652 ) ) ;
#88815 = CARTESIAN_POINT ( 'NONE',  ( 178.9896671260052301, 258.6863495541695670, -11.59027018806768794 ) ) ;
#88816 = CARTESIAN_POINT ( 'NONE',  ( 24.15577373785222193, 19.11029122506294797, -8.090169943749478065 ) ) ;
#88817 = CARTESIAN_POINT ( 'NONE',  ( 34.93377400070185956, 197.6427522451419065, 10.00000000000009415 ) ) ;
#88818 = CARTESIAN_POINT ( 'NONE',  ( 157.4805323096970255, 257.8827121670497036, -16.70238855805511591 ) ) ;
#88819 = CARTESIAN_POINT ( 'NONE',  ( 72.21763474066925426, 71.89576300834814049, -3.847854183869324984 ) ) ;
#88820 = CARTESIAN_POINT ( 'NONE',  ( 190.5541309856500050, 300.5975588711562523, -4.167177996129430184 ) ) ;
#88821 = CARTESIAN_POINT ( 'NONE',  ( 73.89313514058181909, 55.59551747721973669, -16.58534802875433911 ) ) ;
#88822 = EDGE_CURVE ( 'NONE', #89585, #18415, #62227, .T. ) ;
#88824 = CARTESIAN_POINT ( 'NONE',  ( 65.24466313315720356, 215.1427522451419065, -10.00000000000009415 ) ) ;
#88823 = CARTESIAN_POINT ( 'NONE',  ( 172.6714394711437706, 279.8122014979473988, -15.90111829678659028 ) ) ;
#88825 = CARTESIAN_POINT ( 'NONE',  ( 75.87740499823547680, 55.03138904370663198, 16.59596780044815389 ) ) ;
#88826 = CARTESIAN_POINT ( 'NONE',  ( 30.89548221274965556, 26.03677371833803633, 10.00000000000000533 ) ) ;
#88827 = CARTESIAN_POINT ( 'NONE',  ( 171.1295603993285965, 249.6517061031812545, 4.344809613321301889 ) ) ;
#88828 = ADVANCED_BREP_SHAPE_REPRESENTATION ( '', ( #10898, #68784 ), #54221 ) ;
#88829 = CARTESIAN_POINT ( 'NONE',  ( 35.52916646935157274, 197.9865022471903160, -10.00000000000009415 ) ) ;
#88830 = CARTESIAN_POINT ( 'NONE',  ( 182.7818713244062678, 292.2108625818275982, 9.360646295977867126 ) ) ;
#88831 = CARTESIAN_POINT ( 'NONE',  ( 149.7178657912151607, 271.8703460001313488, -11.47881117598261369 ) ) ;
#88832 = AXIS2_PLACEMENT_3D ( 'NONE', #17460, #8369, #1780 ) ;
#88833 = CARTESIAN_POINT ( 'NONE',  ( -0.3657822996961275219, 170.5958772461660544, -9.188101187500095079 ) ) ;
#88834 = CARTESIAN_POINT ( 'NONE',  ( 30.44305165777243971, 40.68290643055189548, 3.479690158560446702E-15 ) ) ;
#88835 = CARTESIAN_POINT ( 'NONE',  ( 6.089871667348707440, 48.19321075732142390, 59.99999999999999289 ) ) ;
#88836 = CARTESIAN_POINT ( 'NONE',  ( 152.7153488183568300, 266.1362520814392951, 17.33540622643059237 ) ) ;
#88837 = CARTESIAN_POINT ( 'NONE',  ( 36.41017387241338810, 23.94754757982092030, 5.678558825948272215 ) ) ;
#88838 = CARTESIAN_POINT ( 'NONE',  ( 75.41814989884494480, 225.8967562850346837, -4.648177544792955347E-16 ) ) ;
#88840 = CARTESIAN_POINT ( 'NONE',  ( 179.4126076325937902, 277.4822272090366369, 16.59173480958843072 ) ) ;
#88839 = AXIS2_PLACEMENT_3D ( 'NONE', #20759, #6546, #7030 ) ;
#88841 = CARTESIAN_POINT ( 'NONE',  ( 196.4170778717353585, 290.4426369823788718, -17.78762421190030452 ) ) ;
#88842 = CARTESIAN_POINT ( 'NONE',  ( 87.93887446415499198, 44.76116579897428238, -4.704258403839747693 ) ) ;
#88843 = AXIS2_PLACEMENT_3D ( 'NONE', #13468, #74289, #59526 ) ;
#88844 = CARTESIAN_POINT ( 'NONE',  ( 7.128892988474023085, 19.51421378149916563, -9.188101187500004485 ) ) ;
#88845 = CARTESIAN_POINT ( 'NONE',  ( 71.90360357134966307, 72.59530952775405410, 1.145984468326222805 ) ) ;
#88846 = CARTESIAN_POINT ( 'NONE',  ( 12.64980493759981250, 22.70171378149917985, -9.188101187500004485 ) ) ;
#88847 = CARTESIAN_POINT ( 'NONE',  ( 159.1258744071607225, 259.4344880999452130, 16.68999608692717018 ) ) ;
#88848 = CARTESIAN_POINT ( 'NONE',  ( 193.7261517370125432, 295.1034577671335342, 14.97744313279139661 ) ) ;
#88849 = VERTEX_POINT ( 'NONE', #23236 ) ;
#88850 = AXIS2_PLACEMENT_3D ( 'NONE', #89947, #45292, #76226 ) ;
#88851 = CARTESIAN_POINT ( 'NONE',  ( 156.8438492009701974, 276.4973248573016349, 10.30341974258334936 ) ) ;
#88852 = CARTESIAN_POINT ( 'NONE',  ( 81.09965965012654010, 42.48948382993172856, 7.836446954449344915 ) ) ;
#88853 = FACE_OUTER_BOUND ( 'NONE', #43571, .T. ) ;
#88854 = EDGE_LOOP ( 'NONE', ( #47769, #74767, #39915, #31264 ) ) ;
#88855 = CARTESIAN_POINT ( 'NONE',  ( 192.1640094933931096, 297.8091675017319062, 12.36911124822534447 ) ) ;
#88856 = CARTESIAN_POINT ( 'NONE',  ( 207.2383675728608239, 271.6996134166075763, 7.873592648726489784 ) ) ;
#88857 = CARTESIAN_POINT ( 'NONE',  ( 66.48584631922960853, 68.21027895571930344, 4.536531987665620491 ) ) ;
#88858 = CARTESIAN_POINT ( 'NONE',  ( 87.14442862271327783, 45.34583212582730738, 7.067040553115585766 ) ) ;
#88859 = VERTEX_POINT ( 'NONE', #30351 ) ;
#88860 = VECTOR ( 'NONE', #67480, 1000.000000000000227 ) ;
#88861 = VERTEX_POINT ( 'NONE', #8555 ) ;
#88863 = CARTESIAN_POINT ( 'NONE',  ( -19.65312891409030271, 93.06504152958497400, -10.00000000000000888 ) ) ;
#88862 = CARTESIAN_POINT ( 'NONE',  ( 159.7486141406463673, 278.6331531155009884, -9.641193493407582693 ) ) ;
#88864 = CARTESIAN_POINT ( 'NONE',  ( 152.9920137376499838, 265.6570543845515431, 16.15798175643282164 ) ) ;
#88865 = ORIENTED_EDGE ( 'NONE', *, *, #1085, .T. ) ;
#88866 = CARTESIAN_POINT ( 'NONE',  ( 77.58762503914641684, 56.56502062187109914, 16.17780933088086925 ) ) ;
#88867 = CARTESIAN_POINT ( 'NONE',  ( 174.6563431587044590, 262.3393413554219933, 14.36283845981329144 ) ) ;
#88868 = EDGE_LOOP ( 'NONE', ( #9940, #54114, #92599, #59622 ) ) ;
#88869 = DIRECTION ( 'NONE',  ( 0.3693965786901519111, -0.9292718480896805522, 0.000000000000000000 ) ) ;
#88870 = CARTESIAN_POINT ( 'NONE',  ( 80.90528918492583443, 217.5177522451418497, -10.00000000000009592 ) ) ;
#88871 = B_SPLINE_CURVE_WITH_KNOTS ( 'NONE', 3,
 ( #31204, #24111, #100136, #77833, #37802, #91552, #77322, #8416, #55004, #69708, #7408, #39780, #68710, #39288, #93550, #316, #93039, #84951, #23595, #70198, #69210, #62595, #85467, #53013, #16012, #76341, #6914, #92073, #99636, #22623, #84462, #76814, #30218, #61101 ),
 .UNSPECIFIED., .F., .F.,
 ( 4, 2, 2, 2, 2, 2, 2, 2, 2, 2, 2, 2, 2, 2, 2, 2, 4 ),
 ( 0.001328748612904130048, 0.001671321452974920511, 0.002013894293045710542, 0.002699039973187349582, 0.004069331333470678838, 0.004754477013612343900, 0.005097049853683153012, 0.005268336273718570578, 0.005353979483736278494, 0.005396801088745134187, 0.005439622693753988145, 0.005525265903771676979, 0.005610909113789364078, 0.005782195533824741746, 0.006124768373895498816, 0.006467341213966254151, 0.006809914054037011222 ),
 .UNSPECIFIED. ) ;
#88872 = CARTESIAN_POINT ( 'NONE',  ( 196.6800254274587019, 289.9871984561398222, -17.90749311895638129 ) ) ;
#88873 = VECTOR ( 'NONE', #94758, 1000.000000000000000 ) ;
#88874 = CARTESIAN_POINT ( 'NONE',  ( 39.33606980327277824, 193.5177522451418781, -10.00000000000009592 ) ) ;
#88875 = EDGE_CURVE ( 'NONE', #24654, #96030, #65936, .T. ) ;
#88876 = ORIENTED_EDGE ( 'NONE', *, *, #98251, .T. ) ;
#88877 = CARTESIAN_POINT ( 'NONE',  ( 161.6256441450323678, 250.7031678651938762, 14.48526717260977037 ) ) ;
#88878 = CARTESIAN_POINT ( 'NONE',  ( 82.93017357788673394, 175.3855496052738374, -21.50000000000000000 ) ) ;
#88879 = CARTESIAN_POINT ( 'NONE',  ( 73.13476967714908028, 57.39438153525127007, 15.88807208273858684 ) ) ;
#88880 = B_SPLINE_SURFACE_WITH_KNOTS ( 'NONE', 3, 1, ( 
 ( #18455, #49343 ),
 ( #41726, #72671 ),
 ( #38606, #6724 ),
 ( #125, #46194 ),
 ( #84755, #30013 ),
 ( #53310, #98448 ),
 ( #21429, #98943 ),
 ( #45696, #15294 ),
 ( #76623, #82778 ),
 ( #7209, #67518 ),
 ( #30517, #14812 ),
 ( #29526, #22419 ),
 ( #5723, #44702 ),
 ( #92359, #77110 ),
 ( #36611, #60898 ),
 ( #13344, #69511 ),
 ( #60398, #59401 ),
 ( #29039, #91354 ),
 ( #53794, #76150 ),
 ( #84265, #99436 ),
 ( #90377, #68515 ),
 ( #91862, #21917 ),
 ( #38092, #7714 ),
 ( #37115, #61406 ),
 ( #20955, #51838 ),
 ( #44209, #69004 ),
 ( #75145, #99933 ),
 ( #52806, #59910 ),
 ( #90881, #22907 ),
 ( #52316, #83763 ),
 ( #83255, #13822 ) ),
 .UNSPECIFIED., .F., .F., .F.,
 ( 4, 3, 3, 3, 3, 3, 3, 3, 3, 3, 4 ),
 ( 2, 2 ),
 ( 0.000000000000000000, 0.1122669598086770831, 0.2243161639709709554, 0.3396355846219147323, 0.4553962076585074126, 0.5677860799922471724, 0.6749047109689605417, 0.7773884377078307262, 0.8775581155834273339, 0.9782364162377794603, 1.000000000000000000 ),
 ( 0.000000000000000000, 1.000000000000000000 ),
 .UNSPECIFIED. ) ;
#88881 = VERTEX_POINT ( 'NONE', #91684 ) ;
#88882 = CARTESIAN_POINT ( 'NONE',  ( 148.9228818358559749, 272.7049975811580680, 12.13823097167056275 ) ) ;
#88883 = EDGE_CURVE ( 'NONE', #50922, #19773, #39423, .T. ) ;
#88884 = ORIENTED_EDGE ( 'NONE', *, *, #19225, .F. ) ;
#88885 = CARTESIAN_POINT ( 'NONE',  ( 160.3232326710177063, 268.8205896071553980, -16.66338050398602277 ) ) ;
#88886 = EDGE_LOOP ( 'NONE', ( #93082, #57374, #35580, #54885, #73146 ) ) ;
#88887 = CARTESIAN_POINT ( 'NONE',  ( 158.7190333866803655, 269.4707014042647302, 15.62828681828240107 ) ) ;
#88888 = VERTEX_POINT ( 'NONE', #14656 ) ;
#88889 = CARTESIAN_POINT ( 'NONE',  ( 158.8065584601817477, 260.0459917420977263, 17.43621632757881557 ) ) ;
#88890 = CARTESIAN_POINT ( 'NONE',  ( 193.7606469113726462, 295.0437103725260499, 14.91128319924638745 ) ) ;
#88891 = CARTESIAN_POINT ( 'NONE',  ( 19.18375657693640335, 36.32959363016014720, 10.00000000000000000 ) ) ;
#88892 = CARTESIAN_POINT ( 'NONE',  ( 12.29152061481545566, 25.83478043621387243, -8.090169943749479842 ) ) ;
#88893 = CARTESIAN_POINT ( 'NONE',  ( 193.7173197858508900, 294.7288552955487830, 13.42109144984733682 ) ) ;
#88894 = EDGE_CURVE ( 'NONE', #82087, #73983, #70796, .T. ) ;
#88895 = CARTESIAN_POINT ( 'NONE',  ( 178.3444744936179518, 291.9204168475665711, 7.080535521235421292 ) ) ;
#88896 = CARTESIAN_POINT ( 'NONE',  ( 197.0367503649972036, 289.3693327399964801, -16.94195272704401845 ) ) ;
#88897 = ORIENTED_EDGE ( 'NONE', *, *, #57683, .F. ) ;
#88898 = LINE ( 'NONE', #71653, #51237 ) ;
#88899 = CARTESIAN_POINT ( 'NONE',  ( 29.87828763904599683, 19.11110640527293469, -2.839279412974138328 ) ) ;
#88900 = CARTESIAN_POINT ( 'NONE',  ( 87.85384634344086408, 209.9824982072973967, 3.021315404115420679E-15 ) ) ;
#88902 = CARTESIAN_POINT ( 'NONE',  ( 164.7462163020046262, 245.2981783406326599, 1.451255823150352064 ) ) ;
#88901 = CARTESIAN_POINT ( 'NONE',  ( 30.54350413710242051, 75.98152451519752049, 59.99999999999999289 ) ) ;
#88903 = CARTESIAN_POINT ( 'NONE',  ( 198.4772197948566372, 286.8743665007300478, 18.43646439804394532 ) ) ;
#88904 = ORIENTED_EDGE ( 'NONE', *, *, #88410, .T. ) ;
#88905 = CARTESIAN_POINT ( 'NONE',  ( 190.3865446062718547, 300.8878269948957040, 5.596937249297124772 ) ) ;
#88906 = CARTESIAN_POINT ( 'NONE',  ( 171.4730959963652595, 259.7561518679366372, -14.77276439450797696 ) ) ;
#88907 = DIRECTION ( 'NONE',  ( -0.8660254037844387076, -0.4999999999999998890, -0.000000000000000000 ) ) ;
#88908 = EDGE_CURVE ( 'NONE', #83705, #23987, #88998, .T. ) ;
#88909 = FACE_OUTER_BOUND ( 'NONE', #24612, .T. ) ;
#88910 = ADVANCED_FACE ( 'NONE', ( #38433 ), #53147, .F. ) ;
#88911 = B_SPLINE_CURVE_WITH_KNOTS ( 'NONE', 3,
 ( #46924, #86485, #8425, #61611, #47904, #78844, #31698, #55012, #93558, #45902, #24124, #9428, #94558, #85992, #47414, #16519 ),
 .UNSPECIFIED., .F., .F.,
 ( 4, 1, 2, 2, 2, 1, 2, 2, 4 ),
 ( 0.000000000000000000, 0.1249999999999982792, 0.1874999999999990286, 0.2499999999999997780, 0.5000000000000002220, 0.6250000000000003331, 0.6875000000000003331, 0.7500000000000002220, 1.000000000000000000 ),
 .UNSPECIFIED. ) ;
#88912 = CARTESIAN_POINT ( 'NONE',  ( 160.1913727725009835, 253.1873987542595614, -16.21806651737331251 ) ) ;
#88913 = CARTESIAN_POINT ( 'NONE',  ( 190.4876730617585849, 300.7126673719016594, -1.247921881438171621 ) ) ;
#88914 = ORIENTED_EDGE ( 'NONE', *, *, #52522, .F. ) ;
#88915 = CARTESIAN_POINT ( 'NONE',  ( 167.3930310403720796, 252.8207621138501224, -12.36123731186929930 ) ) ;
#88916 = CARTESIAN_POINT ( 'NONE',  ( -22.42236680055709641, 157.8615022471902591, 0.000000000000000000 ) ) ;
#88917 = CARTESIAN_POINT ( 'NONE',  ( 201.1060504099706350, 282.3210983108598384, -18.18000168485860257 ) ) ;
#88918 = VECTOR ( 'NONE', #88409, 1000.000000000000000 ) ;
#88919 = CARTESIAN_POINT ( 'NONE',  ( 207.1059763530604698, 271.9289217357780899, 6.370907250589925575 ) ) ;
#88920 = CARTESIAN_POINT ( 'NONE',  ( 38.03703169759616287, 182.7677522451417929, -5.000000000000041744 ) ) ;
#88921 = CARTESIAN_POINT ( 'NONE',  ( 109.2678814824639204, 224.7048013555410080, 4.594050593750051981 ) ) ;
#88922 = CARTESIAN_POINT ( 'NONE',  ( 183.9211145108844221, 296.5969538952800235, -2.738914410665766130 ) ) ;
#88923 = VECTOR ( 'NONE', #17992, 1000.000000000000000 ) ;
#88924 = CARTESIAN_POINT ( 'NONE',  ( 164.0550791845173535, 280.3860225496770795, -11.45558117589946612 ) ) ;
#88925 = CARTESIAN_POINT ( 'NONE',  ( 84.80172950927561715, 50.19486025153374698, 13.34007759942641336 ) ) ;
#88926 = CARTESIAN_POINT ( 'NONE',  ( 208.2018443082727970, 270.0308227589636090, 1.727811837614598556 ) ) ;
#88927 = CARTESIAN_POINT ( 'NONE',  ( 10.56744132731740216, 189.1589784336661637, -6.496448406907675876E-16 ) ) ;
#88928 = CARTESIAN_POINT ( 'NONE',  ( 47.49582885874516336, 78.29235751436857527, 10.00000000000000000 ) ) ;
#88929 = ORIENTED_EDGE ( 'NONE', *, *, #29714, .F. ) ;
#88930 = VECTOR ( 'NONE', #41223, 1000.000000000000000 ) ;
#88931 = ORIENTED_EDGE ( 'NONE', *, *, #84658, .F. ) ;
#88932 = CARTESIAN_POINT ( 'NONE',  ( 73.83553503644242255, 68.51229284434135991, 11.41127707145445491 ) ) ;
#88933 = CARTESIAN_POINT ( 'NONE',  ( 185.1797296270955542, 259.8357583151453696, -5.558726417257365604 ) ) ;
#88934 = FACE_OUTER_BOUND ( 'NONE', #43329, .T. ) ;
#88935 = CARTESIAN_POINT ( 'NONE',  ( 45.29894525614687950, 66.96469553601605185, 177.5919119679930134 ) ) ;
#88936 = CARTESIAN_POINT ( 'NONE',  ( 193.0398521437286377, 263.8906099786534583, -4.323427293014181494 ) ) ;
#88937 = CARTESIAN_POINT ( 'NONE',  ( 4.482002306134333480, 24.36126292948892669, 6.180339887498949913 ) ) ;
#88938 = AXIS2_PLACEMENT_3D ( 'NONE', #81844, #74233, #15239 ) ;
#88939 = CARTESIAN_POINT ( 'NONE',  ( 182.3656953904154534, 284.2887812106879437, 14.91155821018728034 ) ) ;
#88940 = DIRECTION ( 'NONE',  ( 0.5000000000000006661, -0.8660254037844383745, 2.435752736085845824E-15 ) ) ;
#88941 = ADVANCED_FACE ( 'NONE', ( #26750 ), #63249, .T. ) ;
#88942 = CARTESIAN_POINT ( 'NONE',  ( 42.06911538997637479, 207.3464784336661637, 1.353441290958777525E-15 ) ) ;
#88943 = CARTESIAN_POINT ( 'NONE',  ( 102.5559242795368391, 220.0177522451417929, 5.000000000000051514 ) ) ;
#88944 = ORIENTED_EDGE ( 'NONE', *, *, #57176, .T. ) ;
#88945 = CARTESIAN_POINT ( 'NONE',  ( 150.0670708984111457, 271.4758772266419555, -12.06937736578899312 ) ) ;
#88946 = ADVANCED_FACE ( 'NONE', ( #71367 ), #32348, .F. ) ;
#88947 = ADVANCED_FACE ( 'NONE', ( #64247 ), #94684, .T. ) ;
#88948 = AXIS2_PLACEMENT_3D ( 'NONE', #67699, #37778, #6888 ) ;
#88949 = CARTESIAN_POINT ( 'NONE',  ( 2.719259653403430121, 178.5024278399160949, -9.188101187500093303 ) ) ;
#88950 = ADVANCED_FACE ( 'NONE', ( #49057 ), #95197, .T. ) ;
#88951 = CARTESIAN_POINT ( 'NONE',  ( 68.71802935033312565, 64.09262139948224046, -11.98471630605159177 ) ) ;
#88952 = CARTESIAN_POINT ( 'NONE',  ( 150.6386650955079176, 269.7331738006648720, -15.06054658539322766 ) ) ;
#88953 = CARTESIAN_POINT ( 'NONE',  ( 80.92193103463624482, 53.39041974847280159, 15.96582457958936274 ) ) ;
#88954 = CARTESIAN_POINT ( 'NONE',  ( 193.0142717932987182, 296.3364699985351081, -13.30037542329744937 ) ) ;
#88955 = CARTESIAN_POINT ( 'NONE',  ( 182.0312531846501258, 257.2221692175513112, -7.485986072910417732 ) ) ;
#88956 = CARTESIAN_POINT ( 'NONE',  ( 203.6760479211504276, 276.2018596621056190, 13.30539550760933132 ) ) ;
#88957 = CARTESIAN_POINT ( 'NONE',  ( 68.43296295610389279, 66.95241442033321277, 8.990821635125779920 ) ) ;
#88958 = CARTESIAN_POINT ( 'NONE',  ( 206.9059968923335475, 272.2752963222270068, 6.902135944297345560 ) ) ;
#88959 = ORIENTED_EDGE ( 'NONE', *, *, #21901, .F. ) ;
#88960 = CARTESIAN_POINT ( 'NONE',  ( 1.754175721758462370, 178.4865022471903728, -10.00000000000009415 ) ) ;
#88961 = B_SPLINE_CURVE_WITH_KNOTS ( 'NONE', 3,
 ( #46333, #77257, #7865, #71683, #93998, #48365, #40237, #751, #54428, #85404, #8853, #71178, #23535, #64058, #39722, #87444, #31634, #16946, #56452, #8364, #33156, #62535, #95002, #25563, #17455, #72177, #47833, #1775, #55926, #2275, #24053, #86922, #79805, #93494, #79312, #9881, #32654, #17977, #10369, #48871, #54948, #85925, #15952, #78270 ),
 .UNSPECIFIED., .F., .F.,
 ( 4, 2, 2, 2, 2, 2, 2, 2, 2, 2, 2, 2, 2, 2, 2, 2, 2, 2, 2, 2, 2, 4 ),
 ( 0.002346744725963096061, 0.002773758852798046456, 0.002987265916215522087, 0.003094019447924267058, 0.003200772979633012896, 0.003307526511341757867, 0.003414280043050503272, 0.003627787106467994516, 0.004054801233303112311, 0.004908829486973232542, 0.005762857740643351906, 0.006616885994313471270, 0.007043900121148489318, 0.007470914247983505632, 0.007577667779692260144, 0.007631044545546630462, 0.007684421311401002513, 0.007791174843109744882, 0.007897928374818488986, 0.008324942501653435911, 0.008751956628488386306, 0.009178970755323333230 ),
 .UNSPECIFIED. ) ;
#88962 = CARTESIAN_POINT ( 'NONE',  ( 1.233819684896646951, 25.98176417558038764, -10.00000000000000000 ) ) ;
#88963 = CARTESIAN_POINT ( 'NONE',  ( 124.6666353716822186, 242.7833772461660544, -9.188101187500095079 ) ) ;
#88964 = CARTESIAN_POINT ( 'NONE',  ( 17.13451663979182626, 31.93396525600390135, 2.839279412974139660 ) ) ;
#88965 = CARTESIAN_POINT ( 'NONE',  ( 74.81608510805732237, 67.12708246140779522, 12.96692076351790490 ) ) ;
#88966 = DIRECTION ( 'NONE',  ( -0.000000000000000000, 0.000000000000000000, -1.000000000000000000 ) ) ;
#88968 = PLANE ( 'NONE',  #50608 ) ;
#88967 = CARTESIAN_POINT ( 'NONE',  ( -24.63924516542738274, 141.7012482093459198, -1.732050807568746853 ) ) ;
#88969 = CARTESIAN_POINT ( 'NONE',  ( 190.5994576334820181, 300.5190508141740793, -7.527957223721390534 ) ) ;
#88970 = ORIENTED_EDGE ( 'NONE', *, *, #72707, .F. ) ;
#88971 = CARTESIAN_POINT ( 'NONE',  ( 151.4025156491502742, 268.4101458323662541, 14.71049357081981235 ) ) ;
#88972 = CARTESIAN_POINT ( 'NONE',  ( 207.6314056968649595, 271.0188514165208744, -1.280821594136880126 ) ) ;
#88973 = LINE ( 'NONE', #84325, #57205 ) ;
#88974 = CARTESIAN_POINT ( 'NONE',  ( 169.5601139872289309, 266.0306789591197116, -17.01818431075402671 ) ) ;
#88975 = CARTESIAN_POINT ( 'NONE',  ( 81.74618951931624622, 55.66798611840641087, -15.97864541239357727 ) ) ;
#88976 = ORIENTED_EDGE ( 'NONE', *, *, #56222, .F. ) ;
#88977 = CARTESIAN_POINT ( 'NONE',  ( 71.68087887753404175, 71.27905009602892505, 4.678563896432837765 ) ) ;
#88978 = CARTESIAN_POINT ( 'NONE',  ( 168.4739816692278396, 271.7343923863479063, -17.32961767935828590 ) ) ;
#88979 = CARTESIAN_POINT ( 'NONE',  ( 71.80888402837304341, 72.55032655444115619, 1.016447747306864269 ) ) ;
#88980 = CARTESIAN_POINT ( 'NONE',  ( 83.66549642538166154, 42.56717918585069782, 5.117918876049285970 ) ) ;
#88981 = CARTESIAN_POINT ( 'NONE',  ( 80.02440815614393443, 53.77024961372720924, 15.74125996130883465 ) ) ;
#88983 = CARTESIAN_POINT ( 'NONE',  ( 185.5205021638500114, 297.3465265719306103, 5.673669933437759383 ) ) ;
#88982 = B_SPLINE_CURVE_WITH_KNOTS ( 'NONE', 3,
 ( #47323, #24025, #46831, #54924 ),
 .UNSPECIFIED., .F., .F.,
 ( 4, 4 ),
 ( 0.01057495740738979666, 0.01616209098191098009 ),
 .UNSPECIFIED. ) ;
#88984 = DIRECTION ( 'NONE',  ( 0.5000000000000003331, -0.8660254037844385966, 0.000000000000000000 ) ) ;
#88985 = CARTESIAN_POINT ( 'NONE',  ( 149.1326317111226558, 276.5594127424867565, -0.0002112342455116459836 ) ) ;
#88986 = CARTESIAN_POINT ( 'NONE',  ( 194.1909060474912110, 282.8098373099740570, 17.20683189011229430 ) ) ;
#88987 = CARTESIAN_POINT ( 'NONE',  ( 42.85004829832550399, 33.24335787977766188, -9.188101187500008038 ) ) ;
#88988 = CARTESIAN_POINT ( 'NONE',  ( 173.8490933012782307, 272.4998881216204154, -16.42193024097150200 ) ) ;
#88989 = ORIENTED_EDGE ( 'NONE', *, *, #24292, .F. ) ;
#88990 = CYLINDRICAL_SURFACE ( 'NONE', #78978, 17.82106496071139645 ) ;
#88991 = EDGE_CURVE ( 'NONE', #9838, #21251, #91268, .T. ) ;
#88992 = CARTESIAN_POINT ( 'NONE',  ( 197.7196744852244876, 271.6120449130532393, 13.56729386884406630 ) ) ;
#88993 = CARTESIAN_POINT ( 'NONE',  ( 156.2033007795417348, 262.0734030644348991, -16.95518515663351877 ) ) ;
#88994 = VERTEX_POINT ( 'NONE', #10058 ) ;
#88995 = VECTOR ( 'NONE', #2944, 1000.000000000000000 ) ;
#88996 = CARTESIAN_POINT ( 'NONE',  ( 46.74097198175142154, 116.0488203434314727, -10.00000000000000000 ) ) ;
#88997 = LINE ( 'NONE', #19550, #18485 ) ;
#88998 = B_SPLINE_CURVE_WITH_KNOTS ( 'NONE', 3,
 ( #76940, #24253, #29852, #45533 ),
 .UNSPECIFIED., .F., .F.,
 ( 4, 4 ),
 ( 0.02742407849190809863, 0.03663494907973673109 ),
 .UNSPECIFIED. ) ;
#88999 = LINE ( 'NONE', #28605, #59350 ) ;
#89000 = CARTESIAN_POINT ( 'NONE',  ( -22.42236680055716036, 157.8615022471903444, 5.188172501216621122E-14 ) ) ;
#89001 = ORIENTED_EDGE ( 'NONE', *, *, #1566, .T. ) ;
#89002 = CARTESIAN_POINT ( 'NONE',  ( 91.40610752940987993, 214.3923013555409796, 4.594050593750050204 ) ) ;
#89003 = AXIS2_PLACEMENT_3D ( 'NONE', #53470, #74932, #42497 ) ;
#89004 = CARTESIAN_POINT ( 'NONE',  ( 79.04618249573870514, 51.69161574664858705, -15.34666239050040026 ) ) ;
#89005 = CYLINDRICAL_SURFACE ( 'NONE', #16495, 10.00000000000010658 ) ;
#89006 = CARTESIAN_POINT ( 'NONE',  ( 185.2750378117470689, 259.6499128198802282, -6.774890732820249895 ) ) ;
#89007 = ORIENTED_EDGE ( 'NONE', *, *, #19483, .T. ) ;
#89008 = VERTEX_POINT ( 'NONE', #94190 ) ;
#89009 = CARTESIAN_POINT ( 'NONE',  ( 92.93017357788669131, 158.0650415295850735, 36.50000000000000000 ) ) ;
#89010 = EDGE_LOOP ( 'NONE', ( #9941, #29344, #82613, #23534 ) ) ;
#89011 = FACE_OUTER_BOUND ( 'NONE', #52024, .T. ) ;
#89012 = ORIENTED_EDGE ( 'NONE', *, *, #30530, .F. ) ;
#89013 = CARTESIAN_POINT ( 'NONE',  ( 33.63407072503001416, 49.62913085183823370, -10.00000000000000000 ) ) ;
#89015 = CARTESIAN_POINT ( 'NONE',  ( 155.0304386007204016, 262.1263989543018056, -17.12961552904782181 ) ) ;
#89014 = VECTOR ( 'NONE', #90005, 1000.000000000000114 ) ;
#89016 = ORIENTED_EDGE ( 'NONE', *, *, #91671, .F. ) ;
#89017 = CARTESIAN_POINT ( 'NONE',  ( 182.8048260423933584, 279.9985300298516790, -16.23004993202965807 ) ) ;
#89018 = CARTESIAN_POINT ( 'NONE',  ( 81.94547001506749950, 41.15136089338242442, 3.786739421817370665 ) ) ;
#89019 = CARTESIAN_POINT ( 'NONE',  ( 161.3257284758417143, 277.4216702933620695, -13.36329991415315455 ) ) ;
#89020 = CARTESIAN_POINT ( 'NONE',  ( 24.69086998626516305, 38.90223361192549589, -10.00000000000000000 ) ) ;
#89021 = DIRECTION ( 'NONE',  ( -0.8660254037844377084, -0.5000000000000014433, -0.000000000000000000 ) ) ;
#89022 = EDGE_CURVE ( 'NONE', #21377, #43244, #16645, .T. ) ;
#89023 = CARTESIAN_POINT ( 'NONE',  ( 5.723458822437168081, 174.1115022471902591, 10.00000000000009592 ) ) ;
#89024 = CARTESIAN_POINT ( 'NONE',  ( 148.2390246527636748, 247.2048013555409511, 4.594050593750051981 ) ) ;
#89025 = ORIENTED_EDGE ( 'NONE', *, *, #51197, .T. ) ;
#89026 = CARTESIAN_POINT ( 'NONE',  ( 70.70031318904726447, 61.05212235982030933, -14.44737232470619404 ) ) ;
#89027 = CARTESIAN_POINT ( 'NONE',  ( 6.007877864960585512, 21.65586893147753855, -7.433330006724137462 ) ) ;
#89028 = EDGE_LOOP ( 'NONE', ( #92950, #52556, #95676, #89846 ) ) ;
#89029 = AXIS2_PLACEMENT_3D ( 'NONE', #33206, #64105, #77826 ) ;
#89031 = ORIENTED_EDGE ( 'NONE', *, *, #6687, .T. ) ;
#89030 = CARTESIAN_POINT ( 'NONE',  ( 200.4530980307013124, 270.4255315980906289, 9.273059835868647127 ) ) ;
#89032 = CARTESIAN_POINT ( 'NONE',  ( -14.04074883167679566, 104.9358293318823456, 10.41391694355407083 ) ) ;
#89033 = FACE_OUTER_BOUND ( 'NONE', #21615, .T. ) ;
#89034 = CARTESIAN_POINT ( 'NONE',  ( 127.7428297729342717, 237.8927522451417929, -10.00000000000009237 ) ) ;
#89035 = FACE_OUTER_BOUND ( 'NONE', #95738, .T. ) ;
#89036 = EDGE_CURVE ( 'NONE', #10368, #100061, #25769, .T. ) ;
#89037 = CARTESIAN_POINT ( 'NONE',  ( 83.12008827683904144, 49.71316083303308631, -14.04899104105282603 ) ) ;
#89038 =( BOUNDED_CURVE ( )  B_SPLINE_CURVE ( 2, ( #47676, #85760, #24395, #39563, #72007, #95358, #23879, #16289, #87769 ),
 .UNSPECIFIED., .F., .T. ) 
 B_SPLINE_CURVE_WITH_KNOTS ( ( 3, 2, 2, 2, 3 ),
 ( 0.6491935483870967527, 0.6505376344086021279, 0.6532258064516128782, 0.6559139784946236285, 0.6572580645161290036 ),
 .UNSPECIFIED. ) 
 CURVE ( )  GEOMETRIC_REPRESENTATION_ITEM ( )  RATIONAL_B_SPLINE_CURVE ( ( 0.9330127018922194093, 0.9330127018922194093, 1.000000000000000000, 0.8660254037844387076, 1.000000000000000000, 0.8660254037844387076, 1.000000000000000000, 0.9330127018922194093, 0.9330127018922194093 ) ) 
 REPRESENTATION_ITEM ( '' )  );
#89039 = CARTESIAN_POINT ( 'NONE',  ( 174.7756533518544302, 282.0975554114792203, 14.28861982422490762 ) ) ;
#89040 = EDGE_CURVE ( 'NONE', #69469, #98279, #24744, .T. ) ;
#89041 = LINE ( 'NONE', #11489, #32139 ) ;
#89042 = CARTESIAN_POINT ( 'NONE',  ( 88.21629111658447187, 43.86250281267856366, -2.113840622537501268 ) ) ;
#89043 = ORIENTED_EDGE ( 'NONE', *, *, #72853, .F. ) ;
#89044 = CARTESIAN_POINT ( 'NONE',  ( 184.1103630465501624, 272.4158174899661731, -17.30342150099949450 ) ) ;
#89045 = CARTESIAN_POINT ( 'NONE',  ( 66.16044157329372410, 68.77389650870436810, 0.09421816583955693047 ) ) ;
#89046 = ORIENTED_EDGE ( 'NONE', *, *, #36705, .F. ) ;
#89047 = CARTESIAN_POINT ( 'NONE',  ( 194.2102773769292128, 293.8493148023329127, -14.16464662972703614 ) ) ;
#89048 = CARTESIAN_POINT ( 'NONE',  ( 200.9384910137331417, 267.7722853946023065, -2.751277086281960216 ) ) ;
#89049 = PLANE ( 'NONE',  #67657 ) ;
#89050 = CARTESIAN_POINT ( 'NONE',  ( -19.65312891409030271, 93.06504152958497400, 10.00000000000000888 ) ) ;
#89051 = CARTESIAN_POINT ( 'NONE',  ( 164.0982892389591825, 274.1344140775349842, 14.77298282198140456 ) ) ;
#89053 = CARTESIAN_POINT ( 'NONE',  ( 88.09744597521934395, 43.85530739230785002, 2.493575494356675915 ) ) ;
#89052 = CARTESIAN_POINT ( 'NONE',  ( -13.35616335646270691, 163.0958772461660544, -9.188101187500095079 ) ) ;
#89054 = CARTESIAN_POINT ( 'NONE',  ( 202.2072345662346038, 269.4162813440198647, 6.010783582451708185 ) ) ;
#89055 = ORIENTED_EDGE ( 'NONE', *, *, #849, .F. ) ;
#89056 = CARTESIAN_POINT ( 'NONE',  ( 77.93608175853721320, 60.44472089337216403, -15.94298384165975335 ) ) ;
#89057 = CARTESIAN_POINT ( 'NONE',  ( 189.8573735225914731, 274.2923351804632830, -15.65845412275707105 ) ) ;
#89058 = LINE ( 'NONE', #19105, #25728 ) ;
#89059 = CARTESIAN_POINT ( 'NONE',  ( 26.15794687706369004, 39.79426100978996317, 10.00000000000000000 ) ) ;
#89060 = CARTESIAN_POINT ( 'NONE',  ( 80.63072111635572981, 43.41492672548933029, -9.458890991678615023 ) ) ;
#89061 = DIRECTION ( 'NONE',  ( -0.8660254037844387076, -0.4999999999999998890, -0.000000000000000000 ) ) ;
#89062 = EDGE_CURVE ( 'NONE', #16631, #28403, #64760, .T. ) ;
#89063 = CARTESIAN_POINT ( 'NONE',  ( 15.38522827951586081, 173.5643266524160140, -9.188101187500093303 ) ) ;
#89064 = CARTESIAN_POINT ( 'NONE',  ( 103.5572661544365332, 230.5958772461660260, -9.188101187500095079 ) ) ;
#89065 = CARTESIAN_POINT ( 'NONE',  ( 202.8549823380854491, 279.2918593523859272, -16.39745931995414807 ) ) ;
#89066 = CARTESIAN_POINT ( 'NONE',  ( 87.93946558867349950, 44.22841546557597781, -4.388681702043149890 ) ) ;
#89067 = CARTESIAN_POINT ( 'NONE',  ( 180.1480783116751923, 255.5411283896334567, -2.368270940572544614 ) ) ;
#89069 = DIRECTION ( 'NONE',  ( 0.9972444261165168689, -0.07418594597050690020, 0.000000000000000000 ) ) ;
#89068 = AXIS2_PLACEMENT_3D ( 'NONE', #81638, #97818, #90242 ) ;
#89070 = B_SPLINE_CURVE_WITH_KNOTS ( 'NONE', 3,
 ( #71351, #95696, #3456, #64746, #88100, #80988, #56631, #34335, #94671, #48024, #26243, #65231, #42413, #18649 ),
 .UNSPECIFIED., .F., .F.,
 ( 4, 2, 2, 2, 2, 2, 4 ),
 ( 0.001093769620356032464, 0.001335766207658145837, 0.001577762794960259427, 0.002061755969564524772, 0.002303752556866657444, 0.002545749144168790116, 0.003029742318773055460 ),
 .UNSPECIFIED. ) ;
#89071 = CARTESIAN_POINT ( 'NONE',  ( 76.46473898121278978, 51.50464710109596211, 15.63208781809325210 ) ) ;
#89072 = CARTESIAN_POINT ( 'NONE',  ( 157.8501323257721083, 280.8042112442767007, -7.123878780571343050 ) ) ;
#89073 = CARTESIAN_POINT ( 'NONE',  ( 148.0346525705264469, 274.2434557974783615, -9.381294579651672905 ) ) ;
#89074 = ADVANCED_FACE ( 'NONE', ( #56644 ), #78468, .T. ) ;
#89075 = CARTESIAN_POINT ( 'NONE',  ( 84.70570963598828484, 50.54194691030828324, 13.58719792634913048 ) ) ;
#89076 = CARTESIAN_POINT ( 'NONE',  ( 81.76693488703203627, 53.61405564248835276, -15.52540917180992608 ) ) ;
#89077 = CARTESIAN_POINT ( 'NONE',  ( 79.49584607199039965, 46.25465621355715484, -13.22861432332135045 ) ) ;
#89078 = AXIS2_PLACEMENT_3D ( 'NONE', #54708, #8631, #46105 ) ;
#89079 = CARTESIAN_POINT ( 'NONE',  ( 172.9743055469626825, 262.8123507573143343, -16.34602756528129319 ) ) ;
#89080 = CARTESIAN_POINT ( 'NONE',  ( 85.15457341978220995, 207.7202760586659167, -5.415160957724236172E-17 ) ) ;
#89081 = CARTESIAN_POINT ( 'NONE',  ( 161.6755750489535046, 250.6166850027345276, -13.01404233079112061 ) ) ;
#89082 = CARTESIAN_POINT ( 'NONE',  ( 163.2257943664163236, 247.9316263820140307, 0.000000000000000000 ) ) ;
#89083 = CARTESIAN_POINT ( 'NONE',  ( -16.38799186764660831, 103.2525231626253657, 12.73778727189863780 ) ) ;
#89085 = CARTESIAN_POINT ( 'NONE',  ( 199.7543762271261301, 284.6622666708254314, 18.24097302174371293 ) ) ;
#89084 = CARTESIAN_POINT ( 'NONE',  ( 196.4351339088274813, 290.4113630087520050, 17.20526457544535504 ) ) ;
#89086 = CARTESIAN_POINT ( 'NONE',  ( 151.1126408083691501, 268.9122237844355254, -15.82705194100464396 ) ) ;
#89087 = CARTESIAN_POINT ( 'NONE',  ( 173.2921293650385337, 267.8776318488850734, -16.33130809225368552 ) ) ;
#89088 = CARTESIAN_POINT ( 'NONE',  ( 28.84929788977513709, 34.84336893147758474, -7.433330006724137462 ) ) ;
#89089 = CARTESIAN_POINT ( 'NONE',  ( 85.07407126341273340, 47.84811938996161018, -12.04656201052697639 ) ) ;
#89090 = CARTESIAN_POINT ( 'NONE',  ( 85.32304387868026652, 46.66374142128459113, -10.20885714811630685 ) ) ;
#89091 = ORIENTED_EDGE ( 'NONE', *, *, #3217, .T. ) ;
#89092 = CARTESIAN_POINT ( 'NONE',  ( 21.14648969749996610, 33.18502408145591431, 5.678558825948277544 ) ) ;
#89093 = CARTESIAN_POINT ( 'NONE',  ( 173.1211852740584334, 289.6938670388238393, -0.9942850523788112627 ) ) ;
#89094 = DIRECTION ( 'NONE',  ( 0.000000000000000000, -0.000000000000000000, 1.000000000000000000 ) ) ;
#89095 = CARTESIAN_POINT ( 'NONE',  ( 191.7482382276744772, 287.9955150116063010, -15.83237412442799830 ) ) ;
#89096 = LINE ( 'NONE', #49032, #87471 ) ;
#89098 = ADVANCED_FACE ( 'NONE', ( #63751 ), #56127, .F. ) ;
#89097 = CARTESIAN_POINT ( 'NONE',  ( 157.7355870688748496, 268.4989845473052696, 15.89826748515501009 ) ) ;
#89099 = DIRECTION ( 'NONE',  ( 0.1783728972749306640, 0.9839629614562466209, 0.000000000000000000 ) ) ;
#89100 = CARTESIAN_POINT ( 'NONE',  ( 128.2660534579352145, 254.8615022471902876, 5.000000000000046185 ) ) ;
#89101 = CARTESIAN_POINT ( 'NONE',  ( 204.7519188734507622, 276.0062688943993408, -12.76027478560537531 ) ) ;
#89102 = CARTESIAN_POINT ( 'NONE',  ( 74.92637023225178439, 53.29515228095790036, 16.04570802865760726 ) ) ;
#89103 = ORIENTED_EDGE ( 'NONE', *, *, #81639, .F. ) ;
#89104 = CARTESIAN_POINT ( 'NONE',  ( 169.5934039790062684, 248.5513711909993901, -1.936694667797326685 ) ) ;
#89105 = ORIENTED_EDGE ( 'NONE', *, *, #67817, .F. ) ;
#89106 = CARTESIAN_POINT ( 'NONE',  ( 162.6626107288841467, 248.9070890562113902, 10.12509462564867313 ) ) ;
#89107 = CARTESIAN_POINT ( 'NONE',  ( 84.09425856091186802, 41.95143607498360439, 1.796127423495148090 ) ) ;
#89108 = EDGE_CURVE ( 'NONE', #85978, #98021, #50150, .T. ) ;
#89109 = VERTEX_POINT ( 'NONE', #5447 ) ;
#89110 = CARTESIAN_POINT ( 'NONE',  ( 77.29872171176955931, 63.11034017860918510, -15.25129268891816636 ) ) ;
#89111 = VERTEX_POINT ( 'NONE', #58621 ) ;
#89112 = CARTESIAN_POINT ( 'NONE',  ( 72.19330168037886608, 71.72436257440323004, 5.504111378373452546 ) ) ;
#89113 = CARTESIAN_POINT ( 'NONE',  ( 11.51180284259942610, 11.81029122506292595, 8.090169943749479842 ) ) ;
#89114 = CARTESIAN_POINT ( 'NONE',  ( 137.5794118583994532, 267.3524639162450285, 1.815056976409021644E-15 ) ) ;
#89115 = CARTESIAN_POINT ( 'NONE',  ( 87.76333951327919181, 44.16327574611633366, -4.502641440754707958 ) ) ;
#89116 = CARTESIAN_POINT ( 'NONE',  ( 23.46864935082055581, 158.3759306620404743, -30.52142883766493853 ) ) ;
#89117 = CARTESIAN_POINT ( 'NONE',  ( 33.64972468124413751, 31.37878583063843152, 9.188101187500006262 ) ) ;
#89118 = CARTESIAN_POINT ( 'NONE',  ( 74.26468799828701606, 60.22538159402847668, -15.47038156723467317 ) ) ;
#89119 = CARTESIAN_POINT ( 'NONE',  ( 164.1807942228835770, 275.2290214034088081, 14.89732332872395304 ) ) ;
#89120 = FACE_OUTER_BOUND ( 'NONE', #50372, .T. ) ;
#89121 = EDGE_LOOP ( 'NONE', ( #52026, #58881, #32044, #93160 ) ) ;
#89122 = ORIENTED_EDGE ( 'NONE', *, *, #78956, .F. ) ;
#89123 = CARTESIAN_POINT ( 'NONE',  ( 182.6850850546973106, 296.4922765959772164, 0.2764116486899246827 ) ) ;
#89125 = CARTESIAN_POINT ( 'NONE',  ( 165.9392095978298869, 274.2621017338486809, -15.13082047531800178 ) ) ;
#89124 = CARTESIAN_POINT ( 'NONE',  ( 68.21928072586437963, 65.89764169037908914, 10.80738802253310382 ) ) ;
#89126 = CARTESIAN_POINT ( 'NONE',  ( 85.68248700152321362, 48.85324039464858714, -12.07567358188643603 ) ) ;
#89127 = CARTESIAN_POINT ( 'NONE',  ( 201.2981219894440414, 274.9036200554554625, -14.05226934314597464 ) ) ;
#89128 = CARTESIAN_POINT ( 'NONE',  ( -40.67952639183666008, 27.60432558407080350, 10.00000000000000000 ) ) ;
#89129 = CARTESIAN_POINT ( 'NONE',  ( -27.42236680055714260, 166.5217562850347406, 1.224646799147364892E-15 ) ) ;
#89130 = CARTESIAN_POINT ( 'NONE',  ( 207.7579944447645346, 270.7995932734924054, -3.579072180489195620 ) ) ;
#89131 = VECTOR ( 'NONE', #54232, 1000.000000000000000 ) ;
#89132 = CARTESIAN_POINT ( 'NONE',  ( 169.4258527407971826, 267.1907338905178904, 17.61138475887533517 ) ) ;
#89133 = DIRECTION ( 'NONE',  ( 0.000000000000000000, 0.000000000000000000, 1.000000000000000000 ) ) ;
#89134 = CARTESIAN_POINT ( 'NONE',  ( 103.0163473728362504, 218.0327760586659451, 1.948934522072303157E-15 ) ) ;
#89135 = ORIENTED_EDGE ( 'NONE', *, *, #20917, .T. ) ;
#89136 = FACE_OUTER_BOUND ( 'NONE', #87610, .T. ) ;
#89137 = DIRECTION ( 'NONE',  ( 0.000000000000000000, 1.000000000000000000, 0.000000000000000000 ) ) ;
#89138 = CARTESIAN_POINT ( 'NONE',  ( 166.7207440965885326, 278.5315519395303454, -13.22152219497125358 ) ) ;
#89139 = ORIENTED_EDGE ( 'NONE', *, *, #46065, .F. ) ;
#89140 = ORIENTED_EDGE ( 'NONE', *, *, #61460, .F. ) ;
#89141 = CARTESIAN_POINT ( 'NONE',  ( 183.1426684129219780, 267.5694331394444703, -16.03671021927237206 ) ) ;
#89142 = CARTESIAN_POINT ( 'NONE',  ( 177.5820306303727136, 292.5357431145801002, -2.681843810317637189 ) ) ;
#89143 = CARTESIAN_POINT ( 'NONE',  ( 164.7647380297938184, 248.9862001899016946, 10.10785415616959071 ) ) ;
#89144 = CARTESIAN_POINT ( 'NONE',  ( 159.9635946688021022, 268.7707599091479551, -17.14635356962945778 ) ) ;
#89145 = ADVANCED_FACE ( 'NONE', ( #36330 ), #73852, .T. ) ;
#89146 = DIRECTION ( 'NONE',  ( -0.9985437513708431689, -0.05394790633790857298, 0.000000000000000000 ) ) ;
#89147 = CARTESIAN_POINT ( 'NONE',  ( 99.98491136382573075, 228.5333772461660828, 9.188101187500095079 ) ) ;
#89148 = ORIENTED_EDGE ( 'NONE', *, *, #10623, .F. ) ;
#89149 = EDGE_CURVE ( 'NONE', #35732, #43419, #4441, .T. ) ;
#89150 = AXIS2_PLACEMENT_3D ( 'NONE', #35511, #65416, #96359 ) ;
#89151 = ORIENTED_EDGE ( 'NONE', *, *, #61391, .T. ) ;
#89152 = PLANE ( 'NONE',  #65734 ) ;
#89154 = ADVANCED_FACE ( 'NONE', ( #5939 ), #90596, .F. ) ;
#89153 = DIRECTION ( 'NONE',  ( -0.1580495287025880657, -0.9874311856918890351, 0.000000000000000000 ) ) ;
#89155 = ORIENTED_EDGE ( 'NONE', *, *, #17833, .T. ) ;
#89156 = EDGE_CURVE ( 'NONE', #60494, #39924, #42949, .T. ) ;
#89157 = CARTESIAN_POINT ( 'NONE',  ( 194.6929193942598317, 266.3728879037764159, -7.804718999318556172 ) ) ;
#89158 = FACE_OUTER_BOUND ( 'NONE', #34593, .T. ) ;
#89159 = CARTESIAN_POINT ( 'NONE',  ( 68.46675863972684795, 69.16680760964652563, -5.177149215189699838 ) ) ;
#89161 = CARTESIAN_POINT ( 'NONE',  ( 69.65303681785772483, 62.65480059021348325, -13.32895749987356560 ) ) ;
#89160 = CARTESIAN_POINT ( 'NONE',  ( 132.1361044793229951, 247.0958772461660544, -9.188101187500095079 ) ) ;
#89162 = CARTESIAN_POINT ( 'NONE',  ( -5.625082409869304634, 160.8927522451418213, 10.00000000000009592 ) ) ;
#89163 = CARTESIAN_POINT ( 'NONE',  ( 30.96785900501025424, 44.34188169337050311, -10.00000000000000000 ) ) ;
#89164 = ORIENTED_EDGE ( 'NONE', *, *, #1639, .F. ) ;
#89165 = CARTESIAN_POINT ( 'NONE',  ( 205.0957184426459321, 275.4107905729332515, 13.78964280781899632 ) ) ;
#89166 = CARTESIAN_POINT ( 'NONE',  ( 160.6678256987136706, 275.6111059978462663, 12.91046967929992384 ) ) ;
#89167 = CARTESIAN_POINT ( 'NONE',  ( 81.96261277299991832, 41.02826309496089152, -3.256590647522187965 ) ) ;
#89168 = CARTESIAN_POINT ( 'NONE',  ( 80.52662281699345215, 43.47104460342509213, 9.598632849592865668 ) ) ;
#89169 = CARTESIAN_POINT ( 'NONE',  ( 177.9371141619689070, 285.1367043548689821, 13.03223046609528879 ) ) ;
#89170 = CARTESIAN_POINT ( 'NONE',  ( 19.98788723728717898, 104.4047874917408336, 22.50000000000002132 ) ) ;
#89171 = PLANE ( 'NONE',  #21118 ) ;
#89172 = CARTESIAN_POINT ( 'NONE',  ( -19.65312891409030271, 93.06504152958497400, 25.00000000000000000 ) ) ;
#89173 = CARTESIAN_POINT ( 'NONE',  ( 80.85680478625504009, 54.83540491762479263, 15.90941129233622675 ) ) ;
#89174 = CARTESIAN_POINT ( 'NONE',  ( 206.6148326247335092, 272.1004287451723371, 7.183687323914591971 ) ) ;
#89175 = CARTESIAN_POINT ( 'NONE',  ( 167.7724828596593341, 250.0038861993971295, 6.958639209991310359 ) ) ;
#89176 = LINE ( 'NONE', #19723, #54735 ) ;
#89177 = CARTESIAN_POINT ( 'NONE',  ( 207.6555576926778883, 270.9770189326688410, -1.235081510489080436 ) ) ;
#89178 = LINE ( 'NONE', #5875, #36589 ) ;
#89179 = CARTESIAN_POINT ( 'NONE',  ( 71.12330115413381293, 70.98152915379483829, -4.639273218532493637 ) ) ;
#89180 = CARTESIAN_POINT ( 'NONE',  ( 185.3369900536077068, 266.4498558932299375, 13.14662191727306073 ) ) ;
#89181 = LINE ( 'NONE', #3533, #15832 ) ;
#89182 = CARTESIAN_POINT ( 'NONE',  ( 39.82000823235115661, 28.15404122711136736, 8.090169943749479842 ) ) ;
#89183 = DIRECTION ( 'NONE',  ( -0.000000000000000000, -0.000000000000000000, 1.000000000000000000 ) ) ;
#89184 = PRESENTATION_STYLE_ASSIGNMENT (( #11631 ) ) ;
#89185 = DIRECTION ( 'NONE',  ( -0.9140770918436990078, -0.4055404667435369426, 0.000000000000000000 ) ) ;
#89186 = CARTESIAN_POINT ( 'NONE',  ( 85.00527620810069607, 43.38834873272450210, -5.370498173854784341 ) ) ;
#89187 = CARTESIAN_POINT ( 'NONE',  ( 207.1158949475991164, 271.9117422260973740, -5.823035679195911918 ) ) ;
#89188 = CARTESIAN_POINT ( 'NONE',  ( 11.92112666437810908, 171.5643266524160140, 9.188101187500095079 ) ) ;
#89189 = CARTESIAN_POINT ( 'NONE',  ( -34.24356256989597114, 94.88921800892812541, 45.19948692389422717 ) ) ;
#89190 = ORIENTED_EDGE ( 'NONE', *, *, #56864, .F. ) ;
#89191 = CARTESIAN_POINT ( 'NONE',  ( 86.62141849789249193, 46.36649306945518134, 9.067576869787547622 ) ) ;
#89192 = CARTESIAN_POINT ( 'NONE',  ( 30.33301404664494427, 194.9865022471903160, -10.00000000000009592 ) ) ;
#89193 = CARTESIAN_POINT ( 'NONE',  ( 71.51903464973995028, 72.36264346112822921, -1.271393898589449512 ) ) ;
#89194 = CARTESIAN_POINT ( 'NONE',  ( 32.11017034222032862, 189.3458772461660544, 9.188101187500095079 ) ) ;
#89195 = ADVANCED_FACE ( 'NONE', ( #51029 ), #36833, .T. ) ;
#89196 = CARTESIAN_POINT ( 'NONE',  ( 200.8551880497955437, 282.7556046643899776, 18.00894873733387058 ) ) ;
#89197 = CARTESIAN_POINT ( 'NONE',  ( 147.4811722709131914, 275.2021117973970377, 3.890385073228495916 ) ) ;
#89198 = CARTESIAN_POINT ( 'NONE',  ( 41.38738224522862907, 24.86426979415093186, -3.090169943749474069 ) ) ;
#89199 = CARTESIAN_POINT ( 'NONE',  ( 201.8398744800204838, 269.4056535102417342, -6.425511374294321953 ) ) ;
#89200 = CARTESIAN_POINT ( 'NONE',  ( 147.2180753513904961, 275.6578090293250511, 0.4909717733184589261 ) ) ;
#89201 = CARTESIAN_POINT ( 'NONE',  ( 179.0376912146908523, 278.3007504662035103, -16.65281315354532410 ) ) ;
#89202 = CARTESIAN_POINT ( 'NONE',  ( 68.98552337397570966, 67.88664236019715759, -8.139828674801092845 ) ) ;
#89203 = CARTESIAN_POINT ( 'NONE',  ( 87.14537157594897110, 46.05544232951319827, -8.218268012384905674 ) ) ;
#89204 = CARTESIAN_POINT ( 'NONE',  ( 80.15404930735284950, 58.24487849859603017, -16.60713908503101877 ) ) ;
#89205 = VECTOR ( 'NONE', #75716, 1000.000000000000114 ) ;
#89206 = DIRECTION ( 'NONE',  ( -0.9689885751534065284, -0.2471055264905481497, 0.000000000000000000 ) ) ;
#89207 = CARTESIAN_POINT ( 'NONE',  ( 79.69646206235795205, 223.4865022471902591, -10.00000000000009415 ) ) ;
#89208 = DIRECTION ( 'NONE',  ( -0.8279987035736700030, -0.5607300124661794838, 0.000000000000000000 ) ) ;
#89209 = LINE ( 'NONE', #72472, #9366 ) ;
#89210 = EDGE_LOOP ( 'NONE', ( #48471, #4078, #791, #36570 ) ) ;
#89211 = CARTESIAN_POINT ( 'NONE',  ( 40.25596147474394826, 203.2369531367911293, -4.594050593750048428 ) ) ;
#89212 = ORIENTED_EDGE ( 'NONE', *, *, #28920, .T. ) ;
#89213 = DIRECTION ( 'NONE',  ( 0.3666034970181715757, -0.9303772761487930643, 0.000000000000000000 ) ) ;
#89214 = CARTESIAN_POINT ( 'NONE',  ( 190.3286155001717930, 300.9881631498979004, -5.624828231725103045 ) ) ;
#89215 = CARTESIAN_POINT ( 'NONE',  ( 67.66662286171703045, 66.83249233868968986, -8.522559018194412417 ) ) ;
#89216 = EDGE_LOOP ( 'NONE', ( #87442, #5870, #19254, #69649 ) ) ;
#89217 = CARTESIAN_POINT ( 'NONE',  ( 171.0937289546497766, 286.9986480494256966, 8.572633432616918014 ) ) ;
#89218 = FACE_OUTER_BOUND ( 'NONE', #70222, .T. ) ;
#89219 = DIRECTION ( 'NONE',  ( 1.000000000000000000, -2.158987274672848517E-13, 0.000000000000000000 ) ) ;
#89220 = CARTESIAN_POINT ( 'NONE',  ( 33.57875857642567752, 25.10170272979928896, -7.433330006724141015 ) ) ;
#89221 = CARTESIAN_POINT ( 'NONE',  ( 186.9609134277102669, 264.2677986880410685, 10.82359653245352682 ) ) ;
#89222 = CARTESIAN_POINT ( 'NONE',  ( 196.4501996009505831, 290.3852684645433442, -17.82325615854289680 ) ) ;
#89223 = CARTESIAN_POINT ( 'NONE',  ( 172.6087892508253390, 256.3355526837004845, 11.23066983786553941 ) ) ;
#89224 = VERTEX_POINT ( 'NONE', #34830 ) ;
#89225 = CARTESIAN_POINT ( 'NONE',  ( 20.93478768117288524, 17.80170272979926338, 7.433330006724137462 ) ) ;
#89226 = CYLINDRICAL_SURFACE ( 'NONE', #46189, 70.00000000000002842 ) ;
#89227 = CARTESIAN_POINT ( 'NONE',  ( 172.5056581661058033, 253.5720814276482997, 8.377529669797983303 ) ) ;
#89228 = CARTESIAN_POINT ( 'NONE',  ( 16.45310489419773958, 168.7592609112379876, 2.679491924311254714 ) ) ;
#89229 = ORIENTED_EDGE ( 'NONE', *, *, #15084, .F. ) ;
#89230 = CARTESIAN_POINT ( 'NONE',  ( 181.9138868423064821, 283.8759538834763134, 14.95563825545625747 ) ) ;
#89231 = FACE_OUTER_BOUND ( 'NONE', #90958, .T. ) ;
#89232 = CARTESIAN_POINT ( 'NONE',  ( 70.48357858576694923, 65.23080690043917684, -12.53072601663070706 ) ) ;
#89233 = ORIENTED_EDGE ( 'NONE', *, *, #91233, .T. ) ;
#89234 = VERTEX_POINT ( 'NONE', #19668 ) ;
#89236 = FACE_OUTER_BOUND ( 'NONE', #90249, .T. ) ;
#89235 = CARTESIAN_POINT ( 'NONE',  ( 161.8668411317136986, 250.2854024296290447, -13.43522912998426655 ) ) ;
#89237 = CARTESIAN_POINT ( 'NONE',  ( -106.6146531411566798, 123.6868197944956620, 37.50000000000002132 ) ) ;
#89238 = VERTEX_POINT ( 'NONE', #50531 ) ;
#89239 = CARTESIAN_POINT ( 'NONE',  ( -19.65312891409030271, 93.06504152958497400, 177.5919119679930134 ) ) ;
#89240 = CARTESIAN_POINT ( 'NONE',  ( -27.52599651137547809, 146.7012482093459198, 37.49999999999998579 ) ) ;
#89241 = DIRECTION ( 'NONE',  ( 1.000000000000000000, 0.000000000000000000, 0.000000000000000000 ) ) ;
#89242 = CARTESIAN_POINT ( 'NONE',  ( 78.40057582686800686, 61.29346224198984316, -15.87704840749689161 ) ) ;
#89243 = CARTESIAN_POINT ( 'NONE',  ( 197.9771301758180186, 286.8468337050553600, 16.93947910494098608 ) ) ;
#89244 = CARTESIAN_POINT ( 'NONE',  ( 123.6384037525706958, 236.0643266524160140, 9.188101187500095079 ) ) ;
#89245 = DIRECTION ( 'NONE',  ( -0.8660254037844384856, -0.5000000000000002220, 0.000000000000000000 ) ) ;
#89246 = DIRECTION ( 'NONE',  ( 0.4999999999999992784, -0.8660254037844390407, 0.000000000000000000 ) ) ;
#89247 = CARTESIAN_POINT ( 'NONE',  ( 74.97949069045873216, 202.5494855054051584, -2.679491924311248496 ) ) ;
#89248 = CARTESIAN_POINT ( 'NONE',  ( 163.7595992360150490, 247.0070492265414828, -6.976205010573520049 ) ) ;
#89249 = VERTEX_POINT ( 'NONE', #74377 ) ;
#89250 = B_SPLINE_CURVE_WITH_KNOTS ( 'NONE', 3,
 ( #14505, #38781, #76318, #53485 ),
 .UNSPECIFIED., .F., .F.,
 ( 4, 4 ),
 ( 0.005435284012089665502, 0.01347523137567103318 ),
 .UNSPECIFIED. ) ;
#89251 = CARTESIAN_POINT ( 'NONE',  ( 38.91320803870388545, 23.26216523072497466, -2.296566073217252530E-15 ) ) ;
#89252 = CARTESIAN_POINT ( 'NONE',  ( 159.6419305724666344, 254.1390605605417079, 16.92015248457581933 ) ) ;
#89253 = DIRECTION ( 'NONE',  ( -0.8660254037844387076, -0.4999999999999998890, -0.000000000000000000 ) ) ;
#89254 = CARTESIAN_POINT ( 'NONE',  ( 75.46539357129627490, 220.5024278399160949, -9.188101187500093303 ) ) ;
#89255 = CARTESIAN_POINT ( 'NONE',  ( 176.4104406952913848, 285.9470522879340137, 13.60907346279267927 ) ) ;
#89256 = CARTESIAN_POINT ( 'NONE',  ( 151.4025156491502742, 268.4101458323662541, 14.71049357081981235 ) ) ;
#89257 = CARTESIAN_POINT ( 'NONE',  ( 154.9455285025717615, 262.2734675583710100, 18.28470720339922551 ) ) ;
#89258 = CARTESIAN_POINT ( 'NONE',  ( 175.5536407316448333, 278.4519599138486114, 15.47712664167736030 ) ) ;
#89259 = ORIENTED_EDGE ( 'NONE', *, *, #55712, .F. ) ;
#89260 = EDGE_CURVE ( 'NONE', #69600, #90508, #78919, .T. ) ;
#89261 = CARTESIAN_POINT ( 'NONE',  ( 74.49454245850880341, 63.15023117209727843, -14.55457805515772840 ) ) ;
#89262 = FACE_OUTER_BOUND ( 'NONE', #40850, .T. ) ;
#89263 = ORIENTED_EDGE ( 'NONE', *, *, #75314, .F. ) ;
#89264 = CARTESIAN_POINT ( 'NONE',  ( 194.7327554194830554, 293.3599690460087572, 15.69670373610146363 ) ) ;
#89265 = CARTESIAN_POINT ( 'NONE',  ( -16.97593537095525917, 172.5530062829863027, 9.296355089585912665E-16 ) ) ;
#89266 = CARTESIAN_POINT ( 'NONE',  ( 160.5379721355672586, 258.2968622624442787, -16.86137763422037494 ) ) ;
#89267 = EDGE_CURVE ( 'NONE', #79622, #72764, #40689, .T. ) ;
#89268 = CARTESIAN_POINT ( 'NONE',  ( 206.7036107519802783, 270.2074794926728032, 1.825126258972860516 ) ) ;
#89269 = CARTESIAN_POINT ( 'NONE',  ( 84.14312167556933275, 48.98415679381830756, 0.000000000000000000 ) ) ;
#89270 = CARTESIAN_POINT ( 'NONE',  ( 150.3616303100281471, 275.4795733169851815, 8.855240024576275459 ) ) ;
#89271 = CARTESIAN_POINT ( 'NONE',  ( 164.4573439719129340, 245.7985198932525748, 1.541132361166968501 ) ) ;
#89272 = FILL_AREA_STYLE ('',( #58295 ) ) ;
#89273 = DIRECTION ( 'NONE',  ( -1.000000000000000000, 0.000000000000000000, 0.000000000000000000 ) ) ;
#89274 = CARTESIAN_POINT ( 'NONE',  ( 125.6141109788952122, 234.1423013555409796, -4.594050593750043987 ) ) ;
#89275 = ORIENTED_EDGE ( 'NONE', *, *, #11020, .T. ) ;
#89276 = CARTESIAN_POINT ( 'NONE',  ( 146.5310397537613483, 276.8477895910274356, -0.2793038414862049068 ) ) ;
#89277 = CARTESIAN_POINT ( 'NONE',  ( -115.0954152546897973, 78.37593066204027537, 37.50000000000002132 ) ) ;
#89278 = CARTESIAN_POINT ( 'NONE',  ( 205.6477917841175156, 273.8035238412935541, -10.40835627202817903 ) ) ;
#89279 = CARTESIAN_POINT ( 'NONE',  ( 164.4272222519600746, 245.8506922426221593, 7.021336339662529902 ) ) ;
#89280 = CARTESIAN_POINT ( 'NONE',  ( 74.23186439702232065, 58.41354208856498786, 15.85634166313547588 ) ) ;
#89281 = CIRCLE ( 'NONE', #24486, 7.298499999999999766 ) ;
#89282 = DIRECTION ( 'NONE',  ( 0.000000000000000000, -0.000000000000000000, -1.000000000000000000 ) ) ;
#89283 = ORIENTED_EDGE ( 'NONE', *, *, #63640, .F. ) ;
#89284 = CARTESIAN_POINT ( 'NONE',  ( 76.89472034703643999, 56.68234231651032928, 16.18388797058281980 ) ) ;
#89285 = CARTESIAN_POINT ( 'NONE',  ( 167.5883605658670490, 249.2390751195395353, -5.691470653330944707 ) ) ;
#89286 = PLANE ( 'NONE',  #64562 ) ;
#89287 = CARTESIAN_POINT ( 'NONE',  ( -42.47074677134370546, 28.21475011077167849, 10.00000000000000000 ) ) ;
#89288 = CARTESIAN_POINT ( 'NONE',  ( 142.6123662252853421, 259.5780487066560340, -7.305945665944390655 ) ) ;
#89289 = CARTESIAN_POINT ( 'NONE',  ( 195.4818567523729200, 263.4360957373327778, 0.8675948490323511786 ) ) ;
#89290 = DIRECTION ( 'NONE',  ( 0.5906904945688895570, 0.000000000000000000, 0.8068982213550607296 ) ) ;
#89291 = CARTESIAN_POINT ( 'NONE',  ( 180.2260403442535051, 295.0423342771414923, -3.480517403894910711 ) ) ;
#89292 = CARTESIAN_POINT ( 'NONE',  ( 192.2429491947952158, 297.0140665128034243, 10.97773268720420248 ) ) ;
#89293 = CARTESIAN_POINT ( 'NONE',  ( 12.38042018312781067, 30.08080186712591697, -3.090169943749475845 ) ) ;
#89294 = CARTESIAN_POINT ( 'NONE',  ( 149.3833831332874240, 271.9073859370555510, 11.40518020539810173 ) ) ;
#89295 = CARTESIAN_POINT ( 'NONE',  ( 81.58361516609492980, 41.71275962428084227, 5.900248587975138292 ) ) ;
#89296 = CARTESIAN_POINT ( 'NONE',  ( 169.4074305931134461, 285.1542170432204557, -8.003578837916338173 ) ) ;
#89297 = CARTESIAN_POINT ( 'NONE',  ( 198.1300353965528984, 287.4757075181870505, 18.48278456664528946 ) ) ;
#89298 = CARTESIAN_POINT ( 'NONE',  ( 196.1370092075112268, 290.1209220278959720, 16.40156295354631411 ) ) ;
#89299 =( BOUNDED_CURVE ( )  B_SPLINE_CURVE ( 2, ( #87606, #54726, #7135, #16243, #60820, #47134, #78058, #8646, #18133 ),
 .UNSPECIFIED., .F., .T. ) 
 B_SPLINE_CURVE_WITH_KNOTS ( ( 3, 2, 2, 2, 3 ),
 ( 0.8911290322580645018, 0.8924731182795698770, 0.8951612903225806273, 0.8978494623655913776, 0.8991935483870967527 ),
 .UNSPECIFIED. ) 
 CURVE ( )  GEOMETRIC_REPRESENTATION_ITEM ( )  RATIONAL_B_SPLINE_CURVE ( ( 0.9330127018922194093, 0.9330127018922194093, 1.000000000000000000, 0.8660254037844387076, 1.000000000000000000, 0.8660254037844387076, 1.000000000000000000, 0.9330127018922194093, 0.9330127018922194093 ) ) 
 REPRESENTATION_ITEM ( '' )  );
#89300 = CARTESIAN_POINT ( 'NONE',  ( 146.7232198725432113, 245.5177522451417644, 5.000000000000051514 ) ) ;
#89301 = CARTESIAN_POINT ( 'NONE',  ( 183.1489178096782950, 278.9636052248775400, 17.34984484178414377 ) ) ;
#89302 = ORIENTED_EDGE ( 'NONE', *, *, #28193, .F. ) ;
#89303 = CARTESIAN_POINT ( 'NONE',  ( 157.7529601300917363, 257.4108533407307959, 16.91445305439664892 ) ) ;
#89304 = CARTESIAN_POINT ( 'NONE',  ( 189.8533352240220893, 301.8113727360248504, -0.2033756396389863053 ) ) ;
#89305 = CARTESIAN_POINT ( 'NONE',  ( 1.204062292545672319, 165.3768266524160140, 9.188101187500096856 ) ) ;
#89306 = EDGE_CURVE ( 'NONE', #57725, #28914, #45904, .T. ) ;
#89307 = CARTESIAN_POINT ( 'NONE',  ( 51.37958267218910891, 188.2202760586659451, -5.415160957724236172E-17 ) ) ;
#89308 = CARTESIAN_POINT ( 'NONE',  ( 178.4286190058349746, 259.0350523900441431, -10.32048496258370918 ) ) ;
#89309 = CARTESIAN_POINT ( 'NONE',  ( 17.39660613652184296, 31.81751292744056059, -6.180339887498951690 ) ) ;
#89310 = CARTESIAN_POINT ( 'NONE',  ( 88.08725135673812190, 43.63233996731285202, 0.09640656973314638833 ) ) ;
#89311 = CARTESIAN_POINT ( 'NONE',  ( 164.2257943664163236, 246.1995755744451060, 2.059986336238496279E-15 ) ) ;
#89312 = CARTESIAN_POINT ( 'NONE',  ( 72.10046935555597258, 72.37486351763082837, -3.289382622874389206 ) ) ;
#89313 = FACE_OUTER_BOUND ( 'NONE', #12996, .T. ) ;
#89314 = CARTESIAN_POINT ( 'NONE',  ( 74.13991727214688865, 55.63178720252560794, -16.58981027534304431 ) ) ;
#89315 = CARTESIAN_POINT ( 'NONE',  ( 167.6657660674999022, 256.6202425009460626, 13.71097750828161743 ) ) ;
#89316 = CARTESIAN_POINT ( 'NONE',  ( 75.97157031761298640, 55.45432131483929794, 16.60500414049532480 ) ) ;
#89317 = CARTESIAN_POINT ( 'NONE',  ( 49.09245556086620610, 93.56363653685789927, -10.00000000000000000 ) ) ;
#89318 = LINE ( 'NONE', #9782, #88766 ) ;
#89319 = EDGE_CURVE ( 'NONE', #81254, #38046, #99946, .T. ) ;
#89320 = CARTESIAN_POINT ( 'NONE',  ( 45.92147131476491495, 183.9865022471901455, 1.119607411625061291E-15 ) ) ;
#89321 = CARTESIAN_POINT ( 'NONE',  ( 182.0785557626968796, 291.7619114360715002, 9.330709163805311235 ) ) ;
#89322 = CARTESIAN_POINT ( 'NONE',  ( 149.7165891736972014, 271.9666657501144869, -11.45573312492119022 ) ) ;
#89323 = CARTESIAN_POINT ( 'NONE',  ( 2.070087696330116689, 165.8768266524159856, -9.188101187500091527 ) ) ;
#89324 = CARTESIAN_POINT ( 'NONE',  ( 164.3014958605646143, 285.1311274651320673, 4.328674906941893497 ) ) ;
#89326 = EDGE_CURVE ( 'NONE', #19809, #18420, #97368, .T. ) ;
#89325 = CARTESIAN_POINT ( 'NONE',  ( 80.52836418950521136, 57.78044297351195269, -16.24599850453018846 ) ) ;
#89327 = CARTESIAN_POINT ( 'NONE',  ( 79.18223904501012100, 60.01793730243658587, 16.13539395559152467 ) ) ;
#89328 = CARTESIAN_POINT ( 'NONE',  ( 39.23796756512304995, 23.44966523072497822, -2.296566073217252530E-15 ) ) ;
#89329 = CARTESIAN_POINT ( 'NONE',  ( 82.10523990517461357, 41.85707133252695655, -5.529865280922476423 ) ) ;
#89330 = CARTESIAN_POINT ( 'NONE',  ( 179.3397263455709663, 277.6061668572808117, 16.87921206249952633 ) ) ;
#89331 = CARTESIAN_POINT ( 'NONE',  ( 154.9344967692067598, 262.2925750810547356, 17.30210568643136781 ) ) ;
#89332 = CARTESIAN_POINT ( 'NONE',  ( 196.4808189786114951, 290.3322341467384717, -17.84817245450773271 ) ) ;
#89333 = CARTESIAN_POINT ( 'NONE',  ( 4.394486334025504704, 45.80786630299208895, 59.99999999999999289 ) ) ;
#89334 = DIRECTION ( 'NONE',  ( 1.000000000000000000, 0.000000000000000000, 0.000000000000000000 ) ) ;
#89335 = CARTESIAN_POINT ( 'NONE',  ( 17.19524200933981817, 21.87878583063841020, -9.188101187500006262 ) ) ;
#89336 = CARTESIAN_POINT ( 'NONE',  ( 118.0722127640079577, 245.6427522451419350, 10.00000000000009415 ) ) ;
#89337 = CARTESIAN_POINT ( 'NONE',  ( 82.27982384062090659, 54.25399372119451158, 15.63186620393292436 ) ) ;
#89338 = CARTESIAN_POINT ( 'NONE',  ( 159.2638637293276531, 259.2554630532692954, 16.67674092906833394 ) ) ;
#89339 = CARTESIAN_POINT ( 'NONE',  ( 153.2048789493636605, 277.6616380186837318, -5.192392496551228476 ) ) ;
#89340 = ORIENTED_EDGE ( 'NONE', *, *, #82372, .F. ) ;
#89341 = CARTESIAN_POINT ( 'NONE',  ( 103.8809628199470012, 242.3297689869269504, -2.679491924311252493 ) ) ;
#89342 = CARTESIAN_POINT ( 'NONE',  ( 75.11546922477293720, 53.61976721164031545, -16.54181461514712836 ) ) ;
#89343 = CARTESIAN_POINT ( 'NONE',  ( 81.13608137687064925, 42.60696278352305910, 7.988320930663083352 ) ) ;
#89344 = ORIENTED_EDGE ( 'NONE', *, *, #34155, .F. ) ;
#89345 = CARTESIAN_POINT ( 'NONE',  ( 153.1390349443021535, 266.6901594501808290, 16.22385130400761710 ) ) ;
#89346 = CARTESIAN_POINT ( 'NONE',  ( 67.38519378865026965, 69.44927455685115092, 1.146917413897621918 ) ) ;
#89347 = CARTESIAN_POINT ( 'NONE',  ( 66.51856882819618022, 68.22589165948441803, 4.545885137720724778 ) ) ;
#89348 = CARTESIAN_POINT ( 'NONE',  ( 87.12892733211938889, 45.32551623454932610, 7.045331451850512572 ) ) ;
#89349 = ORIENTED_EDGE ( 'NONE', *, *, #65244, .T. ) ;
#89350 = ORIENTED_EDGE ( 'NONE', *, *, #8847, .F. ) ;
#89352 = CARTESIAN_POINT ( 'NONE',  ( 204.1793240545508752, 276.9980322128846524, 14.17550310845996187 ) ) ;
#89351 = DIRECTION ( 'NONE',  ( -0.000000000000000000, -0.000000000000000000, -1.000000000000000000 ) ) ;
#89353 = CARTESIAN_POINT ( 'NONE',  ( 152.7618747630824885, 266.0556667813044101, 16.41480086888796919 ) ) ;
#89354 = ORIENTED_EDGE ( 'NONE', *, *, #74227, .T. ) ;
#89355 = CARTESIAN_POINT ( 'NONE',  ( 80.47503692277169307, 57.63887959601478883, -16.59359448248663682 ) ) ;
#89356 = CARTESIAN_POINT ( 'NONE',  ( 177.6567394906847710, 263.3673336801520577, 15.42114140403424649 ) ) ;
#89357 = ORIENTED_EDGE ( 'NONE', *, *, #1692, .F. ) ;
#89358 = DIRECTION ( 'NONE',  ( -0.000000000000000000, 0.000000000000000000, 1.000000000000000000 ) ) ;
#89359 = CARTESIAN_POINT ( 'NONE',  ( 82.92091453256576017, 49.04847585767068807, -13.26297005650615368 ) ) ;
#89360 = ORIENTED_EDGE ( 'NONE', *, *, #66201, .T. ) ;
#89361 = CARTESIAN_POINT ( 'NONE',  ( 202.9779954277112495, 268.0318619332833805, 2.519114201778603679 ) ) ;
#89362 = CARTESIAN_POINT ( 'NONE',  ( 168.4437225316406170, 276.0757796713103289, -16.34630765130609120 ) ) ;
#89363 = CARTESIAN_POINT ( 'NONE',  ( 73.49378489868225017, 58.86888438589103600, 15.66859131630157087 ) ) ;
#89364 = VERTEX_POINT ( 'NONE', #61614 ) ;
#89365 = ADVANCED_FACE ( 'NONE', ( #37323 ), #55871, .F. ) ;
#89366 = EDGE_CURVE ( 'NONE', #2381, #30665, #54004, .T. ) ;
#89367 = CARTESIAN_POINT ( 'NONE',  ( 177.7711228786548077, 279.3620349116163197, -16.19571528524508963 ) ) ;
#89368 = CARTESIAN_POINT ( 'NONE',  ( 169.3408527021580881, 261.4620406432418349, -16.56737040952816642 ) ) ;
#89369 = ORIENTED_EDGE ( 'NONE', *, *, #44983, .T. ) ;
#89370 = CARTESIAN_POINT ( 'NONE',  ( 156.9003456755540924, 266.6926263611233026, -16.21475809265606571 ) ) ;
#89371 = ORIENTED_EDGE ( 'NONE', *, *, #13353, .F. ) ;
#89372 = DIRECTION ( 'NONE',  ( 0.3887219701524006754, 0.9213551052231903071, 0.000000000000000000 ) ) ;
#89373 = EDGE_LOOP ( 'NONE', ( #44565, #45100, #55865, #57661 ) ) ;
#89374 = LINE ( 'NONE', #50801, #93389 ) ;
#89375 = CARTESIAN_POINT ( 'NONE',  ( 110.0000000000000000, 15.00000000000003908, 59.99999999999999289 ) ) ;
#89376 = CARTESIAN_POINT ( 'NONE',  ( 188.6399219150083297, 298.6042682482373607, -4.272446188806214629 ) ) ;
#89377 = CARTESIAN_POINT ( 'NONE',  ( 143.7588392505102206, 242.2592609112379876, 2.679491924311254714 ) ) ;
#89378 = CARTESIAN_POINT ( 'NONE',  ( 152.6615646578087819, 266.2294089801508221, 16.94722993326405813 ) ) ;
#89379 = EDGE_CURVE ( 'NONE', #63497, #91664, #634, .T. ) ;
#89380 = CARTESIAN_POINT ( 'NONE',  ( 178.3915236234910537, 291.5165576824842901, 6.088472439993570795 ) ) ;
#89381 = EDGE_CURVE ( 'NONE', #54783, #85413, #64700, .T. ) ;
#89382 = CARTESIAN_POINT ( 'NONE',  ( 158.8815770798748588, 255.4560314414227662, -16.10048816751885425 ) ) ;
#89383 = ORIENTED_EDGE ( 'NONE', *, *, #19417, .T. ) ;
#89384 = CARTESIAN_POINT ( 'NONE',  ( 78.20921595494600354, 56.55723432008092288, -16.20170577005126233 ) ) ;
#89385 = LINE ( 'NONE', #54797, #70487 ) ;
#89386 = AXIS2_PLACEMENT_3D ( 'NONE', #69346, #53632, #7042 ) ;
#89388 = CARTESIAN_POINT ( 'NONE',  ( 180.6066648745947134, 283.7006809008031496, -16.18202752516933174 ) ) ;
#89387 = CARTESIAN_POINT ( 'NONE',  ( 77.52175738690283424, 49.76289862564163968, -14.96722493358440964 ) ) ;
#89390 = VERTEX_POINT ( 'NONE', #9828 ) ;
#89389 = CARTESIAN_POINT ( 'NONE',  ( 198.6587626159274294, 286.5599251108861267, 17.99840276545888784 ) ) ;
#89391 = ORIENTED_EDGE ( 'NONE', *, *, #10962, .T. ) ;
#89392 = CARTESIAN_POINT ( 'NONE',  ( 187.5500012533888423, 277.1004024971114745, 17.01394763479494898 ) ) ;
#89393 = CARTESIAN_POINT ( 'NONE',  ( 82.82392674575149272, 51.78329203972547390, -14.70596644949177367 ) ) ;
#89394 = CARTESIAN_POINT ( 'NONE',  ( 28.65130504220245555, 111.5816539614736485, 59.99999999999999289 ) ) ;
#89395 = CARTESIAN_POINT ( 'NONE',  ( 175.6925083280133322, 275.2066185980531259, -17.63772206380936680 ) ) ;
#89396 = CARTESIAN_POINT ( 'NONE',  ( 198.6433817073464922, 286.5865656260148171, -17.57789766230896689 ) ) ;
#89397 = CARTESIAN_POINT ( 'NONE',  ( 148.2514616260410776, 273.8679314977858894, -10.42361479059151996 ) ) ;
#89398 = ORIENTED_EDGE ( 'NONE', *, *, #1901, .F. ) ;
#89399 = CARTESIAN_POINT ( 'NONE',  ( 170.4959927957777097, 255.7634325838962184, -12.27116094425178616 ) ) ;
#89400 = DIRECTION ( 'NONE',  ( 0.5000000000000002220, -0.8660254037844387076, -0.000000000000000000 ) ) ;
#89401 = CARTESIAN_POINT ( 'NONE',  ( -106.6146531411567224, 123.6868197944957188, -37.49999999999997868 ) ) ;
#89402 = DIRECTION ( 'NONE',  ( -0.8660254037844387076, -0.5000000000000000000, 0.000000000000000000 ) ) ;
#89403 = CARTESIAN_POINT ( 'NONE',  ( 28.07773955407504118, 197.0177522451419350, 5.000000000000046185 ) ) ;
#89404 = CARTESIAN_POINT ( 'NONE',  ( 106.3175485811169239, 238.3149278399160949, -9.188101187500095079 ) ) ;
#89405 = CARTESIAN_POINT ( 'NONE',  ( 183.9039741337527403, 297.0480174192951495, -2.803343177518471396 ) ) ;
#89406 = CARTESIAN_POINT ( 'NONE',  ( 167.7101951474509463, 282.4104349734390098, -10.63977280035835449 ) ) ;
#89407 = CARTESIAN_POINT ( 'NONE',  ( 84.49949969528468330, 50.67006985176584521, 13.73213175918632523 ) ) ;
#89408 = DIRECTION ( 'NONE',  ( -0.8660254037844387076, -0.4999999999999998890, -0.000000000000000000 ) ) ;
#89409 = CARTESIAN_POINT ( 'NONE',  ( 24.04513522159523475, 190.8149278399161233, 9.188101187500093303 ) ) ;
#89410 = CARTESIAN_POINT ( 'NONE',  ( 161.7587802986029999, 250.4725692828850754, 14.33336164792646450 ) ) ;
#89411 = ORIENTED_EDGE ( 'NONE', *, *, #75362, .F. ) ;
#89412 = ORIENTED_EDGE ( 'NONE', *, *, #74668, .T. ) ;
#89413 = DIRECTION ( 'NONE',  ( -0.8660254037844387076, -0.4999999999999998890, -0.000000000000000000 ) ) ;
#89414 = CARTESIAN_POINT ( 'NONE',  ( 74.23555041547365363, 68.49601928387087924, -11.11897725275786719 ) ) ;
#89415 = CARTESIAN_POINT ( 'NONE',  ( 74.55808943708029801, 66.56006064317872983, 13.25253988228418933 ) ) ;
#89416 = DIRECTION ( 'NONE',  ( 0.01068548594337171906, -0.9999429085653609439, 0.000000000000000000 ) ) ;
#89417 = CARTESIAN_POINT ( 'NONE',  ( 161.0965315767822972, 251.6196177163260188, -13.76772246540905442 ) ) ;
#89418 = CARTESIAN_POINT ( 'NONE',  ( -19.65312891409030271, 93.06504152958497400, 60.00000000000000000 ) ) ;
#89419 = CARTESIAN_POINT ( 'NONE',  ( 55.03304057046344866, 193.3923013555409796, 4.594050593750050204 ) ) ;
#89420 = CARTESIAN_POINT ( 'NONE',  ( 84.80240350195578003, 229.7677522451419350, -5.000000000000047962 ) ) ;
#89421 = ORIENTED_EDGE ( 'NONE', *, *, #59652, .T. ) ;
#89422 = B_SPLINE_CURVE_WITH_KNOTS ( 'NONE', 3,
 ( #59992, #4309, #21519, #97543 ),
 .UNSPECIFIED., .F., .F.,
 ( 4, 4 ),
 ( 0.7749614532321769111, 1.000000000000000000 ),
 .UNSPECIFIED. ) ;
#89423 = CARTESIAN_POINT ( 'NONE',  ( 194.7831888682312638, 266.3050563660650027, -7.630817898648720288 ) ) ;
#89424 = CARTESIAN_POINT ( 'NONE',  ( 178.7614077125761298, 259.1314107520656194, -10.22190746354665514 ) ) ;
#89425 = ADVANCED_FACE ( 'NONE', ( #6925 ), #37814, .F. ) ;
#89426 = CARTESIAN_POINT ( 'NONE',  ( 1.258015332399702757, 171.5333772461660828, 9.188101187500095079 ) ) ;
#89427 = CARTESIAN_POINT ( 'NONE',  ( 198.4860348845112981, 286.8590983175747056, -18.20461732983060088 ) ) ;
#89428 = CARTESIAN_POINT ( 'NONE',  ( 79.31945258186283354, 46.38531387088102775, -12.78158360291588203 ) ) ;
#89429 = CARTESIAN_POINT ( 'NONE',  ( 147.5749398328735822, 275.0397016159798227, -4.620786157167191099 ) ) ;
#89430 = EDGE_CURVE ( 'NONE', #94451, #43534, #68262, .T. ) ;
#89431 = CARTESIAN_POINT ( 'NONE',  ( 208.0045976720423084, 270.3724639545367836, 2.002128742561712471 ) ) ;
#89432 = CARTESIAN_POINT ( 'NONE',  ( 43.25185672232382217, 62.35734246106904521, 10.00000000000000000 ) ) ;
#89433 = CARTESIAN_POINT ( 'NONE',  ( 69.93400774566801203, 69.49255144249838168, 6.423098758560858990 ) ) ;
#89434 = CARTESIAN_POINT ( 'NONE',  ( 207.2383675728608239, 271.6996134166075763, 7.873592648726489784 ) ) ;
#89435 = ORIENTED_EDGE ( 'NONE', *, *, #2397, .T. ) ;
#89436 = CARTESIAN_POINT ( 'NONE',  ( -5.967884128652756637, 167.3615022471902591, -10.00000000000009592 ) ) ;
#89437 = CARTESIAN_POINT ( 'NONE',  ( 84.95610959662400319, 47.13610345203377960, 11.47420349594596800 ) ) ;
#89438 = CARTESIAN_POINT ( 'NONE',  ( 126.7237928014352804, 231.7202760586659736, -5.415160957724236172E-17 ) ) ;
#89439 = CARTESIAN_POINT ( 'NONE',  ( 21.31005897544419980, 27.70171378149919050, -9.188101187500004485 ) ) ;
#89441 = EDGE_CURVE ( 'NONE', #98683, #10673, #76825, .T. ) ;
#89440 = LINE ( 'NONE', #67069, #75029 ) ;
#89442 = CARTESIAN_POINT ( 'NONE',  ( 179.9400117196032340, 293.3606267625540340, -7.512348598490236284 ) ) ;
#89444 = CARTESIAN_POINT ( 'NONE',  ( 74.62401959271109320, 66.89443057110609914, 13.05059976691390311 ) ) ;
#89443 = CARTESIAN_POINT ( 'NONE',  ( 157.8562613713738472, 257.2319303423452652, 17.81420683562559404 ) ) ;
#89445 = CARTESIAN_POINT ( 'NONE',  ( 20.17205688044380452, 16.81029122506294371, 8.090169943749479842 ) ) ;
#89446 = ORIENTED_EDGE ( 'NONE', *, *, #86391, .T. ) ;
#89447 = CARTESIAN_POINT ( 'NONE',  ( 191.5694344253287511, 298.8390017285333897, 8.250976118904059575 ) ) ;
#89448 = CARTESIAN_POINT ( 'NONE',  ( 207.9188266366356572, 270.5210237456789173, -1.812149220496467317 ) ) ;
#89449 = CARTESIAN_POINT ( 'NONE',  ( 168.7096392155106344, 280.2107777274362093, -14.47775774749160682 ) ) ;
#89450 = CARTESIAN_POINT ( 'NONE',  ( 172.7932728846461998, 268.7208518688015602, -16.72593362587508992 ) ) ;
#89451 = CARTESIAN_POINT ( 'NONE',  ( 81.46946648389129564, 55.43478263998397182, -16.31964423845218093 ) ) ;
#89452 = ORIENTED_EDGE ( 'NONE', *, *, #49300, .F. ) ;
#89453 = CARTESIAN_POINT ( 'NONE',  ( 70.27326910769903634, 69.23385671948467746, 7.233023378589638064 ) ) ;
#89454 = DIRECTION ( 'NONE',  ( 0.8660254037844378194, 0.5000000000000014433, 0.000000000000000000 ) ) ;
#89456 = EDGE_CURVE ( 'NONE', #83671, #7444, #78721, .T. ) ;
#89455 = VECTOR ( 'NONE', #85589, 1000.000000000000000 ) ;
#89457 = B_SPLINE_SURFACE_WITH_KNOTS ( 'NONE', 3, 1, ( 
 ( #98441, #84258 ),
 ( #76615, #52796 ),
 ( #83755, #37595 ),
 ( #14316, #99428 ),
 ( #30005, #60889 ),
 ( #22411, #14805 ),
 ( #45688, #38085 ),
 ( #68997, #75137 ),
 ( #30508, #61399 ),
 ( #92351, #46184 ),
 ( #77103, #7706 ),
 ( #69503, #90368 ),
 ( #59392, #20947 ),
 ( #82770, #13337 ),
 ( #5715, #36604 ),
 ( #94348, #71030 ),
 ( #9212, #93855 ),
 ( #2122, #39083 ),
 ( #87292, #93342 ),
 ( #79155, #31493 ),
 ( #24902, #24410 ),
 ( #9736, #40591 ),
 ( #48724, #85252 ),
 ( #611, #23392 ),
 ( #8711, #86266 ),
 ( #32516, #69996 ),
 ( #8213, #71530 ),
 ( #63409, #54282 ),
 ( #33004, #63905 ),
 ( #15797, #55286 ),
 ( #1116, #47199 ) ),
 .UNSPECIFIED., .F., .F., .F.,
 ( 4, 3, 3, 3, 3, 3, 3, 3, 3, 3, 4 ),
 ( 2, 2 ),
 ( 0.000000000000000000, 0.1122669598086777354, 0.2243161639709747579, 0.3396355846219261121, 0.4553962076585106877, 0.5677860799922511692, 0.6749047109689668700, 0.7773884377078540409, 0.8775581155834283331, 0.9782364162377975569, 1.000000000000000000 ),
 ( 0.000000000000000000, 1.000000000000000000 ),
 .UNSPECIFIED. ) ;
#89458 = EDGE_CURVE ( 'NONE', #84833, #98290, #72558, .T. ) ;
#89459 = LINE ( 'NONE', #42287, #92684 ) ;
#89460 = CARTESIAN_POINT ( 'NONE',  ( 197.2265362901041499, 271.3495626856545755, 12.05940019673365882 ) ) ;
#89461 = CARTESIAN_POINT ( 'NONE',  ( 182.0535125315628875, 295.0180786344971011, 4.789782204045892833 ) ) ;
#89462 = CARTESIAN_POINT ( 'NONE',  ( 183.6422324172568210, 264.5785696717482551, 14.31652553825990104 ) ) ;
#89463 = CARTESIAN_POINT ( 'NONE',  ( 150.7717849006677397, 278.2227778944624674, -0.0001987781867447356013 ) ) ;
#89464 = ORIENTED_EDGE ( 'NONE', *, *, #91884, .F. ) ;
#89465 = CARTESIAN_POINT ( 'NONE',  ( 3.631266576971075910, 20.83478043621385467, -8.090169943749479842 ) ) ;
#89466 = CARTESIAN_POINT ( 'NONE',  ( 46.08672700828314817, 69.01776843458344501, -10.00000000000000000 ) ) ;
#89467 = ORIENTED_EDGE ( 'NONE', *, *, #84497, .F. ) ;
#89468 = CARTESIAN_POINT ( 'NONE',  ( 169.8382097412835492, 278.9609387177634403, 15.53294725421295475 ) ) ;
#89469 = CARTESIAN_POINT ( 'NONE',  ( 147.6054094044680198, 274.9869267698931594, -8.596541856229405809 ) ) ;
#89470 = CARTESIAN_POINT ( 'NONE',  ( 156.0496192001932911, 261.9777799244599805, -16.96333935241061397 ) ) ;
#89471 = VERTEX_POINT ( 'NONE', #72636 ) ;
#89472 = CARTESIAN_POINT ( 'NONE',  ( 78.86792953187128319, 59.60067377931095933, 16.50582274385373438 ) ) ;
#89473 = DIRECTION ( 'NONE',  ( 0.5000000000000013323, -0.8660254037844378194, 0.000000000000000000 ) ) ;
#89474 = CIRCLE ( 'NONE', #44115, 0.1418229129681522482 ) ;
#89475 = CARTESIAN_POINT ( 'NONE',  ( 74.72875307343204554, 53.51675845243507723, 16.07614988730082928 ) ) ;
#89476 = EDGE_LOOP ( 'NONE', ( #71407, #38072, #63754, #36754 ) ) ;
#89477 = CARTESIAN_POINT ( 'NONE',  ( 80.66154599400290692, 223.5024278399160949, -9.188101187500093303 ) ) ;
#89478 = CARTESIAN_POINT ( 'NONE',  ( 155.0032822503481498, 262.1734351328947241, 17.58937370742663830 ) ) ;
#89479 = LINE ( 'NONE', #20038, #50479 ) ;
#89480 = CARTESIAN_POINT ( 'NONE',  ( 184.8337230598654628, 259.8048592364006595, -5.814933208005341747 ) ) ;
#89481 = VERTEX_POINT ( 'NONE', #88878 ) ;
#89482 = EDGE_CURVE ( 'NONE', #82234, #66081, #70594, .T. ) ;
#89483 = EDGE_LOOP ( 'NONE', ( #4829, #91950, #43065, #65417 ) ) ;
#89484 = DIRECTION ( 'NONE',  ( 0.5000000000000048850, -0.8660254037844358210, 0.000000000000000000 ) ) ;
#89485 = ORIENTED_EDGE ( 'NONE', *, *, #69149, .F. ) ;
#89486 = CARTESIAN_POINT ( 'NONE',  ( 192.6310446484023089, 294.0709696340792902, 14.41910184865714584 ) ) ;
#89487 = ORIENTED_EDGE ( 'NONE', *, *, #36677, .T. ) ;
#89488 = CARTESIAN_POINT ( 'NONE',  ( 76.00560383303448475, 63.90649832781891604, 14.64634901227351449 ) ) ;
#89489 = CARTESIAN_POINT ( 'NONE',  ( 89.84776793077681134, 45.10341964059156794, 0.3078307376628255376 ) ) ;
#89490 = ORIENTED_EDGE ( 'NONE', *, *, #93781, .F. ) ;
#89491 = ADVANCED_FACE ( 'NONE', ( #11823 ), #88044, .F. ) ;
#89492 = CARTESIAN_POINT ( 'NONE',  ( 182.8998698049672100, 279.8255271273169456, -17.32748555055102813 ) ) ;
#89493 = CARTESIAN_POINT ( 'NONE',  ( 82.09195791283381993, 41.10995726237445069, 3.277656812944607090 ) ) ;
#89494 = CARTESIAN_POINT ( 'NONE',  ( 147.1444650661958065, 275.7853057832419381, -6.658585314799819521 ) ) ;
#89495 = DIRECTION ( 'NONE',  ( -0.5000000000000014433, 0.8660254037844379305, 0.000000000000000000 ) ) ;
#89496 = LINE ( 'NONE', #49438, #80948 ) ;
#89497 = CARTESIAN_POINT ( 'NONE',  ( 18.88643602551048417, 33.83705186507754092, 3.090169943749475401 ) ) ;
#89498 = EDGE_CURVE ( 'NONE', #31479, #83705, #25949, .T. ) ;
#89499 = CARTESIAN_POINT ( 'NONE',  ( 134.8963869060034142, 254.8149278399161233, -9.188101187500095079 ) ) ;
#89500 = CARTESIAN_POINT ( 'NONE',  ( 195.7590296971629300, 291.5824098545663219, -17.26820314939903156 ) ) ;
#89501 = VERTEX_POINT ( 'NONE', #59879 ) ;
#89502 = CARTESIAN_POINT ( 'NONE',  ( -2.073866539663252073, 26.60322154129611505, 10.00000000000000000 ) ) ;
#89503 = ORIENTED_EDGE ( 'NONE', *, *, #34139, .F. ) ;
#89504 = ADVANCED_FACE ( 'NONE', ( #1090 ), #24385, .T. ) ;
#89505 = CARTESIAN_POINT ( 'NONE',  ( 197.9901163037401943, 272.1418500761980681, -13.83221381771805625 ) ) ;
#89507 = EDGE_LOOP ( 'NONE', ( #63658, #13234, #60031, #58626 ) ) ;
#89506 = CARTESIAN_POINT ( 'NONE',  ( 203.0372054888979392, 271.5441584837204800, 9.486415998612690359 ) ) ;
#89508 = EDGE_CURVE ( 'NONE', #32335, #23143, #93, .T. ) ;
#89509 = LINE ( 'NONE', #88517, #10993 ) ;
#89510 = CARTESIAN_POINT ( 'NONE',  ( -0.4289299871626708338, 163.8927522451418213, 10.00000000000009948 ) ) ;
#89511 = DIRECTION ( 'NONE',  ( -1.000000000000000000, 0.000000000000000000, 0.000000000000000000 ) ) ;
#89512 = CARTESIAN_POINT ( 'NONE',  ( 156.7314430005651786, 279.2576428315608723, 7.355496758818486747 ) ) ;
#89513 = CARTESIAN_POINT ( 'NONE',  ( 70.97534519514762508, 61.01255604146208356, 14.53188312944952543 ) ) ;
#89514 = CARTESIAN_POINT ( 'NONE',  ( -115.0954152546897973, 78.37593066204027537, -37.49999999999999289 ) ) ;
#89515 = CARTESIAN_POINT ( 'NONE',  ( 86.23748403073643942, 43.56198212328983033, 3.817419489612863703 ) ) ;
#89516 = CARTESIAN_POINT ( 'NONE',  ( 88.26483236760812190, 44.33866273282983173, -2.345556310904765684 ) ) ;
#89517 = VERTEX_POINT ( 'NONE', #93315 ) ;
#89518 = CARTESIAN_POINT ( 'NONE',  ( 147.6508870500795467, 274.9081571770856272, -8.950912509993816712 ) ) ;
#89519 = ORIENTED_EDGE ( 'NONE', *, *, #93904, .F. ) ;
#89520 = CARTESIAN_POINT ( 'NONE',  ( 160.4603375272029382, 276.0096574431570389, 12.65041034736400505 ) ) ;
#89521 = LINE ( 'NONE', #33794, #71301 ) ;
#89522 = FACE_OUTER_BOUND ( 'NONE', #50068, .T. ) ;
#89523 = CARTESIAN_POINT ( 'NONE',  ( 149.5633513747893346, 271.5956717990251832, 12.83777201928511325 ) ) ;
#89525 = VECTOR ( 'NONE', #3064, 1000.000000000000000 ) ;
#89524 = CARTESIAN_POINT ( 'NONE',  ( 160.7925456682749257, 272.6590809960079014, 15.51096013201097534 ) ) ;
#89527 = CARTESIAN_POINT ( 'NONE',  ( 88.28417999105286640, 44.35115056094939234, 2.384166010199538110 ) ) ;
#89526 = CARTESIAN_POINT ( 'NONE',  ( 8.004356468201564212, 74.63722199011714054, -10.00000000000000000 ) ) ;
#89528 = CARTESIAN_POINT ( 'NONE',  ( 158.8270733235451075, 260.0119502166541565, 17.68969926203419618 ) ) ;
#89529 = ORIENTED_EDGE ( 'NONE', *, *, #45133, .F. ) ;
#89530 = VERTEX_POINT ( 'NONE', #53762 ) ;
#89531 = CARTESIAN_POINT ( 'NONE',  ( 76.91358264944020107, 60.84600432610378107, -15.73813892003315651 ) ) ;
#89532 = CARTESIAN_POINT ( 'NONE',  ( 117.1033946842824633, 249.9637435831424739, 2.679491924311251605 ) ) ;
#89533 = AXIS2_PLACEMENT_3D ( 'NONE', #56851, #85835, #2180 ) ;
#89534 = CARTESIAN_POINT ( 'NONE',  ( 69.86610170196659908, 66.23337933603376371, -10.74216025327337931 ) ) ;
#89535 = CARTESIAN_POINT ( 'NONE',  ( 67.09968926803097133, 66.79733971661106295, -9.013546469615247858 ) ) ;
#89536 = CARTESIAN_POINT ( 'NONE',  ( 152.8522706834672533, 265.8990964544007056, 17.63080661522264947 ) ) ;
#89537 = CARTESIAN_POINT ( 'NONE',  ( 80.95554863947107549, 43.36305847308316430, -9.979587924406191135 ) ) ;
#89538 = CARTESIAN_POINT ( 'NONE',  ( 202.7282074973916792, 277.5114398175890642, -15.40750263959311184 ) ) ;
#89539 = CARTESIAN_POINT ( 'NONE',  ( -0.5554856785977280165, 179.6744531367911577, 4.594050593750047540 ) ) ;
#89540 = CARTESIAN_POINT ( 'NONE',  ( 95.24857461505581568, 234.9869531367911293, 4.594050593750046652 ) ) ;
#89541 = CARTESIAN_POINT ( 'NONE',  ( 154.9048824156581361, 262.3438686460345366, -17.40627786727128168 ) ) ;
#89542 = CARTESIAN_POINT ( 'NONE',  ( 48.99872857692556494, 187.5494855054051868, -2.679491924311248496 ) ) ;
#89543 = CARTESIAN_POINT ( 'NONE',  ( 180.5275139809070595, 254.9285515434814329, -2.470345461842613499 ) ) ;
#89544 = CARTESIAN_POINT ( 'NONE',  ( 77.94050277262006432, 51.16694309523679607, 15.34650497222302334 ) ) ;
#89545 = AXIS2_PLACEMENT_3D ( 'NONE', #48030, #64238, #9560 ) ;
#89546 = CARTESIAN_POINT ( 'NONE',  ( 75.82794950087699704, 51.68186498792067596, 15.74941689662516531 ) ) ;
#89547 = DIRECTION ( 'NONE',  ( -0.000000000000000000, -0.000000000000000000, 1.000000000000000000 ) ) ;
#89548 = CARTESIAN_POINT ( 'NONE',  ( 194.1972774922283236, 294.2874440223457100, -15.09915398317898649 ) ) ;
#89549 = CARTESIAN_POINT ( 'NONE',  ( 84.57934031330240998, 50.64028946732422298, 13.68816099377781015 ) ) ;
#89550 = LINE ( 'NONE', #5400, #9250 ) ;
#89551 = DIRECTION ( 'NONE',  ( 1.000000000000000000, 0.000000000000000000, 0.000000000000000000 ) ) ;
#89552 = CARTESIAN_POINT ( 'NONE',  ( 172.9031624820008233, 263.9926013823168205, -15.45005316810910578 ) ) ;
#89553 = CARTESIAN_POINT ( 'NONE',  ( 80.66154599400290692, 223.5024278399160949, -9.188101187500093303 ) ) ;
#89554 = CARTESIAN_POINT ( 'NONE',  ( 207.8718670335145475, 270.6023601641878713, -6.322166851501095586 ) ) ;
#89556 = EDGE_CURVE ( 'NONE', #38703, #32075, #23870, .T. ) ;
#89555 = CARTESIAN_POINT ( 'NONE',  ( 88.07426949318437437, 43.62472922332415237, 0.07787791115677746012 ) ) ;
#89557 = CARTESIAN_POINT ( 'NONE',  ( 71.94941146435354540, 134.4047874917408478, -22.49999999999983658 ) ) ;
#89559 = CARTESIAN_POINT ( 'NONE',  ( 152.3267809444392071, 266.8092713812532679, 15.53817502085608204 ) ) ;
#89558 = CARTESIAN_POINT ( 'NONE',  ( 190.5217943342473745, 281.4870030958396683, 17.81127109971334121 ) ) ;
#89560 = CARTESIAN_POINT ( 'NONE',  ( 151.3999564459286375, 268.4145785023736153, -15.40574304386609050 ) ) ;
#89561 = DIRECTION ( 'NONE',  ( 0.000000000000000000, -0.000000000000000000, 1.000000000000000000 ) ) ;
#89562 = CARTESIAN_POINT ( 'NONE',  ( 146.9978162861947908, 276.0393089210717790, -5.134868500856280882 ) ) ;
#89563 = CARTESIAN_POINT ( 'NONE',  ( 86.70600090578749075, 46.44620277030321631, -9.070728233001970509 ) ) ;
#89564 = VERTEX_POINT ( 'NONE', #22876 ) ;
#89565 = CARTESIAN_POINT ( 'NONE',  ( 26.56574046957052460, 17.19860640527293327, 2.839279412974134775 ) ) ;
#89566 = DIRECTION ( 'NONE',  ( 0.001368469433193686413, -0.9999990636452668058, 0.000000000000000000 ) ) ;
#89567 = CARTESIAN_POINT ( 'NONE',  ( 29.54281338067077911, 40.55466486950702176, -1.111400068045478839E-16 ) ) ;
#89568 = CARTESIAN_POINT ( 'NONE',  ( 55.51991954004235907, 212.8615022471903160, 5.000000000000046185 ) ) ;
#89569 = EDGE_CURVE ( 'NONE', #166, #8200, #88791, .T. ) ;
#89570 = B_SPLINE_CURVE_WITH_KNOTS ( 'NONE', 3,
 ( #57866, #74598, #51254, #82718, #34572, #20888, #67457, #59336, #19888, #50759, #88845, #81712, #75081, #50267, #81220, #11796, #12285, #98385, #12793, #42651, #5173, #36052, #43656, #73585, #43145, #4678, #35568, #89809, #28976, #20382, #82220 ),
 .UNSPECIFIED., .F., .F.,
 ( 4, 3, 3, 3, 3, 3, 3, 3, 3, 3, 4 ),
 ( 0.000000000000000000, 0.1333490885032311002, 0.3007194338854346505, 0.4699862290245186980, 0.5844252810809363874, 0.6686540514502655741, 0.7354980260655468172, 0.8028463152565521455, 0.8633854507757170449, 0.9437142632667351316, 1.000000000000000000 ),
 .UNSPECIFIED. ) ;
#89571 = EDGE_CURVE ( 'NONE', #22609, #31605, #23993, .T. ) ;
#89572 = CARTESIAN_POINT ( 'NONE',  ( 70.92847601347175157, 61.07039847582737480, 15.02503073586101934 ) ) ;
#89573 = CARTESIAN_POINT ( 'NONE',  ( 153.6515342823389290, 266.9718399987636417, 16.58081301308793698 ) ) ;
#89574 = CARTESIAN_POINT ( 'NONE',  ( 186.2855123196275713, 281.1790728086402282, -17.65699997733639037 ) ) ;
#89576 =( BOUNDED_CURVE ( )  B_SPLINE_CURVE ( 2, ( #43608, #50707, #58795, #74545, #18342, #12234, #43094, #74036, #35517 ),
 .UNSPECIFIED., .F., .T. ) 
 B_SPLINE_CURVE_WITH_KNOTS ( ( 3, 2, 2, 2, 3 ),
 ( 0.2862903225806451846, 0.2876344086021505597, 0.2903225806451613100, 0.2930107526881720603, 0.2943548387096774355 ),
 .UNSPECIFIED. ) 
 CURVE ( )  GEOMETRIC_REPRESENTATION_ITEM ( )  RATIONAL_B_SPLINE_CURVE ( ( 0.9330127018922194093, 0.9330127018922194093, 1.000000000000000000, 0.8660254037844387076, 1.000000000000000000, 0.8660254037844387076, 1.000000000000000000, 0.9330127018922194093, 0.9330127018922194093 ) ) 
 REPRESENTATION_ITEM ( '' )  );
#89575 = CARTESIAN_POINT ( 'NONE',  ( 135.6272693901029243, 259.1115022471903444, -5.000000000000047962 ) ) ;
#89577 = CYLINDRICAL_SURFACE ( 'NONE', #18176, 45.19948692389423428 ) ;
#89578 = CARTESIAN_POINT ( 'NONE',  ( 75.44698045856164015, 53.24411920270586762, 16.49076459687135809 ) ) ;
#89579 = ORIENTED_EDGE ( 'NONE', *, *, #69593, .F. ) ;
#89580 = CARTESIAN_POINT ( 'NONE',  ( -19.68164973832074338, 92.92611600555152052, 59.99999999999999289 ) ) ;
#89581 = CARTESIAN_POINT ( 'NONE',  ( 168.7200283246967274, 248.5543435357514568, -1.887890150557830271 ) ) ;
#89582 = ORIENTED_EDGE ( 'NONE', *, *, #37923, .T. ) ;
#89583 = DIRECTION ( 'NONE',  ( 0.5000000000000013323, -0.8660254037844378194, 0.000000000000000000 ) ) ;
#89584 = CARTESIAN_POINT ( 'NONE',  ( 84.98597642252352102, 42.67336299467312699, 3.100190142275117022 ) ) ;
#89585 = VERTEX_POINT ( 'NONE', #99897 ) ;
#89586 = CARTESIAN_POINT ( 'NONE',  ( 86.09173314450353587, 43.00402348852082923, 1.099162958027281034 ) ) ;
#89587 = VERTEX_POINT ( 'NONE', #7683 ) ;
#89588 = CARTESIAN_POINT ( 'NONE',  ( 192.7874605187217014, 292.5376213369709149, 15.36506066506490598 ) ) ;
#89589 = CARTESIAN_POINT ( 'NONE',  ( 158.3666238253319705, 256.3479566418141076, 17.18714134412729777 ) ) ;
#89590 = CARTESIAN_POINT ( 'NONE',  ( 157.7201504851624918, 257.9064828177920958, -16.69192179801337161 ) ) ;
#89591 = CARTESIAN_POINT ( 'NONE',  ( 204.1512742367690976, 273.0118811181309866, 11.00484496069812224 ) ) ;
#89592 = CARTESIAN_POINT ( 'NONE',  ( 83.59149176045259821, 49.15513213620079824, 13.56910806411459980 ) ) ;
#89593 = CLOSED_SHELL ( 'NONE', ( #96, #3356, #78904, #98140, #48017, #48107, #38625, #3654, #78289, #96993, #73434, #34536, #29475, #27008, #82558, #87071, #47763, #7029, #16556, #66765, #15756, #22075, #35883, #7663, #16428, #51120, #29896, #70757, #36333, #12007, #73204, #59753, #48622, #32100, #21709, #1828, #80350, #35374, #32679, #77860, #43218, #33294, #80301, #80615, #54882, #24472, #57860, #28651, #61823, #51576, #43554, #93386, #51588, #2360, #74579, #72740, #79018, #71888, #39576, #36331, #91931, #64710, #1815, #26844, #66426, #3330, #57332, #80677, #88000, #73721, #32007, #81518 ) ) ;
#89594 = CARTESIAN_POINT ( 'NONE',  ( 34.69977369993910798, 22.96004757982091959, -5.678558825948275768 ) ) ;
#89595 = CARTESIAN_POINT ( 'NONE',  ( 73.35648102757406264, 60.49408656809458051, -15.23552882400795028 ) ) ;
#89596 = DIRECTION ( 'NONE',  ( -0.03304531753666254540, -0.9994538543569189137, 0.000000000000000000 ) ) ;
#89597 =( BOUNDED_CURVE ( )  B_SPLINE_CURVE ( 2, ( #36664, #98504, #83315, #13877, #75691, #37172, #68070, #16371, #55350 ),
 .UNSPECIFIED., .F., .T. ) 
 B_SPLINE_CURVE_WITH_KNOTS ( ( 3, 2, 2, 2, 3 ),
 ( 0.5040322580645161255, 0.5053763440860215006, 0.5080645161290322509, 0.5107526881720430012, 0.5120967741935483764 ),
 .UNSPECIFIED. ) 
 CURVE ( )  GEOMETRIC_REPRESENTATION_ITEM ( )  RATIONAL_B_SPLINE_CURVE ( ( 0.9330127018922194093, 0.9330127018922194093, 1.000000000000000000, 0.8660254037844387076, 1.000000000000000000, 0.8660254037844387076, 1.000000000000000000, 0.9330127018922194093, 0.9330127018922194093 ) ) 
 REPRESENTATION_ITEM ( '' )  );
#89598 = CARTESIAN_POINT ( 'NONE',  ( 190.1058098001619499, 300.4953350946266823, 0.1248780210120518375 ) ) ;
#89599 = ORIENTED_EDGE ( 'NONE', *, *, #46124, .T. ) ;
#89600 = ORIENTED_EDGE ( 'NONE', *, *, #10980, .F. ) ;
#89601 = CARTESIAN_POINT ( 'NONE',  ( 81.39623687408305841, 42.43901693502521510, 7.471974766692582648 ) ) ;
#89602 = ADVANCED_FACE ( 'NONE', ( #92814 ), #59716, .F. ) ;
#89604 = DIRECTION ( 'NONE',  ( -1.000000000000000000, 0.000000000000000000, 0.000000000000000000 ) ) ;
#89603 = CARTESIAN_POINT ( 'NONE',  ( 163.7010375032499212, 247.1084811230698506, 6.649922295230481950 ) ) ;
#89605 = CARTESIAN_POINT ( 'NONE',  ( 85.70209702422732789, 48.64685655562228561, 12.37813881961889528 ) ) ;
#89606 = DIRECTION ( 'NONE',  ( 0.8660254037844395958, 0.4999999999999985567, 0.000000000000000000 ) ) ;
#89607 = AXIS2_PLACEMENT_3D ( 'NONE', #16474, #277, #63075 ) ;
#89608 = LINE ( 'NONE', #57643, #30202 ) ;
#89609 = CARTESIAN_POINT ( 'NONE',  ( 110.0000000000000000, 0.000000000000000000, 59.99999999999999289 ) ) ;
#89610 = CARTESIAN_POINT ( 'NONE',  ( 49.17298586869600996, 105.8308522718264584, -10.00000000000000000 ) ) ;
#89611 = CARTESIAN_POINT ( 'NONE',  ( 161.5780152162786294, 275.6215250102659979, -14.77109549141536604 ) ) ;
#89612 = VECTOR ( 'NONE', #100019, 1000.000000000000000 ) ;
#89613 = CARTESIAN_POINT ( 'NONE',  ( 182.0331739629101833, 256.8600016389484608, 5.117587312389543008 ) ) ;
#89614 = EDGE_CURVE ( 'NONE', #27521, #36145, #99724, .T. ) ;
#89615 = CARTESIAN_POINT ( 'NONE',  ( 94.19319292813476352, 231.3149278399160664, 9.188101187500093303 ) ) ;
#89616 = ORIENTED_EDGE ( 'NONE', *, *, #39192, .T. ) ;
#89617 = CARTESIAN_POINT ( 'NONE',  ( 15.48905510666703478, 53.35892832886757020, 59.99999999999999289 ) ) ;
#89618 = CARTESIAN_POINT ( 'NONE',  ( 163.2872205587920007, 276.9580280363520046, -14.32771847714696989 ) ) ;
#89619 = ORIENTED_EDGE ( 'NONE', *, *, #64577, .F. ) ;
#89620 = ORIENTED_EDGE ( 'NONE', *, *, #24343, .T. ) ;
#89621 = CARTESIAN_POINT ( 'NONE',  ( 86.98925081226386169, 46.40596221211884398, -8.809588356812486865 ) ) ;
#89622 = EDGE_CURVE ( 'NONE', #14275, #1030, #45980, .T. ) ;
#89623 = CARTESIAN_POINT ( 'NONE',  ( 176.7665383743514838, 292.6345017810178888, -2.761319672360143862 ) ) ;
#89624 = CARTESIAN_POINT ( 'NONE',  ( 157.1135969804030310, 258.5182628004787944, 17.19660297500358226 ) ) ;
#89625 = CARTESIAN_POINT ( 'NONE',  ( 206.3454060440500086, 273.2462681537123785, -9.268083217908118954 ) ) ;
#89626 = CARTESIAN_POINT ( 'NONE',  ( 207.1975773162273811, 271.0654058925244954, -3.690837417035307766 ) ) ;
#89627 = ORIENTED_EDGE ( 'NONE', *, *, #27080, .F. ) ;
#89628 = ORIENTED_EDGE ( 'NONE', *, *, #59084, .T. ) ;
#89629 = CARTESIAN_POINT ( 'NONE',  ( -54.25007008209492199, 32.21233689110872689, -10.00000000000000000 ) ) ;
#89630 = VERTEX_POINT ( 'NONE', #83050 ) ;
#89631 = CARTESIAN_POINT ( 'NONE',  ( 194.7008455304638233, 266.4113774656392479, -8.389308597226909470 ) ) ;
#89632 = CARTESIAN_POINT ( 'NONE',  ( 153.2303786119591678, 265.7391886871019437, 16.12463036271180883 ) ) ;
#89633 = CARTESIAN_POINT ( 'NONE',  ( 82.18459391862934638, 44.45332069473768399, 9.672573637705005112 ) ) ;
#89635 = CARTESIAN_POINT ( 'NONE',  ( 69.71517978252398962, 62.25915488727545721, -13.58123164448667985 ) ) ;
#89634 = CARTESIAN_POINT ( 'NONE',  ( 131.9738982639959488, 240.8768266524160140, -9.188101187500091527 ) ) ;
#89636 = CARTESIAN_POINT ( 'NONE',  ( 156.9694903541507074, 266.1758412851487492, -17.34135443527054576 ) ) ;
#89637 = ORIENTED_EDGE ( 'NONE', *, *, #61593, .F. ) ;
#89638 = CARTESIAN_POINT ( 'NONE',  ( 146.8516045228164160, 276.2925551239072774, 3.995954059407343273 ) ) ;
#89639 = CARTESIAN_POINT ( 'NONE',  ( 71.67038792483674570, 63.34331654576415360, 13.62529284351906078 ) ) ;
#89640 = CARTESIAN_POINT ( 'NONE',  ( 159.7692415128758228, 253.9185515433934768, -16.85856106119654285 ) ) ;
#89641 = CARTESIAN_POINT ( 'NONE',  ( 170.4855375986076638, 248.6613294790634541, -0.2716024841417116753 ) ) ;
#89642 = CARTESIAN_POINT ( 'NONE',  ( 178.5227689348290028, 285.2834003422560727, 13.20235085433959732 ) ) ;
#89643 = B_SPLINE_CURVE_WITH_KNOTS ( 'NONE', 3,
 ( #64769, #20171, #65742, #10569 ),
 .UNSPECIFIED., .F., .F.,
 ( 4, 4 ),
 ( 0.03159426384393204668, 0.04060813801016246311 ),
 .UNSPECIFIED. ) ;
#89644 = CARTESIAN_POINT ( 'NONE',  ( 76.07161074972545123, 51.48760201263585401, -16.16757060908070898 ) ) ;
#89645 = CARTESIAN_POINT ( 'NONE',  ( 196.6627808473781158, 280.4533039363431044, -16.65813739920714909 ) ) ;
#89646 = CARTESIAN_POINT ( 'NONE',  ( 130.4311169673963775, 236.1115022471901739, -5.000000000000041744 ) ) ;
#89647 = CARTESIAN_POINT ( 'NONE',  ( 80.26331314844821918, 51.25704456883815396, 15.00005997246581835 ) ) ;
#89648 = LINE ( 'NONE', #97234, #28469 ) ;
#89649 = CARTESIAN_POINT ( 'NONE',  ( 159.9770824720811220, 253.5585604421560788, -16.42166711341322483 ) ) ;
#89650 = CARTESIAN_POINT ( 'NONE',  ( 73.08094384907833785, 54.14441083166272506, 0.000000000000000000 ) ) ;
#89651 = CARTESIAN_POINT ( 'NONE',  ( 207.6163508138795635, 271.0449272387537576, -1.385071889578343152 ) ) ;
#89652 = EDGE_CURVE ( 'NONE', #1959, #38287, #30310, .T. ) ;
#89653 = CARTESIAN_POINT ( 'NONE',  ( -22.42236680055709641, 157.8615022471902591, 0.000000000000000000 ) ) ;
#89654 = AXIS2_PLACEMENT_3D ( 'NONE', #84689, #36545, #28969 ) ;
#89655 = CARTESIAN_POINT ( 'NONE',  ( 68.42965730954357184, 70.07997676687871547, -1.242414669626054957 ) ) ;
#89657 = CARTESIAN_POINT ( 'NONE',  ( -20.77833267539040918, 95.14038972553191797, 45.19944339805625333 ) ) ;
#89656 = CARTESIAN_POINT ( 'NONE',  ( 173.4026771546767804, 273.2456497557084845, -17.70700034978624515 ) ) ;
#89658 = CARTESIAN_POINT ( 'NONE',  ( -35.39007723419273788, 42.43010318828366678, 59.99999999999999289 ) ) ;
#89659 = CARTESIAN_POINT ( 'NONE',  ( 34.97582608256301739, 32.14441083166263979, 10.00000000000000533 ) ) ;
#89660 = CARTESIAN_POINT ( 'NONE',  ( 149.7259699431006652, 272.1435073784675751, -11.43438802284230249 ) ) ;
#89661 = CARTESIAN_POINT ( 'NONE',  ( 203.1044072055706806, 278.8598428092302584, -16.67109798570195878 ) ) ;
#89662 = DIRECTION ( 'NONE',  ( -0.6139877827364750296, 0.7893155279419930004, 0.000000000000000000 ) ) ;
#89663 = CARTESIAN_POINT ( 'NONE',  ( 81.92870213848958372, 43.19805473905109494, -8.210944645206849302 ) ) ;
#89664 = CARTESIAN_POINT ( 'NONE',  ( 12.00188267627663308, 186.9244531367911293, -4.594050593750046652 ) ) ;
#89665 = AXIS2_PLACEMENT_3D ( 'NONE', #84541, #15085, #82563 ) ;
#89666 = CARTESIAN_POINT ( 'NONE',  ( 43.32339510341152788, 202.4865022471903160, -10.00000000000009592 ) ) ;
#89667 = ORIENTED_EDGE ( 'NONE', *, *, #41483, .F. ) ;
#89670 = EDGE_CURVE ( 'NONE', #53889, #86525, #29513, .T. ) ;
#89669 = CARTESIAN_POINT ( 'NONE',  ( 86.82393771405537564, 45.90093866298671799, 8.916403221032373594 ) ) ;
#89668 = AXIS2_PLACEMENT_3D ( 'NONE', #91441, #76231, #29124 ) ;
#89671 = PLANE ( 'NONE',  #6289 ) ;
#89672 = CARTESIAN_POINT ( 'NONE',  ( 72.07067459802226495, 72.25717277724338317, -1.547674812006160305 ) ) ;
#89673 = CARTESIAN_POINT ( 'NONE',  ( 29.24128764430186322, 193.8149278399160664, 9.188101187500093303 ) ) ;
#89674 = CARTESIAN_POINT ( 'NONE',  ( 86.79998443407272646, 45.86195168027221314, 8.882059948630848467 ) ) ;
#89675 = CARTESIAN_POINT ( 'NONE',  ( 151.1699610800269511, 268.8129421616204695, -14.28929860221299286 ) ) ;
#89676 = CARTESIAN_POINT ( 'NONE',  ( 190.9335643195044838, 299.9403610588350944, -4.692880224846124548 ) ) ;
#89677 = CARTESIAN_POINT ( 'NONE',  ( 4.462289544239296468, 25.68290643055184574, 3.479690158560446702E-15 ) ) ;
#89678 = CARTESIAN_POINT ( 'NONE',  ( 203.2115566785326450, 269.6228474973083280, -7.486280564945728244 ) ) ;
#89679 = CARTESIAN_POINT ( 'NONE',  ( 178.7545946287733898, 293.8895248776133258, 2.709369586333742586 ) ) ;
#89680 = CARTESIAN_POINT ( 'NONE',  ( 179.7878600106018894, 276.7683181353822874, 16.31861665154247376 ) ) ;
#89681 = CARTESIAN_POINT ( 'NONE',  ( 181.0417453565561914, 279.3340925255673710, -16.14945566808648891 ) ) ;
#89682 = DIRECTION ( 'NONE',  ( 0.2649596321166021728, -0.4589235447807153423, -0.8480480961564252906 ) ) ;
#89683 = PRODUCT ( 'Upper Movable Jaw Swivel Body', 'Upper Movable Jaw Swivel Body', '', ( #60829 ) ) ;
#89684 = CARTESIAN_POINT ( 'NONE',  ( 87.10573541114747798, 46.00189626469253312, -8.174982887696250700 ) ) ;
#89685 = EDGE_CURVE ( 'NONE', #66081, #79277, #88795, .T. ) ;
#89686 = EDGE_CURVE ( 'NONE', #68396, #19346, #100021, .T. ) ;
#89687 = FACE_OUTER_BOUND ( 'NONE', #51520, .T. ) ;
#89688 = CARTESIAN_POINT ( 'NONE',  ( 96.22311351791105949, 216.3615022471902023, 5.000000000000051514 ) ) ;
#89689 = CARTESIAN_POINT ( 'NONE',  ( 7.984193807443177526, 186.9637435831424739, 2.679491924311251605 ) ) ;
#89690 = CARTESIAN_POINT ( 'NONE',  ( -69.50121871515369776, 62.11365277976253907, 59.99999999999999289 ) ) ;
#89691 = ORIENTED_EDGE ( 'NONE', *, *, #99932, .T. ) ;
#89692 = CARTESIAN_POINT ( 'NONE',  ( 59.22776434610305785, 198.8768266524159856, -9.188101187500091527 ) ) ;
#89693 = ORIENTED_EDGE ( 'NONE', *, *, #37903, .T. ) ;
#89694 = CARTESIAN_POINT ( 'NONE',  ( -19.65312891409030271, 93.06504152958497400, 10.00000000000000888 ) ) ;
#89695 = CARTESIAN_POINT ( 'NONE',  ( 47.39496755818312579, 108.2889530649357681, -10.00000000000000000 ) ) ;
#89696 = LINE ( 'NONE', #43533, #22381 ) ;
#89697 = ORIENTED_EDGE ( 'NONE', *, *, #8510, .F. ) ;
#89698 = DIRECTION ( 'NONE',  ( -0.6386832404231509441, -0.7694697644498993405, 0.000000000000000000 ) ) ;
#89699 = CARTESIAN_POINT ( 'NONE',  ( 207.4285356523023154, 271.3702326410368642, 7.833982582429932506 ) ) ;
#89700 = DIRECTION ( 'NONE',  ( -1.000000000000000000, 0.000000000000000000, 0.000000000000000000 ) ) ;
#89701 = CARTESIAN_POINT ( 'NONE',  ( 30.77620441319551503, 35.95586893147757479, 7.433330006724141015 ) ) ;
#89702 = CARTESIAN_POINT ( 'NONE',  ( 185.8599028000333817, 262.9727172135272326, 11.31732244974326207 ) ) ;
#89703 = CARTESIAN_POINT ( 'NONE',  ( 34.81516168915606357, 51.10768172523390973, -10.00000000000000000 ) ) ;
#89704 = CARTESIAN_POINT ( 'NONE',  ( 156.7423333928520890, 259.1613101971172455, 17.21575223094429319 ) ) ;
#89705 = VERTEX_POINT ( 'NONE', #63205 ) ;
#89706 = CARTESIAN_POINT ( 'NONE',  ( 19.86064915544625009, 12.26216523072493914, -2.296566073217252530E-15 ) ) ;
#89707 = CARTESIAN_POINT ( 'NONE',  ( 68.42452078367514900, 64.50266422004676770, 12.17129190631728441 ) ) ;
#89708 = CARTESIAN_POINT ( 'NONE',  ( -57.46197106626858186, 34.15416430719361074, 10.00000000000000000 ) ) ;
#89709 = PLANE ( 'NONE',  #13335 ) ;
#89710 = EDGE_LOOP ( 'NONE', ( #71692, #82007, #8359 ) ) ;
#89711 = CARTESIAN_POINT ( 'NONE',  ( 76.65983718867957464, 54.53321319951793811, 16.54430215486172528 ) ) ;
#89712 = CARTESIAN_POINT ( 'NONE',  ( 191.5766842709549280, 298.8264446275616137, 8.039910086100929831 ) ) ;
#89713 = CARTESIAN_POINT ( 'NONE',  ( 84.99999999999998579, 15.00000000000000000, 2.106367960268921369 ) ) ;
#89714 = VERTEX_POINT ( 'NONE', #46489 ) ;
#89715 = ADVANCED_FACE ( 'NONE', ( #9525 ), #31787, .T. ) ;
#89717 = DIRECTION ( 'NONE',  ( 1.000000000000000000, 0.000000000000000000, 0.000000000000000000 ) ) ;
#89716 = CARTESIAN_POINT ( 'NONE',  ( 207.5785076975260779, 271.1104734389944042, -6.824813054587777650 ) ) ;
#89718 = CARTESIAN_POINT ( 'NONE',  ( 196.4501996009505831, 290.3852684645433442, -17.82325615854289680 ) ) ;
#89719 = EDGE_LOOP ( 'NONE', ( #17526, #76280, #26378, #20164 ) ) ;
#89720 = CARTESIAN_POINT ( 'NONE',  ( 66.27921550192024824, 69.23555237665273410, -2.128515666495896852 ) ) ;
#89721 = DIRECTION ( 'NONE',  ( -0.9042435392811277728, -0.4270171210482544000, 0.000000000000000000 ) ) ;
#89722 = CARTESIAN_POINT ( 'NONE',  ( 81.90070505019525626, 55.28399500932853528, 16.25061773925407493 ) ) ;
#89723 = CARTESIAN_POINT ( 'NONE',  ( 78.12682272674805972, 61.49995998885079729, -16.15539878443392396 ) ) ;
#89724 = CARTESIAN_POINT ( 'NONE',  ( 121.0403275412173656, 234.5643266524160140, 9.188101187500095079 ) ) ;
#89725 = CARTESIAN_POINT ( 'NONE',  ( 111.9072422615758313, 246.9637435831425023, 2.679491924311251605 ) ) ;
#89726 = CARTESIAN_POINT ( 'NONE',  ( 85.81045474425822306, 231.8967562850347122, -4.648177544792955347E-16 ) ) ;
#89727 = EDGE_LOOP ( 'NONE', ( #80094, #94467 ) ) ;
#89728 = CARTESIAN_POINT ( 'NONE',  ( 164.4698008747318738, 245.7769439046653019, -6.272955660526681854 ) ) ;
#89729 = ORIENTED_EDGE ( 'NONE', *, *, #8174, .T. ) ;
#89730 = EDGE_LOOP ( 'NONE', ( #20911, #98311, #16557, #48610 ) ) ;
#89731 = CARTESIAN_POINT ( 'NONE',  ( 198.5558597050348908, 286.7381581807989051, 17.16554469393394200 ) ) ;
#89732 = CARTESIAN_POINT ( 'NONE',  ( 75.10797937051889051, 66.37172067175724521, -13.15131572357236323 ) ) ;
#89733 = CARTESIAN_POINT ( 'NONE',  ( 71.05451054047556170, 202.6423013555409796, -4.594050593750043987 ) ) ;
#89734 = CARTESIAN_POINT ( 'NONE',  ( 14.31700456906896868, 190.6199935810940929, 2.679491924311251605 ) ) ;
#89735 = CARTESIAN_POINT ( 'NONE',  ( 81.71596569511639530, 55.69046771286013353, 16.33797717450969955 ) ) ;
#89736 = CARTESIAN_POINT ( 'NONE',  ( 198.0355408163131585, 287.6393769322024241, 18.20720360189982756 ) ) ;
#89737 = CARTESIAN_POINT ( 'NONE',  ( -18.22861911365886201, 171.8297689869269504, -2.679491924311252049 ) ) ;
#89738 = CARTESIAN_POINT ( 'NONE',  ( 87.37622458635497935, 44.94434973981049808, 6.879737256407633339 ) ) ;
#89739 = VERTEX_POINT ( 'NONE', #78424 ) ;
#89740 = CARTESIAN_POINT ( 'NONE',  ( 69.12672858200174630, 64.33651235087042153, -11.97836756590942997 ) ) ;
#89741 = CARTESIAN_POINT ( 'NONE',  ( 201.4617167010348737, 281.7050662241970826, -17.43131506460443703 ) ) ;
#89742 = CARTESIAN_POINT ( 'NONE',  ( 203.3205561747472814, 278.4854618126124706, -15.14439614831292147 ) ) ;
#89743 = EDGE_LOOP ( 'NONE', ( #95865, #51419, #47068, #24243 ) ) ;
#89744 = CARTESIAN_POINT ( 'NONE',  ( -19.65312891409030271, 93.06504152958497400, 177.5919119679930134 ) ) ;
#89745 = CARTESIAN_POINT ( 'NONE',  ( 160.4627341472859428, 258.2288165694186546, -16.94036994928822182 ) ) ;
#89746 = CARTESIAN_POINT ( 'NONE',  ( 164.2540650184052708, 246.7815632513715514, 5.192739529124178688 ) ) ;
#89747 = AXIS2_PLACEMENT_3D ( 'NONE', #34609, #42690, #65509 ) ;
#89748 = LINE ( 'NONE', #65892, #916 ) ;
#89749 = ADVANCED_FACE ( 'NONE', ( #39380 ), #70814, .F. ) ;
#89750 = PLANE ( 'NONE',  #36498 ) ;
#89751 = ORIENTED_EDGE ( 'NONE', *, *, #42911, .F. ) ;
#89752 = CARTESIAN_POINT ( 'NONE',  ( 163.7012083107868534, 247.1081852757374975, -6.544933039329257518 ) ) ;
#89753 = CARTESIAN_POINT ( 'NONE',  ( 121.5540962550081190, 250.1744531367911009, 4.594050593750047540 ) ) ;
#89754 = ORIENTED_EDGE ( 'NONE', *, *, #1566, .F. ) ;
#89755 = CARTESIAN_POINT ( 'NONE',  ( 146.7434471017767521, 276.4798892723637209, 0.7354350123930684102 ) ) ;
#89756 = CARTESIAN_POINT ( 'NONE',  ( 72.03003869383933022, 67.53192604503671248, -11.37324896331792345 ) ) ;
#89757 = CARTESIAN_POINT ( 'NONE',  ( 43.53831125515428369, 65.97156238185917232, -10.00000000000000000 ) ) ;
#89758 = CARTESIAN_POINT ( 'NONE',  ( 204.4781092559247782, 276.4805210635553863, 13.30606382016679490 ) ) ;
#89759 = LINE ( 'NONE', #20328, #50230 ) ;
#89760 = ORIENTED_EDGE ( 'NONE', *, *, #26633, .T. ) ;
#89761 = CARTESIAN_POINT ( 'NONE',  ( 76.51707580940211528, 54.71355426065986194, 16.11649618684974428 ) ) ;
#89762 = CARTESIAN_POINT ( 'NONE',  ( 183.4890902768438536, 276.5613345365970304, -16.51246737540926546 ) ) ;
#89763 = CARTESIAN_POINT ( 'NONE',  ( 166.7438987807396416, 248.6309438778351364, -5.495826098545110838 ) ) ;
#89764 = CARTESIAN_POINT ( 'NONE',  ( 165.0260329286864760, 244.8135217264176049, -2.114260670082726890 ) ) ;
#89765 = CARTESIAN_POINT ( 'NONE',  ( 200.2169152151696210, 267.0719894846549778, 0.8300188801736234634 ) ) ;
#89766 = CARTESIAN_POINT ( 'NONE',  ( 172.6012549852709412, 290.2025030293380610, -5.021894074213228087 ) ) ;
#89767 = CARTESIAN_POINT ( 'NONE',  ( 196.2134504588463244, 270.7881804218938555, 11.99659543724280830 ) ) ;
#89768 = CARTESIAN_POINT ( 'NONE',  ( 16.25994779760269182, 31.16126292948895227, -6.180339887498951690 ) ) ;
#89769 = CARTESIAN_POINT ( 'NONE',  ( 149.7119746935222793, 271.3382486597900538, 12.05352563709836922 ) ) ;
#89770 = CARTESIAN_POINT ( 'NONE',  ( 169.1470411999185046, 285.5095826478136587, -9.079696797922760965 ) ) ;
#89771 = CARTESIAN_POINT ( 'NONE',  ( 202.7676489560256528, 279.4431252073101746, -16.04062356091568020 ) ) ;
#89772 = CARTESIAN_POINT ( 'NONE',  ( 161.2700728932001368, 251.3190353390782263, 13.72566802940053421 ) ) ;
#89773 = CARTESIAN_POINT ( 'NONE',  ( 134.6710330032098000, 241.8927522451418213, 10.00000000000009592 ) ) ;
#89774 = CARTESIAN_POINT ( 'NONE',  ( 183.0161482713612031, 278.8971254581520611, 17.42167469373847055 ) ) ;
#89775 = VERTEX_POINT ( 'NONE', #55091 ) ;
#89776 = CARTESIAN_POINT ( 'NONE',  ( 157.7861133721078772, 257.3534302411229646, 18.03837896619386783 ) ) ;
#89777 = CARTESIAN_POINT ( 'NONE',  ( 151.4188942279983223, 268.3817773016460251, -14.77302265413830895 ) ) ;
#89778 = CARTESIAN_POINT ( 'NONE',  ( -1.935626891937929139, 175.8149278399161233, 9.188101187500093303 ) ) ;
#89779 = CARTESIAN_POINT ( 'NONE',  ( 55.03304057046344866, 193.3923013555409796, 4.594050593750050204 ) ) ;
#89780 = CARTESIAN_POINT ( 'NONE',  ( 85.49770414599811375, 44.29146548767710101, 7.659876876720736583 ) ) ;
#89781 = CARTESIAN_POINT ( 'NONE',  ( 23.12210336471560623, 25.30066082961422325, -10.00000000000000533 ) ) ;
#89782 = CARTESIAN_POINT ( 'NONE',  ( 85.39369755680034757, 48.58767798792116821, 12.46940421135661481 ) ) ;
#89783 = CARTESIAN_POINT ( 'NONE',  ( 204.8385597977314490, 275.8562024115307167, -12.64672659107585240 ) ) ;
#89784 = CARTESIAN_POINT ( 'NONE',  ( 72.06656620204616104, 72.31304997165260318, -3.465063205002326452 ) ) ;
#89785 = CARTESIAN_POINT ( 'NONE',  ( 74.11229751948719979, 55.49134365809288028, -16.11695285934779065 ) ) ;
#89786 = CARTESIAN_POINT ( 'NONE',  ( 170.4061711814250941, 277.8873091166869358, -16.16315208799353442 ) ) ;
#89787 = CARTESIAN_POINT ( 'NONE',  ( 179.4666841005951312, 254.9493157538499304, -4.056432808702910009 ) ) ;
#89788 = CARTESIAN_POINT ( 'NONE',  ( 198.7520972810255842, 286.3982647288286785, 17.58825518441947722 ) ) ;
#89789 = EDGE_CURVE ( 'NONE', #22585, #59735, #1420, .T. ) ;
#89790 = AXIS2_PLACEMENT_3D ( 'NONE', #81395, #11963, #50441 ) ;
#89791 = EDGE_CURVE ( 'NONE', #58170, #42330, #1722, .T. ) ;
#89792 = CARTESIAN_POINT ( 'NONE',  ( 59.85004655896462111, 195.3615022471901739, 5.000000000000051514 ) ) ;
#89793 = CARTESIAN_POINT ( 'NONE',  ( 181.2925019527557993, 292.4819523310474096, 9.067989712515277745 ) ) ;
#89794 = CARTESIAN_POINT ( 'NONE',  ( 163.1953264782998758, 283.8895661455310915, -7.125257539458086598 ) ) ;
#89795 = EDGE_CURVE ( 'NONE', #34942, #23533, #56041, .T. ) ;
#89796 = CARTESIAN_POINT ( 'NONE',  ( 20.58103360645747770, 188.8149278399161233, -9.188101187500095079 ) ) ;
#89797 = CARTESIAN_POINT ( 'NONE',  ( 167.4367084379770461, 285.8522310990644542, 4.088904900943554743 ) ) ;
#89798 = ADVANCED_FACE ( 'NONE', ( #62184 ), #48518, .T. ) ;
#89799 = CARTESIAN_POINT ( 'NONE',  ( 78.72005499730052236, 59.93730459920318765, 16.11786052172796957 ) ) ;
#89800 = CARTESIAN_POINT ( 'NONE',  ( 36.75658403392715456, 24.14754757982092315, -5.678558825948276656 ) ) ;
#89801 = CARTESIAN_POINT ( 'NONE',  ( 161.3261849411383650, 273.2032229615781489, 15.91718547624222957 ) ) ;
#89802 = VECTOR ( 'NONE', #64733, 1000.000000000000000 ) ;
#89803 = CARTESIAN_POINT ( 'NONE',  ( 183.2210599555355088, 278.9435890925142303, 16.90865785365091156 ) ) ;
#89804 = CARTESIAN_POINT ( 'NONE',  ( 66.31795133315472413, 69.20145725301702555, 2.477662600322605879 ) ) ;
#89805 = CARTESIAN_POINT ( 'NONE',  ( 124.8019518427975356, 232.8615022471901739, 5.000000000000051514 ) ) ;
#89806 = CARTESIAN_POINT ( 'NONE',  ( 143.9266795097038596, 247.2365022471902023, 10.00000000000009948 ) ) ;
#89807 = CARTESIAN_POINT ( 'NONE',  ( 0.000000000000000000, 0.000000000000000000, 0.000000000000000000 ) ) ;
#89808 = CARTESIAN_POINT ( 'NONE',  ( 11.81506597172265316, 27.79752408145591502, -5.678558825948271327 ) ) ;
#89809 = CARTESIAN_POINT ( 'NONE',  ( 71.51113537273407417, 72.37632541024542832, 1.045464050329073080 ) ) ;
#89810 = CARTESIAN_POINT ( 'NONE',  ( 82.30806329515122854, 54.25783888570826718, 15.62849564502622535 ) ) ;
#89811 = CARTESIAN_POINT ( 'NONE',  ( 24.19030146973739193, 38.49624447322263876, 10.00000000000000000 ) ) ;
#89812 = CARTESIAN_POINT ( 'NONE',  ( -59.65739779450132829, 37.15562860896453401, -10.00000000000000000 ) ) ;
#89813 = ORIENTED_EDGE ( 'NONE', *, *, #77485, .T. ) ;
#89814 = CARTESIAN_POINT ( 'NONE',  ( 182.1439385020048860, 290.0253507885926183, 13.01467259685074573 ) ) ;
#89815 = CARTESIAN_POINT ( 'NONE',  ( 27.68909066282341058, 16.39040679176984128, 1.333680081654574804E-15 ) ) ;
#89816 = CARTESIAN_POINT ( 'NONE',  ( 75.07322640240430189, 53.47801449719656830, -16.05294907914215585 ) ) ;
#89817 = CARTESIAN_POINT ( 'NONE',  ( 81.09886180088987828, 42.51057861825624684, 7.870722850269344484 ) ) ;
#89818 = ORIENTED_EDGE ( 'NONE', *, *, #76246, .T. ) ;
#89819 = FACE_OUTER_BOUND ( 'NONE', #4298, .T. ) ;
#89820 = CARTESIAN_POINT ( 'NONE',  ( 67.20229271573394669, 69.31781426814865199, 1.387273778539772628 ) ) ;
#89821 = CARTESIAN_POINT ( 'NONE',  ( 66.40550710205239682, 68.63594664406403467, 4.834922236012838326 ) ) ;
#89822 = CARTESIAN_POINT ( 'NONE',  ( 155.6281496932864457, 261.0911329737299980, -18.07904265579665548 ) ) ;
#89823 = ORIENTED_EDGE ( 'NONE', *, *, #76170, .F. ) ;
#89824 = VERTEX_POINT ( 'NONE', #77920 ) ;
#89826 = CARTESIAN_POINT ( 'NONE',  ( 163.9942050550062049, 246.6007000282974673, 5.791111691696777974 ) ) ;
#89825 = CARTESIAN_POINT ( 'NONE',  ( -22.42236680055709641, 157.8615022471902591, 0.000000000000000000 ) ) ;
#89827 = CARTESIAN_POINT ( 'NONE',  ( 153.1745822862813498, 265.3408363824576668, 16.18092354043443493 ) ) ;
#89828 = VERTEX_POINT ( 'NONE', #8512 ) ;
#89829 = CARTESIAN_POINT ( 'NONE',  ( 88.39284856500222531, 43.98633817645592359, -2.257003550805378733 ) ) ;
#89830 = CARTESIAN_POINT ( 'NONE',  ( 80.09948508391848065, 57.43746099958096352, -16.59413991463535964 ) ) ;
#89831 = CARTESIAN_POINT ( 'NONE',  ( 174.5613027801699104, 262.3032192610774018, 14.37391627158726592 ) ) ;
#89832 = ORIENTED_EDGE ( 'NONE', *, *, #70539, .F. ) ;
#89833 = CARTESIAN_POINT ( 'NONE',  ( 78.09472128404415514, 61.02041436207807834, -15.89733411056267975 ) ) ;
#89834 = CARTESIAN_POINT ( 'NONE',  ( 78.58954130030575413, 50.31985150518112704, -14.97515835093867409 ) ) ;
#89835 = B_SPLINE_CURVE_WITH_KNOTS ( 'NONE', 3,
 ( #22774, #14177, #53651, #7062 ),
 .UNSPECIFIED., .F., .F.,
 ( 4, 4 ),
 ( 0.009239321009562585091, 0.01510611881184145515 ),
 .UNSPECIFIED. ) ;
#89836 = CARTESIAN_POINT ( 'NONE',  ( 149.4456112649506281, 271.7996036513546869, -12.95648166494593667 ) ) ;
#89837 = CARTESIAN_POINT ( 'NONE',  ( 81.04951158705246428, 43.05756051927024686, 9.551121383308712964 ) ) ;
#89838 = CIRCLE ( 'NONE', #73610, 45.19948692389423428 ) ;
#89839 = ORIENTED_EDGE ( 'NONE', *, *, #5915, .T. ) ;
#89840 = CARTESIAN_POINT ( 'NONE',  ( 177.2486161470519903, 269.3311939352316813, 16.08193494513130872 ) ) ;
#89841 = CARTESIAN_POINT ( 'NONE',  ( 206.3505875407052486, 273.2372935382459787, 11.62318091048137880 ) ) ;
#89842 = DIRECTION ( 'NONE',  ( -1.000000000000000000, 0.000000000000000000, 0.000000000000000000 ) ) ;
#89843 = EDGE_LOOP ( 'NONE', ( #36358, #67467, #5868, #3218 ) ) ;
#89844 = CARTESIAN_POINT ( 'NONE',  ( 149.0761751337341821, 272.4394858007734683, 11.56094486755886130 ) ) ;
#89845 = CARTESIAN_POINT ( 'NONE',  ( 171.7602284589083297, 263.3278815159662827, -15.48272920416244780 ) ) ;
#89846 = ORIENTED_EDGE ( 'NONE', *, *, #27823, .T. ) ;
#89847 = DIRECTION ( 'NONE',  ( -0.000000000000000000, -0.000000000000000000, -1.000000000000000000 ) ) ;
#89848 = VERTEX_POINT ( 'NONE', #908 ) ;
#89849 = CARTESIAN_POINT ( 'NONE',  ( 158.9550220667411224, 269.6099541869315317, 15.63534711726525650 ) ) ;
#89850 = CARTESIAN_POINT ( 'NONE',  ( 156.2799659027096482, 267.3694502300024851, -16.55794083374155079 ) ) ;
#89851 = CARTESIAN_POINT ( 'NONE',  ( 168.9959839960517343, 272.4983489875348823, 17.21357309856028550 ) ) ;
#89852 = DIRECTION ( 'NONE',  ( -0.000000000000000000, 0.000000000000000000, -1.000000000000000000 ) ) ;
#89853 = CARTESIAN_POINT ( 'NONE',  ( 190.0791367161676817, 299.5868483356907177, -4.299622452797303929 ) ) ;
#89854 = LINE ( 'NONE', #20429, #1002 ) ;
#89855 = CARTESIAN_POINT ( 'NONE',  ( 192.8325075361489382, 296.6512949269187516, 11.74553025762331515 ) ) ;
#89856 = CARTESIAN_POINT ( 'NONE',  ( 37.40555484421791732, 185.7365022471902023, 10.00000000000009948 ) ) ;
#89857 = CARTESIAN_POINT ( 'NONE',  ( 196.9614093077011034, 289.4998272791294767, -17.73636689563254265 ) ) ;
#89858 = VERTEX_POINT ( 'NONE', #15588 ) ;
#89859 = CARTESIAN_POINT ( 'NONE',  ( 77.52349842883717201, 56.82266075537747696, -16.19943627310666656 ) ) ;
#89860 = EDGE_CURVE ( 'NONE', #52219, #31824, #67641, .T. ) ;
#89861 = CARTESIAN_POINT ( 'NONE',  ( 165.0538309624641613, 244.7653741195639157, 2.311334310144196547 ) ) ;
#89862 = DIRECTION ( 'NONE',  ( -0.8944271909999158554, 0.000000000000000000, -0.4472135954999578722 ) ) ;
#89863 = DIRECTION ( 'NONE',  ( 0.000000000000000000, 0.000000000000000000, 1.000000000000000000 ) ) ;
#89864 = CARTESIAN_POINT ( 'NONE',  ( 190.5326571414909154, 300.2205002393729956, 2.724935789587299872 ) ) ;
#89865 = CARTESIAN_POINT ( 'NONE',  ( 32.35804664341760883, 67.52305595790635095, 59.99999999999999289 ) ) ;
#89866 = ORIENTED_EDGE ( 'NONE', *, *, #96045, .F. ) ;
#89867 = CARTESIAN_POINT ( 'NONE',  ( 81.22979812886450190, 55.45288652294036069, -16.34461090620092349 ) ) ;
#89868 = CARTESIAN_POINT ( 'NONE',  ( 195.3907986064563431, 271.8404647846490434, 14.62512701364267720 ) ) ;
#89869 = CARTESIAN_POINT ( 'NONE',  ( 174.5502087336647890, 274.2231652844577070, -17.67598756992128983 ) ) ;
#89870 = AXIS2_PLACEMENT_3D ( 'NONE', #36704, #67611, #78222 ) ;
#89871 = CARTESIAN_POINT ( 'NONE',  ( 160.0818573676674248, 253.3770849996428467, -14.73248899536566725 ) ) ;
#89872 = CARTESIAN_POINT ( 'NONE',  ( 148.5965889108988733, 273.2701535053342354, -9.061290301873665243 ) ) ;
#89873 = ORIENTED_EDGE ( 'NONE', *, *, #90378, .F. ) ;
#89874 = CARTESIAN_POINT ( 'NONE',  ( 167.4572242298301319, 253.2714284328981762, -12.01198848564598798 ) ) ;
#89875 = CARTESIAN_POINT ( 'NONE',  ( 205.6309316812484553, 272.7254639723831815, 10.07723110209571438 ) ) ;
#89876 = CARTESIAN_POINT ( 'NONE',  ( 153.1627746953036535, 265.3612877299463548, -17.72069958822647351 ) ) ;
#89878 = EDGE_CURVE ( 'NONE', #19964, #91708, #56083, .T. ) ;
#89877 = CARTESIAN_POINT ( 'NONE',  ( 164.2953672501826929, 246.0790718049323687, -2.576662677987826111 ) ) ;
#89879 = CARTESIAN_POINT ( 'NONE',  ( 24.54146915528859196, 191.6427522451419350, 10.00000000000009237 ) ) ;
#89880 = CARTESIAN_POINT ( 'NONE',  ( 124.1796696299359724, 236.3768266524159856, -9.188101187500093303 ) ) ;
#89881 = DIRECTION ( 'NONE',  ( -0.3782958374750610142, 0.000000000000000000, 0.9256847516023164468 ) ) ;
#89882 = CARTESIAN_POINT ( 'NONE',  ( 164.9647332961995403, 281.3995515670802092, -11.83162694151289429 ) ) ;
#89883 = CARTESIAN_POINT ( 'NONE',  ( 157.1837449796689725, 258.3967629017010381, 16.97243084443542216 ) ) ;
#89884 = CARTESIAN_POINT ( 'NONE',  ( 207.6256228060221076, 271.0288676772754002, 1.885008341157026646 ) ) ;
#89885 = CARTESIAN_POINT ( 'NONE',  ( 38.60536087060361154, 193.0958772461660544, -9.188101187500095079 ) ) ;
#89886 = CARTESIAN_POINT ( 'NONE',  ( 161.5431944097339851, 250.8459749958011287, 14.52339846942414603 ) ) ;
#89887 = ORIENTED_EDGE ( 'NONE', *, *, #7264, .T. ) ;
#89888 = ORIENTED_EDGE ( 'NONE', *, *, #69795, .F. ) ;
#89889 = CYLINDRICAL_SURFACE ( 'NONE', #54323, 7.499999999999992895 ) ;
#89890 = CARTESIAN_POINT ( 'NONE',  ( 74.43609056695282788, 68.34186375642043743, -11.37380148218260523 ) ) ;
#89891 = CARTESIAN_POINT ( 'NONE',  ( 71.74212438849298223, 71.89688598250658913, -2.523334318048504166 ) ) ;
#89892 = CARTESIAN_POINT ( 'NONE',  ( 76.38701104150307231, 51.11410097943224429, 16.04685272891217807 ) ) ;
#89893 = CARTESIAN_POINT ( 'NONE',  ( 81.85212985314085188, 41.17943844758806193, -5.658149982800025235 ) ) ;
#89894 = FACE_OUTER_BOUND ( 'NONE', #33871, .T. ) ;
#89895 = CARTESIAN_POINT ( 'NONE',  ( 176.1937425061808256, 285.1457250574052296, -12.61256593275989601 ) ) ;
#89896 = DIRECTION ( 'NONE',  ( -0.8660254037844387076, -0.4999999999999998890, -0.000000000000000000 ) ) ;
#89897 = CARTESIAN_POINT ( 'NONE',  ( 98.29796604426333317, 220.8927522451418213, 10.00000000000009592 ) ) ;
#89898 = ORIENTED_EDGE ( 'NONE', *, *, #4916, .T. ) ;
#89899 = CARTESIAN_POINT ( 'NONE',  ( 198.6181852710878104, 267.3834214339108257, -8.306438527148390705 ) ) ;
#89900 = CARTESIAN_POINT ( 'NONE',  ( 158.5924551307156491, 281.8915015218287863, -1.614670045172950763 ) ) ;
#89901 = DIRECTION ( 'NONE',  ( 0.000000000000000000, -0.000000000000000000, 1.000000000000000000 ) ) ;
#89902 = CARTESIAN_POINT ( 'NONE',  ( 7.238742955462222461, 184.1744531367911293, 4.594050593750047540 ) ) ;
#89903 = CARTESIAN_POINT ( 'NONE',  ( 151.1126408083691501, 268.9122237844355254, -15.82705194100464396 ) ) ;
#89904 = CARTESIAN_POINT ( 'NONE',  ( 72.52865609843787809, 57.51546068812135815, 16.29679984377914437 ) ) ;
#89905 = CARTESIAN_POINT ( 'NONE',  ( 71.52927238475341198, 59.05921948282066580, -15.82638290425087213 ) ) ;
#89906 = CARTESIAN_POINT ( 'NONE',  ( 66.41141984641225804, 68.22144906810552811, -4.374511944796394047 ) ) ;
#89907 = EDGE_CURVE ( 'NONE', #72231, #58877, #82271, .T. ) ;
#89908 = CARTESIAN_POINT ( 'NONE',  ( 46.88655524640979166, 204.0024278399160949, -9.188101187500093303 ) ) ;
#89909 = CARTESIAN_POINT ( 'NONE',  ( 164.4578252119609090, 245.7976863610386999, -6.211333091911165560 ) ) ;
#89910 = CARTESIAN_POINT ( 'NONE',  ( 204.9427641582406636, 275.6757151647582305, 14.40446820030680897 ) ) ;
#89911 = CARTESIAN_POINT ( 'NONE',  ( 69.30365146289868505, 68.49145811655579053, 7.529959361284295660 ) ) ;
#89912 = CARTESIAN_POINT ( 'NONE',  ( 66.18968672750138182, 68.49487770620631011, -4.881532527428047885 ) ) ;
#89913 = ORIENTED_EDGE ( 'NONE', *, *, #21394, .F. ) ;
#89914 = AXIS2_PLACEMENT_3D ( 'NONE', #20063, #12971, #35745 ) ;
#89915 = CARTESIAN_POINT ( 'NONE',  ( 2.620201125542898080, 178.9865022471903160, 10.00000000000009237 ) ) ;
#89916 = CARTESIAN_POINT ( 'NONE',  ( -13.11024591527734628, 27.99999999999999645, 32.50000000000000000 ) ) ;
#89917 = CARTESIAN_POINT ( 'NONE',  ( 134.5180214354952284, 236.2202760586659736, -5.415160957724236172E-17 ) ) ;
#89918 = CARTESIAN_POINT ( 'NONE',  ( 29.31840136419365805, 25.43085787977764056, -9.188101187500008038 ) ) ;
#89919 = CARTESIAN_POINT ( 'NONE',  ( 183.8381394033181095, 262.6696733492485691, 12.83785572541065356 ) ) ;
#89920 = EDGE_CURVE ( 'NONE', #89828, #70911, #31822, .T. ) ;
#89921 = DIRECTION ( 'NONE',  ( -0.8660254037844387076, -0.4999999999999998890, -0.000000000000000000 ) ) ;
#89922 = CARTESIAN_POINT ( 'NONE',  ( 81.98377181849168949, 58.72426045759348057, 0.1209609477998357385 ) ) ;
#89924 = CARTESIAN_POINT ( 'NONE',  ( 189.3135512084097627, 289.8933911928067459, 14.45002620918027603 ) ) ;
#89923 = CARTESIAN_POINT ( 'NONE',  ( 157.4177733328310467, 257.9914139036126812, 18.29188238796808363 ) ) ;
#89925 = CARTESIAN_POINT ( 'NONE',  ( 68.53556746510957964, 64.33380229643456971, 11.71290893539683076 ) ) ;
#89926 = ORIENTED_EDGE ( 'NONE', *, *, #62303, .T. ) ;
#89927 = CARTESIAN_POINT ( 'NONE',  ( 151.2455280670316711, 268.6820563007532314, 14.35914944935941229 ) ) ;
#89928 = CARTESIAN_POINT ( 'NONE',  ( 163.4095610489648323, 247.6133331511015570, 7.708395487792730094 ) ) ;
#89929 = LINE ( 'NONE', #20507, #70145 ) ;
#89930 = CARTESIAN_POINT ( 'NONE',  ( 170.0748205669605966, 266.3782777737114884, -16.69754429407689145 ) ) ;
#89931 = CARTESIAN_POINT ( 'NONE',  ( 197.3031208747801770, 273.3096235846996933, -13.48493542629869424 ) ) ;
#89932 = ORIENTED_EDGE ( 'NONE', *, *, #29628, .T. ) ;
#89933 = CARTESIAN_POINT ( 'NONE',  ( 69.27429168244785274, 67.49347697646621214, 8.920200208771037254 ) ) ;
#89934 = CARTESIAN_POINT ( 'NONE',  ( 170.3926468640515282, 283.5039894459525271, -11.04026963884475698 ) ) ;
#89935 = VECTOR ( 'NONE', #92793, 1000.000000000000000 ) ;
#89936 = CARTESIAN_POINT ( 'NONE',  ( 82.41914487369291464, 41.31337197830497132, 3.340431838514237750 ) ) ;
#89937 = CARTESIAN_POINT ( 'NONE',  ( 196.1373634161230939, 271.0470652014707298, 12.52493849620521438 ) ) ;
#89938 = B_SPLINE_CURVE_WITH_KNOTS ( 'NONE', 3,
 ( #64567, #11390, #40739, #64060, #25053, #25565, #49360, #65058, #18983, #73179, #17978, #87445, #55430, #95524, #16947, #48872, #86419, #79806, #9360, #2789, #40238, #41240, #71180, #72178, #1776, #26069, #75169, #36137, #59422, #52336, #28045, #5743, #66057, #19495, #29062, #13365, #20466, #67039, #35651, #68041, #97006, #97964, #4769, #89891, #27068, #75656 ),
 .UNSPECIFIED., .F., .F.,
 ( 4, 1, 1, 1, 2, 2, 1, 1, 1, 2, 2, 1, 1, 2, 2, 1, 1, 2, 2, 1, 1, 2, 2, 1, 2, 2, 1, 2, 2, 4 ),
 ( 0.000000000000000000, 0.06250000000001762479, 0.09375000000002652045, 0.1093750000000299621, 0.1171875000000316969, 0.1250000000000334177, 0.1875000000000454359, 0.2187500000000504596, 0.2343750000000519862, 0.2421875000000517919, 0.2500000000000515699, 0.3125000000000497935, 0.3437500000000499600, 0.3593750000000500711, 0.3750000000000501266, 0.4375000000000536793, 0.4687500000000536238, 0.4843750000000536238, 0.5000000000000535127, 0.5625000000000512923, 0.5937500000000489608, 0.6093750000000478506, 0.6250000000000466294, 0.6875000000000398570, 0.7187500000000370814, 0.7500000000000341949, 0.8125000000000272005, 0.8437500000000224265, 0.8750000000000176525, 1.000000000000000000 ),
 .UNSPECIFIED. ) ;
#89939 = AXIS2_PLACEMENT_3D ( 'NONE', #32220, #55013, #87508 ) ;
#89940 = CARTESIAN_POINT ( 'NONE',  ( 181.8805694890828590, 295.3104365690353461, 4.888136459776745824 ) ) ;
#89941 = CARTESIAN_POINT ( 'NONE',  ( 68.88895345938509251, 70.13622972219421570, 2.764439259769861934 ) ) ;
#89942 = CARTESIAN_POINT ( 'NONE',  ( 150.4247937244904847, 277.5422073757840735, -0.0002234595357659979081 ) ) ;
#89943 = CARTESIAN_POINT ( 'NONE',  ( 2.403541337051680493, 23.16126292948892740, -6.180339887498951690 ) ) ;
#89944 = CARTESIAN_POINT ( 'NONE',  ( 191.9824032073976241, 287.6194387751458521, -17.05427143794285882 ) ) ;
#89945 = ORIENTED_EDGE ( 'NONE', *, *, #21827, .T. ) ;
#89946 = CARTESIAN_POINT ( 'NONE',  ( 73.65799801046682660, 55.43801576298897515, 16.58642910536338633 ) ) ;
#89947 = CARTESIAN_POINT ( 'NONE',  ( -18.31116180715439512, 22.81812098060338911, -10.00000000000000000 ) ) ;
#89948 = CARTESIAN_POINT ( 'NONE',  ( 156.2927583276759265, 261.4325586500398799, -17.29092458739067339 ) ) ;
#89949 = ORIENTED_EDGE ( 'NONE', *, *, #93952, .T. ) ;
#89950 = PLANE ( 'NONE',  #68500 ) ;
#89951 = CARTESIAN_POINT ( 'NONE',  ( 185.2906591010065824, 291.2658010436550740, 11.98603346923743196 ) ) ;
#89952 = CARTESIAN_POINT ( 'NONE',  ( 164.3961040135806968, 245.9045906125373904, 7.095190383188031191 ) ) ;
#89953 = LINE ( 'NONE', #12943, #25392 ) ;
#89954 = FACE_OUTER_BOUND ( 'NONE', #33895, .T. ) ;
#89955 = ORIENTED_EDGE ( 'NONE', *, *, #40532, .T. ) ;
#89956 = CARTESIAN_POINT ( 'NONE',  ( 85.69549220138247847, 220.2833772461660544, -9.188101187500095079 ) ) ;
#89957 = DIRECTION ( 'NONE',  ( 0.000000000000000000, -1.000000000000000000, 0.000000000000000000 ) ) ;
#89958 = CARTESIAN_POINT ( 'NONE',  ( 189.9427917847951335, 300.2559228831493101, 3.234880823342468403 ) ) ;
#89959 = CARTESIAN_POINT ( 'NONE',  ( 81.21547345588363953, 42.27537644322796950, -7.379875351412039208 ) ) ;
#89960 = VERTEX_POINT ( 'NONE', #50489 ) ;
#89961 = EDGE_LOOP ( 'NONE', ( #41729, #60402, #29604, #83496 ) ) ;
#89962 = CARTESIAN_POINT ( 'NONE',  ( -3.078821053925192786, 157.4824982072974251, -4.415768667553307481E-15 ) ) ;
#89963 = ORIENTED_EDGE ( 'NONE', *, *, #69067, .T. ) ;
#89964 = CARTESIAN_POINT ( 'NONE',  ( 80.42949956019809576, 46.69659513737585144, 12.58869027114300820 ) ) ;
#89965 = ORIENTED_EDGE ( 'NONE', *, *, #6915, .F. ) ;
#89966 = CARTESIAN_POINT ( 'NONE',  ( 159.5402296058379932, 258.6146098258784605, 17.42708900733146393 ) ) ;
#89967 = FACE_OUTER_BOUND ( 'NONE', #15932, .T. ) ;
#89968 = ORIENTED_EDGE ( 'NONE', *, *, #95173, .T. ) ;
#89969 = CARTESIAN_POINT ( 'NONE',  ( 86.94711308317737064, 232.5530062829863027, -4.648177544792955347E-16 ) ) ;
#89970 = DIRECTION ( 'NONE',  ( -0.8660254037844387076, -0.4999999999999998890, -0.000000000000000000 ) ) ;
#89971 = LINE ( 'NONE', #67623, #56002 ) ;
#89972 = DIRECTION ( 'NONE',  ( -0.000000000000000000, -0.000000000000000000, -1.000000000000000000 ) ) ;
#89973 = B_SPLINE_CURVE_WITH_KNOTS ( 'NONE', 3,
 ( #66867, #20795, #51687, #13196 ),
 .UNSPECIFIED., .F., .F.,
 ( 4, 4 ),
 ( 2.510712456960930795E-15, 0.0006326563949759604621 ),
 .UNSPECIFIED. ) ;
#89974 = CARTESIAN_POINT ( 'NONE',  ( 73.90428922879758034, 67.91979487962545647, -11.48018831094223025 ) ) ;
#89975 = CARTESIAN_POINT ( 'NONE',  ( 165.3647683453818900, 265.5104300138660278, -16.61231484167872807 ) ) ;
#89976 = ORIENTED_EDGE ( 'NONE', *, *, #86789, .F. ) ;
#89977 = CARTESIAN_POINT ( 'NONE',  ( 66.00998368741205979, 68.68708060386751413, -0.4081457534283032262 ) ) ;
#89978 = CARTESIAN_POINT ( 'NONE',  ( 13.91516400911260298, 10.96004757982088584, -5.678558825948276656 ) ) ;
#89979 = VERTEX_POINT ( 'NONE', #12015 ) ;
#89981 = ADVANCED_FACE ( 'NONE', ( #58582 ), #44354, .F. ) ;
#89980 = AXIS2_PLACEMENT_3D ( 'NONE', #54061, #61671, #37865 ) ;
#89982 = CARTESIAN_POINT ( 'NONE',  ( 166.1657757771597232, 246.5300435090155702, 3.345633037118004971 ) ) ;
#89984 = ORIENTED_EDGE ( 'NONE', *, *, #79857, .F. ) ;
#89983 = CARTESIAN_POINT ( 'NONE',  ( 199.9670970817828959, 270.1972007199732388, 9.297565887923761707 ) ) ;
#89985 = CARTESIAN_POINT ( 'NONE',  ( -13.86269525828471849, 104.3301040240179418, 10.56608444709879713 ) ) ;
#89986 = CARTESIAN_POINT ( 'NONE',  ( 202.8499463704053198, 279.3005819042728604, 17.04674939340617001 ) ) ;
#89987 = ADVANCED_FACE ( 'NONE', ( #5406 ), #70290, .T. ) ;
#89988 = DIRECTION ( 'NONE',  ( -0.8660254037844359321, -0.5000000000000051070, -0.000000000000000000 ) ) ;
#89989 = CARTESIAN_POINT ( 'NONE',  ( 161.2692160765192000, 281.6605574864539676, -6.284999054169885468 ) ) ;
#89990 = CARTESIAN_POINT ( 'NONE',  ( 70.35604517217940668, 61.15948129931610566, 14.31845027234643375 ) ) ;
#89991 = AXIS2_PLACEMENT_3D ( 'NONE', #13931, #44810, #32107 ) ;
#89992 = CARTESIAN_POINT ( 'NONE',  ( 192.8204393314547929, 292.0303437406023477, -14.99545193480984295 ) ) ;
#89993 = CARTESIAN_POINT ( 'NONE',  ( 168.2231244631735763, 252.8766363897699136, 11.96496842206752298 ) ) ;
#89994 = CARTESIAN_POINT ( 'NONE',  ( 88.29571403098292137, 44.29400929412249610, -2.002076236142582122 ) ) ;
#89995 = ORIENTED_EDGE ( 'NONE', *, *, #84876, .F. ) ;
#89996 = CARTESIAN_POINT ( 'NONE',  ( 194.3387753395540472, 294.0423625616157892, -15.64827765940100868 ) ) ;
#89997 = CARTESIAN_POINT ( 'NONE',  ( 77.10839581433575063, 61.44820719566746448, -15.66518503319612066 ) ) ;
#89998 = ORIENTED_EDGE ( 'NONE', *, *, #54891, .T. ) ;
#90000 = EDGE_CURVE ( 'NONE', #51127, #77284, #14957, .T. ) ;
#89999 = CARTESIAN_POINT ( 'NONE',  ( 161.0848266318867843, 275.9577594623067398, 12.81057407668478909 ) ) ;
#90001 = CARTESIAN_POINT ( 'NONE',  ( 196.2350291401047571, 264.4780031501763347, 5.359379669934941859 ) ) ;
#90002 = CARTESIAN_POINT ( 'NONE',  ( 164.1105936565050740, 246.3991090570794427, -8.431210343695774156 ) ) ;
#90003 = CARTESIAN_POINT ( 'NONE',  ( 81.11634633033922626, 44.85415553531951360, -10.71945838295695808 ) ) ;
#90004 = CARTESIAN_POINT ( 'NONE',  ( 164.4864175853093400, 274.3409801786992830, 14.76212816031865316 ) ) ;
#90006 = CARTESIAN_POINT ( 'NONE',  ( 88.07864672190808619, 43.84249974723677212, 2.482382391715414194 ) ) ;
#90005 = DIRECTION ( 'NONE',  ( -0.6313854049612632746, -0.7754691937155863135, 0.000000000000000000 ) ) ;
#90007 = DIRECTION ( 'NONE',  ( 0.4999999999999998890, -0.8660254037844385966, 0.000000000000000000 ) ) ;
#90008 = ORIENTED_EDGE ( 'NONE', *, *, #66791, .F. ) ;
#90009 = AXIS2_PLACEMENT_3D ( 'NONE', #56702, #64814, #22922 ) ;
#90010 = ORIENTED_EDGE ( 'NONE', *, *, #28697, .F. ) ;
#90011 = DIRECTION ( 'NONE',  ( -0.6602847420308683990, -0.7510153523339117010, 0.000000000000000000 ) ) ;
#90012 = CARTESIAN_POINT ( 'NONE',  ( -73.66720466879951346, 50.53642055324488780, -10.00000000000000000 ) ) ;
#90013 = LINE ( 'NONE', #82914, #59684 ) ;
#90014 = EDGE_CURVE ( 'NONE', #73177, #83882, #37240, .T. ) ;
#90015 = CARTESIAN_POINT ( 'NONE',  ( 175.6288174815807395, 290.9689912212052718, 2.671585321903346966 ) ) ;
#90016 = VECTOR ( 'NONE', #56327, 1000.000000000000000 ) ;
#90017 = DIRECTION ( 'NONE',  ( 0.4999999999999992784, -0.8660254037844390407, 0.000000000000000000 ) ) ;
#90018 = CARTESIAN_POINT ( 'NONE',  ( 70.57121147093401703, 70.14490917978909579, 6.900396944493546236 ) ) ;
#90019 = LINE ( 'NONE', #43864, #80718 ) ;
#90020 = CARTESIAN_POINT ( 'NONE',  ( 15.00651571324267763, 167.2202760586659736, -5.415160957724236172E-17 ) ) ;
#90021 = CARTESIAN_POINT ( 'NONE',  ( 103.7194723697636221, 236.8149278399160949, -9.188101187500095079 ) ) ;
#90022 = CARTESIAN_POINT ( 'NONE',  ( 43.46773267070898328, 189.2365022471901739, -10.00000000000009237 ) ) ;
#90023 = CARTESIAN_POINT ( 'NONE',  ( 180.2025839467132187, 255.6036467507360896, -2.364551107801861729 ) ) ;
#90024 = CARTESIAN_POINT ( 'NONE',  ( 78.82063543606528810, 55.18920479240949817, 16.06735020332761721 ) ) ;
#90025 = CYLINDRICAL_SURFACE ( 'NONE', #3787, 10.00000000000010658 ) ;
#90026 = CARTESIAN_POINT ( 'NONE',  ( -27.52599651137551007, 146.7012482093458914, 2.297459087388069147E-14 ) ) ;
#90027 = CARTESIAN_POINT ( 'NONE',  ( 180.4684049967686121, 272.9861046151806931, 17.22288380119585938 ) ) ;
#90028 = CARTESIAN_POINT ( 'NONE',  ( 194.2900850603946310, 294.1266965989547657, -15.88613936555681505 ) ) ;
#90029 = EDGE_CURVE ( 'NONE', #31705, #23235, #74218, .T. ) ;
#90030 = CARTESIAN_POINT ( 'NONE',  ( 84.22641972556617418, 50.60946249816755227, 13.78776958506131933 ) ) ;
#90031 = CARTESIAN_POINT ( 'NONE',  ( 196.5203034526607553, 266.3675359752309078, 8.294030003277784502 ) ) ;
#90032 = LINE ( 'NONE', #28689, #54485 ) ;
#90033 = CARTESIAN_POINT ( 'NONE',  ( 55.88622395072203375, 214.6199935810940929, 2.679491924311251605 ) ) ;
#90034 = CARTESIAN_POINT ( 'NONE',  ( 163.4341025207368716, 282.8476932499685859, 9.116081536633066307 ) ) ;
#90035 = EDGE_CURVE ( 'NONE', #46807, #27838, #21106, .T. ) ;
#90036 = CARTESIAN_POINT ( 'NONE',  ( 172.7618964688483914, 263.9129700666785538, -15.45032261957535091 ) ) ;
#90037 = CARTESIAN_POINT ( 'NONE',  ( 78.06346978264959091, 222.0024278399160949, -9.188101187500093303 ) ) ;
#90038 = CARTESIAN_POINT ( 'NONE',  ( 161.8750289368003621, 250.2712207352165592, -13.97436367953006098 ) ) ;
#90039 = CARTESIAN_POINT ( 'NONE',  ( 166.7187202459675746, 278.5591580196478958, -14.78021074750266273 ) ) ;
#90040 = EDGE_CURVE ( 'NONE', #72111, #65613, #71667, .T. ) ;
#90041 = CARTESIAN_POINT ( 'NONE',  ( 58.97569090598253183, 178.8759306620404175, 18.47570218321542868 ) ) ;
#90043 = CARTESIAN_POINT ( 'NONE',  ( 199.8309894386080714, 284.5295686960079706, 18.38040563926018933 ) ) ;
#90042 = CARTESIAN_POINT ( 'NONE',  ( 196.2048238403250764, 290.8102717488927169, 17.53926796892840656 ) ) ;
#90044 = CARTESIAN_POINT ( 'NONE',  ( 75.84977083960791333, 65.49147256048033228, 14.30114164871030979 ) ) ;
#90045 = CARTESIAN_POINT ( 'NONE',  ( 79.96041668311714545, 44.45513045632799276, 11.65481888797057053 ) ) ;
#90046 = AXIS2_PLACEMENT_3D ( 'NONE', #18793, #34478, #88244 ) ;
#90047 = CARTESIAN_POINT ( 'NONE',  ( 40.90268743793880901, 35.56628583063844218, 9.188101187500006262 ) ) ;
#90048 = CARTESIAN_POINT ( 'NONE',  ( 147.5749398328735822, 275.0397016159798227, -4.620786157167191099 ) ) ;
#90049 = FACE_OUTER_BOUND ( 'NONE', #91450, .T. ) ;
#90050 = ORIENTED_EDGE ( 'NONE', *, *, #39996, .F. ) ;
#90051 = CARTESIAN_POINT ( 'NONE',  ( 23.42942861845947178, 22.03085787977762777, 9.188101187500006262 ) ) ;
#90052 = CARTESIAN_POINT ( 'NONE',  ( 16.96546585850747491, 10.76426979415088603, 3.090169943749476733 ) ) ;
#90053 = VECTOR ( 'NONE', #96478, 1000.000000000000000 ) ;
#90054 = CARTESIAN_POINT ( 'NONE',  ( 146.7944005049231180, 276.3916353892955726, -4.243051111306586520 ) ) ;
#90055 = CARTESIAN_POINT ( 'NONE',  ( 63.38631695775107033, 200.7365022471902023, 10.00000000000009948 ) ) ;
#90056 = ADVANCED_FACE ( 'NONE', ( #70120 ), #24531, .T. ) ;
#90057 = EDGE_CURVE ( 'NONE', #65702, #1543, #45720, .T. ) ;
#90058 = VERTEX_POINT ( 'NONE', #64039 ) ;
#90059 = AXIS2_PLACEMENT_3D ( 'NONE', #58639, #57150, #88626 ) ;
#90060 = CARTESIAN_POINT ( 'NONE',  ( 70.54892256928862082, 60.87711404068373611, 14.48624038529373692 ) ) ;
#90061 = CARTESIAN_POINT ( 'NONE',  ( 76.03323602888910671, 65.53324422044475739, -14.33394004605309036 ) ) ;
#90062 = LINE ( 'NONE', #98136, #65496 ) ;
#90063 = DIRECTION ( 'NONE',  ( -0.3374500364938434194, -0.9413434404457831084, 0.000000000000000000 ) ) ;
#90064 = CARTESIAN_POINT ( 'NONE',  ( 131.7301550730730071, 246.8615022471902591, -10.00000000000009592 ) ) ;
#90065 = CARTESIAN_POINT ( 'NONE',  ( 157.1539462478114615, 258.4483758192793061, -17.96006278656275867 ) ) ;
#90066 = ORIENTED_EDGE ( 'NONE', *, *, #6907, .F. ) ;
#90067 = CARTESIAN_POINT ( 'NONE',  ( 191.1702014251404762, 299.1495971912260075, -6.870741027620923091 ) ) ;
#90068 = ORIENTED_EDGE ( 'NONE', *, *, #97350, .T. ) ;
#90069 = CARTESIAN_POINT ( 'NONE',  ( -19.65312891409030271, 93.06504152958497400, -10.00000000000000888 ) ) ;
#90070 = CARTESIAN_POINT ( 'NONE',  ( 83.74409828966761893, 41.70414196250850836, 1.316375386105367973 ) ) ;
#90071 = ORIENTED_EDGE ( 'NONE', *, *, #97462, .F. ) ;
#90072 = DIRECTION ( 'NONE',  ( 0.000000000000000000, 0.000000000000000000, 1.000000000000000000 ) ) ;
#90073 = ORIENTED_EDGE ( 'NONE', *, *, #84079, .T. ) ;
#90074 = CARTESIAN_POINT ( 'NONE',  ( 152.3360070569975449, 270.2436951681156643, -14.78697292633622951 ) ) ;
#90075 = CARTESIAN_POINT ( 'NONE',  ( 158.8212741314356151, 255.5604792119658839, 16.06181463215755656 ) ) ;
#90076 = CARTESIAN_POINT ( 'NONE',  ( 46.85966550219794868, 197.8615022471903444, 4.537668576076728569E-14 ) ) ;
#90077 = CARTESIAN_POINT ( 'NONE',  ( 88.05604604623943032, 44.30204071979397185, -4.408624695025144646 ) ) ;
#90078 = CARTESIAN_POINT ( 'NONE',  ( 201.2949053258274148, 281.9939920013367782, -18.04004790210578335 ) ) ;
#90079 = LINE ( 'NONE', #68219, #7595 ) ;
#90080 = CIRCLE ( 'NONE', #78700, 15.60714546451156970 ) ;
#90081 = AXIS2_PLACEMENT_3D ( 'NONE', #91105, #59651, #99178 ) ;
#90082 = CARTESIAN_POINT ( 'NONE',  ( 76.92488294255016967, 59.33389770090989401, -15.98887582225194315 ) ) ;
#90083 = CARTESIAN_POINT ( 'NONE',  ( 168.0256816748547521, 276.6459939533307306, 15.18346966318006963 ) ) ;
#90084 = CARTESIAN_POINT ( 'NONE',  ( 46.22371820283660782, 112.7232458147606451, 10.00000000000000000 ) ) ;
#90085 = AXIS2_PLACEMENT_3D ( 'NONE', #34070, #69674, #77283 ) ;
#90086 = ORIENTED_EDGE ( 'NONE', *, *, #12481, .T. ) ;
#90087 = EDGE_LOOP ( 'NONE', ( #52158, #73622, #76594, #68607 ) ) ;
#90088 = CARTESIAN_POINT ( 'NONE',  ( 175.1271263694729328, 272.4273639404348728, 17.81557788710851042 ) ) ;
#90090 = CARTESIAN_POINT ( 'NONE',  ( 147.8163551302855296, 274.6215580551378821, -9.286329195885331345 ) ) ;
#90089 = CARTESIAN_POINT ( 'NONE',  ( 174.2275517580468716, 256.7939704606039300, -12.33692674397253519 ) ) ;
#90091 = CARTESIAN_POINT ( 'NONE',  ( 85.35998281785300890, 48.55136375776380930, 12.45655298324007632 ) ) ;
#90092 = DIRECTION ( 'NONE',  ( -1.000000000000000000, 0.000000000000000000, 0.000000000000000000 ) ) ;
#90093 = DIRECTION ( 'NONE',  ( -0.3986482622784278673, -0.9171038997749326738, 0.000000000000000000 ) ) ;
#90094 = CARTESIAN_POINT ( 'NONE',  ( 189.8533352240220893, 301.8113727360248504, -0.2033756396389863053 ) ) ;
#90095 = CARTESIAN_POINT ( 'NONE',  ( 167.9989611498101283, 286.3222843798857866, -4.708603968260846706 ) ) ;
#90096 = CARTESIAN_POINT ( 'NONE',  ( 76.93764771006534886, 63.33963654317832948, -15.47180374620822008 ) ) ;
#90097 = CARTESIAN_POINT ( 'NONE',  ( 78.94581588320816934, 59.75573664777502358, 16.49495449398541425 ) ) ;
#90098 = CARTESIAN_POINT ( 'NONE',  ( 99.66015183740654493, 228.3458772461660544, 9.188101187500095079 ) ) ;
#90099 = ORIENTED_EDGE ( 'NONE', *, *, #48115, .T. ) ;
#90100 = CARTESIAN_POINT ( 'NONE',  ( 22.96769398916923777, 37.53608102203546792, 10.00000000000000000 ) ) ;
#90101 = CARTESIAN_POINT ( 'NONE',  ( 163.8835510476618254, 277.4261113242017132, -14.47671527678674330 ) ) ;
#90102 = ORIENTED_EDGE ( 'NONE', *, *, #86126, .F. ) ;
#90103 = VERTEX_POINT ( 'NONE', #55412 ) ;
#90104 = CARTESIAN_POINT ( 'NONE',  ( 87.09255433220386067, 46.36910785074704933, -8.684712773181464840 ) ) ;
#90105 = CARTESIAN_POINT ( 'NONE',  ( -13.11024591527723437, 6.000000000000000000, -25.00000000000017053 ) ) ;
#90106 = CARTESIAN_POINT ( 'NONE',  ( 195.9713281756800427, 291.2146981034049418, 17.52210387885178022 ) ) ;
#90107 = CARTESIAN_POINT ( 'NONE',  ( 34.45917901495312208, 20.86426979415091765, -3.090169943749474069 ) ) ;
#90108 = CARTESIAN_POINT ( 'NONE',  ( 207.1185389259403564, 270.6189067899559291, -3.459716224787868111 ) ) ;
#90109 = ORIENTED_EDGE ( 'NONE', *, *, #36522, .F. ) ;
#90110 = ORIENTED_EDGE ( 'NONE', *, *, #52910, .F. ) ;
#90111 = CARTESIAN_POINT ( 'NONE',  ( 163.4178923001155681, 247.5989030008181260, -10.38047187240561442 ) ) ;
#90112 = VERTEX_POINT ( 'NONE', #94984 ) ;
#90113 = EDGE_CURVE ( 'NONE', #64789, #63141, #1758, .T. ) ;
#90114 = CARTESIAN_POINT ( 'NONE',  ( 194.6831946052555224, 266.4359861671931640, -8.033020006878627939 ) ) ;
#90115 = CARTESIAN_POINT ( 'NONE',  ( 24.58352123714976045, 26.14441083166261848, 10.00000000000000533 ) ) ;
#90116 = CARTESIAN_POINT ( 'NONE',  ( 66.76298077169236933, 68.73162322739956664, -3.360950600179818615 ) ) ;
#90118 = CARTESIAN_POINT ( 'NONE',  ( 69.40417236955050839, 62.75999532108927781, -13.75910047794655888 ) ) ;
#90117 = CARTESIAN_POINT ( 'NONE',  ( 140.8778087205959650, 242.9548013555409796, -4.594050593750042211 ) ) ;
#90119 = LINE ( 'NONE', #51582, #38317 ) ;
#90120 = EDGE_LOOP ( 'NONE', ( #38852, #65172, #5676, #62594 ) ) ;
#90122 = CARTESIAN_POINT ( 'NONE',  ( 190.1858949294064871, 301.2353624297489887, -5.249932979468886707 ) ) ;
#90121 = VECTOR ( 'NONE', #50649, 1000.000000000000000 ) ;
#90123 = CARTESIAN_POINT ( 'NONE',  ( 82.55658783523657007, 52.19925090473437024, 14.89975261573945353 ) ) ;
#90124 = CARTESIAN_POINT ( 'NONE',  ( 82.37981659293198788, 40.82262905711825596, -3.714377343554210675 ) ) ;
#90125 = CARTESIAN_POINT ( 'NONE',  ( 170.0299321831109580, 248.8356535510476704, -0.2657980000988006131 ) ) ;
#90127 = ADVANCED_FACE ( 'NONE', ( #63533 ), #25029, .F. ) ;
#90126 = CARTESIAN_POINT ( 'NONE',  ( 171.2966090128296059, 286.2859491661027960, 10.55860849112605848 ) ) ;
#90128 = CIRCLE ( 'NONE', #20541, 0.1418229129681522482 ) ;
#90129 = CARTESIAN_POINT ( 'NONE',  ( 72.14978007694548978, 72.25075206688683238, 3.885827817524732275 ) ) ;
#90130 = EDGE_CURVE ( 'NONE', #52772, #90841, #96984, .T. ) ;
#90131 = B_SPLINE_CURVE_WITH_KNOTS ( 'NONE', 3,
 ( #99381, #53259, #60838, #15238 ),
 .UNSPECIFIED., .F., .F.,
 ( 4, 4 ),
 ( 0.01398566235667206108, 0.02029681779994522983 ),
 .UNSPECIFIED. ) ;
#90132 = CARTESIAN_POINT ( 'NONE',  ( 198.7898295845099881, 282.4313312432652197, -17.48232341387986111 ) ) ;
#90133 = CARTESIAN_POINT ( 'NONE',  ( 141.9600801517287607, 252.7677522451418497, 10.00000000000009592 ) ) ;
#90134 = CARTESIAN_POINT ( 'NONE',  ( 79.91228614544331776, 49.76825289431341304, 14.47702846840523883 ) ) ;
#90135 = PLANE ( 'NONE',  #22038 ) ;
#90136 = CARTESIAN_POINT ( 'NONE',  ( 64.74832919946385346, 214.3149278399160949, -9.188101187500095079 ) ) ;
#90137 = DIRECTION ( 'NONE',  ( -0.9659258262890674240, 0.2588190451025240146, -2.299878683274403996E-16 ) ) ;
#90138 = CARTESIAN_POINT ( 'NONE',  ( 197.6456421031980994, 287.3858497455466932, 17.15283754821559015 ) ) ;
#90139 = CARTESIAN_POINT ( 'NONE',  ( 178.3664302925846812, 292.5873534235060447, -5.659256624530483393 ) ) ;
#90140 = CARTESIAN_POINT ( 'NONE',  ( 197.2363158218765307, 288.6427788515542261, -16.66249965469193839 ) ) ;
#90141 = AXIS2_PLACEMENT_3D ( 'NONE', #54310, #61918, #93372 ) ;
#90142 = PLANE ( 'NONE',  #88642 ) ;
#90143 = AXIS2_PLACEMENT_3D ( 'NONE', #47693, #95377, #48726 ) ;
#90144 = CARTESIAN_POINT ( 'NONE',  ( -20.79560377010869487, 95.11135092968059723, 45.19947544897750191 ) ) ;
#90145 = CARTESIAN_POINT ( 'NONE',  ( 16.11573996861870128, 9.708529653044783103, 1.583844403245364907 ) ) ;
#90146 = CARTESIAN_POINT ( 'NONE',  ( 34.80818111321084274, 38.83478043621391151, -8.090169943749479842 ) ) ;
#90147 = PLANE ( 'NONE',  #27191 ) ;
#90148 = CARTESIAN_POINT ( 'NONE',  ( 82.33860354803769610, 54.25881085800082104, 15.62396609633239386 ) ) ;
#90149 = VECTOR ( 'NONE', #10313, 1000.000000000000114 ) ;
#90150 = CARTESIAN_POINT ( 'NONE',  ( 71.93253201618666992, 72.27632922802737880, 3.295383250428983946 ) ) ;
#90151 =( BOUNDED_CURVE ( )  B_SPLINE_CURVE ( 2, ( #54677, #37980, #68891, #99818, #15182, #16202, #39472, #61294, #92257 ),
 .UNSPECIFIED., .F., .T. ) 
 B_SPLINE_CURVE_WITH_KNOTS ( ( 3, 2, 2, 2, 3 ),
 ( 0.5846774193548387455, 0.5860215053763441206, 0.5887096774193548709, 0.5913978494623656212, 0.5927419354838709964 ),
 .UNSPECIFIED. ) 
 CURVE ( )  GEOMETRIC_REPRESENTATION_ITEM ( )  RATIONAL_B_SPLINE_CURVE ( ( 0.9330127018922194093, 0.9330127018922194093, 1.000000000000000000, 0.8660254037844387076, 1.000000000000000000, 0.8660254037844387076, 1.000000000000000000, 0.9330127018922194093, 0.9330127018922194093 ) ) 
 REPRESENTATION_ITEM ( '' )  );
#90152 = EDGE_CURVE ( 'NONE', #23266, #46780, #84544, .T. ) ;
#90153 = CARTESIAN_POINT ( 'NONE',  ( 9.836819166815537585, 185.6744531367911293, 4.594050593750047540 ) ) ;
#90154 = CARTESIAN_POINT ( 'NONE',  ( 49.89075441544358824, 189.6115022471902023, -5.000000000000041744 ) ) ;
#90155 = ORIENTED_EDGE ( 'NONE', *, *, #32793, .T. ) ;
#90156 = ADVANCED_FACE ( 'NONE', ( #90381 ), #98593, .F. ) ;
#90157 = CARTESIAN_POINT ( 'NONE',  ( 181.4044655424706036, 257.2299798609144545, -8.137251057251219777 ) ) ;
#90159 = CARTESIAN_POINT ( 'NONE',  ( 199.4805356068138167, 277.5836055926158110, 15.20881834789949494 ) ) ;
#90158 = B_SPLINE_CURVE_WITH_KNOTS ( 'NONE', 3,
 ( #92725, #77509, #24294, #63784, #85129, #54164, #15678, #47083, #93734, #78003, #8595, #31381 ),
 .UNSPECIFIED., .F., .F.,
 ( 4, 2, 2, 2, 2, 4 ),
 ( 7.936458345170772500E-15, 0.0004846319482286064900, 0.0009692638964492765116, 0.001453895844669946371, 0.001696211818780285745, 0.001938527792890625120 ),
 .UNSPECIFIED. ) ;
#90160 = EDGE_CURVE ( 'NONE', #441, #87238, #95952, .T. ) ;
#90161 = CARTESIAN_POINT ( 'NONE',  ( -47.77400264604317925, 41.56691441172057466, 59.99999999999999289 ) ) ;
#90162 = CARTESIAN_POINT ( 'NONE',  ( 31.84840506572257723, 40.16126292948897003, -6.180339887498951690 ) ) ;
#90163 = CARTESIAN_POINT ( 'NONE',  ( 41.74435586355720318, 207.1589784336661637, -6.496448406907676862E-16 ) ) ;
#90164 = CARTESIAN_POINT ( 'NONE',  ( 200.7583183585857967, 282.9233878912788214, 16.96937806979494212 ) ) ;
#90165 = CARTESIAN_POINT ( 'NONE',  ( 151.3999564459286375, 268.4145785023736153, -15.40574304386609050 ) ) ;
#90166 = CARTESIAN_POINT ( 'NONE',  ( 146.7845206192450007, 276.4087478532630939, 4.443586170796542945 ) ) ;
#90167 = CARTESIAN_POINT ( 'NONE',  ( 5.558032429380089567, 24.18502408145590010, 5.678558825948277544 ) ) ;
#90168 = CARTESIAN_POINT ( 'NONE',  ( 159.8005360292372075, 255.6865549803747797, -16.53985196810166869 ) ) ;
#90169 = CARTESIAN_POINT ( 'NONE',  ( 178.0910872001942664, 292.7183277186941268, 2.601818848788350458 ) ) ;
#90170 = EDGE_CURVE ( 'NONE', #68063, #47151, #90883, .T. ) ;
#90171 = CARTESIAN_POINT ( 'NONE',  ( 176.2039003160224411, 274.8852082280174614, 16.86700035928189934 ) ) ;
#90172 = CARTESIAN_POINT ( 'NONE',  ( 73.05076519265766422, 63.10628205629707566, 14.17491965763273853 ) ) ;
#90173 = DIRECTION ( 'NONE',  ( -0.7082622432767082810, -0.7059494278973847958, 0.000000000000000000 ) ) ;
#90174 = CARTESIAN_POINT ( 'NONE',  ( 93.04999876614748189, 212.9824982072973683, 3.021315404115420679E-15 ) ) ;
#90175 = CARTESIAN_POINT ( 'NONE',  ( 158.2603635358720453, 279.8418491720760812, 9.156985719881870267 ) ) ;
#90176 = CARTESIAN_POINT ( 'NONE',  ( 98.74902094561561228, 234.4865022471902876, 10.00000000000009237 ) ) ;
#90177 = CARTESIAN_POINT ( 'NONE',  ( -2.073866539663252073, 26.60322154129611505, -10.00000000000000000 ) ) ;
#90178 = CARTESIAN_POINT ( 'NONE',  ( 194.7418280156398396, 285.5977080998097790, -17.49241544463354714 ) ) ;
#90179 = EDGE_LOOP ( 'NONE', ( #96886, #91809, #94687, #66475, #24643, #61359 ) ) ;
#90180 = CARTESIAN_POINT ( 'NONE',  ( 50.02589733512838421, 205.8149278399161233, 9.188101187500093303 ) ) ;
#90181 = ORIENTED_EDGE ( 'NONE', *, *, #218, .F. ) ;
#90182 = CARTESIAN_POINT ( 'NONE',  ( 166.5911685708541086, 264.6661525622017734, 17.39495636922530863 ) ) ;
#90183 = CARTESIAN_POINT ( 'NONE',  ( 162.8756881843043516, 250.5380280774768949, 12.81046238701583029 ) ) ;
#90184 = FACE_OUTER_BOUND ( 'NONE', #67881, .T. ) ;
#90185 = ORIENTED_EDGE ( 'NONE', *, *, #6479, .F. ) ;
#90186 = CARTESIAN_POINT ( 'NONE',  ( -43.70040200909111405, 27.32518560721127798, 177.5919119679930134 ) ) ;
#90187 = CARTESIAN_POINT ( 'NONE',  ( 165.0509870607838252, 244.7702999017660375, -2.356357909806504392 ) ) ;
#90188 = LINE ( 'NONE', #21254, #3872 ) ;
#90189 = CARTESIAN_POINT ( 'NONE',  ( 27.20206195878591870, 37.74646525600392266, 2.839279412974139660 ) ) ;
#90190 = CARTESIAN_POINT ( 'NONE',  ( 189.7638670438123540, 264.4198756543991635, 11.07887947409659368 ) ) ;
#90191 = CARTESIAN_POINT ( 'NONE',  ( 86.53588498072504365, 47.33349044025582231, -10.24843137454403674 ) ) ;
#90192 = AXIS2_PLACEMENT_3D ( 'NONE', #93766, #31905, #24324 ) ;
#90193 = CARTESIAN_POINT ( 'NONE',  ( 204.3341445623842674, 276.7298752272635625, 14.23430099947301031 ) ) ;
#90194 = ORIENTED_EDGE ( 'NONE', *, *, #74528, .T. ) ;
#90195 = AXIS2_PLACEMENT_3D ( 'NONE', #87996, #80888, #18544 ) ;
#90196 = CARTESIAN_POINT ( 'NONE',  ( 22.39139443204644664, 24.87878583063842086, -9.188101187500006262 ) ) ;
#90197 = CARTESIAN_POINT ( 'NONE',  ( 22.59275855922847498, 34.81751292744058190, -6.180339887498951690 ) ) ;
#90198 = CARTESIAN_POINT ( 'NONE',  ( 175.0308087517243507, 255.0036995273806610, 7.960308888445424280 ) ) ;
#90199 = CARTESIAN_POINT ( 'NONE',  ( 5.270092192305421364, 185.3967562850347122, -4.648177544792955347E-16 ) ) ;
#90200 = ORIENTED_EDGE ( 'NONE', *, *, #15660, .F. ) ;
#90201 = CYLINDRICAL_SURFACE ( 'NONE', #51408, 17.82106496071139645 ) ;
#90202 = CARTESIAN_POINT ( 'NONE',  ( 167.4230310137581910, 261.5705748858933930, 17.03473681314420674 ) ) ;
#90203 = CARTESIAN_POINT ( 'NONE',  ( 206.8775514429320026, 272.3245652858344670, -9.838455694836268250 ) ) ;
#90204 = B_SPLINE_CURVE_WITH_KNOTS ( 'NONE', 3,
 ( #4727, #70490, #54786, #68988, #53774, #54270, #24398, #55273, #69492, #63396, #99912, #46172, #15277, #38074, #1104, #23381, #596, #93844, #47188, #84736, #30498, #86252, #8698, #7188 ),
 .UNSPECIFIED., .F., .F.,
 ( 4, 2, 2, 2, 2, 2, 2, 2, 2, 2, 2, 4 ),
 ( 0.000000000000000000, 0.1250000000000101308, 0.2500000000000202616, 0.3750000000000304201, 0.4375000000000273670, 0.5000000000000243139, 0.5625000000000213163, 0.6250000000000182077, 0.6875000000000152101, 0.7500000000000121014, 0.8750000000000061062, 1.000000000000000000 ),
 .UNSPECIFIED. ) ;
#90205 = ORIENTED_EDGE ( 'NONE', *, *, #26893, .T. ) ;
#90206 = VECTOR ( 'NONE', #1371, 1000.000000000000000 ) ;
#90208 = CARTESIAN_POINT ( 'NONE',  ( 53.05609693179983566, 212.9860189848785410, -2.679491924311252493 ) ) ;
#90207 = CARTESIAN_POINT ( 'NONE',  ( 161.6127771116929921, 250.7254542206800352, -12.96229604595372464 ) ) ;
#90209 = CARTESIAN_POINT ( 'NONE',  ( 148.9504735598738137, 272.6572073132907690, -11.88406006066344744 ) ) ;
#90210 = ORIENTED_EDGE ( 'NONE', *, *, #89622, .T. ) ;
#90211 = CARTESIAN_POINT ( 'NONE',  ( 159.9770824720811220, 253.5585604421560788, -16.42166711341322483 ) ) ;
#90212 = CARTESIAN_POINT ( 'NONE',  ( 159.6610344727618269, 254.1059716346071866, 15.33388637456589620 ) ) ;
#90213 = LINE ( 'NONE', #51157, #74281 ) ;
#90214 = CARTESIAN_POINT ( 'NONE',  ( 180.7318441963247437, 294.8020894299626775, 5.305383234495177902 ) ) ;
#90215 = B_SPLINE_CURVE_WITH_KNOTS ( 'NONE', 3,
 ( #80458, #64208, #56606, #41902, #26713, #32306, #63208, #71329, #88574, #57093, #96149, #33307, #11029, #1920, #39881, #40389 ),
 .UNSPECIFIED., .F., .F.,
 ( 4, 1, 2, 2, 2, 1, 2, 2, 4 ),
 ( 0.000000000000000000, 0.1249999999999978351, 0.1874999999999980294, 0.2499999999999982236, 0.5000000000000008882, 0.6250000000000035527, 0.6875000000000035527, 0.7500000000000034417, 1.000000000000000000 ),
 .UNSPECIFIED. ) ;
#90216 = ADVANCED_FACE ( 'NONE', ( #82780 ), #29043, .T. ) ;
#90217 = CARTESIAN_POINT ( 'NONE',  ( 123.0967907794404113, 248.0024278399161517, 9.188101187500095079 ) ) ;
#90218 = FACE_OUTER_BOUND ( 'NONE', #76619, .T. ) ;
#90220 = EDGE_LOOP ( 'NONE', ( #80237, #66769, #75785, #79397 ) ) ;
#90219 = B_SPLINE_CURVE_WITH_KNOTS ( 'NONE', 3,
 ( #17071, #1890, #47473, #78397 ),
 .UNSPECIFIED., .F., .F.,
 ( 4, 4 ),
 ( 0.002837985946942163905, 0.008232558240303692806 ),
 .UNSPECIFIED. ) ;
#90222 = CARTESIAN_POINT ( 'NONE',  ( 170.4462059903102045, 263.7743965880969768, 15.83889961394278245 ) ) ;
#90221 = B_SPLINE_CURVE_WITH_KNOTS ( 'NONE', 3,
 ( #71735, #49409, #80356, #79362 ),
 .UNSPECIFIED., .F., .F.,
 ( 4, 4 ),
 ( 0.04736994433111862968, 0.04887120950165270428 ),
 .UNSPECIFIED. ) ;
#90223 = CARTESIAN_POINT ( 'NONE',  ( 203.6925490392534925, 269.5270927311577793, 7.084861529579629114 ) ) ;
#90224 = ORIENTED_EDGE ( 'NONE', *, *, #6151, .F. ) ;
#90225 = AXIS2_PLACEMENT_3D ( 'NONE', #234, #2253, #15925 ) ;
#90226 = CARTESIAN_POINT ( 'NONE',  ( 160.1860556839894230, 253.6250155762421059, 14.83728034098512616 ) ) ;
#90227 = ORIENTED_EDGE ( 'NONE', *, *, #81325, .T. ) ;
#90228 = ORIENTED_EDGE ( 'NONE', *, *, #9839, .F. ) ;
#90229 = CARTESIAN_POINT ( 'NONE',  ( 198.5612432604688991, 286.7288335892616260, 18.30793681285053509 ) ) ;
#90230 = DIRECTION ( 'NONE',  ( -0.000000000000000000, -0.000000000000000000, -1.000000000000000000 ) ) ;
#90231 = CARTESIAN_POINT ( 'NONE',  ( 84.04489159724214176, 210.1423013555409796, -4.594050593750043987 ) ) ;
#90232 = PLANE ( 'NONE',  #9335 ) ;
#90233 = CARTESIAN_POINT ( 'NONE',  ( -75.69529296620470404, 50.68926341652933587, -10.00000000000000000 ) ) ;
#90234 = CARTESIAN_POINT ( 'NONE',  ( -68.29659580619643577, 42.72804590294295224, 177.5919119679930134 ) ) ;
#90235 = CARTESIAN_POINT ( 'NONE',  ( 174.8748641034385969, 278.1051818648194853, 15.47627503780401703 ) ) ;
#90236 = ORIENTED_EDGE ( 'NONE', *, *, #20961, .F. ) ;
#90237 = DIRECTION ( 'NONE',  ( -0.7884491381006394350, 0.6150999566154746745, 0.000000000000000000 ) ) ;
#90238 = AXIS2_PLACEMENT_3D ( 'NONE', #64183, #95132, #46465 ) ;
#90239 = CARTESIAN_POINT ( 'NONE',  ( 201.3505934466285510, 281.8975373467312693, -16.83770227898004279 ) ) ;
#90240 = PLANE ( 'NONE',  #77125 ) ;
#90241 = VERTEX_POINT ( 'NONE', #7717 ) ;
#90242 = DIRECTION ( 'NONE',  ( 0.3984034379158949979, -0.9172102815913020235, 0.000000000000000000 ) ) ;
#90243 = CARTESIAN_POINT ( 'NONE',  ( 163.9684994123220179, 260.5718777511302164, -16.18805203446126129 ) ) ;
#90244 = CARTESIAN_POINT ( 'NONE',  ( 175.0387250457744983, 253.3993311541219953, -7.863511161993287146 ) ) ;
#90245 = EDGE_CURVE ( 'NONE', #96457, #48389, #13346, .T. ) ;
#90246 = CARTESIAN_POINT ( 'NONE',  ( -4.429217378738782962, 26.01694505731172313, 10.00000000000000000 ) ) ;
#90247 = CARTESIAN_POINT ( 'NONE',  ( 206.3505875407052486, 273.2372935382459787, 11.62318091048137880 ) ) ;
#90248 = CARTESIAN_POINT ( 'NONE',  ( 47.74604483422196921, 186.8262482093457777, 3.021315404115420679E-15 ) ) ;
#90249 = EDGE_LOOP ( 'NONE', ( #4749, #73504, #37094, #83860 ) ) ;
#90250 = CARTESIAN_POINT ( 'NONE',  ( 5.561079055679667427, 174.0177522451418781, -10.00000000000009592 ) ) ;
#90251 = CARTESIAN_POINT ( 'NONE',  ( 132.6230702210692414, 253.5024278399160949, -9.188101187500093303 ) ) ;
#90252 = ORIENTED_EDGE ( 'NONE', *, *, #83628, .F. ) ;
#90253 = CARTESIAN_POINT ( 'NONE',  ( -6.040052912301486998, 173.9865022471903160, -10.00000000000009592 ) ) ;
#90254 = CARTESIAN_POINT ( 'NONE',  ( 182.5422306857729495, 258.3868535584214214, 6.448336885657590223 ) ) ;
#90255 = CARTESIAN_POINT ( 'NONE',  ( 155.8781371459173215, 261.8896788882548208, -16.97225651315609696 ) ) ;
#90256 = EDGE_CURVE ( 'NONE', #68464, #85874, #76625, .T. ) ;
#90257 = B_SPLINE_CURVE_WITH_KNOTS ( 'NONE', 3,
 ( #100080, #68655, #99577, #61043 ),
 .UNSPECIFIED., .F., .F.,
 ( 4, 4 ),
 ( 0.007478447391378081031, 0.01563385345884502065 ),
 .UNSPECIFIED. ) ;
#90258 = CARTESIAN_POINT ( 'NONE',  ( 163.8670932201372352, 246.8208641845333773, 5.912697114930636211 ) ) ;
#90259 = EDGE_CURVE ( 'NONE', #81326, #45691, #54796, .T. ) ;
#90260 = DIRECTION ( 'NONE',  ( 0.000000000000000000, 0.000000000000000000, 1.000000000000000000 ) ) ;
#90261 = CARTESIAN_POINT ( 'NONE',  ( 178.7600897929267774, 254.1784503161647706, 4.743017227330367014 ) ) ;
#90262 = VERTEX_POINT ( 'NONE', #53796 ) ;
#90263 = CARTESIAN_POINT ( 'NONE',  ( 76.19782269962939836, 53.23845936708418947, 15.97715781805315949 ) ) ;
#90264 = CARTESIAN_POINT ( 'NONE',  ( -13.51183432020139819, 142.4280072687214442, 0.000000000000000000 ) ) ;
#90265 = CARTESIAN_POINT ( 'NONE',  ( 80.85980389730832485, 50.83193235690592360, 14.69879135629361500 ) ) ;
#90266 = CARTESIAN_POINT ( 'NONE',  ( 202.5213466331059351, 267.6576707457072644, 0.8617883848194879404 ) ) ;
#90267 = CARTESIAN_POINT ( 'NONE',  ( 197.2988255893771736, 265.5460696373069709, 0.8212393553507734145 ) ) ;
#90268 = CARTESIAN_POINT ( 'NONE',  ( 190.1607982559816890, 301.2788311432216233, -4.972636536415983244 ) ) ;
#90269 = CARTESIAN_POINT ( 'NONE',  ( 182.8932037339787939, 280.6271841624986791, 16.75229298683104417 ) ) ;
#90270 = AXIS2_PLACEMENT_3D ( 'NONE', #28410, #27439, #72559 ) ;
#90271 = VECTOR ( 'NONE', #68440, 1000.000000000000227 ) ;
#90272 = CARTESIAN_POINT ( 'NONE',  ( 204.6235849755581455, 276.2285497258825444, -13.59355699282649432 ) ) ;
#90273 = CARTESIAN_POINT ( 'NONE',  ( 192.8438934858417895, 268.2918492126220258, 12.53398668708618402 ) ) ;
#90274 = B_SPLINE_SURFACE_WITH_KNOTS ( 'NONE', 3, 1, ( 
 ( #54510, #93572 ),
 ( #16037, #46938 ),
 ( #77855, #70229 ),
 ( #834, #24141 ),
 ( #7290, #30600 ),
 ( #1590, #71487 ),
 ( #2082, #38171 ),
 ( #94309, #69589 ),
 ( #100015, #79108 ),
 ( #14886, #25363 ),
 ( #6304, #32472 ),
 ( #44784, #61486 ),
 ( #84341, #75720 ),
 ( #92436, #17263 ),
 ( #14409, #76225 ),
 ( #7800, #45775 ),
 ( #46270, #30100 ),
 ( #13903, #45291 ),
 ( #15372, #48167 ),
 ( #63864, #38685 ),
 ( #37195, #60982 ),
 ( #56254, #32959 ),
 ( #69089, #91947 ),
 ( #9691, #94803 ),
 ( #22498, #22983 ),
 ( #40553, #68593 ),
 ( #53389, #77193 ),
 ( #99019, #68097 ),
 ( #24861, #29605 ),
 ( #60478, #91436 ),
 ( #63369, #21997 ),
 ( #52892, #83844 ),
 ( #55736, #53872 ),
 ( #76697, #84834 ) ),
 .UNSPECIFIED., .T., .F., .F.,
 ( 4, 2, 2, 2, 2, 2, 2, 2, 2, 2, 2, 2, 2, 2, 2, 2, 4 ),
 ( 2, 2 ),
 ( 0.000000000000000000, 0.06250000000000000000, 0.1250000000000000000, 0.1875000000000000000, 0.2500000000000000000, 0.3125000000000000000, 0.3750000000000000000, 0.4375000000000000000, 0.5000000000000000000, 0.5625000000000000000, 0.6250000000000000000, 0.6875000000000000000, 0.7500000000000000000, 0.8125000000000000000, 0.8750000000000000000, 0.9375000000000000000, 1.000000000000000000 ),
 ( 0.000000000000000000, 1.000000000000000000 ),
 .UNSPECIFIED. ) ;
#90275 = CARTESIAN_POINT ( 'NONE',  ( 13.14225634397871367, 29.36126292948895156, 6.180339887498949913 ) ) ;
#90276 = CARTESIAN_POINT ( 'NONE',  ( 149.0802055316563326, 272.4325049467973940, 12.84384348890831085 ) ) ;
#90277 = CARTESIAN_POINT ( 'NONE',  ( 93.96857342517719758, 10.00000000000001243, 0.000000000000000000 ) ) ;
#90278 = CARTESIAN_POINT ( 'NONE',  ( 22.83062064355499032, 21.38052372038641380, 10.00000000000000533 ) ) ;
#90279 = CARTESIAN_POINT ( 'NONE',  ( 159.2077906806335932, 254.8910129107889588, 16.14624949541834553 ) ) ;
#90280 = CARTESIAN_POINT ( 'NONE',  ( 207.2031141856176930, 271.7606740744515719, 5.319265574913023542 ) ) ;
#90281 = VECTOR ( 'NONE', #85807, 1000.000000000000227 ) ;
#90282 = ADVANCED_FACE ( 'NONE', ( #83259 ), #63674, .T. ) ;
#90283 = CARTESIAN_POINT ( 'NONE',  ( 126.3716228836088362, 253.7677522451419065, -5.000000000000047962 ) ) ;
#90284 = CARTESIAN_POINT ( 'NONE',  ( 182.1760933249994139, 278.4465760882033578, 17.66821597207981398 ) ) ;
#90285 = VERTEX_POINT ( 'NONE', #85787 ) ;
#90286 = VECTOR ( 'NONE', #21751, 1000.000000000000000 ) ;
#90287 = CARTESIAN_POINT ( 'NONE',  ( 66.52985639494735892, 67.77629683309557151, -6.953963155367802074 ) ) ;
#90288 = CARTESIAN_POINT ( 'NONE',  ( 150.7691137448031213, 269.5072301123068428, -15.63821625702598084 ) ) ;
#90289 = CARTESIAN_POINT ( 'NONE',  ( 18.33521408509785644, 172.2048013555409796, 4.594050593750051981 ) ) ;
#90290 = CARTESIAN_POINT ( 'NONE',  ( 178.6505746094053961, 259.2109398937957963, -10.36763312313177110 ) ) ;
#90291 = CARTESIAN_POINT ( 'NONE',  ( 24.00897855452593888, 29.56454794089042082, 10.00000000000000355 ) ) ;
#90292 = CARTESIAN_POINT ( 'NONE',  ( 85.66514145605599140, 48.89467697360638709, 12.11710310453397099 ) ) ;
#90293 = AXIS2_PLACEMENT_3D ( 'NONE', #70485, #96328, #35482 ) ;
#90294 = CARTESIAN_POINT ( 'NONE',  ( 205.3708847852691406, 274.9341884869767227, -13.70973585089674174 ) ) ;
#90295 = CARTESIAN_POINT ( 'NONE',  ( 85.51062282364698319, 48.96702101389664108, -12.23238128493630583 ) ) ;
#90296 = CARTESIAN_POINT ( 'NONE',  ( 73.85266254684545117, 55.03492225557787521, -16.12802322512867548 ) ) ;
#90297 = CARTESIAN_POINT ( 'NONE',  ( 167.5258221105458745, 256.6147765433380528, 14.95940915016304551 ) ) ;
#90298 = ADVANCED_FACE ( 'NONE', ( #16318 ), #1127, .T. ) ;
#90299 = CARTESIAN_POINT ( 'NONE',  ( 75.48012123268173923, 53.33211347945791658, 16.49774674168797617 ) ) ;
#90300 = CARTESIAN_POINT ( 'NONE',  ( 150.9462701294987141, 269.2003862531290110, 13.98983978186602073 ) ) ;
#90301 = CARTESIAN_POINT ( 'NONE',  ( 51.11762373747147592, 206.9865022471902876, -10.00000000000009415 ) ) ;
#90302 = CARTESIAN_POINT ( 'NONE',  ( 185.0483992081186670, 294.1025820707552043, 9.705500343873069369 ) ) ;
#90303 = VECTOR ( 'NONE', #29312, 1000.000000000000227 ) ;
#90304 = CARTESIAN_POINT ( 'NONE',  ( 147.8465295590381743, 274.5692944114487091, 9.322947948439978205 ) ) ;
#90305 = CARTESIAN_POINT ( 'NONE',  ( 26.56245542105003210, 176.9548013555409796, -4.594050593750042211 ) ) ;
#90306 = CARTESIAN_POINT ( 'NONE',  ( 72.82956929615318131, 70.88121797294114401, -7.877017184599606203 ) ) ;
#90307 = CARTESIAN_POINT ( 'NONE',  ( 192.2943420783192323, 297.5834248427583475, 12.53393473147773562 ) ) ;
#90308 = CARTESIAN_POINT ( 'NONE',  ( 40.31210609084968866, 28.98920272979929535, 7.433330006724137462 ) ) ;
#90309 = FACE_OUTER_BOUND ( 'NONE', #43436, .T. ) ;
#90310 = CARTESIAN_POINT ( 'NONE',  ( 181.8200170576783705, 278.0724415165672099, 16.45581006755550746 ) ) ;
#90311 = CARTESIAN_POINT ( 'NONE',  ( 185.5878794376151575, 266.6731272799339649, 13.19771459954216652 ) ) ;
#90312 = CARTESIAN_POINT ( 'NONE',  ( -55.56624327025929944, 44.99999999999998579, -10.00000000000000000 ) ) ;
#90313 = CARTESIAN_POINT ( 'NONE',  ( 163.4142949803911620, 281.2077642141172760, 8.863657438064944216 ) ) ;
#90314 = EDGE_CURVE ( 'NONE', #31643, #83325, #55297, .T. ) ;
#90315 = CARTESIAN_POINT ( 'NONE',  ( 15.13723537722347778, 17.24335787977762280, -9.188101187500008038 ) ) ;
#90316 = CARTESIAN_POINT ( 'NONE',  ( 189.4199209167946663, 300.3895034224956930, 3.306026617473488027 ) ) ;
#90317 = CARTESIAN_POINT ( 'NONE',  ( 82.78605335669568888, 53.79744310428999654, 15.41452286606368283 ) ) ;
#90318 = CARTESIAN_POINT ( 'NONE',  ( 189.2845499996045930, 259.5340837477176024, -0.8149847707460528001 ) ) ;
#90319 = CARTESIAN_POINT ( 'NONE',  ( 155.5204415533959548, 261.2776889444089647, 17.19127227448963424 ) ) ;
#90320 = ORIENTED_EDGE ( 'NONE', *, *, #2, .F. ) ;
#90321 = CARTESIAN_POINT ( 'NONE',  ( 181.5350816980370325, 289.2740427057465809, 12.64428308550723479 ) ) ;
#90322 = CARTESIAN_POINT ( 'NONE',  ( 108.3474691708931630, 233.3615022471902591, -10.00000000000009592 ) ) ;
#90323 = FACE_OUTER_BOUND ( 'NONE', #70095, .T. ) ;
#90324 = ORIENTED_EDGE ( 'NONE', *, *, #71424, .T. ) ;
#90325 = CARTESIAN_POINT ( 'NONE',  ( 196.0896742213610082, 290.2260983427040060, -16.35227306082677146 ) ) ;
#90326 = CARTESIAN_POINT ( 'NONE',  ( 67.56996644992010204, 69.57760016826152594, 0.9047167175399849492 ) ) ;
#90327 = CARTESIAN_POINT ( 'NONE',  ( 66.69731441546797157, 68.33447113151889596, 4.530513419427100175 ) ) ;
#90328 = CARTESIAN_POINT ( 'NONE',  ( 203.4682009197399566, 278.2297336128146412, -15.36039508894693206 ) ) ;
#90329 = VERTEX_POINT ( 'NONE', #18832 ) ;
#90330 = VERTEX_POINT ( 'NONE', #25936 ) ;
#90332 = CARTESIAN_POINT ( 'NONE',  ( 164.4936379324916516, 245.7356569095223051, 6.719479797016231437 ) ) ;
#90331 = DIRECTION ( 'NONE',  ( 1.000000000000000000, -1.003165804393444873E-13, 0.000000000000000000 ) ) ;
#90333 = CARTESIAN_POINT ( 'NONE',  ( 192.8132846206021611, 296.6845899933152850, 11.53748932578252351 ) ) ;
#90334 = VERTEX_POINT ( 'NONE', #51198 ) ;
#90335 = CARTESIAN_POINT ( 'NONE',  ( 190.8001679306945277, 300.1714103817999444, 7.815449226872675403 ) ) ;
#90336 = AXIS2_PLACEMENT_3D ( 'NONE', #96401, #87838, #18883 ) ;
#90337 = CARTESIAN_POINT ( 'NONE',  ( 80.42785451945398734, 57.51445601405281138, -16.58998511169260937 ) ) ;
#90338 = CARTESIAN_POINT ( 'NONE',  ( 174.5060864132779557, 262.3161859066883039, 14.40012180740343872 ) ) ;
#90339 = EDGE_LOOP ( 'NONE', ( #17409, #91823, #24728, #18433 ) ) ;
#90340 = CARTESIAN_POINT ( 'NONE',  ( 87.69605122943771391, 45.27158203283479310, -6.304490442501953673 ) ) ;
#90341 = AXIS2_PLACEMENT_3D ( 'NONE', #24925, #72044, #93364 ) ;
#90342 = ORIENTED_EDGE ( 'NONE', *, *, #34513, .F. ) ;
#90343 = CARTESIAN_POINT ( 'NONE',  ( 164.9617201910520237, 244.9249146555742414, 2.745022583679548767 ) ) ;
#90344 = AXIS2_PLACEMENT_3D ( 'NONE', #54655, #47072, #8583 ) ;
#90345 = CARTESIAN_POINT ( 'NONE',  ( 39.80235952159635815, 84.99999999999998579, 59.99999999999999289 ) ) ;
#90346 = VERTEX_POINT ( 'NONE', #56811 ) ;
#90347 = DIRECTION ( 'NONE',  ( 1.000000000000000000, 0.000000000000000000, 0.000000000000000000 ) ) ;
#90348 = CARTESIAN_POINT ( 'NONE',  ( 172.3812282607925397, 263.7635464947321111, -15.48109893273863236 ) ) ;
#90349 = VERTEX_POINT ( 'NONE', #26429 ) ;
#90350 = CARTESIAN_POINT ( 'NONE',  ( 83.32840393668934098, 230.4637435831425023, 2.679491924311251605 ) ) ;
#90351 = CARTESIAN_POINT ( 'NONE',  ( 147.1034852426517148, 275.8562849197056153, -3.648177088342072327 ) ) ;
#90352 = ORIENTED_EDGE ( 'NONE', *, *, #36752, .T. ) ;
#90353 = EDGE_LOOP ( 'NONE', ( #23567, #65849, #7911, #65654 ) ) ;
#90354 = VECTOR ( 'NONE', #96253, 1000.000000000000000 ) ;
#90355 = CARTESIAN_POINT ( 'NONE',  ( 73.66300103671132149, 69.67160076658454670, 9.549075820628328160 ) ) ;
#90356 = LINE ( 'NONE', #58883, #13752 ) ;
#90357 = CARTESIAN_POINT ( 'NONE',  ( 188.6257896815903621, 298.5631806337704006, -4.505592037249916970 ) ) ;
#90358 = CARTESIAN_POINT ( 'NONE',  ( 27.80861752939100029, 41.25950758903265836, 10.00000000000000000 ) ) ;
#90359 = CARTESIAN_POINT ( 'NONE',  ( 153.4619471835925708, 264.8431057800031567, 16.95044998314351758 ) ) ;
#90360 = CARTESIAN_POINT ( 'NONE',  ( 191.8308278875103099, 298.3862549712684995, 9.280152759256424133 ) ) ;
#90361 = CARTESIAN_POINT ( 'NONE',  ( 147.2999496562918296, 275.5159985734018164, -0.1418322875769767455 ) ) ;
#90362 = B_SPLINE_CURVE_WITH_KNOTS ( 'NONE', 3,
 ( #32629, #17427, #1750, #723 ),
 .UNSPECIFIED., .F., .F.,
 ( 4, 4 ),
 ( 0.003952496786374898145, 0.009435233971604372813 ),
 .UNSPECIFIED. ) ;
#90363 = ORIENTED_EDGE ( 'NONE', *, *, #71939, .T. ) ;
#90364 = CARTESIAN_POINT ( 'NONE',  ( 73.30040493051414785, 58.25693415237071804, -15.77479770186053898 ) ) ;
#90365 = CARTESIAN_POINT ( 'NONE',  ( 31.25301259707286050, 39.81751292744058901, -6.180339887498951690 ) ) ;
#90367 = CARTESIAN_POINT ( 'NONE',  ( 206.5508451493652444, 272.8904371854448527, 11.05407534521577695 ) ) ;
#90366 = CARTESIAN_POINT ( 'NONE',  ( 148.9504735598738137, 272.6572073132907690, -11.88406006066344744 ) ) ;
#90369 = EDGE_LOOP ( 'NONE', ( #92707, #64673, #70342, #10870 ) ) ;
#90368 = CARTESIAN_POINT ( 'NONE',  ( 67.22111511317197596, 66.59540578004832412, 8.496167826198702144 ) ) ;
#90370 = CARTESIAN_POINT ( 'NONE',  ( 169.0014201196099748, 286.7460675995289989, 4.080809884116825437 ) ) ;
#90371 = B_SPLINE_CURVE_WITH_KNOTS ( 'NONE', 3,
 ( #1034, #92760, #62305, #8136 ),
 .UNSPECIFIED., .F., .F.,
 ( 4, 4 ),
 ( 0.009425792323206581835, 0.01476071270588196274 ),
 .UNSPECIFIED. ) ;
#90372 = CARTESIAN_POINT ( 'NONE',  ( 176.5750811079351763, 290.0661888821730372, -9.631901365267058424 ) ) ;
#90373 = ORIENTED_EDGE ( 'NONE', *, *, #12801, .F. ) ;
#90374 = CARTESIAN_POINT ( 'NONE',  ( 149.3583220794619422, 271.9507929555723535, -11.49772206859406332 ) ) ;
#90375 = CARTESIAN_POINT ( 'NONE',  ( 77.89973555931712212, 53.60260371492954334, -15.91514005743381155 ) ) ;
#90376 = CARTESIAN_POINT ( 'NONE',  ( 202.9752796556865064, 278.6631792541300001, 14.99201349560580532 ) ) ;
#90377 = CARTESIAN_POINT ( 'NONE',  ( 79.53682116969469007, 45.82036653282950311, 12.91785852832784265 ) ) ;
#90378 = EDGE_CURVE ( 'NONE', #78755, #47892, #59640, .T. ) ;
#90379 = CARTESIAN_POINT ( 'NONE',  ( 198.7177703306137460, 286.4577207510109247, -18.34263739182689790 ) ) ;
#90380 = EDGE_CURVE ( 'NONE', #53811, #45557, #94896, .T. ) ;
#90381 = FACE_OUTER_BOUND ( 'NONE', #42110, .T. ) ;
#90382 = ORIENTED_EDGE ( 'NONE', *, *, #97710, .F. ) ;
#90383 = CARTESIAN_POINT ( 'NONE',  ( 170.3022864262811140, 255.3823714536916327, -11.62275972992479645 ) ) ;
#90384 = CARTESIAN_POINT ( 'NONE',  ( 83.89296645697339727, 43.48164506579582422, 7.866080993069674676 ) ) ;
#90385 = AXIS2_PLACEMENT_3D ( 'NONE', #32717, #1835, #46919 ) ;
#90386 = EDGE_CURVE ( 'NONE', #26065, #51970, #11245, .T. ) ;
#90387 = CARTESIAN_POINT ( 'NONE',  ( 207.6727254509676186, 270.9472835030587703, 7.315149605389819953 ) ) ;
#90388 = EDGE_CURVE ( 'NONE', #65702, #39606, #66902, .T. ) ;
#90389 = CARTESIAN_POINT ( 'NONE',  ( 36.66582480827081980, 178.6427522451417644, 1.119607411625061291E-15 ) ) ;
#90390 = CARTESIAN_POINT ( 'NONE',  ( 113.7873647845227083, 230.3768266524159856, -9.188101187500093303 ) ) ;
#90391 = CARTESIAN_POINT ( 'NONE',  ( 151.1699610800269511, 268.8129421616204695, -14.28929860221299286 ) ) ;
#90392 = CARTESIAN_POINT ( 'NONE',  ( 167.9211909854000169, 281.9652706170933243, -10.87640062917275507 ) ) ;
#90393 = CARTESIAN_POINT ( 'NONE',  ( 190.7405042774493324, 298.2747508605859821, 9.591131971744578877 ) ) ;
#90394 = LINE ( 'NONE', #59923, #38496 ) ;
#90395 = CARTESIAN_POINT ( 'NONE',  ( 35.05980905203730913, 200.2369531367911293, -4.594050593750048428 ) ) ;
#90396 = VECTOR ( 'NONE', #66918, 1000.000000000000000 ) ;
#90397 = CARTESIAN_POINT ( 'NONE',  ( 37.67364948790085322, 52.89489741671173562, 177.5919119679930134 ) ) ;
#90398 = ORIENTED_EDGE ( 'NONE', *, *, #48708, .F. ) ;
#90399 = DIRECTION ( 'NONE',  ( 0.4999999999999992784, -0.8660254037844390407, 0.000000000000000000 ) ) ;
#90400 = CARTESIAN_POINT ( 'NONE',  ( 181.3415465419150792, 267.7713915340963240, 14.97876564237039254 ) ) ;
#90401 = CARTESIAN_POINT ( 'NONE',  ( 88.22316733864592209, 44.26875609612613971, 2.029272769359137474 ) ) ;
#90402 = CARTESIAN_POINT ( 'NONE',  ( 82.07381172419997029, 41.42616999410403622, -5.934122665073511271 ) ) ;
#90403 = CARTESIAN_POINT ( 'NONE',  ( 14.09675671201943992, 9.108019796199272378, 3.090169943749476733 ) ) ;
#90404 = CARTESIAN_POINT ( 'NONE',  ( 179.4042561553460757, 287.8475187006056331, -12.55830537432352401 ) ) ;
#90405 = CARTESIAN_POINT ( 'NONE',  ( 164.2365267202495431, 249.9047677799958365, 11.29870037847212672 ) ) ;
#90406 = CARTESIAN_POINT ( 'NONE',  ( 95.19470834736904408, 235.7677522451419065, -5.000000000000047962 ) ) ;
#90407 = AXIS2_PLACEMENT_3D ( 'NONE', #87936, #88940, #19500 ) ;
#90408 = ORIENTED_EDGE ( 'NONE', *, *, #3460, .F. ) ;
#90409 = B_SPLINE_CURVE_WITH_KNOTS ( 'NONE', 3,
 ( #13379, #44248, #7753, #45249, #75184, #52849, #83799, #14363, #91900, #76185, #22942, #6760, #68549, #53831, #69551, #5758, #36648, #83296, #156, #69045, #61931, #22455, #67554, #53350, #59943, #92883, #98487, #98977, #37638, #61443, #99474, #76657, #51873, #13860, #84791, #7245, #30050, #82811, #44739, #6258, #29561, #37155, #77150, #29078, #91391, #38127, #15332, #93897, #55820, #47245 ),
 .UNSPECIFIED., .F., .F.,
 ( 4, 2, 2, 2, 2, 2, 2, 2, 2, 2, 2, 2, 2, 2, 2, 2, 2, 2, 2, 2, 2, 2, 2, 2, 4 ),
 ( 0.0006309157225252743240, 0.0008450400362799124782, 0.001059164350034550849, 0.001166226506911871011, 0.001273288663789191172, 0.001380350820666511550, 0.001487412977543831711, 0.001701537291298473335, 0.001915661605053114959, 0.002343910232562398423, 0.003200407487580905069, 0.004056904742599411716, 0.004913401997617919230, 0.005341650625127209416, 0.005555774938881930837, 0.005662837095759329711, 0.005716368174197957591, 0.005769899252636586338, 0.005876961409513709392, 0.005984023566390833312, 0.006198147880145075950, 0.006412272193899318587, 0.006626396507653561224, 0.007054645135162053438, 0.007482893762670545651 ),
 .UNSPECIFIED. ) ;
#90410 = CARTESIAN_POINT ( 'NONE',  ( 194.9180876943665055, 266.4584948954776564, -7.740551621638591229 ) ) ;
#90411 = AXIS2_PLACEMENT_3D ( 'NONE', #64347, #95311, #85188 ) ;
#90412 = CARTESIAN_POINT ( 'NONE',  ( 155.5784045870823036, 279.7726721642641792, -1.593457801340965929 ) ) ;
#90413 = CARTESIAN_POINT ( 'NONE',  ( -19.65312891409030271, 93.06504152958497400, 60.00000000000000000 ) ) ;
#90414 = B_SPLINE_CURVE_WITH_KNOTS ( 'NONE', 3,
 ( #65966, #87848, #50265, #35059, #81218, #18388, #88337, #97390, #12281, #42649, #18894, #10786, #49773, #74085, #4674, #97881, #66465, #42162, #73098, #74595, #27958, #51250, #66952, #82218, #12790, #3208, #36049, #34093, #95926, #80729, #11794, #11304, #3690, #73581, #34569, #4163, #65470, #45633, #84691, #69447, #76561, #7649, #7142, #38029, #67454, #84206, #30450, #14752 ),
 .UNSPECIFIED., .F., .F.,
 ( 4, 2, 2, 2, 2, 2, 2, 2, 2, 2, 2, 2, 2, 2, 2, 2, 2, 2, 2, 2, 2, 2, 2, 4 ),
 ( 0.0001582601720098061036, 0.0006504983501745226302, 0.001142736528339238994, 0.001388855617421661144, 0.001634974706504083077, 0.001758034251045258265, 0.001881093795586433453, 0.002004153340127608641, 0.002127212884668783829, 0.002373331973751017978, 0.002619451062833252561, 0.003111689240997658843, 0.004096165597326570720, 0.005080641953655483031, 0.005572880131819939187, 0.005818999220902246194, 0.006065118309984554069, 0.006126648082255130821, 0.006188177854525706706, 0.006311237399066868016, 0.006557356488149255688, 0.007049594666314037104, 0.007541832844478820255, 0.008034071022643600804 ),
 .UNSPECIFIED. ) ;
#90415 = AXIS2_PLACEMENT_3D ( 'NONE', #72895, #39934, #71382 ) ;
#90416 = CARTESIAN_POINT ( 'NONE',  ( 22.31343150979137846, 177.5643266524160424, 9.188101187500095079 ) ) ;
#90417 = CIRCLE ( 'NONE', #3043, 45.00000000000000000 ) ;
#90418 = CARTESIAN_POINT ( 'NONE',  ( 6.499975723459110455, 22.49103043416547010, -8.090169943749479842 ) ) ;
#90419 = CARTESIAN_POINT ( 'NONE',  ( 79.27712787825650764, 45.82676469203064329, -12.41914995154098911 ) ) ;
#90420 = DIRECTION ( 'NONE',  ( 0.000000000000000000, 0.000000000000000000, 1.000000000000000000 ) ) ;
#90421 = CARTESIAN_POINT ( 'NONE',  ( 66.71234638643888104, 68.39628657080208995, -4.370994838407439964 ) ) ;
#90422 = CARTESIAN_POINT ( 'NONE',  ( 57.11665387649598813, 203.7833772461660828, -9.188101187500095079 ) ) ;
#90423 = CARTESIAN_POINT ( 'NONE',  ( 198.7134558283731280, 282.8386145195935910, 17.66748989068429054 ) ) ;
#90424 = DIRECTION ( 'NONE',  ( -0.9659258262890667579, 0.2588190451025264016, -1.433922627038915147E-16 ) ) ;
#90425 = CARTESIAN_POINT ( 'NONE',  ( 70.20553746537656536, 69.89474460070350403, 5.933681650480220782 ) ) ;
#90426 = CARTESIAN_POINT ( 'NONE',  ( 66.38800753050692549, 68.05348521546564200, -4.839280302337260586 ) ) ;
#90427 = ORIENTED_EDGE ( 'NONE', *, *, #40222, .T. ) ;
#90428 = AXIS2_PLACEMENT_3D ( 'NONE', #52291, #44676, #15780 ) ;
#90429 = CARTESIAN_POINT ( 'NONE',  ( 12.29081813446910409, 191.2365022471903444, 2.944929066748280225E-16 ) ) ;
#90430 = CARTESIAN_POINT ( 'NONE',  ( -54.21831688459418785, 33.63902229265146104, 10.00000000000000000 ) ) ;
#90431 = CARTESIAN_POINT ( 'NONE',  ( 140.4172988551291610, 258.0024278399160949, -9.188101187500093303 ) ) ;
#90432 = CARTESIAN_POINT ( 'NONE',  ( 26.18025557360336464, 27.06628583063842797, -9.188101187500006262 ) ) ;
#90433 = CARTESIAN_POINT ( 'NONE',  ( 207.5610651195029845, 271.1406848703456944, -7.832979109022246256 ) ) ;
#90434 = LINE ( 'NONE', #44758, #17719 ) ;
#90435 = CARTESIAN_POINT ( 'NONE',  ( 47.78135487164287554, 106.4364430393875267, -10.00000000000000000 ) ) ;
#90437 = CARTESIAN_POINT ( 'NONE',  ( 74.92881689719639837, 67.14644430943499742, 12.99852016367276875 ) ) ;
#90436 = FACE_OUTER_BOUND ( 'NONE', #14574, .T. ) ;
#90438 = CARTESIAN_POINT ( 'NONE',  ( 171.7154418923348942, 259.3365693118849435, -15.26938553599716641 ) ) ;
#90439 = VERTEX_POINT ( 'NONE', #97831 ) ;
#90440 = CARTESIAN_POINT ( 'NONE',  ( 191.5544531425776427, 298.8649500714207647, 8.366689293739112188 ) ) ;
#90441 = CARTESIAN_POINT ( 'NONE',  ( -57.77801984846012573, 31.16909059156539996, -10.00000000000000178 ) ) ;
#90442 = EDGE_CURVE ( 'NONE', #63506, #72984, #64432, .T. ) ;
#90443 = CARTESIAN_POINT ( 'NONE',  ( 151.3638679738639610, 268.9271637915409769, -14.29068541092436462 ) ) ;
#90444 = CARTESIAN_POINT ( 'NONE',  ( 170.0766860910346168, 266.2494559554864395, -17.52215767842801242 ) ) ;
#90445 = DIRECTION ( 'NONE',  ( -0.8660254037844387076, -0.4999999999999998890, -0.000000000000000000 ) ) ;
#90447 = ORIENTED_EDGE ( 'NONE', *, *, #92662, .T. ) ;
#90446 = VECTOR ( 'NONE', #28306, 1000.000000000000114 ) ;
#90448 = CARTESIAN_POINT ( 'NONE',  ( 68.43551180206651452, 65.84368784619988446, 10.25479611292870885 ) ) ;
#90449 = CARTESIAN_POINT ( 'NONE',  ( 168.4165475187242862, 282.2027335547327311, -10.92266496736840686 ) ) ;
#90450 = CARTESIAN_POINT ( 'NONE',  ( 71.94311743993219466, 72.25799473628046599, 0.6149828437083229016 ) ) ;
#90451 = DIRECTION ( 'NONE',  ( 0.000000000000000000, -0.000000000000000000, 1.000000000000000000 ) ) ;
#90452 = DIRECTION ( 'NONE',  ( -0.8660254037844387076, -0.4999999999999998890, -0.000000000000000000 ) ) ;
#90453 = DIRECTION ( 'NONE',  ( -0.8660254037844387076, -0.4999999999999998890, -0.000000000000000000 ) ) ;
#90454 = CARTESIAN_POINT ( 'NONE',  ( 69.20334762877976686, 70.41346677573686463, 2.281924207914373781 ) ) ;
#90455 = CARTESIAN_POINT ( 'NONE',  ( 150.8074912838825128, 278.0825890836262602, -0.0002049239830752711748 ) ) ;
#90456 = LINE ( 'NONE', #36187, #93730 ) ;
#90457 = LINE ( 'NONE', #3818, #51907 ) ;
#90458 = CARTESIAN_POINT ( 'NONE',  ( 16.97222724706318076, 11.92755873383624632, 6.180339887498953466 ) ) ;
#90459 = CARTESIAN_POINT ( 'NONE',  ( 147.7840666256145425, 276.6774833857293174, 0.9737628777943441172 ) ) ;
#90460 = ORIENTED_EDGE ( 'NONE', *, *, #78472, .F. ) ;
#90461 = CARTESIAN_POINT ( 'NONE',  ( 163.3838389430857774, 253.5546336541830783, 14.73126852126472386 ) ) ;
#90462 = ADVANCED_FACE ( 'NONE', ( #51724 ), #82667, .T. ) ;
#90463 = LINE ( 'NONE', #83340, #38573 ) ;
#90464 = CARTESIAN_POINT ( 'NONE',  ( 159.1138359885003126, 263.7651727890922757, -17.14152579247067720 ) ) ;
#90465 = VERTEX_POINT ( 'NONE', #1744 ) ;
#90466 = CARTESIAN_POINT ( 'NONE',  ( 147.2405539530007559, 275.6188749492528132, 0.4306668706573002492 ) ) ;
#90467 = CARTESIAN_POINT ( 'NONE',  ( 204.6823371430232896, 272.9704135290961062, -9.754921121218281144 ) ) ;
#90468 = CARTESIAN_POINT ( 'NONE',  ( 163.7010375032499212, 247.1084811230698506, 6.649922295230481950 ) ) ;
#90469 = CARTESIAN_POINT ( 'NONE',  ( 13.43400709863221820, 31.08381733381234469, 10.00000000000000000 ) ) ;
#90470 = ORIENTED_EDGE ( 'NONE', *, *, #50966, .T. ) ;
#90471 = CARTESIAN_POINT ( 'NONE',  ( 94.00418374076319594, 215.8923013555410080, 4.594050593750050204 ) ) ;
#90472 = CARTESIAN_POINT ( 'NONE',  ( 169.5608527833963421, 251.6396950762901952, -9.960993533446050208 ) ) ;
#90473 = CARTESIAN_POINT ( 'NONE',  ( 73.09452573934707686, 69.60050248057373778, -9.839270276345128963 ) ) ;
#90474 = CARTESIAN_POINT ( 'NONE',  ( 181.3013930180519253, 271.1797949997417732, -15.98288922033975012 ) ) ;
#90475 = CARTESIAN_POINT ( 'NONE',  ( 181.9690984642188312, 257.1582083484186114, -6.131635832278763409 ) ) ;
#90476 = EDGE_LOOP ( 'NONE', ( #74396, #99379, #82753, #55612 ) ) ;
#90477 = ORIENTED_EDGE ( 'NONE', *, *, #52628, .F. ) ;
#90478 = CARTESIAN_POINT ( 'NONE',  ( -8.728340106763567974, 165.7677522451418781, 10.00000000000009592 ) ) ;
#90479 = ORIENTED_EDGE ( 'NONE', *, *, #99668, .F. ) ;
#90480 = CARTESIAN_POINT ( 'NONE',  ( -45.06544009570465903, 71.64693071047494755, -10.00000000000000000 ) ) ;
#90481 = ORIENTED_EDGE ( 'NONE', *, *, #80206, .F. ) ;
#90482 = CARTESIAN_POINT ( 'NONE',  ( -78.57153713424663977, 57.64153020465174393, 10.00000000000000000 ) ) ;
#90483 = ORIENTED_EDGE ( 'NONE', *, *, #57233, .T. ) ;
#90484 = CARTESIAN_POINT ( 'NONE',  ( -27.77457187288641904, 24.79904599702367562, -10.00000000000000000 ) ) ;
#90485 = CARTESIAN_POINT ( 'NONE',  ( 82.63495489645998759, 40.85464596424811390, 3.248838194811724200 ) ) ;
#90486 = CIRCLE ( 'NONE', #7926, 70.00000000000001421 ) ;
#90487 = CARTESIAN_POINT ( 'NONE',  ( 153.0790963368640689, 265.5062228982576471, -17.74594954892339160 ) ) ;
#90488 = FACE_OUTER_BOUND ( 'NONE', #89730, .T. ) ;
#90490 = CARTESIAN_POINT ( 'NONE',  ( 71.06913592625164711, 68.39894819183987806, -9.182066607298049021 ) ) ;
#90489 = VECTOR ( 'NONE', #95455, 1000.000000000000114 ) ;
#90491 = CARTESIAN_POINT ( 'NONE',  ( 168.3064590912703693, 267.1730826594816790, -17.42781320323403804 ) ) ;
#90492 = ORIENTED_EDGE ( 'NONE', *, *, #46060, .F. ) ;
#90493 = CARTESIAN_POINT ( 'NONE',  ( 77.12841425132344852, 62.56755827935163694, 15.36159490606874556 ) ) ;
#90494 = CARTESIAN_POINT ( 'NONE',  ( 9.401013375279877238, 17.37878583063838889, 9.188101187500006262 ) ) ;
#90495 = AXIS2_PLACEMENT_3D ( 'NONE', #89170, #42475, #50582 ) ;
#90496 = VERTEX_POINT ( 'NONE', #39195 ) ;
#90497 = CARTESIAN_POINT ( 'NONE',  ( 40.37736971981244238, 56.55791953817036699, 10.00000000000000000 ) ) ;
#90499 = VERTEX_POINT ( 'NONE', #40709 ) ;
#90498 = CARTESIAN_POINT ( 'NONE',  ( 199.9393105959312891, 270.2060721569587258, 10.05715988195613164 ) ) ;
#90500 = CARTESIAN_POINT ( 'NONE',  ( 163.2437751800324293, 247.9004826992694461, 9.806027032984305336 ) ) ;
#90501 = CARTESIAN_POINT ( 'NONE',  ( 188.6938424665491141, 259.9925076287862566, 2.228382896047578665 ) ) ;
#90502 = CARTESIAN_POINT ( 'NONE',  ( 149.4444163961335050, 276.2143034153455687, -5.416261063417526778 ) ) ;
#90503 = CARTESIAN_POINT ( 'NONE',  ( 70.36532766715068021, 61.07443295118657289, 14.35799568614401345 ) ) ;
#90504 = CARTESIAN_POINT ( 'NONE',  ( 192.7288556637334125, 292.1918731402626577, -15.52061534916644447 ) ) ;
#90505 = CARTESIAN_POINT ( 'NONE',  ( 170.0343890063719527, 248.3992706227272151, -0.1813713061637557133 ) ) ;
#90506 = CARTESIAN_POINT ( 'NONE',  ( 195.1681749095326097, 291.9751310054545570, 15.48020786373133184 ) ) ;
#90507 = AXIS2_PLACEMENT_3D ( 'NONE', #32209, #56510, #9933 ) ;
#90508 = VERTEX_POINT ( 'NONE', #9850 ) ;
#90509 = CARTESIAN_POINT ( 'NONE',  ( 181.5560669682341484, 271.2834731898979044, -15.97545557697810104 ) ) ;
#90510 = CARTESIAN_POINT ( 'NONE',  ( 68.90560621877192204, 63.79076715805910425, -12.30144644517788421 ) ) ;
#90511 = ORIENTED_EDGE ( 'NONE', *, *, #86527, .T. ) ;
#90512 = CARTESIAN_POINT ( 'NONE',  ( 160.5756158696236469, 275.8270879902572688, 12.72679581559236617 ) ) ;
#90513 = EDGE_CURVE ( 'NONE', #93866, #12312, #49889, .T. ) ;
#90514 = CARTESIAN_POINT ( 'NONE',  ( 174.3820402454518614, 281.0329706854971619, -14.18843254014566924 ) ) ;
#90515 = CARTESIAN_POINT ( 'NONE',  ( 204.2406320560561142, 276.8918436393669822, -14.88456622902110915 ) ) ;
#90516 = CARTESIAN_POINT ( 'NONE',  ( 174.4665098196985298, 288.5002641398569949, -10.08633113632384237 ) ) ;
#90517 = CARTESIAN_POINT ( 'NONE',  ( 164.8411062115066841, 274.0701676799238840, 15.65099743181538194 ) ) ;
#90519 = CARTESIAN_POINT ( 'NONE',  ( 76.06516313603486878, 65.42396348981594656, 14.39793886682782187 ) ) ;
#90518 = CARTESIAN_POINT ( 'NONE',  ( -15.79203335248894469, 167.8149278399160949, -9.188101187500095079 ) ) ;
#90520 = CARTESIAN_POINT ( 'NONE',  ( 185.1996946330573621, 295.7366452146979441, 8.572466393607147239 ) ) ;
#90521 = ORIENTED_EDGE ( 'NONE', *, *, #47274, .F. ) ;
#90522 = B_SPLINE_SURFACE_WITH_KNOTS ( 'NONE', 3, 1, ( 
 ( #48186, #24881 ),
 ( #9190, #2100 ),
 ( #10697, #32495 ),
 ( #48700, #41576 ),
 ( #17282, #86244 ),
 ( #9712, #32980 ),
 ( #72517, #54774 ),
 ( #79634, #41064 ),
 ( #25908, #78098 ),
 ( #2606, #56780 ),
 ( #87763, #3126 ),
 ( #78604, #85753 ),
 ( #40065, #16282 ),
 ( #47176, #24389 ),
 ( #93835, #55262 ),
 ( #16781, #47672 ),
 ( #3604, #88747 ),
 ( #74509, #66870 ),
 ( #34972, #73497 ),
 ( #34483, #95842 ),
 ( #97803, #11703 ),
 ( #89731, #82640 ),
 ( #35968, #81137 ),
 ( #66382, #4080 ),
 ( #74997, #27393 ),
 ( #28372, #19320 ),
 ( #36468, #65874 ),
 ( #59250, #35478 ),
 ( #90229, #5576 ),
 ( #26397, #51169 ),
 ( #20798, #89252 ),
 ( #42080, #5088 ),
 ( #51691, #96830 ),
 ( #44057, #65382 ) ),
 .UNSPECIFIED., .T., .F., .F.,
 ( 4, 2, 2, 2, 2, 2, 2, 2, 2, 2, 2, 2, 2, 2, 2, 2, 4 ),
 ( 2, 2 ),
 ( 0.000000000000000000, 0.06250000000000000000, 0.1250000000000000000, 0.1875000000000000000, 0.2500000000000000000, 0.3125000000000000000, 0.3750000000000000000, 0.4375000000000000000, 0.5000000000000000000, 0.5625000000000000000, 0.6250000000000000000, 0.6875000000000000000, 0.7500000000000000000, 0.8125000000000000000, 0.8750000000000000000, 0.9375000000000000000, 1.000000000000000000 ),
 ( 0.000000000000000000, 1.000000000000000000 ),
 .UNSPECIFIED. ) ;
#90523 = VERTEX_POINT ( 'NONE', #92949 ) ;
#90524 = DIRECTION ( 'NONE',  ( -1.000000000000000000, 0.000000000000000000, 0.000000000000000000 ) ) ;
#90525 = DIRECTION ( 'NONE',  ( -0.000000000000000000, 0.000000000000000000, -1.000000000000000000 ) ) ;
#90526 = CARTESIAN_POINT ( 'NONE',  ( 68.12913145924295577, 66.36538084368893919, -9.493516625238422435 ) ) ;
#90527 = CARTESIAN_POINT ( 'NONE',  ( 67.04719753439840702, 66.82148211118030190, -8.940350841082095101 ) ) ;
#90528 = CARTESIAN_POINT ( 'NONE',  ( 86.73093147390520130, 43.68969761139900498, 3.372955308790926754 ) ) ;
#90529 = CARTESIAN_POINT ( 'NONE',  ( 84.55460127224613132, 47.09886495345954671, 11.09894356431207818 ) ) ;
#90530 = CARTESIAN_POINT ( 'NONE',  ( 150.0802157573592126, 276.6422289437092559, 3.399058894176778534 ) ) ;
#90531 = CARTESIAN_POINT ( 'NONE',  ( 2.719259653403429233, 178.5024278399160949, -9.188101187500093303 ) ) ;
#90532 = CARTESIAN_POINT ( 'NONE',  ( 121.7437996339097310, 241.0958772461660544, -9.188101187500095079 ) ) ;
#90533 = FACE_OUTER_BOUND ( 'NONE', #20420, .T. ) ;
#90534 = CARTESIAN_POINT ( 'NONE',  ( 180.8614647981713119, 256.2301897900337053, -2.334466546830306299 ) ) ;
#90535 = CARTESIAN_POINT ( 'NONE',  ( 78.51615055793223519, 53.63995692175274854, 15.85712610117593080 ) ) ;
#90536 = CARTESIAN_POINT ( 'NONE',  ( 198.4160757083882345, 267.1808215963346242, -8.346050686629251203 ) ) ;
#90537 = CARTESIAN_POINT ( 'NONE',  ( 190.6585475213478560, 299.9177820201669533, -4.437337276038273437 ) ) ;
#90538 = PRODUCT_RELATED_PRODUCT_CATEGORY ( 'part', '', ( #43521 ) ) ;
#90539 = DIRECTION ( 'NONE',  ( 0.8116583814955234955, 0.01378320505841451778, 0.5839697723396178874 ) ) ;
#90540 = CARTESIAN_POINT ( 'NONE',  ( 183.8673499631198354, 275.0308414889168489, 16.36260528999715902 ) ) ;
#90541 = CARTESIAN_POINT ( 'NONE',  ( 148.3629184514745987, 273.6748826132846375, -8.219814532462343948 ) ) ;
#90542 = CARTESIAN_POINT ( 'NONE',  ( 70.60537956472130361, 60.95729775083580648, -14.46506356667156190 ) ) ;
#90543 = CARTESIAN_POINT ( 'NONE',  ( 84.85964987685913741, 50.19146562821751445, 13.75030272624154470 ) ) ;
#90544 = CARTESIAN_POINT ( 'NONE',  ( 196.0328332463135155, 266.6894456190431697, 8.014243085850971227 ) ) ;
#90545 = DIRECTION ( 'NONE',  ( -0.8660254037844387076, -0.4999999999999998890, -0.000000000000000000 ) ) ;
#90546 = CARTESIAN_POINT ( 'NONE',  ( 162.5729406961995096, 251.2985046087954402, -12.76312550842038718 ) ) ;
#90547 = DIRECTION ( 'NONE',  ( 0.3074612162317589825, -0.9515606131578205895, 0.000000000000000000 ) ) ;
#90548 = CARTESIAN_POINT ( 'NONE',  ( 172.9828220029686747, 262.8000787801868228, -16.17504394412311086 ) ) ;
#90549 = CARTESIAN_POINT ( 'NONE',  ( 97.38683515247240052, 227.0333772461660544, 9.188101187500095079 ) ) ;
#90550 = CARTESIAN_POINT ( 'NONE',  ( 8.859747497914600700, 17.06628583063839599, -9.188101187500006262 ) ) ;
#90551 = DIRECTION ( 'NONE',  ( 0.8660254037844395958, 0.4999999999999985567, 0.000000000000000000 ) ) ;
#90552 = CIRCLE ( 'NONE', #85710, 0.1418229129680828593 ) ;
#90553 = DIRECTION ( 'NONE',  ( -0.8903844177683322147, -0.4552093898365321412, 0.000000000000000000 ) ) ;
#90555 = CARTESIAN_POINT ( 'NONE',  ( 83.93039057805418679, 42.25368239170656182, -3.699647659905914931 ) ) ;
#90554 = CARTESIAN_POINT ( 'NONE',  ( 195.9713281756800427, 291.2146981034049418, 17.52210387885178022 ) ) ;
#90556 = CARTESIAN_POINT ( 'NONE',  ( 149.0651262117185354, 272.4586230950732784, 12.81403047969042319 ) ) ;
#90557 = CARTESIAN_POINT ( 'NONE',  ( 205.2706556652093752, 273.1077904153184477, -10.97544480913108167 ) ) ;
#90558 = CARTESIAN_POINT ( 'NONE',  ( 160.9155581428462085, 282.2930683307629920, -7.657675304491033508 ) ) ;
#90559 = EDGE_CURVE ( 'NONE', #77091, #47670, #24519, .T. ) ;
#90560 = CARTESIAN_POINT ( 'NONE',  ( 42.48198750171711424, 33.03085787977767041, 9.188101187500006262 ) ) ;
#90561 = CARTESIAN_POINT ( 'NONE',  ( 146.7842303614460207, 276.4092505945183689, -4.491116827832889236 ) ) ;
#90562 = FACE_BOUND ( 'NONE', #34009, .T. ) ;
#90563 = ORIENTED_EDGE ( 'NONE', *, *, #65419, .T. ) ;
#90564 = CARTESIAN_POINT ( 'NONE',  ( 24.44820476603448611, 26.06628583063842086, -9.188101187500006262 ) ) ;
#90565 = AXIS2_PLACEMENT_3D ( 'NONE', #39230, #31633, #84396 ) ;
#90566 = CARTESIAN_POINT ( 'NONE',  ( 172.4678624035182679, 290.8891845726454903, -0.5858198065817201705 ) ) ;
#90567 = CARTESIAN_POINT ( 'NONE',  ( 197.3327212804159103, 267.5970440452412049, 9.861675131224707513 ) ) ;
#90568 = CARTESIAN_POINT ( 'NONE',  ( 187.9710278913847219, 285.9884846539495129, -16.45153272977178460 ) ) ;
#90569 = VERTEX_POINT ( 'NONE', #17942 ) ;
#90570 = CARTESIAN_POINT ( 'NONE',  ( 70.58551217508033915, 60.91456802530846915, 15.00778779846412192 ) ) ;
#90571 = CARTESIAN_POINT ( 'NONE',  ( 198.6562788533279615, 286.5642271139020636, 17.47134757795404525 ) ) ;
#90573 = EDGE_CURVE ( 'NONE', #8415, #31684, #9393, .T. ) ;
#90572 = CARTESIAN_POINT ( 'NONE',  ( 157.4753914210714356, 268.7471219652609875, 15.64991620571603015 ) ) ;
#90574 = LINE ( 'NONE', #36808, #17795 ) ;
#90575 = AXIS2_PLACEMENT_3D ( 'NONE', #5566, #60732, #14169 ) ;
#90576 = CARTESIAN_POINT ( 'NONE',  ( 134.3282312844263231, 248.3615022471902591, -10.00000000000009592 ) ) ;
#90577 = CARTESIAN_POINT ( 'NONE',  ( 157.0877926458200307, 258.5629572190321710, -17.40668770468195703 ) ) ;
#90578 = ORIENTED_EDGE ( 'NONE', *, *, #64431, .F. ) ;
#90579 = DIRECTION ( 'NONE',  ( -0.8660254037844378194, -0.5000000000000014433, -0.000000000000000000 ) ) ;
#90580 = B_SPLINE_SURFACE_WITH_KNOTS ( 'NONE', 3, 1, ( 
 ( #34328, #73341 ),
 ( #3928, #18643 ),
 ( #57613, #34811 ),
 ( #49523, #73832 ),
 ( #97166, #58601 ),
 ( #4421, #65712 ),
 ( #96168, #96667 ),
 ( #35317, #43410 ),
 ( #41924, #72358 ),
 ( #27235, #25745 ),
 ( #95690, #19651 ),
 ( #51011, #26237 ),
 ( #57112, #20139 ),
 ( #74357, #58120 ),
 ( #56625, #12039 ),
 ( #88592, #88094 ),
 ( #80476, #11046 ),
 ( #89101, #65225 ),
 ( #50513, #72860 ),
 ( #81962, #35821 ),
 ( #87608, #90577 ),
 ( #59091, #13537 ),
 ( #70066, #39153 ),
 ( #100005, #90065 ),
 ( #66716, #92912 ),
 ( #98139, #684 ),
 ( #15362, #53860 ),
 ( #85854, #44407 ),
 ( #77181, #46258 ),
 ( #69579, #69078 ),
 ( #7787, #23974 ),
 ( #46784, #31566 ),
 ( #31069, #93423 ),
 ( #74848, #28724 ) ),
 .UNSPECIFIED., .T., .F., .F.,
 ( 4, 2, 2, 2, 2, 2, 2, 2, 2, 2, 2, 2, 2, 2, 2, 2, 4 ),
 ( 2, 2 ),
 ( 0.000000000000000000, 0.06250000000000000000, 0.1250000000000000000, 0.1875000000000000000, 0.2500000000000000000, 0.3125000000000000000, 0.3750000000000000000, 0.4375000000000000000, 0.5000000000000000000, 0.5625000000000000000, 0.6250000000000000000, 0.6875000000000000000, 0.7500000000000000000, 0.8125000000000000000, 0.8750000000000000000, 0.9375000000000000000, 1.000000000000000000 ),
 ( 0.000000000000000000, 1.000000000000000000 ),
 .UNSPECIFIED. ) ;
#90581 = ORIENTED_EDGE ( 'NONE', *, *, #80604, .T. ) ;
#90582 = CARTESIAN_POINT ( 'NONE',  ( 155.5311623832600958, 261.6886619413561448, 17.00987194985870943 ) ) ;
#90583 = CARTESIAN_POINT ( 'NONE',  ( 83.66501680638440064, 41.65036927881936890, 1.209882539926571354 ) ) ;
#90584 = ADVANCED_FACE ( 'NONE', ( #41204 ), #86886, .T. ) ;
#90585 = ORIENTED_EDGE ( 'NONE', *, *, #49000, .F. ) ;
#90586 = CARTESIAN_POINT ( 'NONE',  ( 181.9559929377375056, 291.6402902057536721, -11.43735378946719372 ) ) ;
#90587 = VERTEX_POINT ( 'NONE', #31604 ) ;
#90588 = DIRECTION ( 'NONE',  ( 0.3213938048432692374, -0.5566703992264209200, -0.7660444431189770143 ) ) ;
#90589 = CARTESIAN_POINT ( 'NONE',  ( 3.297978757390601423, 24.83705186507751606, 3.090169943749475401 ) ) ;
#90590 = CARTESIAN_POINT ( 'NONE',  ( 191.4302501518540396, 279.3169626480661805, -16.56989974033457358 ) ) ;
#90591 = CARTESIAN_POINT ( 'NONE',  ( 192.9772420103627724, 296.4006074639731310, -13.54979510632026063 ) ) ;
#90592 = CARTESIAN_POINT ( 'NONE',  ( 201.4214977800931763, 281.7747274386935601, -17.04225209925078133 ) ) ;
#90593 = VECTOR ( 'NONE', #20017, 1000.000000000000114 ) ;
#90594 = CARTESIAN_POINT ( 'NONE',  ( 39.98734656443052415, 28.80170272979929535, 7.433330006724137462 ) ) ;
#90595 = CARTESIAN_POINT ( 'NONE',  ( 78.02766155223862654, 58.91636306235935905, -16.12600223474660410 ) ) ;
#90596 = PLANE ( 'NONE',  #30365 ) ;
#90597 = CARTESIAN_POINT ( 'NONE',  ( 87.55848707468658176, 45.50985013822432990, 6.922438743303467312 ) ) ;
#90598 = ORIENTED_EDGE ( 'NONE', *, *, #64639, .T. ) ;
#90599 = VERTEX_POINT ( 'NONE', #25013 ) ;
#90600 = CARTESIAN_POINT ( 'NONE',  ( 182.5579995116864325, 296.7134427671203980, 0.3470945606806519201 ) ) ;
#90602 = FACE_OUTER_BOUND ( 'NONE', #84344, .T. ) ;
#90601 = PLANE ( 'NONE',  #58463 ) ;
#90603 = CARTESIAN_POINT ( 'NONE',  ( 181.3346534254663140, 271.3440730695800767, -17.45372068697093226 ) ) ;
#90604 = CARTESIAN_POINT ( 'NONE',  ( 77.57770355975000598, 59.80217626084218097, -16.01913283567768076 ) ) ;
#90605 = CARTESIAN_POINT ( 'NONE',  ( 147.6947327179224487, 274.8322142526899370, 9.090449717876689206 ) ) ;
#90606 = CARTESIAN_POINT ( 'NONE',  ( 167.2132997600114379, 286.2193399160603349, -4.798080686485812762 ) ) ;
#90607 = CARTESIAN_POINT ( 'NONE',  ( 76.86986466358051473, 64.04458250793000218, -15.20481942635857742 ) ) ;
#90608 = CARTESIAN_POINT ( 'NONE',  ( 181.4694507228112457, 256.9988949691801281, 4.992663963241201763 ) ) ;
#90609 = CARTESIAN_POINT ( 'NONE',  ( 104.5854977735480560, 237.3149278399160664, 9.188101187500093303 ) ) ;
#90610 = ORIENTED_EDGE ( 'NONE', *, *, #41746, .T. ) ;
#90612 = B_SPLINE_CURVE_WITH_KNOTS ( 'NONE', 3,
 ( #82414, #90992, #28150, #12979, #36238, #74288, #50945, #29646, #99064, #43840, #21553, #59525 ),
 .UNSPECIFIED., .F., .F.,
 ( 4, 2, 2, 2, 2, 4 ),
 ( 0.001199298977550974313, 0.001655502193913219351, 0.001883603802094317801, 0.002111705410275416250, 0.002567908626637613149, 0.003024111842999810049 ),
 .UNSPECIFIED. ) ;
#90611 = CARTESIAN_POINT ( 'NONE',  ( 148.2404373810095706, 275.8870260502966403, -5.709515531134017330 ) ) ;
#90613 = CARTESIAN_POINT ( 'NONE',  ( 188.2363250879724887, 273.5010258966393621, 15.66123827714173089 ) ) ;
#90614 = VERTEX_POINT ( 'NONE', #40200 ) ;
#90615 = ORIENTED_EDGE ( 'NONE', *, *, #8680, .T. ) ;
#90616 = EDGE_CURVE ( 'NONE', #54113, #32823, #32623, .T. ) ;
#90617 = CARTESIAN_POINT ( 'NONE',  ( 87.04951863019347513, 45.82536234993809643, -8.629913247614998895 ) ) ;
#90618 = EDGE_CURVE ( 'NONE', #65984, #3452, #48841, .T. ) ;
#90619 = CARTESIAN_POINT ( 'NONE',  ( 180.6668490247078864, 294.2638964725952633, -2.198001587704702331 ) ) ;
#90620 = CARTESIAN_POINT ( 'NONE',  ( 196.4994169513186364, 290.3000215130921902, 16.82935102260526961 ) ) ;
#90621 = CARTESIAN_POINT ( 'NONE',  ( 206.6703863510205679, 272.6833857505801006, -10.72500664779635393 ) ) ;
#90622 = CARTESIAN_POINT ( 'NONE',  ( 192.0969986600162827, 271.0201763999182845, -15.22553433325905736 ) ) ;
#90623 = ORIENTED_EDGE ( 'NONE', *, *, #43745, .T. ) ;
#90624 = ORIENTED_EDGE ( 'NONE', *, *, #98157, .F. ) ;
#90625 = DIRECTION ( 'NONE',  ( -0.000000000000000000, 0.000000000000000000, -1.000000000000000000 ) ) ;
#90626 = ORIENTED_EDGE ( 'NONE', *, *, #62910, .F. ) ;
#90627 = CIRCLE ( 'NONE', #67933, 12.50000000000000000 ) ;
#90628 = EDGE_CURVE ( 'NONE', #85879, #17498, #94460, .T. ) ;
#90629 = CARTESIAN_POINT ( 'NONE',  ( 192.6230444026213036, 263.8685375577596233, -8.332581229518458699 ) ) ;
#90630 = CARTESIAN_POINT ( 'NONE',  ( 185.7952724173880483, 257.5178294002433290, 0.9274047933272019373 ) ) ;
#90631 = CARTESIAN_POINT ( 'NONE',  ( 67.95642171729713255, 69.05834527840744386, -4.640993296857849337 ) ) ;
#90633 = CARTESIAN_POINT ( 'NONE',  ( 69.40753887930063115, 62.89835586300766579, -13.67854514043513525 ) ) ;
#90632 = CARTESIAN_POINT ( 'NONE',  ( 187.4684169401624843, 291.1055366833039670, -13.65599679362259167 ) ) ;
#90634 = CARTESIAN_POINT ( 'NONE',  ( 153.0927037754837556, 265.4826541232073964, -16.15085267704102634 ) ) ;
#90635 = ORIENTED_EDGE ( 'NONE', *, *, #31635, .F. ) ;
#90636 = B_SPLINE_CURVE_WITH_KNOTS ( 'NONE', 3,
 ( #41915, #28079, #40893, #74212 ),
 .UNSPECIFIED., .F., .F.,
 ( 4, 4 ),
 ( 0.0008273161503298089633, 0.008754319486608567666 ),
 .UNSPECIFIED. ) ;
#90637 = CARTESIAN_POINT ( 'NONE',  ( 190.2510882691990730, 301.1224442529128851, -5.480893437181090455 ) ) ;
#90638 = ADVANCED_FACE ( 'NONE', ( #72144 ), #86383, .T. ) ;
#90639 = CARTESIAN_POINT ( 'NONE',  ( 71.14846176242140530, 61.60121696541033742, 14.32671748640477460 ) ) ;
#90640 = CARTESIAN_POINT ( 'NONE',  ( 190.6103240053217860, 264.3150132381076673, -9.438093754014104775 ) ) ;
#90641 = EDGE_CURVE ( 'NONE', #80312, #16011, #59560, .T. ) ;
#90642 = CARTESIAN_POINT ( 'NONE',  ( 173.3711701851306941, 251.4955055664892427, -0.7996342223137038463 ) ) ;
#90643 = CARTESIAN_POINT ( 'NONE',  ( 118.7397740163064128, 239.3615022471902307, -10.00000000000009592 ) ) ;
#90644 = CARTESIAN_POINT ( 'NONE',  ( 71.78913936505468030, 72.20160104369585952, 3.260718063500199548 ) ) ;
#90645 = CARTESIAN_POINT ( 'NONE',  ( 83.26766257861952170, 43.36122241240380504, 7.252070224612332972 ) ) ;
#90646 = CARTESIAN_POINT ( 'NONE',  ( 137.1969404309142817, 260.0177522451418781, 5.000000000000046185 ) ) ;
#90647 = AXIS2_PLACEMENT_3D ( 'NONE', #31417, #77546, #69915 ) ;
#90648 = CARTESIAN_POINT ( 'NONE',  ( 79.65794105133953451, 48.82961183344457368, 14.10136067249946024 ) ) ;
#90649 = CARTESIAN_POINT ( 'NONE',  ( 68.03078532392423483, 69.75226796743223190, -1.878725101587667146 ) ) ;
#90650 = CARTESIAN_POINT ( 'NONE',  ( 56.79189435007682363, 203.5958772461660544, -9.188101187500095079 ) ) ;
#90651 = CARTESIAN_POINT ( 'NONE',  ( 159.7692415128758228, 253.9185515433934768, -16.85856106119654285 ) ) ;
#90652 = DIRECTION ( 'NONE',  ( 0.8660254037844399289, 0.4999999999999977240, -0.000000000000000000 ) ) ;
#90653 = CARTESIAN_POINT ( 'NONE',  ( 208.1303168694798273, 270.1547119170880364, -0.9257663487928086132 ) ) ;
#90654 = CARTESIAN_POINT ( 'NONE',  ( 66.63322413591409088, 67.62875759604085601, 6.186734474800332784 ) ) ;
#90655 = B_SPLINE_CURVE_WITH_KNOTS ( 'NONE', 3,
 ( #94018, #7890, #39251, #24570, #55455, #34067, #64958, #26461, #84421, #76778, #7371, #69170, #18865, #57834, #42626, #96387, #57337, #97858, #19862, #74569, #66443, #67427, #51751, #11763, #28429, #49747, #43115, #58332, #81684, #89308, #59311, #5633, #75056, #4139, #74059, #26951, #90290, #82693, #43630, #98358, #4648, #27462, #88311, #80700, #35034, #65442, #58818, #88815, #65938, #96892 ),
 .UNSPECIFIED., .F., .F.,
 ( 4, 2, 2, 2, 2, 2, 2, 2, 2, 2, 2, 2, 2, 2, 2, 2, 2, 2, 2, 2, 2, 2, 2, 2, 4 ),
 ( 0.0002689362054544326024, 0.0007455428061392906005, 0.001222149406824148653, 0.001460452707166577570, 0.001579604357337793114, 0.001698756007509008657, 0.001817907657680224200, 0.001937059307851439743, 0.002175362608193776286, 0.002651969208878449807, 0.003128575809563122461, 0.004081789010932469937, 0.005035002212301816979, 0.005511608812986444964, 0.005749912113328714720, 0.005869063763499849165, 0.005988215413670983610, 0.006047791238756500959, 0.006107367063842016573, 0.006226518714013051271, 0.006464822014355107657, 0.006941428615039225633, 0.007418035215723343609, 0.007656338516065450302, 0.007894641816407556995 ),
 .UNSPECIFIED. ) ;
#90656 = AXIS2_PLACEMENT_3D ( 'NONE', #68665, #36278, #22078 ) ;
#90657 = CARTESIAN_POINT ( 'NONE',  ( 161.8668411317136986, 250.2854024296290447, -13.43522912998426655 ) ) ;
#90658 = CARTESIAN_POINT ( 'NONE',  ( 189.6738045434663320, 300.1223289962524063, 4.832295392723879424 ) ) ;
#90659 = CARTESIAN_POINT ( 'NONE',  ( 185.9562832929018157, 265.4319297318980375, 13.85577190340941378 ) ) ;
#90660 = CARTESIAN_POINT ( 'NONE',  ( 70.80322137413752159, 60.50400129575321273, -14.70302039727343413 ) ) ;
#90661 = CARTESIAN_POINT ( 'NONE',  ( 35.07028576228009342, 43.18080186712595747, 3.090169943749475401 ) ) ;
#90662 = B_SPLINE_CURVE_WITH_KNOTS ( 'NONE', 3,
 ( #21262, #29359, #14153, #60225 ),
 .UNSPECIFIED., .F., .F.,
 ( 4, 4 ),
 ( 0.03672685766160826981, 0.04538173523955296024 ),
 .UNSPECIFIED. ) ;
#90663 = CARTESIAN_POINT ( 'NONE',  ( 149.8532179585512267, 272.8608575990943450, -11.50785342781380116 ) ) ;
#90664 = CARTESIAN_POINT ( 'NONE',  ( 82.43809236625457970, 54.24053208071835286, 15.60321882952343842 ) ) ;
#90665 = CARTESIAN_POINT ( 'NONE',  ( 72.10617024684211174, 72.18421392457028674, 4.031754617348227043 ) ) ;
#90666 = CARTESIAN_POINT ( 'NONE',  ( 32.70573635520464251, 183.5643266524160140, 9.188101187500095079 ) ) ;
#90667 = CARTESIAN_POINT ( 'NONE',  ( 157.6673516573649181, 257.5591315650518141, 16.79781451397666103 ) ) ;
#90668 = CARTESIAN_POINT ( 'NONE',  ( 46.74164954608104949, 27.39040679176987325, -6.890680421881970419E-14 ) ) ;
#90669 = CARTESIAN_POINT ( 'NONE',  ( 77.53589688945717739, 51.31089695689070851, -15.44518354484521083 ) ) ;
#90670 = CARTESIAN_POINT ( 'NONE',  ( 72.00459748831643481, 72.21134089809413581, -1.634945730901812722 ) ) ;
#90671 = CARTESIAN_POINT ( 'NONE',  ( 55.76366273096530080, 196.8768266524160140, 9.188101187500096856 ) ) ;
#90672 = EDGE_CURVE ( 'NONE', #83319, #28762, #98436, .T. ) ;
#90673 = CARTESIAN_POINT ( 'NONE',  ( 19.57800816787531062, 26.70171378149919050, -9.188101187500004485 ) ) ;
#90674 = CARTESIAN_POINT ( 'NONE',  ( 151.4428545556028780, 268.3402767968688067, -15.03309903163500749 ) ) ;
#90675 = CARTESIAN_POINT ( 'NONE',  ( 149.5796913320911870, 271.5673701627850960, -12.80793412251569841 ) ) ;
#90676 = CARTESIAN_POINT ( 'NONE',  ( 3.278110179240818045, 23.93396525600387648, 2.839279412974139660 ) ) ;
#90677 = CARTESIAN_POINT ( 'NONE',  ( 198.1847055346428590, 286.9842163890704683, 16.95145238430053070 ) ) ;
#90678 = CARTESIAN_POINT ( 'NONE',  ( 75.83332386201834652, 58.24149532073650448, 16.46778979864901160 ) ) ;
#90679 = CARTESIAN_POINT ( 'NONE',  ( 179.6504827179812480, 276.7753844222579573, 16.30384834125107218 ) ) ;
#90680 = CARTESIAN_POINT ( 'NONE',  ( 82.21717897060236169, 40.84507121292054421, -1.199451623573249970 ) ) ;
#90681 = CARTESIAN_POINT ( 'NONE',  ( 71.08662668937095930, 67.82508006278297330, -9.836311824178357810 ) ) ;
#90682 = CARTESIAN_POINT ( 'NONE',  ( 163.6073896235010636, 255.4122057569755952, -14.91336208084822168 ) ) ;
#90683 = EDGE_CURVE ( 'NONE', #9269, #30721, #2244, .T. ) ;
#90684 = DIRECTION ( 'NONE',  ( 0.4999999999999992784, -0.8660254037844390407, 0.000000000000000000 ) ) ;
#90685 = CARTESIAN_POINT ( 'NONE',  ( 105.8215617431885818, 225.2365022471902023, -10.00000000000009059 ) ) ;
#90686 = FACE_OUTER_BOUND ( 'NONE', #51898, .T. ) ;
#90687 = CARTESIAN_POINT ( 'NONE',  ( 170.3290958195750022, 289.6815776661216546, -1.151831906498994140 ) ) ;
#90688 = ORIENTED_EDGE ( 'NONE', *, *, #41807, .T. ) ;
#90689 = CARTESIAN_POINT ( 'NONE',  ( 52.89478003304684250, 201.3458772461660260, 9.188101187500095079 ) ) ;
#90690 = ORIENTED_EDGE ( 'NONE', *, *, #37699, .T. ) ;
#90691 = CARTESIAN_POINT ( 'NONE',  ( 166.4514803149947966, 264.9061636045831847, 16.72458767844168648 ) ) ;
#90692 = CARTESIAN_POINT ( 'NONE',  ( 147.3023124603499809, 275.5119060767245287, 5.196938859334171212 ) ) ;
#90693 = ADVANCED_FACE ( 'NONE', ( #77745 ), #18424, .F. ) ;
#90695 = CARTESIAN_POINT ( 'NONE',  ( 171.9208136763257926, 265.2263239767592040, 17.32491798815716422 ) ) ;
#90694 = VECTOR ( 'NONE', #43839, 1000.000000000000000 ) ;
#90696 = ORIENTED_EDGE ( 'NONE', *, *, #52909, .T. ) ;
#90697 = DIRECTION ( 'NONE',  ( -0.8660254037844359321, -0.5000000000000051070, -0.000000000000000000 ) ) ;
#90698 = CARTESIAN_POINT ( 'NONE',  ( 207.6826438088389750, 270.9301044032979462, 7.252082088659585146 ) ) ;
#90699 = DIRECTION ( 'NONE',  ( -0.000000000000000000, -0.000000000000000000, -1.000000000000000000 ) ) ;
#90700 = CARTESIAN_POINT ( 'NONE',  ( 86.40862467444883066, 43.51472063525788059, 4.903409472307490802 ) ) ;
#90701 = FACE_OUTER_BOUND ( 'NONE', #8046, .T. ) ;
#90702 = CARTESIAN_POINT ( 'NONE',  ( 157.3880781592554285, 258.0428474529849723, 18.15852591502753555 ) ) ;
#90703 = VERTEX_POINT ( 'NONE', #96467 ) ;
#90704 = CARTESIAN_POINT ( 'NONE',  ( 17.01121839442928163, 30.79752408145592568, -5.678558825948271327 ) ) ;
#90705 = CARTESIAN_POINT ( 'NONE',  ( 76.13725175568590942, 60.79812444030506668, 15.65525560863753896 ) ) ;
#90706 = CARTESIAN_POINT ( 'NONE',  ( 72.54520184348785961, 70.27380328412901633, -7.860630163369380696 ) ) ;
#90707 = CARTESIAN_POINT ( 'NONE',  ( 75.28634535225387481, 66.86406054372800156, -12.88709815648634383 ) ) ;
#90708 = EDGE_CURVE ( 'NONE', #35, #59274, #67007, .T. ) ;
#90709 = ORIENTED_EDGE ( 'NONE', *, *, #68900, .T. ) ;
#90710 = CARTESIAN_POINT ( 'NONE',  ( 76.87300970902636266, 55.60219541319754200, 16.60077664465815417 ) ) ;
#90711 = CARTESIAN_POINT ( 'NONE',  ( 167.9276914116459523, 262.1860323319936015, 16.09630263804044148 ) ) ;
#90712 = ADVANCED_FACE ( 'NONE', ( #87896 ), #95297, .F. ) ;
#90713 = CARTESIAN_POINT ( 'NONE',  ( 159.2102594322688844, 254.8867369075254885, -16.13039487917589199 ) ) ;
#90714 = VECTOR ( 'NONE', #28530, 1000.000000000000227 ) ;
#90715 = ORIENTED_EDGE ( 'NONE', *, *, #8854, .F. ) ;
#90717 = CYLINDRICAL_SURFACE ( 'NONE', #21645, 10.00000000000010658 ) ;
#90716 = CARTESIAN_POINT ( 'NONE',  ( 70.82117999291602928, 62.89421842260256312, 14.15644170336123153 ) ) ;
#90718 = CARTESIAN_POINT ( 'NONE',  ( 4.102725850843912170, 28.55253618238879909, -10.00000000000000000 ) ) ;
#90719 = CARTESIAN_POINT ( 'NONE',  ( 66.41647611861264977, 68.75673559357331044, -2.143700313894566278 ) ) ;
#90720 = CARTESIAN_POINT ( 'NONE',  ( 159.9880386575927957, 253.5395837721924863, 15.85893018594752846 ) ) ;
#90721 = CARTESIAN_POINT ( 'NONE',  ( 84.68093819348166562, 42.16537887657799644, 0.2499978311480390847 ) ) ;
#90722 = CARTESIAN_POINT ( 'NONE',  ( 164.5959123184142356, 265.0909081389784205, -16.62699299347688253 ) ) ;
#90723 = CARTESIAN_POINT ( 'NONE',  ( 131.9199452241419124, 234.7202760586659736, -5.415160957724236172E-17 ) ) ;
#90724 = CYLINDRICAL_SURFACE ( 'NONE', #66680, 17.82106496071139645 ) ;
#90725 = ORIENTED_EDGE ( 'NONE', *, *, #77029, .T. ) ;
#90726 = CARTESIAN_POINT ( 'NONE',  ( 170.1494630792247449, 264.1798617481715610, 16.79485409072000834 ) ) ;
#90727 = CARTESIAN_POINT ( 'NONE',  ( -22.42236680055709641, 157.8615022471902591, 0.000000000000000000 ) ) ;
#90728 = ORIENTED_EDGE ( 'NONE', *, *, #92013, .F. ) ;
#90729 = CARTESIAN_POINT ( 'NONE',  ( 160.4401160996124815, 253.2479743581097580, 14.60890098605380949 ) ) ;
#90730 = EDGE_LOOP ( 'NONE', ( #71238, #73345, #61509, #66380 ) ) ;
#90731 = ORIENTED_EDGE ( 'NONE', *, *, #30205, .F. ) ;
#90732 = EDGE_CURVE ( 'NONE', #58893, #49038, #14312, .T. ) ;
#90733 = CARTESIAN_POINT ( 'NONE',  ( 87.90566119885008334, 214.8927522451418497, 10.00000000000009948 ) ) ;
#90734 = CARTESIAN_POINT ( 'NONE',  ( 194.7442550381435638, 291.6868277426822260, -16.06123382811687605 ) ) ;
#90735 = CARTESIAN_POINT ( 'NONE',  ( -4.903394573382326094, 174.6427522451419350, -10.00000000000009592 ) ) ;
#90736 = CARTESIAN_POINT ( 'NONE',  ( 25.38399186717684231, 173.9155109091896350, 2.679491924311254714 ) ) ;
#90737 = CARTESIAN_POINT ( 'NONE',  ( 73.05863210132505969, 69.60576123971951290, -9.808587366596233537 ) ) ;
#90738 = CARTESIAN_POINT ( 'NONE',  ( 194.0672051292551430, 294.5127359636757660, 15.53337744471869364 ) ) ;
#90739 = CARTESIAN_POINT ( 'NONE',  ( -19.65312891409030271, 93.06504152958497400, 60.00000000000000000 ) ) ;
#90740 = ORIENTED_EDGE ( 'NONE', *, *, #86739, .F. ) ;
#90741 = ADVANCED_FACE ( 'NONE', ( #92837 ), #49144, .F. ) ;
#90742 = CARTESIAN_POINT ( 'NONE',  ( 114.6081111488702220, 243.6427522451419065, -10.00000000000009592 ) ) ;
#90743 = CARTESIAN_POINT ( 'NONE',  ( 200.7484899876179441, 282.9404111291507888, -16.88964748465601673 ) ) ;
#90744 = CARTESIAN_POINT ( 'NONE',  ( 66.38217553272322391, 68.79393763757845193, -4.316952526664222134 ) ) ;
#90745 = ORIENTED_EDGE ( 'NONE', *, *, #77073, .F. ) ;
#90746 = PLANE ( 'NONE',  #89068 ) ;
#90747 = CARTESIAN_POINT ( 'NONE',  ( 76.05851436047953484, 51.43505017026153325, -16.15825921707162394 ) ) ;
#90748 = LINE ( 'NONE', #67387, #80450 ) ;
#90749 = EDGE_CURVE ( 'NONE', #43182, #89564, #58291, .T. ) ;
#90750 = EDGE_CURVE ( 'NONE', #46359, #64907, #39792, .T. ) ;
#90751 = CARTESIAN_POINT ( 'NONE',  ( 205.8918578537579833, 274.0318366629789466, 11.52627491423194250 ) ) ;
#90752 = EDGE_CURVE ( 'NONE', #61436, #6810, #54554, .T. ) ;
#90753 = CARTESIAN_POINT ( 'NONE',  ( 196.2630260332681189, 290.7094625936034049, -17.43112004684450866 ) ) ;
#90754 = CARTESIAN_POINT ( 'NONE',  ( 194.8811071667591364, 279.6953583877882465, 17.03940305312293901 ) ) ;
#90755 = CARTESIAN_POINT ( 'NONE',  ( 207.5570596878370679, 271.1476224814971374, 2.444960520848353358 ) ) ;
#90756 = EDGE_CURVE ( 'NONE', #94179, #64640, #88265, .T. ) ;
#90757 = CARTESIAN_POINT ( 'NONE',  ( 131.5133883985292016, 255.9244531367911293, -4.594050593750046652 ) ) ;
#90758 = VERTEX_POINT ( 'NONE', #73512 ) ;
#90759 = LINE ( 'NONE', #21310, #96706 ) ;
#90760 = EDGE_CURVE ( 'NONE', #22789, #48279, #18964, .T. ) ;
#90761 = CARTESIAN_POINT ( 'NONE',  ( 71.35329583521033214, 67.64943209593164397, -10.88520583469783887 ) ) ;
#90762 = LINE ( 'NONE', #14206, #59406 ) ;
#90763 = CARTESIAN_POINT ( 'NONE',  ( 72.99046944781451884, 70.71697578006111939, 8.277156641257130687 ) ) ;
#90764 = CARTESIAN_POINT ( 'NONE',  ( 178.7427661924620850, 254.2096309538193282, 4.677055477819860307 ) ) ;
#90765 = VERTEX_POINT ( 'NONE', #56795 ) ;
#90766 = CARTESIAN_POINT ( 'NONE',  ( 76.39332965939082953, 54.12380165434665003, 16.07031247584009392 ) ) ;
#90767 =( BOUNDED_CURVE ( )  B_SPLINE_CURVE ( 2, ( #56268, #17796, #87264, #3121, #31966, #18297, #64891, #80129, #71995 ),
 .UNSPECIFIED., .F., .T. ) 
 B_SPLINE_CURVE_WITH_KNOTS ( ( 3, 2, 2, 2, 3 ),
 ( 0.5927419354838709964, 0.5940860215053763715, 0.5967741935483871218, 0.5994623655913978721, 0.6008064516129032473 ),
 .UNSPECIFIED. ) 
 CURVE ( )  GEOMETRIC_REPRESENTATION_ITEM ( )  RATIONAL_B_SPLINE_CURVE ( ( 0.9330127018922194093, 0.9330127018922194093, 1.000000000000000000, 0.8660254037844387076, 1.000000000000000000, 0.8660254037844387076, 1.000000000000000000, 0.9330127018922194093, 0.9330127018922194093 ) ) 
 REPRESENTATION_ITEM ( '' )  );
#90768 = CARTESIAN_POINT ( 'NONE',  ( 77.93017357788674815, 184.0458036431181768, 30.52142883766498116 ) ) ;
#90769 = CARTESIAN_POINT ( 'NONE',  ( 72.62522464330835703, 71.47837554186844500, -5.665107215650756700 ) ) ;
#90770 = CARTESIAN_POINT ( 'NONE',  ( 81.68759648889933089, 55.58869686435339474, 15.96161034574013904 ) ) ;
#90771 = CARTESIAN_POINT ( 'NONE',  ( 202.4223208072874343, 267.6828090875848147, 0.8583124146943408306 ) ) ;
#90772 = CARTESIAN_POINT ( 'NONE',  ( 190.4240181651484818, 300.8229208869809668, -4.214281362166949485 ) ) ;
#90773 = CARTESIAN_POINT ( 'NONE',  ( 183.0325607505932624, 280.7969938308983160, 17.10607354250000967 ) ) ;
#90774 = CARTESIAN_POINT ( 'NONE',  ( 157.6500260163024620, 257.5891404556457474, -18.23450497588216379 ) ) ;
#90775 = CARTESIAN_POINT ( 'NONE',  ( 192.8720113526765374, 268.2812397856054645, 12.55819112576203977 ) ) ;
#90776 = CARTESIAN_POINT ( 'NONE',  ( 28.02677306626161879, 24.38052372038642091, 10.00000000000000533 ) ) ;
#90777 = CARTESIAN_POINT ( 'NONE',  ( 82.07265110639774264, 53.99302234254209054, 15.59308437138325587 ) ) ;
#90778 = CARTESIAN_POINT ( 'NONE',  ( 71.35865581505748878, 223.5530062829863027, -4.648177544792955347E-16 ) ) ;
#90779 = DIRECTION ( 'NONE',  ( 0.1548189829846108034, -0.9879428538673736826, 0.000000000000000000 ) ) ;
#90780 = CARTESIAN_POINT ( 'NONE',  ( 159.5284711081640125, 254.3355781173132755, 15.34104435652608522 ) ) ;
#90781 = VECTOR ( 'NONE', #100012, 1000.000000000000114 ) ;
#90782 = CARTESIAN_POINT ( 'NONE',  ( 71.88142767616335504, 71.70553083785841864, -3.832731862061182326 ) ) ;
#90783 = CARTESIAN_POINT ( 'NONE',  ( -0.5819415548772214342, 158.2202760586659736, -5.415160957724236172E-17 ) ) ;
#90784 = CARTESIAN_POINT ( 'NONE',  ( 175.1877765885950851, 284.8709350377350233, -12.04777258482997659 ) ) ;
#90785 = EDGE_LOOP ( 'NONE', ( #13776, #82404, #19605, #19778 ) ) ;
#90786 = CARTESIAN_POINT ( 'NONE',  ( 67.15201250546462575, 67.74620447341509077, -6.543367556292805531 ) ) ;
#90787 = CARTESIAN_POINT ( 'NONE',  ( 73.08131391382630682, 70.69050563043288093, -7.679366471979098385 ) ) ;
#90788 = CARTESIAN_POINT ( 'NONE',  ( 150.6626254231123880, 269.6916732958875969, -15.32062296289003811 ) ) ;
#90789 = CARTESIAN_POINT ( 'NONE',  ( -0.8802452050168975139, 179.4869531367911293, 4.594050593750046652 ) ) ;
#90790 = CARTESIAN_POINT ( 'NONE',  ( 181.5896340430631710, 275.4731096103383265, -16.43232654997619235 ) ) ;
#90791 = CARTESIAN_POINT ( 'NONE',  ( 22.17733255989135088, 35.73705186507754661, -3.090169943749475845 ) ) ;
#90792 = CARTESIAN_POINT ( 'NONE',  ( 85.29796244568555608, 48.43343408700369679, 12.39349753750686034 ) ) ;
#90793 = CARTESIAN_POINT ( 'NONE',  ( 157.5487431480040925, 257.7645675294749594, -18.29554785922338311 ) ) ;
#90794 = CARTESIAN_POINT ( 'NONE',  ( 72.03718002748324523, 71.77198201402653410, -3.924036090042733349 ) ) ;
#90795 = CARTESIAN_POINT ( 'NONE',  ( 149.8677590727400855, 277.0051387818008948, 4.638989373348268330 ) ) ;
#90797 = CARTESIAN_POINT ( 'NONE',  ( 73.97708595465037718, 203.5177522451417929, 5.000000000000051514 ) ) ;
#90796 = DIRECTION ( 'NONE',  ( 0.9738769792773321887, 0.2270762630343793331, 0.000000000000000000 ) ) ;
#90798 = FACE_OUTER_BOUND ( 'NONE', #92355, .T. ) ;
#90799 = CARTESIAN_POINT ( 'NONE',  ( 198.3791677596651368, 287.0441976074670833, 16.95474403075850134 ) ) ;
#90800 = CARTESIAN_POINT ( 'NONE',  ( 65.47921168356349142, 198.6115022471902023, -5.000000000000041744 ) ) ;
#90801 = CARTESIAN_POINT ( 'NONE',  ( 69.81582973455007846, 63.14295414310246457, -13.67321376818635059 ) ) ;
#90802 = CARTESIAN_POINT ( 'NONE',  ( -19.65312891409030271, 93.06504152958497400, -10.00000000000000888 ) ) ;
#90803 = CARTESIAN_POINT ( 'NONE',  ( 12.11013585174968554, 186.9869531367911293, 4.594050593750046652 ) ) ;
#90804 = CARTESIAN_POINT ( 'NONE',  ( 168.0810693606937605, 286.6467868267807830, 4.970377858261654680 ) ) ;
#90805 = CARTESIAN_POINT ( 'NONE',  ( 13.97105408662886461, 167.3262482093458061, -5.229199737892075682E-14 ) ) ;
#90806 = CARTESIAN_POINT ( 'NONE',  ( 43.17480782474465428, 33.43085787977766898, -9.188101187500008038 ) ) ;
#90807 = CARTESIAN_POINT ( 'NONE',  ( 172.3741624485570867, 252.4865239976215037, 8.880853820034850798 ) ) ;
#90808 = EDGE_CURVE ( 'NONE', #19784, #99484, #1529, .T. ) ;
#90809 = CARTESIAN_POINT ( 'NONE',  ( 165.0437781805843258, 244.7827860485373606, -2.050141714668513693 ) ) ;
#90810 = CARTESIAN_POINT ( 'NONE',  ( 185.2207215791545707, 266.7315570652577321, 13.46751314241562447 ) ) ;
#90811 = CARTESIAN_POINT ( 'NONE',  ( -46.74660806181546491, 29.87360136034012825, -10.00000000000000000 ) ) ;
#90812 = CARTESIAN_POINT ( 'NONE',  ( 163.0000163990417548, 280.9966438126449475, 8.877784272329016346 ) ) ;
#90813 = SHAPE_DEFINITION_REPRESENTATION ( #87215, #46310 ) ;
#90814 = CARTESIAN_POINT ( 'NONE',  ( 16.25825050073692069, 15.10170272979925876, -7.433330006724141015 ) ) ;
#90815 = CARTESIAN_POINT ( 'NONE',  ( 165.0258157087664870, 286.3787970787498125, -0.1841640296008903166 ) ) ;
#90816 = CARTESIAN_POINT ( 'NONE',  ( 82.98423510826575011, 53.52344736239028578, 15.67380116644084076 ) ) ;
#90817 = CARTESIAN_POINT ( 'NONE',  ( 71.40044295081541748, 59.41588353585593296, 15.70283061017000925 ) ) ;
#90818 = DIRECTION ( 'NONE',  ( -0.8660254037844387076, -0.4999999999999998890, -0.000000000000000000 ) ) ;
#90819 = ORIENTED_EDGE ( 'NONE', *, *, #67001, .T. ) ;
#90820 = CARTESIAN_POINT ( 'NONE',  ( 85.97213429613141500, 45.53948383454844873, -8.355993802508837831 ) ) ;
#90821 = CARTESIAN_POINT ( 'NONE',  ( 173.4877205307014378, 258.6818873298753374, 14.30620870653597976 ) ) ;
#90822 = CARTESIAN_POINT ( 'NONE',  ( 81.40724292810348572, 41.99019188331313757, 7.748015485544303971 ) ) ;
#90823 = EDGE_CURVE ( 'NONE', #78334, #11388, #63241, .T. ) ;
#90824 = EDGE_LOOP ( 'NONE', ( #59040, #81033, #40341, #61523 ) ) ;
#90825 = CARTESIAN_POINT ( 'NONE',  ( 195.3624787578944222, 290.3824063481519602, -16.76522224015156226 ) ) ;
#90826 = CARTESIAN_POINT ( 'NONE',  ( 80.63465624979117763, 207.3615022471901739, 5.000000000000051514 ) ) ;
#90827 = B_SPLINE_CURVE_WITH_KNOTS ( 'NONE', 3,
 ( #7909, #38784, #62073, #2316, #73213, #63592, #24587, #94533, #26605, #40772 ),
 .UNSPECIFIED., .F., .F.,
 ( 4, 2, 2, 2, 4 ),
 ( 0.001461773093899133673, 0.001796020748610993242, 0.002130268403322852812, 0.002464516058034712381, 0.002798763712746571951 ),
 .UNSPECIFIED. ) ;
#90828 = CARTESIAN_POINT ( 'NONE',  ( 38.13144443662678640, 88.76639304957403453, 59.99999999999999289 ) ) ;
#90829 = EDGE_CURVE ( 'NONE', #22676, #24509, #98315, .T. ) ;
#90830 = CARTESIAN_POINT ( 'NONE',  ( 203.3349860717029571, 278.4604684979374838, -16.59553970625579566 ) ) ;
#90831 = ORIENTED_EDGE ( 'NONE', *, *, #91408, .T. ) ;
#90832 = ORIENTED_EDGE ( 'NONE', *, *, #27080, .T. ) ;
#90834 = CARTESIAN_POINT ( 'NONE',  ( 164.2297246530060875, 246.1927681183832988, 5.803160395959773510 ) ) ;
#90833 = CARTESIAN_POINT ( 'NONE',  ( 187.3286608096677526, 272.3913705820498308, -16.85577171651204154 ) ) ;
#90835 = CARTESIAN_POINT ( 'NONE',  ( 192.0712386031329686, 297.9698513971258649, 12.12276320360788873 ) ) ;
#90836 = ORIENTED_EDGE ( 'NONE', *, *, #6838, .T. ) ;
#90837 = CARTESIAN_POINT ( 'NONE',  ( 190.8264243556038195, 300.1259329198319961, 8.466983560044813117 ) ) ;
#90838 = CARTESIAN_POINT ( 'NONE',  ( 31.70419723673859025, 18.70852965304479909, 1.583844403245330712 ) ) ;
#90839 = DIRECTION ( 'NONE',  ( 0.000000000000000000, 0.000000000000000000, 1.000000000000000000 ) ) ;
#90840 = CARTESIAN_POINT ( 'NONE',  ( 13.43400709863221820, 31.08381733381234469, -10.00000000000000000 ) ) ;
#90841 = VERTEX_POINT ( 'NONE', #44573 ) ;
#90842 = CARTESIAN_POINT ( 'NONE',  ( 87.43441255672811963, 45.02171211745687884, -6.109614425055893250 ) ) ;
#90843 = CARTESIAN_POINT ( 'NONE',  ( 196.9728329903666122, 289.4800408803428695, -17.53478045286815856 ) ) ;
#90844 = CARTESIAN_POINT ( 'NONE',  ( 81.11499192049835472, 43.08689460941847926, 9.540678225713152827 ) ) ;
#90845 = ORIENTED_EDGE ( 'NONE', *, *, #71455, .T. ) ;
#90846 = CARTESIAN_POINT ( 'NONE',  ( 206.0691053506789387, 273.7248349927971844, 11.70564474658248422 ) ) ;
#90847 = CARTESIAN_POINT ( 'NONE',  ( 74.96484514675771038, 65.34853496422127250, 13.65623017033944997 ) ) ;
#90848 = ORIENTED_EDGE ( 'NONE', *, *, #19494, .F. ) ;
#90849 = CARTESIAN_POINT ( 'NONE',  ( 174.4171900096681327, 277.1582007793262505, -15.66121359032516658 ) ) ;
#90850 = CARTESIAN_POINT ( 'NONE',  ( 172.3180150275962603, 263.6756876961334797, -15.46435045179676671 ) ) ;
#90851 = VERTEX_POINT ( 'NONE', #83635 ) ;
#90852 = CARTESIAN_POINT ( 'NONE',  ( 158.9933333928889851, 275.2344634518124167, -12.53406194300261767 ) ) ;
#90853 = DIRECTION ( 'NONE',  ( -0.7763215174174871169, 0.6303371332823493045, 0.000000000000000000 ) ) ;
#90854 = LINE ( 'NONE', #6700, #48298 ) ;
#90855 = ORIENTED_EDGE ( 'NONE', *, *, #68950, .T. ) ;
#90856 = CIRCLE ( 'NONE', #60049, 49.99999999999999289 ) ;
#90857 = ORIENTED_EDGE ( 'NONE', *, *, #36055, .T. ) ;
#90858 = EDGE_CURVE ( 'NONE', #41051, #31813, #61003, .T. ) ;
#90859 = CARTESIAN_POINT ( 'NONE',  ( 73.65729962767424865, 69.49757902785616182, 9.740712345197151123 ) ) ;
#90860 = CARTESIAN_POINT ( 'NONE',  ( 190.8545714895799392, 300.0771806536980648, -5.516553996882049837 ) ) ;
#90861 = CARTESIAN_POINT ( 'NONE',  ( 82.56035143084491779, 53.86840602817222390, 15.84327991562211757 ) ) ;
#90862 = CARTESIAN_POINT ( 'NONE',  ( 19.62422909362874535, 11.73415679381821342, 1.333680081654574804E-15 ) ) ;
#90863 = CARTESIAN_POINT ( 'NONE',  ( 153.4242699508872647, 264.9083646613370320, 16.62000820703435267 ) ) ;
#90864 = CARTESIAN_POINT ( 'NONE',  ( 191.8082373951299076, 298.4253828518392879, 9.404421445770532628 ) ) ;
#90865 = CARTESIAN_POINT ( 'NONE',  ( 147.2229325088103735, 275.6493961858936927, -0.4918294119671829390 ) ) ;
#90866 = ORIENTED_EDGE ( 'NONE', *, *, #39194, .T. ) ;
#90867 = EDGE_CURVE ( 'NONE', #79855, #57805, #11231, .T. ) ;
#90868 = CARTESIAN_POINT ( 'NONE',  ( 73.48578390778760649, 58.20067181093861564, -15.80716316672890009 ) ) ;
#90869 = CARTESIAN_POINT ( 'NONE',  ( 30.67947171958994090, 41.21091486745863364, -1.111400068045478839E-16 ) ) ;
#90871 = CARTESIAN_POINT ( 'NONE',  ( 67.88685699899777148, 70.31731532184431899, 0.4175378299487736422 ) ) ;
#90870 = CARTESIAN_POINT ( 'NONE',  ( 197.0313051377892748, 289.3787641501790517, -17.15509075150697882 ) ) ;
#90872 = CARTESIAN_POINT ( 'NONE',  ( 47.83996289752659692, 111.6306699247848968, -10.00000000000000000 ) ) ;
#90873 = CARTESIAN_POINT ( 'NONE',  ( 167.6323876601624647, 287.4389059340153381, 3.681410875200846089 ) ) ;
#90874 = CARTESIAN_POINT ( 'NONE',  ( -22.42236680055709641, 157.8615022471902591, 0.000000000000000000 ) ) ;
#90875 = ORIENTED_EDGE ( 'NONE', *, *, #3534, .F. ) ;
#90876 = CARTESIAN_POINT ( 'NONE',  ( 205.0859877718122561, 268.9368413191317586, -3.038556538008958974 ) ) ;
#90877 = B_SPLINE_CURVE_WITH_KNOTS ( 'NONE', 3,
 ( #84943, #800, #30211, #60590, #61093, #92064, #22613, #309, #70190, #38292, #7399, #39772, #69202, #100128, #23094, #38795, #16003, #54479, #14994, #62086, #6906, #99130, #45403, #29713, #53006, #37795, #53499, #23586, #30714, #46903, #8409, #7921, #78322, #83957, #22113, #15488, #84453, #62584, #39281, #31681, #14521, #24100, #93543, #68699, #54994, #61596 ),
 .UNSPECIFIED., .F., .F.,
 ( 4, 2, 2, 2, 2, 2, 2, 2, 2, 2, 2, 2, 2, 2, 2, 2, 2, 2, 2, 2, 2, 2, 4 ),
 ( 0.0002647527076360194857, 0.001281163540060212573, 0.001789368956272361158, 0.002043471664378435342, 0.002170523018431519055, 0.002297574372484603202, 0.002424625726537686481, 0.002551677080590770627, 0.002805779788696939787, 0.003313985204909353569, 0.004330396037334254856, 0.005346806869759156144, 0.005855012285971683550, 0.006109114994078024448, 0.006363217702184365346, 0.006426743379210956425, 0.006490269056237549239, 0.006553794733264140318, 0.006617320410290732265, 0.006871423118397062754, 0.007379628534609765367, 0.007887833950822469714, 0.008396039367035172327 ),
 .UNSPECIFIED. ) ;
#90878 = CARTESIAN_POINT ( 'NONE',  ( 76.09838423539584085, 54.19830694069673171, -16.08845863169665336 ) ) ;
#90879 = EDGE_CURVE ( 'NONE', #74953, #65613, #62137, .T. ) ;
#90880 = CARTESIAN_POINT ( 'NONE',  ( 202.6932411237282565, 279.0175140182560085, 15.29984597618553543 ) ) ;
#90881 = CARTESIAN_POINT ( 'NONE',  ( 79.70171752247047436, 45.99846658741579120, 12.97553337965657860 ) ) ;
#90882 = CARTESIAN_POINT ( 'NONE',  ( 182.6185197117589212, 284.2352000010978941, -15.00009734104487258 ) ) ;
#90883 = LINE ( 'NONE', #51840, #36933 ) ;
#90884 = EDGE_LOOP ( 'NONE', ( #97826, #49923, #94740, #71710 ) ) ;
#90885 = CARTESIAN_POINT ( 'NONE',  ( 208.3682389855799499, 269.7426187237583690, -1.431169231381201890 ) ) ;
#90886 = CARTESIAN_POINT ( 'NONE',  ( 192.3743613796607406, 267.3190593529452030, 12.60351243473677307 ) ) ;
#90887 = CARTESIAN_POINT ( 'NONE',  ( 164.4440639631384045, 245.8215215431751233, -2.910115319305802029 ) ) ;
#90888 = CARTESIAN_POINT ( 'NONE',  ( 40.63510790894943625, 194.2677522451418781, 10.00000000000009592 ) ) ;
#90889 = CARTESIAN_POINT ( 'NONE',  ( 110.4040191812834735, 243.7369531367911009, -4.594050593750048428 ) ) ;
#90890 = CARTESIAN_POINT ( 'NONE',  ( 180.2260403442535051, 295.0423342771414923, -3.480517403894910711 ) ) ;
#90891 = CYLINDRICAL_SURFACE ( 'NONE', #99845, 17.82106496071139645 ) ;
#90892 = CYLINDRICAL_SURFACE ( 'NONE', #66363, 17.82106496071139645 ) ;
#90893 = DIRECTION ( 'NONE',  ( -0.7071067811865474617, 8.659560562354932858E-17, 0.7071067811865474617 ) ) ;
#90894 = CARTESIAN_POINT ( 'NONE',  ( 37.30632276492696064, 192.3458772461660544, 9.188101187500095079 ) ) ;
#90895 = CARTESIAN_POINT ( 'NONE',  ( 147.6628748529174402, 275.3469524600083105, -3.428921689675848317 ) ) ;
#90896 = ORIENTED_EDGE ( 'NONE', *, *, #82321, .T. ) ;
#90897 = CARTESIAN_POINT ( 'NONE',  ( 48.21858077004885246, 104.0489273421469818, -10.00000000000000000 ) ) ;
#90898 = CARTESIAN_POINT ( 'NONE',  ( 181.8441098414710666, 266.9845076301842823, 15.29841396442351709 ) ) ;
#90899 = CARTESIAN_POINT ( 'NONE',  ( 25.04665064082954729, 185.2677522451418497, 10.00000000000009592 ) ) ;
#90900 = CARTESIAN_POINT ( 'NONE',  ( 190.1635032421960148, 301.2741459696644029, -5.047660290019184259 ) ) ;
#90901 = CARTESIAN_POINT ( 'NONE',  ( 81.66730501177755741, 41.57387089987508944, -5.459456342607252211 ) ) ;
#90902 = CARTESIAN_POINT ( 'NONE',  ( -22.42236680055709641, 157.8615022471902591, 0.000000000000000000 ) ) ;
#90903 = CARTESIAN_POINT ( 'NONE',  ( 179.4099431796017257, 287.9386474004925276, -12.64039063190630685 ) ) ;
#90904 = CARTESIAN_POINT ( 'NONE',  ( 68.59321919598859552, 64.61334443947949069, -12.16043161807688300 ) ) ;
#90905 = CARTESIAN_POINT ( 'NONE',  ( 103.4941184669699936, 223.8927522451417929, 10.00000000000009592 ) ) ;
#90906 = VERTEX_POINT ( 'NONE', #16058 ) ;
#90907 = EDGE_CURVE ( 'NONE', #47085, #52672, #90748, .T. ) ;
#90908 = CARTESIAN_POINT ( 'NONE',  ( 198.4160757083882345, 267.1808215963346242, -8.346050686629251203 ) ) ;
#90909 = B_SPLINE_CURVE_WITH_KNOTS ( 'NONE', 3,
 ( #22074, #5882, #36769, #98608, #29677, #91021, #83415, #44859, #75800, #99585, #6385, #37269, #60552, #68167, #37757, #99093 ),
 .UNSPECIFIED., .F., .F.,
 ( 4, 2, 2, 2, 2, 2, 2, 4 ),
 ( 6.664589960562511959E-17, 0.0003089471551300475966, 0.0006178943102600286232, 0.0009268414653900095956, 0.001235788620519990460, 0.001544735775649971323, 0.001853682930779952404, 0.002471577241040045538 ),
 .UNSPECIFIED. ) ;
#90910 = CARTESIAN_POINT ( 'NONE',  ( 155.4994079124308257, 279.7286834434665366, -1.607709304407256123 ) ) ;
#90911 = CARTESIAN_POINT ( 'NONE',  ( 207.9743173328493526, 270.4249110404894054, -2.481515874287090639 ) ) ;
#90912 = CARTESIAN_POINT ( 'NONE',  ( 8.294124642383250645, 187.8464784336662206, 1.353441290958777327E-15 ) ) ;
#90913 = CARTESIAN_POINT ( 'NONE',  ( 4.767924915890233706, 21.49103043416546654, -8.090169943749479842 ) ) ;
#90914 = CARTESIAN_POINT ( 'NONE',  ( -17.41797074981450777, 104.4091411665443871, 44.55476241542402960 ) ) ;
#90915 = CARTESIAN_POINT ( 'NONE',  ( 71.75564132893636327, 58.72497181799866439, -15.45604496957676233 ) ) ;
#90916 = CARTESIAN_POINT ( 'NONE',  ( 73.23925880138965283, 69.80348372919694100, 9.104443575153400303 ) ) ;
#90918 = CARTESIAN_POINT ( 'NONE',  ( 49.86334402403631572, 211.8464784336661637, 1.353441290958777327E-15 ) ) ;
#90917 = CARTESIAN_POINT ( 'NONE',  ( 174.1338248144772649, 287.3177669875508400, 10.47848546623640686 ) ) ;
#90919 = CARTESIAN_POINT ( 'NONE',  ( 163.9354095869165633, 246.7025367662834014, -7.289870401565430313 ) ) ;
#90920 = CARTESIAN_POINT ( 'NONE',  ( 203.7265596842292439, 276.1056548365280605, 13.24074560745231466 ) ) ;
#90921 = CARTESIAN_POINT ( 'NONE',  ( 70.30840464414876578, 70.04154225169172321, 5.745843947021113785 ) ) ;
#90922 = CARTESIAN_POINT ( 'NONE',  ( 165.0509870607838252, 244.7702999017660375, -2.356357909806504392 ) ) ;
#90923 = ORIENTED_EDGE ( 'NONE', *, *, #1126, .F. ) ;
#90924 = VECTOR ( 'NONE', #59471, 1000.000000000000000 ) ;
#90925 = CARTESIAN_POINT ( 'NONE',  ( 164.4817765375028102, 245.7562014482918755, -6.334578229142199035 ) ) ;
#90926 = CARTESIAN_POINT ( 'NONE',  ( 18.71383987920379255, 171.6115022471901739, -5.000000000000041744 ) ) ;
#90927 = CARTESIAN_POINT ( 'NONE',  ( 164.4963285489318991, 245.7309966251440301, -6.672251175510283794 ) ) ;
#90928 = CARTESIAN_POINT ( 'NONE',  ( 147.0210896547505399, 249.5643266524160140, 9.188101187500095079 ) ) ;
#90929 = CARTESIAN_POINT ( 'NONE',  ( 27.58635055662477953, 24.43085787977765122, -9.188101187500008038 ) ) ;
#90930 = CARTESIAN_POINT ( 'NONE',  ( 206.8387077773648173, 272.3918444881492746, -7.972442346115986567 ) ) ;
#90931 = CARTESIAN_POINT ( 'NONE',  ( 83.63562430374231838, 51.63275018564552710, -14.84107497619760174 ) ) ;
#90932 = CARTESIAN_POINT ( 'NONE',  ( 198.8081898473356262, 282.3983615885804284, -17.60554210735202574 ) ) ;
#90934 = CARTESIAN_POINT ( 'NONE',  ( 74.86935717915280009, 67.14205582119099347, 12.97785457704837775 ) ) ;
#90933 = CARTESIAN_POINT ( 'NONE',  ( 88.42823867725131493, 44.01048851461693801, 2.280060627005670248 ) ) ;
#90935 = CARTESIAN_POINT ( 'NONE',  ( 69.07388362541929894, 64.21813251217939467, 12.04565015971650510 ) ) ;
#90936 = ORIENTED_EDGE ( 'NONE', *, *, #36446, .F. ) ;
#90937 = CARTESIAN_POINT ( 'NONE',  ( 81.70340159412396019, 53.68629051274507447, 15.93867609236433758 ) ) ;
#90938 = CARTESIAN_POINT ( 'NONE',  ( 164.0405267935391294, 246.5204684236636581, 7.644396071283796168 ) ) ;
#90939 = CARTESIAN_POINT ( 'NONE',  ( 70.23041638060261960, 67.14587595898601080, -10.73806474816264434 ) ) ;
#90940 = CARTESIAN_POINT ( 'NONE',  ( 170.3462095380075425, 266.3929324287667555, -17.59993820609288306 ) ) ;
#90941 = CARTESIAN_POINT ( 'NONE',  ( -69.40242143070358338, 43.82067236826411261, -10.00000000000000000 ) ) ;
#90942 = VERTEX_POINT ( 'NONE', #98819 ) ;
#90943 = CARTESIAN_POINT ( 'NONE',  ( 69.72231879373730123, 68.30382478307210192, 8.176497125895556550 ) ) ;
#90944 = DIRECTION ( 'NONE',  ( -0.9515606131578174809, -0.3074612162317687525, 0.000000000000000000 ) ) ;
#90945 = EDGE_CURVE ( 'NONE', #5430, #64025, #6362, .T. ) ;
#90946 = CARTESIAN_POINT ( 'NONE',  ( 148.9346857181035091, 273.2112271305713307, -9.473665380863973695 ) ) ;
#90947 = CARTESIAN_POINT ( 'NONE',  ( 23.40481081636943372, 190.9865022471903160, 10.00000000000009415 ) ) ;
#90948 = CARTESIAN_POINT ( 'NONE',  ( 185.8885322232007979, 296.6982464125469505, 4.785400323938857170 ) ) ;
#90949 = EDGE_CURVE ( 'NONE', #71153, #15777, #62638, .T. ) ;
#90950 = CARTESIAN_POINT ( 'NONE',  ( 149.9706620097691143, 271.4333556379564243, -12.01292532367938293 ) ) ;
#90951 = CARTESIAN_POINT ( 'NONE',  ( 190.4940980602978300, 281.5357392997901798, 17.69179316189531903 ) ) ;
#90952 = CARTESIAN_POINT ( 'NONE',  ( 9.678154728840961951, 27.36126292948894090, 6.180339887498949913 ) ) ;
#90953 = CARTESIAN_POINT ( 'NONE',  ( 192.0403215870056783, 287.5166130765638854, -16.83829816813398139 ) ) ;
#90954 = ORIENTED_EDGE ( 'NONE', *, *, #91136, .T. ) ;
#90955 = CARTESIAN_POINT ( 'NONE',  ( 167.4011299790239775, 281.5488363183706042, 12.98604958840868662 ) ) ;
#90956 = CARTESIAN_POINT ( 'NONE',  ( 86.40784109447328376, 47.52432272822921533, -11.05097720836333330 ) ) ;
#90957 = CARTESIAN_POINT ( 'NONE',  ( 80.45391135454320874, 45.63592357980512304, -11.76834192579569915 ) ) ;
#90958 = EDGE_LOOP ( 'NONE', ( #96551, #92816, #92925 ) ) ;
#90959 = CARTESIAN_POINT ( 'NONE',  ( 146.9235493515124062, 276.1679430252639804, 0.7994986043261682607 ) ) ;
#90960 = CARTESIAN_POINT ( 'NONE',  ( 79.31708208686119121, 59.64451620468177140, -16.52545681491536556 ) ) ;
#90961 = CARTESIAN_POINT ( 'NONE',  ( 164.2059258710715994, 246.2339888178522926, 7.329631442356459914 ) ) ;
#90962 = FACE_OUTER_BOUND ( 'NONE', #46374, .T. ) ;
#90963 = ORIENTED_EDGE ( 'NONE', *, *, #78226, .F. ) ;
#90964 = CARTESIAN_POINT ( 'NONE',  ( 91.83912023130210400, 214.6423013555409796, -4.594050593750043987 ) ) ;
#90965 = CARTESIAN_POINT ( 'NONE',  ( 198.9446342420995109, 283.0329230195785044, 17.26884992386511897 ) ) ;
#90966 = CARTESIAN_POINT ( 'NONE',  ( 68.10710844971850975, 70.39465110784678359, 1.444126812255956516 ) ) ;
#90967 = CARTESIAN_POINT ( 'NONE',  ( 81.82036482997024507, 42.35048943659092657, -7.944650131497826173 ) ) ;
#90968 = ORIENTED_EDGE ( 'NONE', *, *, #46785, .T. ) ;
#90969 = VERTEX_POINT ( 'NONE', #40340 ) ;
#90970 = EDGE_LOOP ( 'NONE', ( #71960, #80120, #25819, #62109 ) ) ;
#90971 = CARTESIAN_POINT ( 'NONE',  ( -19.65312891409030271, 93.06504152958497400, -10.00000000000000888 ) ) ;
#90972 = ORIENTED_EDGE ( 'NONE', *, *, #93523, .T. ) ;
#90973 = CARTESIAN_POINT ( 'NONE',  ( 158.9054571277534649, 258.0742575434156834, 17.39430999040402526 ) ) ;
#90974 = VERTEX_POINT ( 'NONE', #25674 ) ;
#90975 = CARTESIAN_POINT ( 'NONE',  ( 164.5613517958998955, 245.6183730577221809, 2.459055975528789517 ) ) ;
#90976 = EDGE_CURVE ( 'NONE', #38656, #11056, #71279, .T. ) ;
#90977 = CARTESIAN_POINT ( 'NONE',  ( -0.4668637173180778532, 25.74574839753307387, -10.00000000000000000 ) ) ;
#90978 = CARTESIAN_POINT ( 'NONE',  ( -23.39332202855467813, 99.74324603395649547, 45.19937630303414977 ) ) ;
#90979 = CARTESIAN_POINT ( 'NONE',  ( 82.68215287466908592, 53.55713939286302150, -15.73562046651999857 ) ) ;
#90980 = CARTESIAN_POINT ( 'NONE',  ( 156.7370215179966237, 259.1705106342505474, -18.04600119725074947 ) ) ;
#90981 = EDGE_LOOP ( 'NONE', ( #92334, #13428, #38187, #27012 ) ) ;
#90982 = CARTESIAN_POINT ( 'NONE',  ( -76.49344163160107257, 52.20945622995200353, 177.5919119679930134 ) ) ;
#90983 = CARTESIAN_POINT ( 'NONE',  ( 17.99030130830579566, 16.10170272979926054, -7.433330006724141015 ) ) ;
#90984 = ORIENTED_EDGE ( 'NONE', *, *, #9126, .T. ) ;
#90985 = CARTESIAN_POINT ( 'NONE',  ( 166.4301960487401004, 284.1355213801691093, 9.513592484950153860 ) ) ;
#90987 = ORIENTED_EDGE ( 'NONE', *, *, #72048, .F. ) ;
#90986 = CARTESIAN_POINT ( 'NONE',  ( 20.18783944447021383, 170.9155109091896065, 2.679491924311254714 ) ) ;
#90988 = CARTESIAN_POINT ( 'NONE',  ( 163.4260108471723640, 247.5848412648317662, 10.45113099391573108 ) ) ;
#90989 = CARTESIAN_POINT ( 'NONE',  ( 185.1149126255429849, 258.5007932025994819, 2.939304387390308193 ) ) ;
#90990 = CARTESIAN_POINT ( 'NONE',  ( 161.2113459091177674, 281.3599108807870834, -6.589518380948089948 ) ) ;
#90991 = CARTESIAN_POINT ( 'NONE',  ( 165.8064460562817430, 246.4435469418012588, -2.717970023973333316 ) ) ;
#90992 = CARTESIAN_POINT ( 'NONE',  ( 157.4718321624326620, 258.3312158842189774, 16.78309831726782164 ) ) ;
#90993 = CARTESIAN_POINT ( 'NONE',  ( 172.0630936339023265, 254.4764114392720273, 11.54978638049990103 ) ) ;
#90994 = CARTESIAN_POINT ( 'NONE',  ( 158.2761760943415652, 281.1697532028657065, 2.074752331550637319 ) ) ;
#90995 = ORIENTED_EDGE ( 'NONE', *, *, #16899, .F. ) ;
#90996 = DIRECTION ( 'NONE',  ( 0.000000000000000000, -0.000000000000000000, -1.000000000000000000 ) ) ;
#90997 = CARTESIAN_POINT ( 'NONE',  ( 72.74372184067405556, 62.96568689615059355, -14.16853096237499798 ) ) ;
#90998 = CARTESIAN_POINT ( 'NONE',  ( 160.2308819960220490, 276.4003654746809957, 12.70007076641597088 ) ) ;
#90999 = CARTESIAN_POINT ( 'NONE',  ( 13.42747647338834760, 171.8927522451418213, -10.00000000000009059 ) ) ;
#91000 = CARTESIAN_POINT ( 'NONE',  ( -65.00000000000000000, 18.66025403784439973, 54.99999999999999289 ) ) ;
#91001 = DIRECTION ( 'NONE',  ( -1.000000000000000000, 0.000000000000000000, 0.000000000000000000 ) ) ;
#91002 = CARTESIAN_POINT ( 'NONE',  ( 164.0644709900060718, 246.4789958588364698, -8.616711260302015063 ) ) ;
#91003 = LINE ( 'NONE', #59536, #76916 ) ;
#91004 = ADVANCED_FACE ( 'NONE', ( #56555, #95621 ), #48467, .F. ) ;
#91005 = CARTESIAN_POINT ( 'NONE',  ( 164.6506446267413253, 274.3553168417332131, 14.79851574671830505 ) ) ;
#91006 = CARTESIAN_POINT ( 'NONE',  ( 4.289451341410244645, 161.0327760586659451, 1.948934522072303157E-15 ) ) ;
#91007 = CARTESIAN_POINT ( 'NONE',  ( 189.0750166644107821, 297.0310844892443356, 8.177982547853755335 ) ) ;
#91008 = ORIENTED_EDGE ( 'NONE', *, *, #67834, .T. ) ;
#91009 = VERTEX_POINT ( 'NONE', #80411 ) ;
#91010 = CARTESIAN_POINT ( 'NONE',  ( 198.7134558283731280, 282.8386145195935910, 17.66748989068429054 ) ) ;
#91011 = LINE ( 'NONE', #98596, #25380 ) ;
#91012 = CARTESIAN_POINT ( 'NONE',  ( 174.7639949172803995, 290.4895449553895901, 2.562946516734061930 ) ) ;
#91013 = CARTESIAN_POINT ( 'NONE',  ( -71.61465314115659453, 63.06504152958490295, 40.00000000000000000 ) ) ;
#91014 = DIRECTION ( 'NONE',  ( -0.8660254037844382635, -0.5000000000000006661, 0.000000000000000000 ) ) ;
#91015 = CARTESIAN_POINT ( 'NONE',  ( -13.11024591527734628, 6.000000000000000000, -45.00000000000000000 ) ) ;
#91016 = CARTESIAN_POINT ( 'NONE',  ( 153.2019974609038115, 278.5196124964878095, 3.744932174532282332 ) ) ;
#91017 = CARTESIAN_POINT ( 'NONE',  ( 22.39418752168989712, 192.9244531367911293, -4.594050593750046652 ) ) ;
#91018 = CARTESIAN_POINT ( 'NONE',  ( 106.6962611473900893, 244.6589784336661069, -6.496448406907675876E-16 ) ) ;
#91019 = CARTESIAN_POINT ( 'NONE',  ( 40.18174127881769664, 205.5530062829863027, -4.648177544792955347E-16 ) ) ;
#91020 = CARTESIAN_POINT ( 'NONE',  ( 183.7400870242638860, 256.7387704515565474, -3.095244190633015702 ) ) ;
#91021 = CARTESIAN_POINT ( 'NONE',  ( 206.4069886254544031, 272.1500834713139625, -7.842899504808422684 ) ) ;
#91022 = LINE ( 'NONE', #60059, #58191 ) ;
#91023 = AXIS2_PLACEMENT_3D ( 'NONE', #10289, #1190, #56372 ) ;
#91024 = CARTESIAN_POINT ( 'NONE',  ( 80.00195504689109782, 53.61111274759718981, -15.70840541018166725 ) ) ;
#91025 = CARTESIAN_POINT ( 'NONE',  ( 154.8989000222956349, 262.3542304552891551, 17.41779271305265908 ) ) ;
#91026 = CARTESIAN_POINT ( 'NONE',  ( 207.7320178805681508, 270.8445860024863237, -5.379955943374661764 ) ) ;
#91027 = LINE ( 'NONE', #7886, #46741 ) ;
#91028 = CARTESIAN_POINT ( 'NONE',  ( -19.79358564147677413, 93.04540364847184719, 59.99999999999999289 ) ) ;
#91029 = CARTESIAN_POINT ( 'NONE',  ( 85.04793144752866851, 49.76842598555752062, 13.42690168825988373 ) ) ;
#91030 = CARTESIAN_POINT ( 'NONE',  ( 196.6001939379022758, 266.5684052957021208, 8.222072963770980181 ) ) ;
#91031 = CARTESIAN_POINT ( 'NONE',  ( 198.5725620961998459, 266.5936579278944691, -7.138590148556124504 ) ) ;
#91032 = CARTESIAN_POINT ( 'NONE',  ( 164.0412359135344786, 252.8541476746656826, -12.95066152372220536 ) ) ;
#91033 = LINE ( 'NONE', #74822, #59388 ) ;
#91034 = DIRECTION ( 'NONE',  ( -0.000000000000000000, -0.000000000000000000, -1.000000000000000000 ) ) ;
#91035 = CARTESIAN_POINT ( 'NONE',  ( 101.7984123748231298, 220.3923013555410080, 4.594050593750050204 ) ) ;
#91036 = CARTESIAN_POINT ( 'NONE',  ( 2.730238736670422384, 24.68290643055184574, 3.479690158560446702E-15 ) ) ;
#91037 = CARTESIAN_POINT ( 'NONE',  ( 150.6453220160077251, 269.7216436761371483, 14.94145576020818034 ) ) ;
#91038 = LINE ( 'NONE', #21606, #56257 ) ;
#91039 = VECTOR ( 'NONE', #22541, 999.9999999999998863 ) ;
#91041 = CARTESIAN_POINT ( 'NONE',  ( 83.30611589712688669, 42.09688407475692884, -4.353475907038308890 ) ) ;
#91040 = CARTESIAN_POINT ( 'NONE',  ( 157.5042325173297684, 257.8416622032797818, 16.70595240278738203 ) ) ;
#91042 = CARTESIAN_POINT ( 'NONE',  ( 191.2622316156482043, 288.8574828335728171, -16.55244734589887656 ) ) ;
#91043 = CARTESIAN_POINT ( 'NONE',  ( 164.8075539017095252, 280.4672370525465226, 12.63796469268613265 ) ) ;
#91044 = CARTESIAN_POINT ( 'NONE',  ( 80.55977923466276991, 44.53388773495298381, 11.41474457630165062 ) ) ;
#91045 = CARTESIAN_POINT ( 'NONE',  ( 40.97001837269192492, 24.44966523072497466, -2.296566073217252530E-15 ) ) ;
#91046 = CARTESIAN_POINT ( 'NONE',  ( 146.9700173529739970, 276.0874580858064746, -5.099093031535578469 ) ) ;
#91047 = LINE ( 'NONE', #74836, #75034 ) ;
#91048 = EDGE_LOOP ( 'NONE', ( #20686, #38584, #50787, #88914 ) ) ;
#91049 = CARTESIAN_POINT ( 'NONE',  ( 18.86656744736070124, 32.93396525600390845, 2.839279412974139660 ) ) ;
#91050 = DIRECTION ( 'NONE',  ( 0.4999999999999998890, -0.8660254037844385966, 0.000000000000000000 ) ) ;
#91051 = CARTESIAN_POINT ( 'NONE',  ( 147.2567621633200474, 275.5908015054806128, -3.647191014543873955 ) ) ;
#91052 = CARTESIAN_POINT ( 'NONE',  ( 149.4171629335945681, 271.8488776066536730, -11.42564036194071520 ) ) ;
#91053 = ORIENTED_EDGE ( 'NONE', *, *, #86995, .F. ) ;
#91054 =( BOUNDED_CURVE ( )  B_SPLINE_CURVE ( 2, ( #74154, #34147, #34629, #97457, #42710, #4746, #35630, #67018, #96479, #66530, #27047, #96982, #80283 ),
 .UNSPECIFIED., .F., .T. ) 
 B_SPLINE_CURVE_WITH_KNOTS ( ( 3, 2, 2, 2, 2, 2, 3 ),
 ( 0.1875000000000000000, 0.1900000000000000022, 0.1950000000000000067, 0.2000000000000000111, 0.2049999999999999878, 0.2099999999999999922, 0.2124999999999999944 ),
 .UNSPECIFIED. ) 
 CURVE ( )  GEOMETRIC_REPRESENTATION_ITEM ( )  RATIONAL_B_SPLINE_CURVE ( ( 0.9755282581475768211, 0.9755282581475768211, 1.000000000000000000, 0.9510565162951535312, 1.000000000000000000, 0.9510565162951535312, 1.000000000000000000, 0.9510565162951535312, 1.000000000000000000, 0.9510565162951535312, 1.000000000000000000, 0.9755282581475768211, 0.9755282581475768211 ) ) 
 REPRESENTATION_ITEM ( '' )  );
#91055 = EDGE_CURVE ( 'NONE', #18962, #52455, #8959, .T. ) ;
#91056 = CARTESIAN_POINT ( 'NONE',  ( 70.96429761874149733, 61.15374941682173926, 14.99935025261083688 ) ) ;
#91057 = CARTESIAN_POINT ( 'NONE',  ( 198.3075590527773784, 287.1682275260610027, 16.94807365630277118 ) ) ;
#91058 = CARTESIAN_POINT ( 'NONE',  ( 73.72587696377917155, 59.63361033315440807, 16.00582498373660556 ) ) ;
#91059 = EDGE_CURVE ( 'NONE', #59369, #52500, #86028, .T. ) ;
#91060 = CARTESIAN_POINT ( 'NONE',  ( 48.83428215874787526, 87.09189275153327969, -10.00000000000000000 ) ) ;
#91061 = CARTESIAN_POINT ( 'NONE',  ( 133.0291931787496651, 247.6115022471902591, 10.00000000000009592 ) ) ;
#91062 = ORIENTED_EDGE ( 'NONE', *, *, #1004, .T. ) ;
#91063 = CARTESIAN_POINT ( 'NONE',  ( 71.62510740771190854, 67.51121758376429227, 11.15861874543539400 ) ) ;
#91064 = VERTEX_POINT ( 'NONE', #56035 ) ;
#91065 = LINE ( 'NONE', #66235, #4563 ) ;
#91066 = CARTESIAN_POINT ( 'NONE',  ( 84.39844661083043320, 42.18200899752556410, 2.226954688809204885 ) ) ;
#91067 = EDGE_CURVE ( 'NONE', #1734, #65735, #57047, .T. ) ;
#91068 = ORIENTED_EDGE ( 'NONE', *, *, #66648, .T. ) ;
#91069 = CARTESIAN_POINT ( 'NONE',  ( 185.3093006960060336, 292.6213584219709105, -10.65003670060383101 ) ) ;
#91070 = VERTEX_POINT ( 'NONE', #10982 ) ;
#91071 = FACE_OUTER_BOUND ( 'NONE', #2602, .T. ) ;
#91072 = CARTESIAN_POINT ( 'NONE',  ( 205.5340210668974237, 274.6516281586387436, 11.25376706788097714 ) ) ;
#91073 = CARTESIAN_POINT ( 'NONE',  ( 190.6012238204759228, 278.5005121819996816, -16.53506780650642582 ) ) ;
#91074 = CARTESIAN_POINT ( 'NONE',  ( 154.0631780868778264, 263.8017433084320942, -17.71705682590848951 ) ) ;
#91075 = CARTESIAN_POINT ( 'NONE',  ( 152.7375212135632125, 266.0978483664162582, -16.47968945089317572 ) ) ;
#91076 = CARTESIAN_POINT ( 'NONE',  ( 35.86231599663030067, 42.74646525600393687, 2.839279412974139660 ) ) ;
#91077 = CARTESIAN_POINT ( 'NONE',  ( 194.4572733120733119, 265.4698506025051188, 9.231589761896536572 ) ) ;
#91078 = CARTESIAN_POINT ( 'NONE',  ( 77.42588836629299465, 61.59288719192012707, -16.04997787272938936 ) ) ;
#91079 = CARTESIAN_POINT ( 'NONE',  ( 85.93470712620026575, 48.23248545518190866, 11.93606436224419376 ) ) ;
#91080 = VERTEX_POINT ( 'NONE', #41852 ) ;
#91081 = ORIENTED_EDGE ( 'NONE', *, *, #64611, .F. ) ;
#91082 = CARTESIAN_POINT ( 'NONE',  ( 198.1186603539670728, 286.9451690787467442, 16.94706959193672446 ) ) ;
#91083 = DIRECTION ( 'NONE',  ( 0.7713975076906463002, 0.000000000000000000, 0.6363535849892411056 ) ) ;
#91085 = CARTESIAN_POINT ( 'NONE',  ( 162.5812530041002049, 272.3672700969655693, -15.68205036963906807 ) ) ;
#91084 = CARTESIAN_POINT ( 'NONE',  ( 174.0349010169910287, 257.2697708657194084, -11.84118670213688240 ) ) ;
#91086 = FACE_OUTER_BOUND ( 'NONE', #27545, .T. ) ;
#91087 = CARTESIAN_POINT ( 'NONE',  ( 197.4226313177773591, 273.1407988583247288, -13.32284819095123751 ) ) ;
#91088 = CARTESIAN_POINT ( 'NONE',  ( 156.4445880091442120, 261.3333284696779515, -17.64838406174382612 ) ) ;
#91089 = CARTESIAN_POINT ( 'NONE',  ( 190.3691966041315311, 300.9178746160123410, 0.1783449565851275009 ) ) ;
#91090 = CARTESIAN_POINT ( 'NONE',  ( 169.7116465267147873, 287.0218441930870199, -4.634240893799990602 ) ) ;
#91091 = CARTESIAN_POINT ( 'NONE',  ( 77.31293068221884823, 63.17731889312780424, -15.23105203122446838 ) ) ;
#91092 = CARTESIAN_POINT ( 'NONE',  ( 186.3888140740535562, 286.9988348145756163, -16.10978017299487064 ) ) ;
#91093 = CARTESIAN_POINT ( 'NONE',  ( 112.2989703957094605, 226.4548013555409796, -4.594050593750042211 ) ) ;
#91094 = CARTESIAN_POINT ( 'NONE',  ( 83.67416965427615594, 41.61942911856458949, 0.1873010706438003881 ) ) ;
#91095 = CARTESIAN_POINT ( 'NONE',  ( 27.02885687802902837, 37.64646525600391413, -2.839279412974133887 ) ) ;
#91096 = CARTESIAN_POINT ( 'NONE',  ( 191.9588319567279200, 275.3209462115174233, 16.40384393395227747 ) ) ;
#91097 = ORIENTED_EDGE ( 'NONE', *, *, #33747, .F. ) ;
#91098 = AXIS2_PLACEMENT_3D ( 'NONE', #70303, #77925, #15095 ) ;
#91099 = CARTESIAN_POINT ( 'NONE',  ( 74.05204724713870235, 68.33764315531155376, -11.67956189741113349 ) ) ;
#91100 = VECTOR ( 'NONE', #44283, 1000.000000000000227 ) ;
#91102 = B_SPLINE_SURFACE_WITH_KNOTS ( 'NONE', 3, 1, ( 
 ( #1634, #56802 ),
 ( #72540, #87787 ),
 ( #11238, #42101 ),
 ( #18326, #18821 ),
 ( #49705, #49223 ),
 ( #10721, #73035 ),
 ( #41597, #3146 ),
 ( #34031, #64918 ),
 ( #95863, #26421 ),
 ( #57300, #88272 ),
 ( #31995, #62905 ),
 ( #93857, #24412 ),
 ( #55288, #78628 ),
 ( #40088, #71032 ),
 ( #12219, #89752 ),
 ( #35990, #42587 ),
 ( #11725, #82659 ),
 ( #66895, #26915 ),
 ( #75019, #4103 ),
 ( #90755, #44079 ),
 ( #5110, #50692 ),
 ( #81158, #44577 ),
 ( #98320, #67395 ),
 ( #13222, #28911 ),
 ( #43078, #21307 ),
 ( #74531, #97331 ),
 ( #81647, #19822 ),
 ( #58779, #73520 ),
 ( #57795, #59786 ),
 ( #74021, #5601 ),
 ( #52184, #4609 ),
 ( #88774, #83133 ),
 ( #65898, #12728 ),
 ( #35502, #20318 ) ),
 .UNSPECIFIED., .T., .F., .F.,
 ( 4, 2, 2, 2, 2, 2, 2, 2, 2, 2, 2, 2, 2, 2, 2, 2, 4 ),
 ( 2, 2 ),
 ( 0.000000000000000000, 0.06250000000000000000, 0.1250000000000000000, 0.1875000000000000000, 0.2500000000000000000, 0.3125000000000000000, 0.3750000000000000000, 0.4375000000000000000, 0.5000000000000000000, 0.5625000000000000000, 0.6250000000000000000, 0.6875000000000000000, 0.7500000000000000000, 0.8125000000000000000, 0.8750000000000000000, 0.9375000000000000000, 1.000000000000000000 ),
 ( 0.000000000000000000, 1.000000000000000000 ),
 .UNSPECIFIED. ) ;
#91101 = CARTESIAN_POINT ( 'NONE',  ( -31.49356256989596758, 94.88921800892812541, 45.19948692389422717 ) ) ;
#91103 = CARTESIAN_POINT ( 'NONE',  ( 157.1606030646430554, 258.4368458743103361, 17.96998724893680688 ) ) ;
#91104 = CARTESIAN_POINT ( 'NONE',  ( 27.28458541428561901, 34.49103043416550918, -8.090169943749479842 ) ) ;
#91105 = CARTESIAN_POINT ( 'NONE',  ( -22.42236680055709641, 157.8615022471902591, 0.000000000000000000 ) ) ;
#91106 = ORIENTED_EDGE ( 'NONE', *, *, #69177, .T. ) ;
#91107 = CARTESIAN_POINT ( 'NONE',  ( 195.3286257065703069, 292.3278914340530719, 16.60614309818382495 ) ) ;
#91108 = ORIENTED_EDGE ( 'NONE', *, *, #99405, .T. ) ;
#91109 = CARTESIAN_POINT ( 'NONE',  ( -17.26243516413818924, 24.35187462261283997, 10.00000000000000000 ) ) ;
#91110 = ORIENTED_EDGE ( 'NONE', *, *, #45619, .T. ) ;
#91111 = CARTESIAN_POINT ( 'NONE',  ( 206.5117639185820906, 272.9581278627833285, 11.28485531511759099 ) ) ;
#91112 = CIRCLE ( 'NONE', #13500, 10.00000000000011369 ) ;
#91113 = CARTESIAN_POINT ( 'NONE',  ( 194.8492499382162180, 264.8919437935018664, 4.416793385568180241 ) ) ;
#91114 = CARTESIAN_POINT ( 'NONE',  ( 177.5879455283492234, 272.4518736442240083, -17.80684084945183088 ) ) ;
#91115 = EDGE_CURVE ( 'NONE', #94946, #59130, #66812, .T. ) ;
#91116 = CARTESIAN_POINT ( 'NONE',  ( 67.79268864257714711, 69.02054886865253991, -4.467901244201882172 ) ) ;
#91118 = CARTESIAN_POINT ( 'NONE',  ( 70.00592750416963383, 62.80307869517519492, -13.36220121966311858 ) ) ;
#91117 = CARTESIAN_POINT ( 'NONE',  ( 65.82437655349816907, 69.12761348810168727, -0.3171013769033966812 ) ) ;
#91119 = FACE_OUTER_BOUND ( 'NONE', #81026, .T. ) ;
#91120 = EDGE_LOOP ( 'NONE', ( #16142, #73615, #47642, #34479 ) ) ;
#91122 = CARTESIAN_POINT ( 'NONE',  ( 82.15383659063220989, 50.27708431210408691, 14.14486460422176073 ) ) ;
#91121 = B_SPLINE_SURFACE_WITH_KNOTS ( 'NONE', 3, 1, ( 
 ( #33354, #71875 ),
 ( #78989, #31348 ),
 ( #63756, #16154 ),
 ( #54632, #16650 ),
 ( #2473, #94689 ),
 ( #92690, #24748 ),
 ( #17148, #23241 ),
 ( #47052, #39428 ),
 ( #48046, #54128 ),
 ( #56133, #15637 ),
 ( #40438, #62738 ),
 ( #17663, #8065 ),
 ( #62231, #93183 ),
 ( #94194, #93694 ),
 ( #71373, #70347 ),
 ( #47545, #31835 ),
 ( #85091, #32352 ),
 ( #24257, #46534 ),
 ( #69845, #1962 ),
 ( #87131, #86120 ),
 ( #32847, #1471 ),
 ( #55134, #39926 ),
 ( #12564, #2990 ),
 ( #33880, #66255 ),
 ( #56649, #58144 ),
 ( #96692, #4446 ),
 ( #3953, #34836 ),
 ( #27261, #43439 ),
 ( #64765, #97190 ),
 ( #89124, #4964 ),
 ( #25774, #35346 ) ),
 .UNSPECIFIED., .F., .F., .F.,
 ( 4, 3, 3, 3, 3, 3, 3, 3, 3, 3, 4 ),
 ( 2, 2 ),
 ( 0.000000000000000000, 0.1122669598086739884, 0.2243161639709730926, 0.3396355846219151764, 0.4553962076585294505, 0.5677860799922427315, 0.6749047109689578772, 0.7773884377078319474, 0.8775581155834339953, 0.9782364162377981120, 1.000000000000000000 ),
 ( 0.000000000000000000, 1.000000000000000000 ),
 .UNSPECIFIED. ) ;
#91123 = CARTESIAN_POINT ( 'NONE',  ( 82.24301957861473511, 40.72317291277653339, -3.636295274160996183 ) ) ;
#91124 = CARTESIAN_POINT ( 'NONE',  ( 192.5458920237629457, 271.5594986157455537, 14.05193011733685005 ) ) ;
#91125 = CARTESIAN_POINT ( 'NONE',  ( 165.0952264510788154, 281.4963861521250124, -11.84807672454148886 ) ) ;
#91126 = CARTESIAN_POINT ( 'NONE',  ( 72.10617024684209753, 72.18421392457030095, 4.031754617348218162 ) ) ;
#91127 = EDGE_CURVE ( 'NONE', #63007, #8285, #25760, .T. ) ;
#91128 = LINE ( 'NONE', #30790, #16182 ) ;
#91129 = DIRECTION ( 'NONE',  ( -0.3374500364938434194, -0.9413434404457831084, 0.000000000000000000 ) ) ;
#91130 = CARTESIAN_POINT ( 'NONE',  ( 70.48822326768343771, 61.33110110675399085, -14.80687757298846918 ) ) ;
#91131 = CARTESIAN_POINT ( 'NONE',  ( 82.61614429202859355, 53.50419195261176242, -15.73127852458025266 ) ) ;
#91132 = CARTESIAN_POINT ( 'NONE',  ( 84.34250105585179824, 213.3768266524160140, 9.188101187500098632 ) ) ;
#91133 = CARTESIAN_POINT ( 'NONE',  ( 159.2394649670193303, 254.8361514374751664, -16.43133403737800791 ) ) ;
#91134 = CARTESIAN_POINT ( 'NONE',  ( -115.0954152546898257, 78.37593066204033221, -30.52142883766496695 ) ) ;
#91135 = CARTESIAN_POINT ( 'NONE',  ( 62.50798602660128012, 180.9153022007868401, 4.041334437186263538E-16 ) ) ;
#91136 = EDGE_CURVE ( 'NONE', #42726, #1733, #75267, .T. ) ;
#91137 = CARTESIAN_POINT ( 'NONE',  ( 66.43435659019957029, 67.91024671103048149, 6.587328651168637528 ) ) ;
#91138 = CARTESIAN_POINT ( 'NONE',  ( 207.1211793645798878, 271.9025893473983047, -6.294110402770905388 ) ) ;
#91139 = DIRECTION ( 'NONE',  ( 0.000000000000000000, -0.000000000000000000, -1.000000000000000000 ) ) ;
#91140 = CARTESIAN_POINT ( 'NONE',  ( -20.88691866978057377, 95.07703167464532612, 45.19944471151773513 ) ) ;
#91141 = CARTESIAN_POINT ( 'NONE',  ( 111.6751914540069635, 246.8297689869268936, -2.679491924311252493 ) ) ;
#91142 = CARTESIAN_POINT ( 'NONE',  ( 38.46077748372666605, 37.90829794293884447, 10.00000000000000355 ) ) ;
#91143 = CARTESIAN_POINT ( 'NONE',  ( 75.04467193377834633, 57.90891680148014586, -16.45096375161649149 ) ) ;
#91144 = CARTESIAN_POINT ( 'NONE',  ( 82.76645177422848576, 53.88639560009900009, 15.44535535711801977 ) ) ;
#91145 = CARTESIAN_POINT ( 'NONE',  ( 72.27859001089517221, 72.07364561169796957, 3.260268701118359758 ) ) ;
#91146 = CARTESIAN_POINT ( 'NONE',  ( 157.5710319558766344, 257.7259621817996162, 18.28704422422941533 ) ) ;
#91147 = CARTESIAN_POINT ( 'NONE',  ( 199.4716132138953242, 277.5915922024631755, 15.21463707318425662 ) ) ;
#91148 = CARTESIAN_POINT ( 'NONE',  ( 79.78357408300404074, 50.66639049700688702, -14.85564821779047229 ) ) ;
#91149 = CARTESIAN_POINT ( 'NONE',  ( 71.67602448659575032, 72.02732272969839755, -1.570697476799420844 ) ) ;
#91150 = CARTESIAN_POINT ( 'NONE',  ( 50.29670382169353360, 199.8458772461660260, 9.188101187500095079 ) ) ;
#91151 = CARTESIAN_POINT ( 'NONE',  ( 17.68238808236222326, 31.18502408145591787, 5.678558825948276656 ) ) ;
#91152 = CARTESIAN_POINT ( 'NONE',  ( 198.8533049117289977, 286.2229679703367538, -18.60939981449148561 ) ) ;
#91153 = CARTESIAN_POINT ( 'NONE',  ( 6.414422030351863313, 19.10171378149916421, 9.188101187500008038 ) ) ;
#91154 = PLANE ( 'NONE',  #85503 ) ;
#91155 = CARTESIAN_POINT ( 'NONE',  ( 202.3081618345277946, 269.6788042618418331, -6.424812278093250839 ) ) ;
#91156 = CARTESIAN_POINT ( 'NONE',  ( 76.05950007140947378, 59.49804724808203815, 16.31946239994518777 ) ) ;
#91157 = EDGE_LOOP ( 'NONE', ( #11328, #17676, #48019, #13658 ) ) ;
#91158 = CARTESIAN_POINT ( 'NONE',  ( 72.64134535439403351, 61.55457294482811648, 14.72326246863772781 ) ) ;
#91159 = CARTESIAN_POINT ( 'NONE',  ( 153.0558112840829210, 276.6942330888239212, 7.179448329669019024 ) ) ;
#91160 = EDGE_CURVE ( 'NONE', #17251, #93568, #98280, .T. ) ;
#91161 = CARTESIAN_POINT ( 'NONE',  ( 163.7892944603517833, 255.0961238338549322, -15.29376416924185556 ) ) ;
#91162 = VECTOR ( 'NONE', #99362, 1000.000000000000000 ) ;
#91163 = DIRECTION ( 'NONE',  ( 0.9291732088853837945, -0.3696446237802449297, 0.000000000000000000 ) ) ;
#91164 = CARTESIAN_POINT ( 'NONE',  ( 87.49069069641790009, 227.9865022471902876, -10.00000000000009415 ) ) ;
#91165 = CARTESIAN_POINT ( 'NONE',  ( 182.9360775077161918, 292.9515156215683760, -10.62356958548592445 ) ) ;
#91166 = DIRECTION ( 'NONE',  ( -0.7071067811865462405, 8.659560562354915602E-17, 0.7071067811865489050 ) ) ;
#91167 = EDGE_LOOP ( 'NONE', ( #40215, #29366, #4312, #28718 ) ) ;
#91168 = AXIS2_PLACEMENT_3D ( 'NONE', #84931, #78813, #24090 ) ;
#91169 = CARTESIAN_POINT ( 'NONE',  ( 57.33281313167710636, 216.1589784336661921, -6.496448406907675876E-16 ) ) ;
#91170 = ORIENTED_EDGE ( 'NONE', *, *, #85328, .F. ) ;
#91171 = ADVANCED_FACE ( 'NONE', ( #74781 ), #97751, .T. ) ;
#91172 = CARTESIAN_POINT ( 'NONE',  ( 182.7616540338069342, 265.0621685301391040, 14.91793811211548082 ) ) ;
#91173 = CARTESIAN_POINT ( 'NONE',  ( 185.3705633484216264, 298.4094130272380880, -0.2897616204090320280 ) ) ;
#91174 = CARTESIAN_POINT ( 'NONE',  ( -19.65312891409030271, 93.06504152958497400, 177.5919119679930134 ) ) ;
#91175 = EDGE_CURVE ( 'NONE', #2973, #44048, #98237, .T. ) ;
#91176 = ORIENTED_EDGE ( 'NONE', *, *, #12283, .T. ) ;
#91178 = CARTESIAN_POINT ( 'NONE',  ( 159.9950753608005130, 276.8117990079294373, 13.35014033362692487 ) ) ;
#91177 = AXIS2_PLACEMENT_3D ( 'NONE', #59363, #4705, #21879 ) ;
#91179 = CARTESIAN_POINT ( 'NONE',  ( 79.20708015383932832, 46.31796976865181392, -12.77997348381888187 ) ) ;
#91180 = DIRECTION ( 'NONE',  ( -0.000000000000000000, -0.000000000000000000, 1.000000000000000000 ) ) ;
#91181 = CARTESIAN_POINT ( 'NONE',  ( 73.03195784919465439, 70.41880241001356922, -8.079853440356906447 ) ) ;
#91182 = CARTESIAN_POINT ( 'NONE',  ( 206.8139415932446354, 271.7863864866807262, -6.273988927840268737 ) ) ;
#91183 = CARTESIAN_POINT ( 'NONE',  ( 157.1187995864133882, 258.5092516225370218, 18.42986330599266509 ) ) ;
#91184 = EDGE_LOOP ( 'NONE', ( #79005, #63941, #15323, #96280 ) ) ;
#91185 = CARTESIAN_POINT ( 'NONE',  ( 24.50893013558248157, 16.01110640527292261, 2.839279412974134775 ) ) ;
#91186 = CARTESIAN_POINT ( 'NONE',  ( 66.93954981368713675, 69.16002812685212575, -1.529596994131542154 ) ) ;
#91187 = CARTESIAN_POINT ( 'NONE',  ( 75.18619828000903738, 66.99152146615374193, -12.75634951131107364 ) ) ;
#91188 = ORIENTED_EDGE ( 'NONE', *, *, #51324, .T. ) ;
#91189 = DIRECTION ( 'NONE',  ( -0.000000000000000000, -0.000000000000000000, -1.000000000000000000 ) ) ;
#91190 = B_SPLINE_CURVE_WITH_KNOTS ( 'NONE', 3,
 ( #65603, #2330, #55983, #32708 ),
 .UNSPECIFIED., .F., .F.,
 ( 4, 4 ),
 ( 0.01002733877639494162, 0.01522564162345051847 ),
 .UNSPECIFIED. ) ;
#91191 = CARTESIAN_POINT ( 'NONE',  ( 47.96820964746023463, 80.67316705762479501, -10.00000000000000000 ) ) ;
#91192 = ORIENTED_EDGE ( 'NONE', *, *, #100099, .T. ) ;
#91193 = VERTEX_POINT ( 'NONE', #5606 ) ;
#91195 = CYLINDRICAL_SURFACE ( 'NONE', #5513, 70.00000000000002842 ) ;
#91194 = CARTESIAN_POINT ( 'NONE',  ( 168.0160359207364991, 287.1960299647130341, -6.005792533259211474 ) ) ;
#91196 = CARTESIAN_POINT ( 'NONE',  ( 163.0056347026689707, 248.3129541054019569, -11.27842346302751508 ) ) ;
#91197 = CARTESIAN_POINT ( 'NONE',  ( 164.2297246530060875, 246.1927681183832988, 5.803160395959773510 ) ) ;
#91198 = CYLINDRICAL_SURFACE ( 'NONE', #14083, 16.60714546451156792 ) ;
#91199 = CARTESIAN_POINT ( 'NONE',  ( 81.50373498261929228, 55.81176558511297969, 16.37496158676513858 ) ) ;
#91200 = CARTESIAN_POINT ( 'NONE',  ( 164.3713636635203841, 264.9441660766296991, -16.63686112330542599 ) ) ;
#91201 = CARTESIAN_POINT ( 'NONE',  ( 126.7502486777147794, 253.1744531367911009, 4.594050593750047540 ) ) ;
#91202 = CARTESIAN_POINT ( 'NONE',  ( 84.82981389336303835, 207.5327760586659167, 1.948934522072303157E-15 ) ) ;
#91203 = ORIENTED_EDGE ( 'NONE', *, *, #76526, .T. ) ;
#91204 = CARTESIAN_POINT ( 'NONE',  ( 174.1591195100927791, 265.6402296398555904, 16.51580490226363906 ) ) ;
#91205 = CARTESIAN_POINT ( 'NONE',  ( 79.22258912688209875, 45.79454436770367920, 13.02573821740452864 ) ) ;
#91206 = ORIENTED_EDGE ( 'NONE', *, *, #4821, .T. ) ;
#91207 = CARTESIAN_POINT ( 'NONE',  ( 72.52865609843787809, 57.51546068812135815, 16.29679984377914437 ) ) ;
#91208 = ORIENTED_EDGE ( 'NONE', *, *, #99830, .F. ) ;
#91209 = VERTEX_POINT ( 'NONE', #91234 ) ;
#91210 = CARTESIAN_POINT ( 'NONE',  ( 76.16027975956328078, 65.34306562879338287, 14.46508190410746764 ) ) ;
#91211 = CARTESIAN_POINT ( 'NONE',  ( 66.84894034102782712, 67.93781524052256771, 6.996449262558990689 ) ) ;
#91212 = DIRECTION ( 'NONE',  ( -0.5000000000000082157, 0.8660254037844338226, 0.000000000000000000 ) ) ;
#91213 = CARTESIAN_POINT ( 'NONE',  ( 191.8329718516215223, 298.3825415164982928, -8.871589506312979267 ) ) ;
#91214 = DIRECTION ( 'NONE',  ( -0.000000000000000000, 0.000000000000000000, -1.000000000000000000 ) ) ;
#91215 = CARTESIAN_POINT ( 'NONE',  ( 155.5204415533959548, 261.2776889444089647, 17.19127227448963424 ) ) ;
#91216 = CARTESIAN_POINT ( 'NONE',  ( 81.06766895168337328, 207.6115022471902023, -5.000000000000041744 ) ) ;
#91217 = CARTESIAN_POINT ( 'NONE',  ( 182.0915030940412862, 257.1429800395595748, -6.159901684290187696 ) ) ;
#91218 = ORIENTED_EDGE ( 'NONE', *, *, #97446, .F. ) ;
#91219 = CARTESIAN_POINT ( 'NONE',  ( 161.9258069053378222, 250.1832707138045180, -14.03928993546631254 ) ) ;
#91220 = EDGE_LOOP ( 'NONE', ( #36334, #88904, #97570, #42542 ) ) ;
#91221 = CARTESIAN_POINT ( 'NONE',  ( 163.9634607461725011, 260.5862723289976088, -16.19362549185895261 ) ) ;
#91222 = CARTESIAN_POINT ( 'NONE',  ( 164.8962722568797687, 246.6821832418063707, 5.577076257785627433 ) ) ;
#91223 = CARTESIAN_POINT ( 'NONE',  ( 187.4299001019809623, 277.0409167645560728, 16.92852667520122267 ) ) ;
#91224 = CARTESIAN_POINT ( 'NONE',  ( 206.0627831668701901, 273.7357853363691902, 10.14454147593459687 ) ) ;
#91225 = EDGE_CURVE ( 'NONE', #98683, #58073, #59791, .T. ) ;
#91226 = CARTESIAN_POINT ( 'NONE',  ( 149.2223635749290622, 272.1862799931444670, -12.97307652490353647 ) ) ;
#91227 = CARTESIAN_POINT ( 'NONE',  ( 198.6773598015395521, 281.0098537826190181, 16.91893506919627654 ) ) ;
#91228 = CARTESIAN_POINT ( 'NONE',  ( 69.13511649644314616, 71.04256955909853843, 2.869324681485878275E-06 ) ) ;
#91229 = CARTESIAN_POINT ( 'NONE',  ( 146.3987206697217403, 246.1423013555409796, -4.594050593750043987 ) ) ;
#91230 = VERTEX_POINT ( 'NONE', #98826 ) ;
#91231 = CARTESIAN_POINT ( 'NONE',  ( 87.84403297180379866, 44.29423158952226203, 4.754374079557552868 ) ) ;
#91232 = CARTESIAN_POINT ( 'NONE',  ( 85.71285599281509349, 43.91756893743614398, 5.655568829977952738 ) ) ;
#91233 = EDGE_CURVE ( 'NONE', #61436, #91371, #90762, .T. ) ;
#91234 = CARTESIAN_POINT ( 'NONE',  ( 167.2900023830132170, 283.1360949131732809, -11.47530909209802275 ) ) ;
#91235 = CARTESIAN_POINT ( 'NONE',  ( 79.52110638078222848, 59.35728171255717456, -16.21327867740588857 ) ) ;
#91236 = CIRCLE ( 'NONE', #15177, 14.21260523776213347 ) ;
#91237 = CARTESIAN_POINT ( 'NONE',  ( 71.22189038257839400, 67.26187328387359798, -10.54518486082646511 ) ) ;
#91238 = ORIENTED_EDGE ( 'NONE', *, *, #34423, .T. ) ;
#91239 = CARTESIAN_POINT ( 'NONE',  ( 76.47762942987780832, 54.52376294675376300, 16.10255537987762153 ) ) ;
#91240 = CARTESIAN_POINT ( 'NONE',  ( 182.2006005650631266, 275.4475936646326204, -16.49366260708473320 ) ) ;
#91241 = CARTESIAN_POINT ( 'NONE',  ( 172.8951663193395234, 288.9549776225803157, 8.104654168245465584 ) ) ;
#91242 = CARTESIAN_POINT ( 'NONE',  ( 82.57480368249606784, 41.04376301281222794, 1.111617510708536205 ) ) ;
#91243 = CARTESIAN_POINT ( 'NONE',  ( 185.6631226553351439, 263.8051797751761001, -12.74678442662920652 ) ) ;
#91244 = CARTESIAN_POINT ( 'NONE',  ( 202.5128468779458331, 267.1751508879428343, 0.8823122286173835649 ) ) ;
#91245 = ADVANCED_FACE ( 'NONE', ( #68393 ), #28917, .F. ) ;
#91246 = CARTESIAN_POINT ( 'NONE',  ( 195.1818950096821368, 263.7941917347654908, 0.8445903136804231437 ) ) ;
#91247 = AXIS2_PLACEMENT_3D ( 'NONE', #98533, #6310, #92442 ) ;
#91248 = CARTESIAN_POINT ( 'NONE',  ( 147.1199024702499969, 275.8278494473859723, 5.224467159276165340 ) ) ;
#91249 = CARTESIAN_POINT ( 'NONE',  ( 186.8638380190930377, 282.1138426105056283, 17.22312890734132296 ) ) ;
#91250 = CARTESIAN_POINT ( 'NONE',  ( 164.8251969117060298, 245.1613799118173063, -1.508678420156898348 ) ) ;
#91251 = CARTESIAN_POINT ( 'NONE',  ( 196.8251380678160274, 269.8453290852096416, 12.06679547565278909 ) ) ;
#91252 = EDGE_CURVE ( 'NONE', #50939, #68532, #64282, .T. ) ;
#91253 = CARTESIAN_POINT ( 'NONE',  ( 23.52344096658253747, 21.78052372038641238, -10.00000000000000355 ) ) ;
#91254 = EDGE_CURVE ( 'NONE', #17524, #16763, #78868, .T. ) ;
#91255 = CARTESIAN_POINT ( 'NONE',  ( 149.0359194785865498, 272.5092106407810206, 12.76357969772040590 ) ) ;
#91256 = CARTESIAN_POINT ( 'NONE',  ( 79.60625107924921906, 206.7677522451417929, -5.000000000000041744 ) ) ;
#91257 = CARTESIAN_POINT ( 'NONE',  ( 66.82849716633455728, 68.92242650857625108, -4.723788943350095693 ) ) ;
#91258 = B_SPLINE_CURVE_WITH_KNOTS ( 'NONE', 3,
 ( #43598, #20322, #12734, #83645, #67905, #98825, #89756, #90761, #37480, #5114, #97828, #22296, #68392, #59277, #82663, #20827 ),
 .UNSPECIFIED., .F., .F.,
 ( 4, 1, 2, 2, 2, 1, 2, 2, 4 ),
 ( 0.000000000000000000, 0.1249999999999970024, 0.1874999999999956424, 0.2499999999999942824, 0.4999999999999977796, 0.6249999999999977796, 0.6874999999999976685, 0.7499999999999976685, 1.000000000000000000 ),
 .UNSPECIFIED. ) ;
#91259 = CARTESIAN_POINT ( 'NONE',  ( 159.9307118030769175, 253.6388767968520881, 16.60600887889890487 ) ) ;
#91260 = CARTESIAN_POINT ( 'NONE',  ( 207.2934823643110178, 271.6041517975674537, 5.071655803097819160 ) ) ;
#91261 = CARTESIAN_POINT ( 'NONE',  ( 140.7332108297007665, 265.3927522451418781, 2.944929066748280225E-16 ) ) ;
#91262 = LINE ( 'NONE', #66436, #43422 ) ;
#91263 = VERTEX_POINT ( 'NONE', #74537 ) ;
#91264 = CARTESIAN_POINT ( 'NONE',  ( 66.95873798537226662, 67.67772264583786068, -6.456423497743614348 ) ) ;
#91265 = CARTESIAN_POINT ( 'NONE',  ( 72.83785029587782844, 70.28570241188594991, -8.113289319485218698 ) ) ;
#91266 = CARTESIAN_POINT ( 'NONE',  ( 151.0426280674448378, 269.0334894088936153, -15.84467774422408581 ) ) ;
#91267 = CARTESIAN_POINT ( 'NONE',  ( 7.266240119036749157, 168.8768266524159856, -9.188101187500093303 ) ) ;
#91268 = B_SPLINE_CURVE_WITH_KNOTS ( 'NONE', 3,
 ( #65245, #87125, #72879, #57132 ),
 .UNSPECIFIED., .F., .F.,
 ( 4, 4 ),
 ( 0.03752702852749528750, 0.04612527040108949095 ),
 .UNSPECIFIED. ) ;
#91269 = CARTESIAN_POINT ( 'NONE',  ( 26.39215011307057424, 23.43677371833802425, -10.00000000000000355 ) ) ;
#91270 = CARTESIAN_POINT ( 'NONE',  ( 85.05422843502101671, 48.88568976824796408, 12.38837144396399381 ) ) ;
#91271 = CARTESIAN_POINT ( 'NONE',  ( 170.0577865676564215, 270.6915287872138833, -17.14917795963988212 ) ) ;
#91272 = CARTESIAN_POINT ( 'NONE',  ( 24.35067441160642687, 40.23626134430272572, -10.00000000000000000 ) ) ;
#91273 = CARTESIAN_POINT ( 'NONE',  ( 150.1280791300635826, 276.5080219999884434, 3.727701050747722178 ) ) ;
#91274 = EDGE_CURVE ( 'NONE', #97853, #57975, #99497, .T. ) ;
#91275 = CARTESIAN_POINT ( 'NONE',  ( 175.5054462216997422, 253.5402674413775799, -3.793157809723892271 ) ) ;
#91276 = CARTESIAN_POINT ( 'NONE',  ( 150.2678036912315349, 270.3755245954375823, 14.25047800729520375 ) ) ;
#91277 = EDGE_CURVE ( 'NONE', #3243, #53003, #45581, .T. ) ;
#91278 = CARTESIAN_POINT ( 'NONE',  ( 53.86003751612224733, 195.2365022471902023, -10.00000000000009059 ) ) ;
#91279 = DIRECTION ( 'NONE',  ( 0.9659258262890757507, -0.2588190451024926508, 3.165834739509918729E-16 ) ) ;
#91280 = CARTESIAN_POINT ( 'NONE',  ( 148.1672759425158290, 274.0137453789218398, 7.847779094015780110 ) ) ;
#91281 = CARTESIAN_POINT ( 'NONE',  ( 21.98867198337220685, 177.3768266524160140, 9.188101187500098632 ) ) ;
#91282 = CARTESIAN_POINT ( 'NONE',  ( 164.8765683363924666, 284.8271691914964663, 4.187516861581451977 ) ) ;
#91283 = CARTESIAN_POINT ( 'NONE',  ( 152.7531861616124615, 266.0707158804971186, 17.45453282433162556 ) ) ;
#91284 = CARTESIAN_POINT ( 'NONE',  ( 43.77620770598743150, 30.98920272979930601, 7.433330006724137462 ) ) ;
#91285 = DIRECTION ( 'NONE',  ( 0.9999986627203610867, -0.001635407438361276495, 0.000000000000000000 ) ) ;
#91286 = LINE ( 'NONE', #68936, #41834 ) ;
#91287 = EDGE_CURVE ( 'NONE', #20951, #68688, #22154, .T. ) ;
#91288 = CARTESIAN_POINT ( 'NONE',  ( 185.3021252847411802, 266.6084221390160565, 13.26759877312805180 ) ) ;
#91289 = CARTESIAN_POINT ( 'NONE',  ( 153.6392919293977002, 266.5359356698173769, -16.75038546547492402 ) ) ;
#91290 = CARTESIAN_POINT ( 'NONE',  ( -63.30067564770008914, 39.94154026010144065, 10.00000000000000000 ) ) ;
#91291 = SHAPE_DEFINITION_REPRESENTATION ( #71797, #78010 ) ;
#91292 = CARTESIAN_POINT ( 'NONE',  ( 14.66813190280496570, 26.65586893147755276, -7.433330006724137462 ) ) ;
#91293 = CARTESIAN_POINT ( 'NONE',  ( 190.6071113721798156, 300.5057941498820924, -0.4754021072632813594 ) ) ;
#91294 = CARTESIAN_POINT ( 'NONE',  ( 71.88182444303143370, 59.07920979518379312, 15.87605134362294734 ) ) ;
#91295 = ADVANCED_FACE ( 'NONE', ( #62784 ), #31879, .F. ) ;
#91296 = CARTESIAN_POINT ( 'NONE',  ( 155.6276701977099890, 261.0919634844306643, 17.49722577287685255 ) ) ;
#91297 = ORIENTED_EDGE ( 'NONE', *, *, #18196, .T. ) ;
#91298 = DIRECTION ( 'NONE',  ( 0.4999999999999998890, -0.8660254037844385966, 0.000000000000000000 ) ) ;
#91299 = LINE ( 'NONE', #69456, #89131 ) ;
#91300 = EDGE_CURVE ( 'NONE', #6702, #4197, #45109, .T. ) ;
#91301 = CARTESIAN_POINT ( 'NONE',  ( 88.02595808552065648, 44.67474554292944333, 4.297255302186842485 ) ) ;
#91302 = CARTESIAN_POINT ( 'NONE',  ( 81.36830186270630350, 42.43310981303259410, 7.489272701115289088 ) ) ;
#91303 = EDGE_CURVE ( 'NONE', #8797, #67335, #61953, .T. ) ;
#91304 = ORIENTED_EDGE ( 'NONE', *, *, #3947, .F. ) ;
#91305 = CARTESIAN_POINT ( 'NONE',  ( 45.05588048050944394, 66.36777381976860113, 10.00000000000000000 ) ) ;
#91306 = CARTESIAN_POINT ( 'NONE',  ( 148.2404373810095706, 275.8870260502966403, -5.709515531134017330 ) ) ;
#91307 = DIRECTION ( 'NONE',  ( -1.000000000000000000, 0.000000000000000000, 0.000000000000000000 ) ) ;
#91308 = CARTESIAN_POINT ( 'NONE',  ( 203.5629025532486196, 278.0657055720176913, -15.85226727704602823 ) ) ;
#91309 = ORIENTED_EDGE ( 'NONE', *, *, #2788, .T. ) ;
#91310 = ORIENTED_EDGE ( 'NONE', *, *, #7613, .T. ) ;
#91312 = CARTESIAN_POINT ( 'NONE',  ( 164.4272222519600746, 245.8506922426221593, 7.021336339662529902 ) ) ;
#91311 = DIRECTION ( 'NONE',  ( 1.000000000000000000, 0.000000000000000000, 0.000000000000000000 ) ) ;
#91313 = EDGE_LOOP ( 'NONE', ( #67422, #14548, #52124, #77527 ) ) ;
#91314 = CARTESIAN_POINT ( 'NONE',  ( 153.1961624462112752, 265.3034584490234806, -16.19494717845262954 ) ) ;
#91315 = CARTESIAN_POINT ( 'NONE',  ( 29.42770338693789967, 22.15404122711134960, 8.090169943749479842 ) ) ;
#91316 = CARTESIAN_POINT ( 'NONE',  ( 80.74762043199122274, 57.32811249769932260, 16.57232535949601626 ) ) ;
#91317 = CARTESIAN_POINT ( 'NONE',  ( 68.29143555172046831, 69.60586533063577974, -5.163910978133268159 ) ) ;
#91318 = VERTEX_POINT ( 'NONE', #498 ) ;
#91319 = DIRECTION ( 'NONE',  ( -0.9762143704923794685, 0.2168075248790210796, 0.000000000000000000 ) ) ;
#91320 = AXIS2_PLACEMENT_3D ( 'NONE', #51033, #97189, #91083 ) ;
#91321 = CARTESIAN_POINT ( 'NONE',  ( 196.9098758191317700, 289.5890858996224324, -16.54412079817003800 ) ) ;
#91322 = ORIENTED_EDGE ( 'NONE', *, *, #476, .F. ) ;
#91323 = CARTESIAN_POINT ( 'NONE',  ( 164.9171241593586217, 245.0021572482830550, 1.622680932994367220 ) ) ;
#91324 = DIRECTION ( 'NONE',  ( 0.000000000000000000, 0.000000000000000000, 1.000000000000000000 ) ) ;
#91325 = EDGE_LOOP ( 'NONE', ( #72625, #21803, #47344, #8746 ) ) ;
#91326 = CARTESIAN_POINT ( 'NONE',  ( 190.4163244163388242, 300.8362468508201459, 4.691083071570470331 ) ) ;
#91327 = CARTESIAN_POINT ( 'NONE',  ( 195.1474640768281290, 265.6393084148356252, -8.887799905196541062 ) ) ;
#91328 = VERTEX_POINT ( 'NONE', #78008 ) ;
#91329 = CARTESIAN_POINT ( 'NONE',  ( -15.83597077268904663, 73.66574995701986950, 13.56964096002992015 ) ) ;
#91330 = DIRECTION ( 'NONE',  ( -0.5607300124661884766, 0.8279987035736640077, 0.000000000000000000 ) ) ;
#91331 = CYLINDRICAL_SURFACE ( 'NONE', #28924, 15.50000000000000000 ) ;
#91332 = CARTESIAN_POINT ( 'NONE',  ( 103.4423036115607601, 218.9824982072974251, 3.021315404115420679E-15 ) ) ;
#91333 = VERTEX_POINT ( 'NONE', #16196 ) ;
#91334 = VERTEX_POINT ( 'NONE', #8600 ) ;
#91335 =( BOUNDED_CURVE ( )  B_SPLINE_CURVE ( 2, ( #35872, #98195, #66776, #36364, #97701, #28777, #11109, #41979, #34384 ),
 .UNSPECIFIED., .F., .T. ) 
 B_SPLINE_CURVE_WITH_KNOTS ( ( 3, 2, 2, 2, 3 ),
 ( 0.6895161290322581182, 0.6908602150537634934, 0.6935483870967742437, 0.6962365591397849940, 0.6975806451612903691 ),
 .UNSPECIFIED. ) 
 CURVE ( )  GEOMETRIC_REPRESENTATION_ITEM ( )  RATIONAL_B_SPLINE_CURVE ( ( 0.9330127018922194093, 0.9330127018922194093, 1.000000000000000000, 0.8660254037844387076, 1.000000000000000000, 0.8660254037844387076, 1.000000000000000000, 0.9330127018922194093, 0.9330127018922194093 ) ) 
 REPRESENTATION_ITEM ( '' )  );
#91336 = CARTESIAN_POINT ( 'NONE',  ( 73.20149111268449360, 69.78470516290340697, 9.100743165113243549 ) ) ;
#91337 = CARTESIAN_POINT ( 'NONE',  ( 147.4368675721658519, 275.2788497866417288, 5.050119523016719292 ) ) ;
#91338 = CARTESIAN_POINT ( 'NONE',  ( 190.3691966041315311, 300.9178746160123410, 0.1783449565851275009 ) ) ;
#91339 = CARTESIAN_POINT ( 'NONE',  ( 190.1751179328237242, 301.2540287353828035, 3.252640783176552475 ) ) ;
#91340 = CARTESIAN_POINT ( 'NONE',  ( 192.2943420783192323, 297.5834248427583475, 12.53393473147773562 ) ) ;
#91341 = CARTESIAN_POINT ( 'NONE',  ( 147.3005892150715113, 275.5148908251009061, -0.09882562957467407039 ) ) ;
#91342 = CARTESIAN_POINT ( 'NONE',  ( 146.5913834600193582, 276.7432712258716947, -0.4909717733184599253 ) ) ;
#91343 = B_SPLINE_CURVE_WITH_KNOTS ( 'NONE', 3,
 ( #79718, #19402, #65466, #25470, #87359, #50261, #17888, #48787, #72089, #51246 ),
 .UNSPECIFIED., .F., .F.,
 ( 4, 2, 2, 2, 4 ),
 ( 0.0003596424459949675977, 0.0006587098368031852821, 0.0009577772276114028581, 0.001256844618419620434, 0.001555912009227838119 ),
 .UNSPECIFIED. ) ;
#91344 = CARTESIAN_POINT ( 'NONE',  ( 76.92044504429365759, 57.04706196720093914, -16.17893565157367775 ) ) ;
#91345 = CARTESIAN_POINT ( 'NONE',  ( 71.87575657461835021, 71.09473384654326367, 5.547135274974943187 ) ) ;
#91346 = CARTESIAN_POINT ( 'NONE',  ( 48.60927726968589013, 109.6985806698937012, 10.00000000000000000 ) ) ;
#91347 = DIRECTION ( 'NONE',  ( 0.000000000000000000, 0.000000000000000000, 1.000000000000000000 ) ) ;
#91348 = CARTESIAN_POINT ( 'NONE',  ( 168.2949371938393597, 286.3488455771775421, 4.006590656272537743 ) ) ;
#91349 = CARTESIAN_POINT ( 'NONE',  ( 78.54767433042584912, 47.93402356940807607, 13.94239611146432445 ) ) ;
#91350 = EDGE_LOOP ( 'NONE', ( #37815, #42706, #87328, #58231 ) ) ;
#91351 = CARTESIAN_POINT ( 'NONE',  ( 190.0373668968398988, 301.4926205285023002, -3.919393248615649306 ) ) ;
#91352 = CARTESIAN_POINT ( 'NONE',  ( 72.33612429178343461, 70.29735357913294536, 7.619994811607423202 ) ) ;
#91353 = CARTESIAN_POINT ( 'NONE',  ( 148.8662434136574291, 273.1977519777474299, 9.320112586661617016 ) ) ;
#91354 = CARTESIAN_POINT ( 'NONE',  ( 79.22767783863193358, 46.14077938263190504, 12.65241577235085124 ) ) ;
#91355 = CARTESIAN_POINT ( 'NONE',  ( 39.04508293989853485, 204.8967562850347122, -4.648177544792955347E-16 ) ) ;
#91356 = CARTESIAN_POINT ( 'NONE',  ( 147.9216321868252066, 274.4392128443400907, -9.725520637227743848 ) ) ;
#91357 = CARTESIAN_POINT ( 'NONE',  ( 166.8351002587995140, 283.9006457132830974, -8.055937853886671718 ) ) ;
#91358 = EDGE_LOOP ( 'NONE', ( #22602, #85935, #56911, #61133, #4216 ) ) ;
#91359 = CARTESIAN_POINT ( 'NONE',  ( 170.5981529699230066, 255.5880127657044625, -12.68729301884834371 ) ) ;
#91360 = CARTESIAN_POINT ( 'NONE',  ( 82.87158540007671093, 42.03325885046006505, 6.269962817432972457 ) ) ;
#91361 = CARTESIAN_POINT ( 'NONE',  ( 72.60487375326179915, 71.50102857937403655, 5.576306808341180421 ) ) ;
#91362 = CARTESIAN_POINT ( 'NONE',  ( 48.93451802855033606, 192.3927522451418213, 10.00000000000009592 ) ) ;
#91363 = CARTESIAN_POINT ( 'NONE',  ( 120.7155680147981940, 234.3768266524159856, 9.188101187500096856 ) ) ;
#91364 = EDGE_CURVE ( 'NONE', #94561, #45170, #32395, .T. ) ;
#91365 = CARTESIAN_POINT ( 'NONE',  ( 151.2964716097791325, 268.5938194963972592, -15.66250187539618111 ) ) ;
#91366 = DIRECTION ( 'NONE',  ( 0.000000000000000000, 0.000000000000000000, 1.000000000000000000 ) ) ;
#91367 = CARTESIAN_POINT ( 'NONE',  ( 84.15726348823297087, 50.51978324134979204, 13.75935458598990557 ) ) ;
#91368 = CARTESIAN_POINT ( 'NONE',  ( 172.5941544643821999, 251.3792726610714112, -3.974732898687233895 ) ) ;
#91369 = CARTESIAN_POINT ( 'NONE',  ( 30.97333845187074886, 194.8149278399160949, -9.188101187500095079 ) ) ;
#91370 = LINE ( 'NONE', #83272, #34916 ) ;
#91371 = VERTEX_POINT ( 'NONE', #56174 ) ;
#91372 = CARTESIAN_POINT ( 'NONE',  ( 190.1774295428112396, 299.2500249094251217, 7.542682482482700124 ) ) ;
#91373 = CARTESIAN_POINT ( 'NONE',  ( 15.10771242554802463, 167.9824982072973967, -5.229199737892075682E-14 ) ) ;
#91374 = EDGE_CURVE ( 'NONE', #63672, #7578, #24785, .T. ) ;
#91375 = CARTESIAN_POINT ( 'NONE',  ( 18.20865839366279459, 187.9865022471902876, 10.00000000000009415 ) ) ;
#91376 = EDGE_CURVE ( 'NONE', #43419, #68946, #39465, .T. ) ;
#91377 = CARTESIAN_POINT ( 'NONE',  ( 146.8000281410530192, 276.3818880375922049, 4.652863924796177386 ) ) ;
#91378 = CARTESIAN_POINT ( 'NONE',  ( 110.0000000000000000, 15.00000000000003908, 59.99999999999999289 ) ) ;
#91379 = VECTOR ( 'NONE', #67510, 1000.000000000000114 ) ;
#91380 = CARTESIAN_POINT ( 'NONE',  ( 75.75493378409400691, 65.86437009324525604, -14.07593894684414693 ) ) ;
#91381 = CARTESIAN_POINT ( 'NONE',  ( 176.2784227036720210, 285.4830148766054663, -12.04998877190618067 ) ) ;
#91382 = CARTESIAN_POINT ( 'NONE',  ( 164.1276822366001511, 250.0947574105164506, 10.98824708228447733 ) ) ;
#91383 = CARTESIAN_POINT ( 'NONE',  ( 107.7520767022434853, 223.0177522451418213, 5.000000000000051514 ) ) ;
#91384 = ORIENTED_EDGE ( 'NONE', *, *, #78225, .T. ) ;
#91385 = CARTESIAN_POINT ( 'NONE',  ( 195.7767944968437632, 266.9069622423809847, -7.771366023404486789 ) ) ;
#91386 = VECTOR ( 'NONE', #98381, 1000.000000000000114 ) ;
#91387 = CARTESIAN_POINT ( 'NONE',  ( 158.5437609352171933, 281.8370119815768362, -1.612487481721458948 ) ) ;
#91388 = CARTESIAN_POINT ( 'NONE',  ( 163.1369207721744772, 248.0855599626920593, -11.24692769914530110 ) ) ;
#91389 = CARTESIAN_POINT ( 'NONE',  ( 12.43489537816885537, 187.1744531367911293, 4.594050593750047540 ) ) ;
#91390 = CARTESIAN_POINT ( 'NONE',  ( 15.23341505093859816, 9.764269794150882475, 3.090169943749476733 ) ) ;
#91391 = CARTESIAN_POINT ( 'NONE',  ( 192.1258111988436781, 272.3008933654719499, 14.87177412048350966 ) ) ;
#91392 = CARTESIAN_POINT ( 'NONE',  ( 71.62383979505139564, 59.52605231305792444, -15.70840275671411845 ) ) ;
#91393 = CARTESIAN_POINT ( 'NONE',  ( 157.2948870673828026, 280.9759411348209142, 6.053012778684776940 ) ) ;
#91395 = CARTESIAN_POINT ( 'NONE',  ( 63.34103791831414298, 213.5024278399161233, 9.188101187500095079 ) ) ;
#91394 = CARTESIAN_POINT ( 'NONE',  ( 174.9881383257676646, 286.4353486899028667, 10.48873152270803466 ) ) ;
#91396 = CARTESIAN_POINT ( 'NONE',  ( 208.3057440179679531, 269.8508631828800617, 2.969924427282375046 ) ) ;
#91397 = CARTESIAN_POINT ( 'NONE',  ( 73.16773116491842188, 57.32667411120098677, 16.38412366264992315 ) ) ;
#91398 = CARTESIAN_POINT ( 'NONE',  ( 69.75017563541113930, 66.23009299845347186, 11.34195834197200625 ) ) ;
#91399 = CARTESIAN_POINT ( 'NONE',  ( 66.43953443436693362, 68.06212878376058484, -4.898982275787033380 ) ) ;
#91400 = ORIENTED_EDGE ( 'NONE', *, *, #1027, .F. ) ;
#91401 = EDGE_CURVE ( 'NONE', #66291, #80464, #80712, .T. ) ;
#91402 = CARTESIAN_POINT ( 'NONE',  ( 9.548404355818409073, 182.9865022471903160, -10.00000000000009415 ) ) ;
#91403 = CARTESIAN_POINT ( 'NONE',  ( 207.7655736232174206, 270.7864657513322300, 3.530742899761726949 ) ) ;
#91404 = CARTESIAN_POINT ( 'NONE',  ( 132.6230702210692414, 253.5024278399160949, -9.188101187500093303 ) ) ;
#91405 = CARTESIAN_POINT ( 'NONE',  ( 25.24326406500046360, 20.28920272979927475, -7.433330006724141015 ) ) ;
#91406 = CARTESIAN_POINT ( 'NONE',  ( 189.4381674897702794, 265.0040801212285828, 12.03645615491573828 ) ) ;
#91407 = CARTESIAN_POINT ( 'NONE',  ( 83.83095627921952087, 51.88776739408810812, -14.90233955705620694 ) ) ;
#91408 = EDGE_CURVE ( 'NONE', #95312, #98060, #17301, .T. ) ;
#91409 = CARTESIAN_POINT ( 'NONE',  ( 72.69493809724967548, 71.16443809380129437, -7.267007365939463170 ) ) ;
#91411 = CARTESIAN_POINT ( 'NONE',  ( 74.66818547213321722, 67.01009517369644186, 12.98877810528426835 ) ) ;
#91410 = DIRECTION ( 'NONE',  ( -0.5888918169447132644, 0.8082118706970062849, 0.000000000000000000 ) ) ;
#91412 = EDGE_CURVE ( 'NONE', #38035, #90841, #35418, .T. ) ;
#91413 = CARTESIAN_POINT ( 'NONE',  ( 69.13686587061594935, 64.31895405193962745, 11.99662287724233067 ) ) ;
#91414 = ORIENTED_EDGE ( 'NONE', *, *, #91613, .F. ) ;
#91415 = CARTESIAN_POINT ( 'NONE',  ( 81.53593397896733563, 52.71546265156933941, 15.68299913778540500 ) ) ;
#91416 = CARTESIAN_POINT ( 'NONE',  ( 152.1434865710199063, 268.6225420542635902, -15.29845542693487914 ) ) ;
#91417 = CARTESIAN_POINT ( 'NONE',  ( 196.4280118926366185, 289.9318269284742655, 16.33325042109277803 ) ) ;
#91418 = CARTESIAN_POINT ( 'NONE',  ( 67.53167658295855347, 67.09922345392760690, 8.942594108559751120 ) ) ;
#91419 = ORIENTED_EDGE ( 'NONE', *, *, #1818, .F. ) ;
#91420 = CARTESIAN_POINT ( 'NONE',  ( 159.9468613345221684, 253.6109049878705832, 15.91085046606713327 ) ) ;
#91421 = VECTOR ( 'NONE', #7791, 1000.000000000000227 ) ;
#91422 = CARTESIAN_POINT ( 'NONE',  ( -33.12036098009136964, 24.37273002035945169, 10.00000000000000000 ) ) ;
#91423 = EDGE_CURVE ( 'NONE', #16754, #20462, #73407, .T. ) ;
#91424 = EDGE_CURVE ( 'NONE', #69834, #83731, #79546, .T. ) ;
#91425 = DIRECTION ( 'NONE',  ( 0.000000000000000000, -0.000000000000000000, -1.000000000000000000 ) ) ;
#91426 = DIRECTION ( 'NONE',  ( -0.5000000000000013323, 0.8660254037844378194, 0.000000000000000000 ) ) ;
#91427 = CARTESIAN_POINT ( 'NONE',  ( 149.7206294291796667, 272.5596913884758123, 11.32704556092920889 ) ) ;
#91428 = CARTESIAN_POINT ( 'NONE',  ( 175.7622132985686392, 274.0430017844784629, -17.75579533532145504 ) ) ;
#91429 = CARTESIAN_POINT ( 'NONE',  ( 200.7694952279801157, 282.9040289856181403, -17.94628235092568502 ) ) ;
#91430 = VERTEX_POINT ( 'NONE', #49587 ) ;
#91431 = B_SPLINE_CURVE_WITH_KNOTS ( 'NONE', 3,
 ( #649, #15838, #48250, #32032, #16348, #85819, #39121, #85293, #24939, #54836, #78664, #40128, #55816, #47242, #78161, #48762, #8749, #56334, #1669, #39620, #86809, #17342, #79196, #9770 ),
 .UNSPECIFIED., .F., .F.,
 ( 4, 2, 2, 2, 2, 2, 2, 2, 2, 2, 2, 4 ),
 ( 0.000000000000000000, 0.1250000000000026090, 0.2500000000000052180, 0.3750000000000078271, 0.4375000000000070499, 0.5000000000000063283, 0.5625000000000056621, 0.6250000000000048850, 0.6875000000000042188, 0.7500000000000035527, 0.8750000000000017764, 1.000000000000000000 ),
 .UNSPECIFIED. ) ;
#91432 = DIRECTION ( 'NONE',  ( -0.000000000000000000, -0.000000000000000000, -1.000000000000000000 ) ) ;
#91433 = CARTESIAN_POINT ( 'NONE',  ( 15.90241741327948866, 17.38052372038639248, 10.00000000000000533 ) ) ;
#91434 = CARTESIAN_POINT ( 'NONE',  ( 84.34903687182406884, 231.0530062829863027, -4.648177544792955347E-16 ) ) ;
#91435 = ORIENTED_EDGE ( 'NONE', *, *, #84144, .F. ) ;
#91436 = CARTESIAN_POINT ( 'NONE',  ( 148.9719199701866899, 272.6200610409887872, 12.59512981512031438 ) ) ;
#91437 = FACE_OUTER_BOUND ( 'NONE', #7817, .T. ) ;
#91438 = CARTESIAN_POINT ( 'NONE',  ( 1.813001633210440611, 27.74720351945397923, -10.00000000000000000 ) ) ;
#91439 = ORIENTED_EDGE ( 'NONE', *, *, #9468, .T. ) ;
#91440 = CARTESIAN_POINT ( 'NONE',  ( 191.1192699377806719, 299.6187094927299199, -9.526914969203620132 ) ) ;
#91441 = CARTESIAN_POINT ( 'NONE',  ( 87.04122873496829982, 46.31593380912285340, -9.298662157179387933 ) ) ;
#91442 = CARTESIAN_POINT ( 'NONE',  ( 163.7729086741176161, 246.9839966035275438, 6.099406794390714204 ) ) ;
#91443 = CARTESIAN_POINT ( 'NONE',  ( 74.98280371995244309, 53.54625940471802892, -16.54205200350763505 ) ) ;
#91444 = CARTESIAN_POINT ( 'NONE',  ( 69.72103949949544699, 62.67904974704494236, 13.91083112788282072 ) ) ;
#91445 = ORIENTED_EDGE ( 'NONE', *, *, #46602, .F. ) ;
#91446 = CARTESIAN_POINT ( 'NONE',  ( 98.17141035282828909, 236.6744531367911293, 4.594050593750047540 ) ) ;
#91447 = CARTESIAN_POINT ( 'NONE',  ( 202.8812894462602401, 279.2462941044264539, 15.70414016608259722 ) ) ;
#91448 = CARTESIAN_POINT ( 'NONE',  ( 179.2330864023228685, 269.9232757945108006, -16.11891054009439728 ) ) ;
#91449 = CARTESIAN_POINT ( 'NONE',  ( 81.80218481495317917, 42.34898084214702152, -7.958921281150827198 ) ) ;
#91450 = EDGE_LOOP ( 'NONE', ( #67203, #10986, #38862, #624 ) ) ;
#91451 = ORIENTED_EDGE ( 'NONE', *, *, #30959, .T. ) ;
#91452 = VERTEX_POINT ( 'NONE', #3993 ) ;
#91453 = CARTESIAN_POINT ( 'NONE',  ( 81.26485967175177905, 49.45078135016260745, 13.98408766788312896 ) ) ;
#91454 = AXIS2_PLACEMENT_3D ( 'NONE', #98035, #19556, #35221 ) ;
#91455 = ORIENTED_EDGE ( 'NONE', *, *, #7992, .F. ) ;
#91456 = LINE ( 'NONE', #31595, #41152 ) ;
#91457 = EDGE_LOOP ( 'NONE', ( #87735, #85198, #64099, #21392 ) ) ;
#91458 = CARTESIAN_POINT ( 'NONE',  ( 163.7085541710205234, 247.0954618725873217, -6.713544974106887331 ) ) ;
#91460 = ADVANCED_FACE ( 'NONE', ( #34880 ), #88658, .T. ) ;
#91459 = CARTESIAN_POINT ( 'NONE',  ( 200.9521687275011175, 282.5876292032514243, -18.16013154125647944 ) ) ;
#91461 = CARTESIAN_POINT ( 'NONE',  ( -23.55654553378506932, 99.75847253490320554, 45.19947544897750191 ) ) ;
#91462 = CARTESIAN_POINT ( 'NONE',  ( 82.49266829201729934, 54.25868459827957935, -15.95543171357395629 ) ) ;
#91463 = EDGE_LOOP ( 'NONE', ( #97176, #74483, #26091, #49314 ) ) ;
#91465 = CARTESIAN_POINT ( 'NONE',  ( 65.97950814763213145, 68.67089519182323443, -0.3204388555221999724 ) ) ;
#91464 = B_SPLINE_CURVE_WITH_KNOTS ( 'NONE', 3,
 ( #64302, #95253, #41484, #25820, #56697, #87677, #18213, #49105, #49593, #80547 ),
 .UNSPECIFIED., .F., .F.,
 ( 4, 2, 2, 2, 4 ),
 ( 0.001136000421166406512, 0.001208387388216028554, 0.001280774355265650597, 0.001425548289364900753, 0.001715096157563401067 ),
 .UNSPECIFIED. ) ;
#91466 = CARTESIAN_POINT ( 'NONE',  ( 19.11131643181922968, 13.96004757982089473, -5.678558825948276656 ) ) ;
#91467 = CARTESIAN_POINT ( 'NONE',  ( 167.2650757157126407, 283.7916248837542526, 9.058252512891741048 ) ) ;
#91468 = CARTESIAN_POINT ( 'NONE',  ( 80.68870194293324971, 57.51412305112833678, 16.58365939551019608 ) ) ;
#91470 = VERTEX_POINT ( 'NONE', #58184 ) ;
#91469 = CARTESIAN_POINT ( 'NONE',  ( 117.2061873602235238, 245.1427522451419065, -10.00000000000009592 ) ) ;
#91471 = CARTESIAN_POINT ( 'NONE',  ( 199.1165320752825494, 285.7670451491295580, 0.000000000000000000 ) ) ;
#91472 = CARTESIAN_POINT ( 'NONE',  ( 17.60357497223980516, 35.28838536716092023, -10.00000000000000000 ) ) ;
#91473 = CARTESIAN_POINT ( 'NONE',  ( 158.3909187560116436, 280.0920373912738910, -6.736592508546087821 ) ) ;
#91474 = CARTESIAN_POINT ( 'NONE',  ( 48.61286661847091750, 84.94359857078811160, -10.00000000000000000 ) ) ;
#91475 = CARTESIAN_POINT ( 'NONE',  ( -15.31269525828471068, 104.2312461070085021, 45.19948692389422717 ) ) ;
#91476 = CARTESIAN_POINT ( 'NONE',  ( 171.3293103646413726, 255.5786316856422786, 11.21396041803508581 ) ) ;
#91477 = CARTESIAN_POINT ( 'NONE',  ( 157.6839078477695182, 281.5272880355949496, 1.407186217441265264 ) ) ;
#91478 = ORIENTED_EDGE ( 'NONE', *, *, #72142, .F. ) ;
#91479 = CARTESIAN_POINT ( 'NONE',  ( 101.8522786425099156, 219.6115022471901739, -5.000000000000041744 ) ) ;
#91480 = CARTESIAN_POINT ( 'NONE',  ( 83.82827945288542537, 51.88092520783234818, 14.50189114860043205 ) ) ;
#91481 = CARTESIAN_POINT ( 'NONE',  ( -5.227692231867530737, 63.12463727082348441, -10.00000000000000000 ) ) ;
#91482 = CARTESIAN_POINT ( 'NONE',  ( 1.663964738649737374, 161.7677522451418213, -5.000000000000041744 ) ) ;
#91483 = EDGE_CURVE ( 'NONE', #5025, #5362, #65779, .T. ) ;
#91484 = CARTESIAN_POINT ( 'NONE',  ( 193.3208433121157839, 266.9444617411745071, -11.48094634684561122 ) ) ;
#91485 = CARTESIAN_POINT ( 'NONE',  ( 172.1197128340322422, 279.8946286459532757, -14.44200207385173229 ) ) ;
#91486 = CARTESIAN_POINT ( 'NONE',  ( 163.4060470519778505, 247.6194195724207248, -7.715457960547858818 ) ) ;
#91487 = CARTESIAN_POINT ( 'NONE',  ( 72.13241438359672486, 72.32265461515862626, 1.126504182728680803 ) ) ;
#91488 = CARTESIAN_POINT ( 'NONE',  ( 72.78673888116644264, 70.95540242780744222, 7.715912594624930065 ) ) ;
#91490 = CARTESIAN_POINT ( 'NONE',  ( 24.92020183544706668, 36.16126292948897003, -6.180339887498951690 ) ) ;
#91489 = CARTESIAN_POINT ( 'NONE',  ( -15.41332078621576329, 174.1589784336661637, -6.496448406907675876E-16 ) ) ;
#91491 = AXIS2_PLACEMENT_3D ( 'NONE', #95993, #42226, #58423 ) ;
#91492 = CARTESIAN_POINT ( 'NONE',  ( 185.1771979290287220, 295.2786484640562321, 8.360689780431474816 ) ) ;
#91493 = ORIENTED_EDGE ( 'NONE', *, *, #22519, .T. ) ;
#91494 = EDGE_LOOP ( 'NONE', ( #76513, #57135, #89151, #27284, #70194, #22447 ) ) ;
#91495 = CARTESIAN_POINT ( 'NONE',  ( 4.715407580134756138, 161.9824982072973683, 3.021315404115420679E-15 ) ) ;
#91496 = CARTESIAN_POINT ( 'NONE',  ( -13.76211276271278194, 162.8615022471903444, 5.188172501216621122E-14 ) ) ;
#91497 = EDGE_CURVE ( 'NONE', #51125, #72620, #71696, .T. ) ;
#91498 = CARTESIAN_POINT ( 'NONE',  ( 175.0803495703506769, 291.9523537460119655, 3.393087883739125399 ) ) ;
#91499 = DIRECTION ( 'NONE',  ( 1.000000000000000000, 0.000000000000000000, 0.000000000000000000 ) ) ;
#91500 = EDGE_CURVE ( 'NONE', #19199, #38977, #30285, .T. ) ;
#91501 = CARTESIAN_POINT ( 'NONE',  ( 162.5371025824206868, 249.1244755426497477, -11.58906134139951760 ) ) ;
#91502 = EDGE_CURVE ( 'NONE', #69479, #88281, #99197, .T. ) ;
#91503 = CARTESIAN_POINT ( 'NONE',  ( 83.42066707790206692, 44.47267527468968495, 8.844408096855449486 ) ) ;
#91504 = CARTESIAN_POINT ( 'NONE',  ( -48.36978223816941380, 29.22654356899180428, 10.00000000000000000 ) ) ;
#91505 = CARTESIAN_POINT ( 'NONE',  ( 18.30771692152332975, 187.5024278399160949, -9.188101187500093303 ) ) ;
#91506 = CARTESIAN_POINT ( 'NONE',  ( 125.9117204375048544, 237.3768266524159856, 9.188101187500098632 ) ) ;
#91507 = CARTESIAN_POINT ( 'NONE',  ( 182.0998838648946219, 294.4493588421104846, -6.417080199048857736 ) ) ;
#91508 = CARTESIAN_POINT ( 'NONE',  ( 183.6633101453114421, 256.8715506259877088, -3.169286389211312560 ) ) ;
#91509 = LINE ( 'NONE', #52969, #9234 ) ;
#91510 = FACE_OUTER_BOUND ( 'NONE', #87789, .T. ) ;
#91511 = CARTESIAN_POINT ( 'NONE',  ( 81.66084985466937951, 53.00684753587499642, -15.33431951212414646 ) ) ;
#91512 = CARTESIAN_POINT ( 'NONE',  ( 188.1160556981905358, 261.6047048220251554, 8.946321273836643329 ) ) ;
#91513 = DIRECTION ( 'NONE',  ( -1.000000000000000000, 0.000000000000000000, 1.082076799516502080E-16 ) ) ;
#91514 = CARTESIAN_POINT ( 'NONE',  ( 189.9056560155743796, 284.8180517316223472, 17.31073399879909047 ) ) ;
#91515 = CARTESIAN_POINT ( 'NONE',  ( 167.9520823679746684, 278.2100738273422280, 14.36288932855387657 ) ) ;
#91516 = CARTESIAN_POINT ( 'NONE',  ( 192.5741980485687463, 265.2346019687918215, 7.836594753621663578 ) ) ;
#91517 = CARTESIAN_POINT ( 'NONE',  ( 86.71718800452170228, 209.3262482093457493, 3.021315404115420679E-15 ) ) ;
#91518 = CARTESIAN_POINT ( 'NONE',  ( 164.6063343576543048, 274.4739709976624908, 16.17759516952312637 ) ) ;
#91519 = AXIS2_PLACEMENT_3D ( 'NONE', #13834, #20965, #37124 ) ;
#91520 = LINE ( 'NONE', #13020, #46447 ) ;
#91521 = EDGE_CURVE ( 'NONE', #983, #11813, #20918, .T. ) ;
#91522 = CARTESIAN_POINT ( 'NONE',  ( 183.8277868541691191, 269.1745150400024045, 15.18432627555796799 ) ) ;
#91523 = B_SPLINE_CURVE_WITH_KNOTS ( 'NONE', 3,
 ( #23880, #60872, #68486, #85235, #31478, #7184, #38071, #103, #77088, #53771, #14301, #39067, #45188, #46687, #6198, #69979, #68984, #593, #52780, #84733, #61383, #69489, #15273, #53291 ),
 .UNSPECIFIED., .F., .F.,
 ( 4, 2, 2, 2, 2, 2, 2, 2, 2, 2, 2, 4 ),
 ( 0.000000000000000000, 0.1249999999999943379, 0.2499999999999886757, 0.3749999999999830136, 0.4374999999999846789, 0.4999999999999863443, 0.5624999999999880096, 0.6249999999999897859, 0.6874999999999914513, 0.7499999999999932276, 0.8749999999999965583, 1.000000000000000000 ),
 .UNSPECIFIED. ) ;
#91524 = CARTESIAN_POINT ( 'NONE',  ( 103.3411068992554362, 218.2202760586659736, -5.415160957724236172E-17 ) ) ;
#91525 = CARTESIAN_POINT ( 'NONE',  ( 13.11890841201833169, 13.28920272979925166, -7.433330006724141015 ) ) ;
#91527 = CARTESIAN_POINT ( 'NONE',  ( 151.1926529451685326, 268.7736386982768408, 14.30343427984827365 ) ) ;
#91526 = AXIS2_PLACEMENT_3D ( 'NONE', #62569, #30702, #70688 ) ;
#91528 = CARTESIAN_POINT ( 'NONE',  ( 45.57373283677818421, 114.7827874512443032, -10.00000000000000000 ) ) ;
#91530 = CARTESIAN_POINT ( 'NONE',  ( 85.07585738814579202, 42.60566994075947633, -2.415354379879502300 ) ) ;
#91529 = CARTESIAN_POINT ( 'NONE',  ( -46.36014901014638667, 73.28484668120856327, -10.00000000000000000 ) ) ;
#91531 = CARTESIAN_POINT ( 'NONE',  ( 201.4530334248365762, 270.8746905162315670, -9.895680216334456603 ) ) ;
#91532 = CARTESIAN_POINT ( 'NONE',  ( 198.4344074287054696, 286.9485196940960918, -17.83642855442570152 ) ) ;
#91533 = CARTESIAN_POINT ( 'NONE',  ( 149.8302639188106866, 271.5858334631676030, -11.69480209898182110 ) ) ;
#91534 = CARTESIAN_POINT ( 'NONE',  ( 34.28181963472369631, 41.83396525600392835, -2.839279412974133887 ) ) ;
#91535 = CARTESIAN_POINT ( 'NONE',  ( 192.5284579606305613, 297.1779242397361713, -13.15228012403107272 ) ) ;
#91536 = CARTESIAN_POINT ( 'NONE',  ( -70.00000000000000000, 15.00000000000000000, -59.99999999999999289 ) ) ;
#91537 = VERTEX_POINT ( 'NONE', #31270 ) ;
#91538 = CARTESIAN_POINT ( 'NONE',  ( 24.17276070933917609, 32.14336893147756768, 7.433330006724141015 ) ) ;
#91539 = CARTESIAN_POINT ( 'NONE',  ( 157.9225728654248257, 276.1116997103654285, -12.95724163227552239 ) ) ;
#91540 = CARTESIAN_POINT ( 'NONE',  ( 147.5851099763508216, 275.0220864107570264, -4.372720440640867956 ) ) ;
#91541 = CARTESIAN_POINT ( 'NONE',  ( 149.2923684163597784, 272.0650280510108701, -12.99082738998495756 ) ) ;
#91542 = EDGE_LOOP ( 'NONE', ( #2855, #70493, #68380 ) ) ;
#91543 = CARTESIAN_POINT ( 'NONE',  ( 70.69455434939749239, 60.85083930861275547, 14.53159835427401880 ) ) ;
#91544 = CARTESIAN_POINT ( 'NONE',  ( 198.2414483977475754, 287.2827345394944700, 16.94931984969033678 ) ) ;
#91545 = CARTESIAN_POINT ( 'NONE',  ( 176.8917175299031896, 289.5346434493817469, -10.53293604869262978 ) ) ;
#91546 = CARTESIAN_POINT ( 'NONE',  ( 172.9204717250658234, 253.1639062637733275, -9.325132519940664722 ) ) ;
#91547 = CARTESIAN_POINT ( 'NONE',  ( 75.16643821786686885, 52.89298839225886439, -15.99447471506349672 ) ) ;
#91548 = CARTESIAN_POINT ( 'NONE',  ( 152.6615646578087819, 266.2294089801508221, 16.94722993326405813 ) ) ;
#91549 = ORIENTED_EDGE ( 'NONE', *, *, #12523, .T. ) ;
#91550 = CARTESIAN_POINT ( 'NONE',  ( 73.61926920126447271, 69.75873974038962899, 10.00767910897496193 ) ) ;
#91551 = ORIENTED_EDGE ( 'NONE', *, *, #11007, .F. ) ;
#91552 = CARTESIAN_POINT ( 'NONE',  ( 165.0109473288163997, 247.9890283962741080, 7.117481719421622444 ) ) ;
#91553 = CARTESIAN_POINT ( 'NONE',  ( 88.00349997577261263, 44.64923112938743088, 4.253506518527973235 ) ) ;
#91554 = VERTEX_POINT ( 'NONE', #62661 ) ;
#91555 = DIRECTION ( 'NONE',  ( -0.3037402332698226903, -0.8935232438716340653, 0.3306933373297776257 ) ) ;
#91556 = DIRECTION ( 'NONE',  ( -0.8660254037844387076, -0.4999999999999998890, -0.000000000000000000 ) ) ;
#91557 = CARTESIAN_POINT ( 'NONE',  ( 193.5421561915196094, 280.4896855936574411, -16.96249572231928937 ) ) ;
#91558 = CARTESIAN_POINT ( 'NONE',  ( 193.2629712555779236, 295.9057098940524497, -12.42285136223522635 ) ) ;
#91559 = CARTESIAN_POINT ( 'NONE',  ( 200.9812045408918380, 282.5373376992193926, -16.61165062382494284 ) ) ;
#91560 = EDGE_CURVE ( 'NONE', #59881, #40710, #50187, .T. ) ;
#91561 = CARTESIAN_POINT ( 'NONE',  ( 40.09738740370236343, 25.01110640527295104, 2.839279412974134775 ) ) ;
#91562 = CARTESIAN_POINT ( 'NONE',  ( 149.7854447168632817, 277.1467554076948545, 4.663160563959508842 ) ) ;
#91563 = CARTESIAN_POINT ( 'NONE',  ( 77.77867966053455007, 61.43039905302717330, -16.12786080876372807 ) ) ;
#91565 = VECTOR ( 'NONE', #3875, 1000.000000000000000 ) ;
#91564 = CARTESIAN_POINT ( 'NONE',  ( 87.39465943033326312, 45.50146518389362171, 7.088208788914807101 ) ) ;
#91566 = VERTEX_POINT ( 'NONE', #63175 ) ;
#91567 = ORIENTED_EDGE ( 'NONE', *, *, #74474, .T. ) ;
#91568 = CARTESIAN_POINT ( 'NONE',  ( 197.9778315518523755, 286.8276560105644535, 16.94107069242976138 ) ) ;
#91569 = CARTESIAN_POINT ( 'NONE',  ( 169.6029602999246606, 269.2276831600792093, 17.52968384675503088 ) ) ;
#91571 = DIRECTION ( 'NONE',  ( 0.8660254037844378194, 0.5000000000000015543, 0.000000000000000000 ) ) ;
#91570 = CARTESIAN_POINT ( 'NONE',  ( 164.2712161151136172, 246.1209027979328710, 7.276091357954241445 ) ) ;
#91572 = CARTESIAN_POINT ( 'NONE',  ( -16.22246322593621315, 60.00824852743482296, -10.00000000000000000 ) ) ;
#91573 = CARTESIAN_POINT ( 'NONE',  ( 197.9440596760970834, 272.2187063198555848, -13.59033992601415619 ) ) ;
#91574 = CARTESIAN_POINT ( 'NONE',  ( 72.92438617816932833, 61.44597022494355798, -14.84684155615548740 ) ) ;
#91575 = CARTESIAN_POINT ( 'NONE',  ( 82.09534214412946085, 40.77824446403596426, 1.263644830401252861 ) ) ;
#91576 = CARTESIAN_POINT ( 'NONE',  ( 170.9705878662882412, 287.7050143283094030, -4.597967457045799122 ) ) ;
#91577 = CARTESIAN_POINT ( 'NONE',  ( 76.99381129068922291, 63.91386138922637628, -15.28064156999390732 ) ) ;
#91578 = CARTESIAN_POINT ( 'NONE',  ( 186.2570902956351233, 286.9438662100191664, -16.14904440706751032 ) ) ;
#91579 = CARTESIAN_POINT ( 'NONE',  ( 105.2078667585768557, 240.7369531367911009, -4.594050593750048428 ) ) ;
#91580 = ORIENTED_EDGE ( 'NONE', *, *, #60172, .T. ) ;
#91581 = PLANE ( 'NONE',  #30208 ) ;
#91582 = CARTESIAN_POINT ( 'NONE',  ( 43.01361757626971638, 27.76004757982093452, 5.678558825948272215 ) ) ;
#91583 = CARTESIAN_POINT ( 'NONE',  ( 188.1536819913596048, 273.5597847156771536, 15.70283653734317042 ) ) ;
#91584 = EDGE_LOOP ( 'NONE', ( #7963, #34040, #18061, #693 ) ) ;
#91585 = VERTEX_POINT ( 'NONE', #93613 ) ;
#91586 = AXIS2_PLACEMENT_3D ( 'NONE', #68531, #30030, #60915 ) ;
#91587 = VECTOR ( 'NONE', #56075, 1000.000000000000114 ) ;
#91588 = CARTESIAN_POINT ( 'NONE',  ( 86.86990765421666083, 45.77415147683691288, -8.704208088459520098 ) ) ;
#91589 = CARTESIAN_POINT ( 'NONE',  ( 180.6056823850905744, 294.3695497894205459, -2.098957692436339784 ) ) ;
#91590 = CARTESIAN_POINT ( 'NONE',  ( 192.8319655484016835, 296.6522336772339941, 11.62706545001314673 ) ) ;
#91591 = CARTESIAN_POINT ( 'NONE',  ( 149.7247407264208618, 272.0633196944937140, -11.44969454563192279 ) ) ;
#91592 = DIRECTION ( 'NONE',  ( -0.9922852870422786964, 0.1239754375649568807, 0.000000000000000000 ) ) ;
#91593 = VERTEX_POINT ( 'NONE', #46459 ) ;
#91594 = VECTOR ( 'NONE', #42001, 1000.000000000000114 ) ;
#91595 = DIRECTION ( 'NONE',  ( 1.000000000000000000, 0.000000000000000000, -5.984665299743594308E-16 ) ) ;
#91596 = ORIENTED_EDGE ( 'NONE', *, *, #50395, .F. ) ;
#91597 = CARTESIAN_POINT ( 'NONE',  ( 37.46763966367993248, 203.9860189848785694, -2.679491924311201423 ) ) ;
#91598 = VERTEX_POINT ( 'NONE', #55063 ) ;
#91600 = DIRECTION ( 'NONE',  ( -0.5000000000000005551, 0.8660254037844384856, 0.000000000000000000 ) ) ;
#91599 = PRODUCT_DEFINITION_FORMATION_WITH_SPECIFIED_SOURCE ( 'ANY', '', #26520, .NOT_KNOWN. ) ;
#91601 = FACE_OUTER_BOUND ( 'NONE', #56814, .T. ) ;
#91602 = CARTESIAN_POINT ( 'NONE',  ( 175.2682827652102446, 270.4545196086085639, -17.77314019766468078 ) ) ;
#91603 = CARTESIAN_POINT ( 'NONE',  ( 82.43642368079662219, 44.97063798659471701, 10.10360692900326995 ) ) ;
#91605 = CARTESIAN_POINT ( 'NONE',  ( 159.0114971902875425, 280.6994106969128211, 5.657252936029947499 ) ) ;
#91604 = CARTESIAN_POINT ( 'NONE',  ( 198.2102933758524159, 286.2539132522722980, 17.34058952251382735 ) ) ;
#91606 = CARTESIAN_POINT ( 'NONE',  ( 200.9812045408918380, 282.5373376992193926, -16.61165062382494284 ) ) ;
#91607 = ORIENTED_EDGE ( 'NONE', *, *, #9145, .T. ) ;
#91608 = CARTESIAN_POINT ( 'NONE',  ( 58.36827475829091583, 216.0530062829863311, -4.648177544792955347E-16 ) ) ;
#91609 = FACE_OUTER_BOUND ( 'NONE', #44178, .T. ) ;
#91610 = CARTESIAN_POINT ( 'NONE',  ( 190.2591659045147310, 264.3349555848182604, -9.311233699776803263 ) ) ;
#91611 = CARTESIAN_POINT ( 'NONE',  ( 192.8229667366133810, 271.0818589901656424, 14.33785869832464499 ) ) ;
#91612 = CARTESIAN_POINT ( 'NONE',  ( 189.3508290737234745, 269.3566302321018497, -14.03381184610130994 ) ) ;
#91613 = EDGE_CURVE ( 'NONE', #16870, #27243, #61667, .T. ) ;
#91614 = CARTESIAN_POINT ( 'NONE',  ( 151.1237910559533475, 270.8929109891034841, -13.93008610078706688 ) ) ;
#91615 = CARTESIAN_POINT ( 'NONE',  ( 84.67330385480828170, 45.84957715147402268, 9.683287886809928580 ) ) ;
#91616 = EDGE_CURVE ( 'NONE', #65525, #29175, #61168, .T. ) ;
#91617 = CARTESIAN_POINT ( 'NONE',  ( 20.05933935144479108, 19.78052372038640527, -10.00000000000000355 ) ) ;
#91618 = CARTESIAN_POINT ( 'NONE',  ( 191.6801986094837105, 283.7096785499923044, -16.61112168735793659 ) ) ;
#91619 = B_SPLINE_CURVE_WITH_KNOTS ( 'NONE', 3,
 ( #79822, #95024, #55947, #96518, #18492, #73194, #65076, #56473, #79329, #9897, #33694, #48385, #2806, #2298, #57971, #27087 ),
 .UNSPECIFIED., .F., .F.,
 ( 4, 1, 2, 2, 2, 1, 2, 2, 4 ),
 ( 0.000000000000000000, 0.1250000000000056066, 0.1875000000000069111, 0.2500000000000082157, 0.5000000000000036637, 0.6250000000000013323, 0.6875000000000004441, 0.7499999999999994449, 1.000000000000000000 ),
 .UNSPECIFIED. ) ;
#91620 = CARTESIAN_POINT ( 'NONE',  ( 82.59012279121988342, 53.49374897786832150, -15.73261944071848539 ) ) ;
#91621 = EDGE_CURVE ( 'NONE', #69104, #43232, #20717, .T. ) ;
#91622 = CARTESIAN_POINT ( 'NONE',  ( 65.12704176573704729, 220.6589784336661637, -6.496448406907675876E-16 ) ) ;
#91623 = LINE ( 'NONE', #14599, #44336 ) ;
#91624 = CARTESIAN_POINT ( 'NONE',  ( 146.9978162861947908, 276.0393089210717790, -5.134868500856280882 ) ) ;
#91625 = CARTESIAN_POINT ( 'NONE',  ( -23.73952538801239598, 24.43184193311134678, -10.00000000000000000 ) ) ;
#91626 = EDGE_CURVE ( 'NONE', #41192, #86855, #70907, .T. ) ;
#91627 = DIRECTION ( 'NONE',  ( 0.8660254037844394848, 0.4999999999999986122, 0.000000000000000000 ) ) ;
#91628 = CIRCLE ( 'NONE', #47903, 70.00000000000001421 ) ;
#91629 = CARTESIAN_POINT ( 'NONE',  ( 207.8718670335145475, 270.6023601641878713, -6.322166851501095586 ) ) ;
#91630 = CARTESIAN_POINT ( 'NONE',  ( 58.10966550219799132, 178.3759306620403606, -17.47570218321536473 ) ) ;
#91631 = VECTOR ( 'NONE', #31008, 1000.000000000000000 ) ;
#91633 = CARTESIAN_POINT ( 'NONE',  ( -20.95882727533908252, 95.12657743062730731, 45.19937630303415688 ) ) ;
#91632 = CARTESIAN_POINT ( 'NONE',  ( 73.34072767760012823, 69.17406821459752564, -9.926094365178592227 ) ) ;
#91634 = CARTESIAN_POINT ( 'NONE',  ( 192.7686961758011250, 263.9209412561240811, -8.347089341778378468 ) ) ;
#91635 = CARTESIAN_POINT ( 'NONE',  ( 163.9801047297222283, 246.6251225080926588, -5.240962994374625872 ) ) ;
#91636 =( BOUNDED_CURVE ( )  B_SPLINE_CURVE ( 2, ( #54597, #78440, #47513, #61706, #92658, #62201, #77439, #69813, #93151 ),
 .UNSPECIFIED., .F., .T. ) 
 B_SPLINE_CURVE_WITH_KNOTS ( ( 3, 2, 2, 2, 3 ),
 ( 0.4072580645161290591, 0.4086021505376344343, 0.4112903225806451846, 0.4139784946236559349, 0.4153225806451613100 ),
 .UNSPECIFIED. ) 
 CURVE ( )  GEOMETRIC_REPRESENTATION_ITEM ( )  RATIONAL_B_SPLINE_CURVE ( ( 0.9330127018922194093, 0.9330127018922207416, 1.000000000000000000, 0.8660254037844387076, 1.000000000000000000, 0.8660254037844387076, 1.000000000000000000, 0.9330127018922194093, 0.9330127018922194093 ) ) 
 REPRESENTATION_ITEM ( '' )  );
#91637 = CARTESIAN_POINT ( 'NONE',  ( 82.07790669499631520, 54.04471111898705260, 15.60661167468746591 ) ) ;
#91638 = VECTOR ( 'NONE', #55515, 1000.000000000000114 ) ;
#91639 = CARTESIAN_POINT ( 'NONE',  ( 71.98582063699875278, 72.29727681381652360, 3.337216071139561979 ) ) ;
#91640 = CARTESIAN_POINT ( 'NONE',  ( 48.80796233711527776, 208.1744531367911293, 4.594050593750047540 ) ) ;
#91641 = CARTESIAN_POINT ( 'NONE',  ( 157.3363371328520088, 258.1324655395517311, 18.24585617226787093 ) ) ;
#91642 = CARTESIAN_POINT ( 'NONE',  ( 199.5508424383191368, 277.6004065077516429, 15.20186197903527336 ) ) ;
#91643 = CARTESIAN_POINT ( 'NONE',  ( 77.66081197416168891, 51.27534508892328802, -15.41764112584265334 ) ) ;
#91644 = CARTESIAN_POINT ( 'NONE',  ( 142.0139464194155039, 261.9869531367911009, 4.594050593750046652 ) ) ;
#91645 = CARTESIAN_POINT ( 'NONE',  ( 46.56179571999064137, 203.8149278399160949, -9.188101187500095079 ) ) ;
#91646 = B_SPLINE_CURVE_WITH_KNOTS ( 'NONE', 3,
 ( #85979, #83963, #61600, #39285, #77319, #91550, #75844, #55000, #93036, #62090, #14527, #313, #46908, #31201, #23592, #30215, #6431, #76810, #62591, #77830, #31685, #8413, #93547, #84459, #53011, #7925, #37308, #29719, #14999, #37799, #68208 ),
 .UNSPECIFIED., .F., .F.,
 ( 4, 3, 3, 3, 3, 3, 3, 3, 3, 3, 4 ),
 ( 0.000000000000000000, 0.1333490885032317663, 0.3007194338854262683, 0.4699862290245025997, 0.5844252810809391629, 0.6686540514502795629, 0.7354980260655534785, 0.8028463152565619154, 0.8633854507757232621, 0.9437142632667340214, 1.000000000000000000 ),
 .UNSPECIFIED. ) ;
#91647 = CARTESIAN_POINT ( 'NONE',  ( 21.31005897544419625, 27.70171378149919050, -9.188101187500004485 ) ) ;
#91648 = CARTESIAN_POINT ( 'NONE',  ( 171.3409795094679566, 286.6460634318879102, 7.397566566911762287 ) ) ;
#91649 = CARTESIAN_POINT ( 'NONE',  ( 149.6890529486499872, 271.3779502865075983, -12.51465682618088593 ) ) ;
#91650 = CARTESIAN_POINT ( 'NONE',  ( 44.67827877960949223, 26.76426979415094110, 3.090169943749476733 ) ) ;
#91651 = CARTESIAN_POINT ( 'NONE',  ( 204.6235849755581455, 276.2285497258825444, -13.59355699282649432 ) ) ;
#91652 = CARTESIAN_POINT ( 'NONE',  ( 76.62811072403027879, 63.82025679357946046, 14.86655239196480771 ) ) ;
#91653 = CARTESIAN_POINT ( 'NONE',  ( 76.34415836482729389, 61.31935459807998967, 15.96335647903723221 ) ) ;
#91654 = VECTOR ( 'NONE', #55566, 999.9999999999998863 ) ;
#91655 = CARTESIAN_POINT ( 'NONE',  ( 169.5727729373952002, 284.0798650663272156, -11.84966624384599676 ) ) ;
#91656 = CARTESIAN_POINT ( 'NONE',  ( 82.11871479691291142, 40.77613790009904449, -1.068313329471679562 ) ) ;
#91657 = CARTESIAN_POINT ( 'NONE',  ( 152.8305949863981255, 276.5798620968483306, 7.183986870886582388 ) ) ;
#91658 = AXIS2_PLACEMENT_3D ( 'NONE', #97861, #42139, #58335 ) ;
#91659 = DIRECTION ( 'NONE',  ( -0.8660254037844387076, -0.4999999999999998890, -0.000000000000000000 ) ) ;
#91660 = CARTESIAN_POINT ( 'NONE',  ( 87.68255615283939619, 45.40041221884136746, -6.563636875042941021 ) ) ;
#91661 = CARTESIAN_POINT ( 'NONE',  ( 94.49106271034210636, 235.3615022471903160, 5.000000000000046185 ) ) ;
#91662 = CARTESIAN_POINT ( 'NONE',  ( 200.2690241097007799, 283.7708703901988656, 16.96680019208369927 ) ) ;
#91663 = CARTESIAN_POINT ( 'NONE',  ( 165.2675333416819683, 269.7192504327577467, -16.28158008568958692 ) ) ;
#91664 = VERTEX_POINT ( 'NONE', #22689 ) ;
#91665 = CARTESIAN_POINT ( 'NONE',  ( 67.02199298016300588, 203.3768266524159856, -9.188101187500091527 ) ) ;
#91666 = ORIENTED_EDGE ( 'NONE', *, *, #26037, .T. ) ;
#91667 = CARTESIAN_POINT ( 'NONE',  ( 164.9673962408295722, 264.6939453157682465, 16.63392279346217606 ) ) ;
#91668 = CARTESIAN_POINT ( 'NONE',  ( 190.1696443193688708, 301.2635093119881162, -4.804312979389741223 ) ) ;
#91669 = CARTESIAN_POINT ( 'NONE',  ( 186.6728043966838868, 269.6571610938119079, 16.06727167421729163 ) ) ;
#91670 = ORIENTED_EDGE ( 'NONE', *, *, #38764, .F. ) ;
#91671 = EDGE_CURVE ( 'NONE', #3615, #64281, #72408, .T. ) ;
#91672 = CARTESIAN_POINT ( 'NONE',  ( 72.10617024684209753, 72.18421392457030095, 4.031754617348218162 ) ) ;
#91673 = LINE ( 'NONE', #23227, #79834 ) ;
#91674 = CARTESIAN_POINT ( 'NONE',  ( 194.1972774922283236, 294.2874440223457100, -15.09915398317898649 ) ) ;
#91675 = CARTESIAN_POINT ( 'NONE',  ( 85.75842679711398375, 42.78537197811905202, 3.771247107581231717 ) ) ;
#91676 = CYLINDRICAL_SURFACE ( 'NONE', #62829, 17.82106496071139645 ) ;
#91677 = EDGE_CURVE ( 'NONE', #25284, #84360, #57754, .T. ) ;
#91678 = CARTESIAN_POINT ( 'NONE',  ( 157.4843645388753544, 257.8760745514064183, 17.70049730742206862 ) ) ;
#91679 = EDGE_LOOP ( 'NONE', ( #55379, #67329, #10326, #97206 ) ) ;
#91680 = CARTESIAN_POINT ( 'NONE',  ( 20.33338779993010803, 20.24335787977762990, -9.188101187500008038 ) ) ;
#91681 = CARTESIAN_POINT ( 'NONE',  ( 175.2052744318867497, 254.7077291441659952, 7.835194671154784629 ) ) ;
#91682 = CARTESIAN_POINT ( 'NONE',  ( 43.24043327773039636, 120.8247932685368227, 10.00000000000000000 ) ) ;
#91683 = VERTEX_POINT ( 'NONE', #23165 ) ;
#91684 = CARTESIAN_POINT ( 'NONE',  ( -66.34925969370661392, 42.61035540433362456, -10.00000000000000000 ) ) ;
#91685 = CARTESIAN_POINT ( 'NONE',  ( 159.8188415394622268, 253.8326417772889840, -15.43862849427313222 ) ) ;
#91686 = VERTEX_POINT ( 'NONE', #78903 ) ;
#91687 = VERTEX_POINT ( 'NONE', #54056 ) ;
#91688 = CARTESIAN_POINT ( 'NONE',  ( 80.08925426792347935, 49.88496243973265365, -14.48658023246625604 ) ) ;
#91690 = PLANE ( 'NONE',  #62108 ) ;
#91689 = CARTESIAN_POINT ( 'NONE',  ( 159.4254556662896221, 282.2729508943065184, -3.240908821865370992 ) ) ;
#91691 = CARTESIAN_POINT ( 'NONE',  ( 208.1912724900461740, 270.0491336852600170, -0.9856800448607289100 ) ) ;
#91692 = CARTESIAN_POINT ( 'NONE',  ( 1.830000459568766003, 24.55466486950697202, 1.000260061240931054E-15 ) ) ;
#91693 = CARTESIAN_POINT ( 'NONE',  ( 159.8655504377736918, 253.7517395922482706, 15.51368179719542262 ) ) ;
#91694 = CARTESIAN_POINT ( 'NONE',  ( 164.5141650773065862, 265.0320900047184978, -16.63006306576538762 ) ) ;
#91695 = ADVANCED_FACE ( 'NONE', ( #85534 ), #15066, .T. ) ;
#91696 = CARTESIAN_POINT ( 'NONE',  ( 127.4269177983626236, 250.5024278399160949, -9.188101187500093303 ) ) ;
#91697 = CARTESIAN_POINT ( 'NONE',  ( 203.1072020527783479, 267.8656079271395924, 2.549640738347975333 ) ) ;
#91698 = CARTESIAN_POINT ( 'NONE',  ( 178.7125369615259558, 257.8607718938011431, 9.903824436443219525 ) ) ;
#91699 = CARTESIAN_POINT ( 'NONE',  ( 71.86588871287597158, 221.4869531367911293, 4.594050593750046652 ) ) ;
#91700 = ORIENTED_EDGE ( 'NONE', *, *, #34851, .F. ) ;
#91701 = CARTESIAN_POINT ( 'NONE',  ( 173.9684503405311204, 265.6129390675949367, 16.27754927923930950 ) ) ;
#91702 = CARTESIAN_POINT ( 'NONE',  ( 72.93270222632347100, 70.75261854202813083, -7.421515863126944446 ) ) ;
#91703 = DIRECTION ( 'NONE',  ( 0.8660254037844395958, 0.4999999999999985567, 0.000000000000000000 ) ) ;
#91704 = VECTOR ( 'NONE', #89069, 1000.000000000000000 ) ;
#91705 = ORIENTED_EDGE ( 'NONE', *, *, #58039, .T. ) ;
#91706 = FACE_OUTER_BOUND ( 'NONE', #12405, .T. ) ;
#91707 = ORIENTED_EDGE ( 'NONE', *, *, #48028, .F. ) ;
#91708 = VERTEX_POINT ( 'NONE', #8976 ) ;
#91709 = FACE_BOUND ( 'NONE', #62371, .T. ) ;
#91710 = CARTESIAN_POINT ( 'NONE',  ( 66.51083587138683129, 67.82564551438169076, 6.839597181675368454 ) ) ;
#91711 = CARTESIAN_POINT ( 'NONE',  ( 197.7287339728600841, 286.7199927125528234, 16.92603034138073426 ) ) ;
#91712 = B_SPLINE_CURVE_WITH_KNOTS ( 'NONE', 3,
 ( #43637, #74577, #50738, #81693, #27473, #19871, #58341, #36036, #44130, #75064, #42635, #11285, #49758, #43125, #26470, #28437, #73077, #82202, #80709, #3675, #5157, #26961, #66936, #34553 ),
 .UNSPECIFIED., .F., .F.,
 ( 4, 2, 2, 2, 2, 2, 2, 2, 2, 2, 2, 4 ),
 ( 0.000000000000000000, 0.1249999999999972522, 0.2499999999999945044, 0.3749999999999917843, 0.4374999999999891753, 0.4999999999999865663, 0.5624999999999840128, 0.6249999999999813483, 0.6874999999999787947, 0.7499999999999762412, 0.8749999999999881206, 1.000000000000000000 ),
 .UNSPECIFIED. ) ;
#91714 = B_SPLINE_SURFACE_WITH_KNOTS ( 'NONE', 3, 1, ( 
 ( #28653, #59535 ),
 ( #51963, #90002 ),
 ( #88532, #34757 ),
 ( #90515, #19093 ),
 ( #12484, #20577 ),
 ( #51457, #82424 ),
 ( #12989, #82904 ),
 ( #21087, #3395 ),
 ( #13476, #65657 ),
 ( #96615, #58066 ),
 ( #27178, #42838 ),
 ( #19599, #99564 ),
 ( #76274, #92974 ),
 ( #7341, #68147 ),
 ( #98586, #13962 ),
 ( #6848, #91486 ),
 ( #77249, #100069 ),
 ( #44841, #60533 ),
 ( #21565, #67655 ),
 ( #6364, #75777 ),
 ( #84388, #22049 ),
 ( #7856, #37248 ),
 ( #30147, #52448 ),
 ( #38224, #61032 ),
 ( #69642, #37734 ),
 ( #29169, #60037 ),
 ( #22552, #52949 ),
 ( #14461, #31130 ),
 ( #99073, #76748 ),
 ( #45343, #83898 ),
 ( #68643, #15942 ),
 ( #61540, #91002 ),
 ( #38736, #29655 ),
 ( #75278, #83393 ) ),
 .UNSPECIFIED., .T., .F., .F.,
 ( 4, 2, 2, 2, 2, 2, 2, 2, 2, 2, 2, 2, 2, 2, 2, 2, 4 ),
 ( 2, 2 ),
 ( 0.000000000000000000, 0.06250000000000000000, 0.1250000000000000000, 0.1875000000000000000, 0.2500000000000000000, 0.3125000000000000000, 0.3750000000000000000, 0.4375000000000000000, 0.5000000000000000000, 0.5625000000000000000, 0.6250000000000000000, 0.6875000000000000000, 0.7500000000000000000, 0.8125000000000000000, 0.8750000000000000000, 0.9375000000000000000, 1.000000000000000000 ),
 ( 0.000000000000000000, 1.000000000000000000 ),
 .UNSPECIFIED. ) ;
#91713 = CARTESIAN_POINT ( 'NONE',  ( 191.0862225170008628, 299.6759493045793192, -9.402218231374108726 ) ) ;
#91715 = CARTESIAN_POINT ( 'NONE',  ( 81.01777758920067640, 56.07228383068083843, 16.10439022756407468 ) ) ;
#91716 = CARTESIAN_POINT ( 'NONE',  ( 73.62250635243424313, 69.55784274833359859, 10.23584637956792776 ) ) ;
#91717 = AXIS2_PLACEMENT_3D ( 'NONE', #63022, #47315, #39689 ) ;
#91718 = CARTESIAN_POINT ( 'NONE',  ( 70.29920436004088913, 63.58999502166589934, 12.99331325176316376 ) ) ;
#91719 = VERTEX_POINT ( 'NONE', #85013 ) ;
#91720 = DIRECTION ( 'NONE',  ( -0.7300871660154473197, -0.6833540297821713017, 0.000000000000000000 ) ) ;
#91721 = VERTEX_POINT ( 'NONE', #15557 ) ;
#91722 = CARTESIAN_POINT ( 'NONE',  ( 76.13978442645490929, 51.56145741272602834, -16.17442695369989281 ) ) ;
#91723 = CARTESIAN_POINT ( 'NONE',  ( 183.6471037257901173, 275.7322458396929505, 17.25674916785948909 ) ) ;
#91724 = CARTESIAN_POINT ( 'NONE',  ( 206.2456893945931142, 273.4189824569319285, 10.13882547285618152 ) ) ;
#91725 = CARTESIAN_POINT ( 'NONE',  ( 148.9194629746633893, 272.7109192224475009, -12.27648025871169679 ) ) ;
#91726 = CARTESIAN_POINT ( 'NONE',  ( 42.09652578138359047, 195.1115022471902591, 10.00000000000009592 ) ) ;
#91727 = CARTESIAN_POINT ( 'NONE',  ( -19.65312891409030271, 93.06504152958497400, 59.99999999999999289 ) ) ;
#91728 = CARTESIAN_POINT ( 'NONE',  ( 134.1114646098825176, 257.4244531367911577, -4.594050593750046652 ) ) ;
#91729 = VERTEX_POINT ( 'NONE', #77390 ) ;
#91730 = VECTOR ( 'NONE', #86513, 1000.000000000000000 ) ;
#91731 = CARTESIAN_POINT ( 'NONE',  ( 87.88540012852695327, 44.32205958948441094, 4.765779035299133604 ) ) ;
#91732 = CARTESIAN_POINT ( 'NONE',  ( 86.48644980920353476, 45.02549005842475083, 7.069432882560119147 ) ) ;
#91733 = EDGE_CURVE ( 'NONE', #74751, #73620, #61774, .T. ) ;
#91734 = CARTESIAN_POINT ( 'NONE',  ( 79.89247370868126552, 44.63210057524135266, -11.16478091168645470 ) ) ;
#91735 = CARTESIAN_POINT ( 'NONE',  ( 152.9607371460978129, 265.7112270302071124, -16.17698032818104537 ) ) ;
#91736 = CARTESIAN_POINT ( 'NONE',  ( 72.85564822012069897, 70.83604795162270307, 7.235281746655774171 ) ) ;
#91737 = LINE ( 'NONE', #30398, #6563 ) ;
#91738 = VERTEX_POINT ( 'NONE', #16076 ) ;
#91739 = CARTESIAN_POINT ( 'NONE',  ( 195.8065633768937914, 265.4443555257707885, 4.436325927742740483 ) ) ;
#91740 = CARTESIAN_POINT ( 'NONE',  ( 46.99867368304094839, 76.19044720721625197, -10.00000000000000000 ) ) ;
#91741 = FACE_OUTER_BOUND ( 'NONE', #86471, .T. ) ;
#91742 = CARTESIAN_POINT ( 'NONE',  ( 184.7196529705373393, 263.5678720036872278, -12.47054388087118681 ) ) ;
#91743 = CARTESIAN_POINT ( 'NONE',  ( 198.9902718401575044, 266.4967149787970584, 0.8259339281635468266 ) ) ;
#91744 = CARTESIAN_POINT ( 'NONE',  ( 198.8214910967091669, 265.6694977507734734, 0.07193098711981385507 ) ) ;
#91745 = EDGE_CURVE ( 'NONE', #63141, #90758, #39209, .T. ) ;
#91746 = EDGE_LOOP ( 'NONE', ( #24373, #87145 ) ) ;
#91747 = CARTESIAN_POINT ( 'NONE',  ( 190.7403173041394950, 300.2750747078583800, -4.254144485856557800 ) ) ;
#91748 = CARTESIAN_POINT ( 'NONE',  ( 183.1289407222409693, 280.7186293386456555, 16.57674227110009113 ) ) ;
#91749 = CARTESIAN_POINT ( 'NONE',  ( 45.98627256186106393, 118.1229683434676900, -10.00000000000000000 ) ) ;
#91751 = CARTESIAN_POINT ( 'NONE',  ( 192.8158590921061943, 268.4179402270660830, 12.40538664778730826 ) ) ;
#91750 = CARTESIAN_POINT ( 'NONE',  ( 177.2629247679169850, 264.4881137859267710, -15.48121825248645500 ) ) ;
#91752 = CARTESIAN_POINT ( 'NONE',  ( 29.85841906089621389, 18.20801979619929867, -3.090169943749474069 ) ) ;
#91753 = DIRECTION ( 'NONE',  ( -0.000000000000000000, -0.000000000000000000, 1.000000000000000000 ) ) ;
#91754 = CARTESIAN_POINT ( 'NONE',  ( 78.37938175722123901, 209.3927522451418213, -10.00000000000009237 ) ) ;
#91755 = CARTESIAN_POINT ( 'NONE',  ( 67.75058886435806471, 69.10744749125690589, -5.632754406238772660 ) ) ;
#91756 = LINE ( 'NONE', #14720, #31735 ) ;
#91757 = CARTESIAN_POINT ( 'NONE',  ( -11.73236572436687730, 164.0333772461660544, 9.188101187500095079 ) ) ;
#91758 = CARTESIAN_POINT ( 'NONE',  ( -13.90296923609177959, 23.04100004375993649, -10.00000000000000000 ) ) ;
#91759 = ORIENTED_EDGE ( 'NONE', *, *, #11030, .T. ) ;
#91760 = CARTESIAN_POINT ( 'NONE',  ( 66.46435720904777611, 67.83184248247579262, -6.775977428004711811 ) ) ;
#91761 = CARTESIAN_POINT ( 'NONE',  ( 72.77745277708218907, 70.81288354178653321, -7.938184674006797614 ) ) ;
#91762 = CARTESIAN_POINT ( 'NONE',  ( 151.3999564459286375, 268.4145785023736153, -15.40574304386609050 ) ) ;
#91763 = CARTESIAN_POINT ( 'NONE',  ( 0.1751364819041374699, 183.1589784336661353, -6.496448406907676862E-16 ) ) ;
#91764 = VECTOR ( 'NONE', #67549, 1000.000000000000114 ) ;
#91765 = CARTESIAN_POINT ( 'NONE',  ( 172.1128792045810201, 290.3147750570036010, 2.746125360738576937 ) ) ;
#91766 = CARTESIAN_POINT ( 'NONE',  ( 180.4252347176669389, 274.7960680257757531, -16.49030086573319309 ) ) ;
#91767 = CARTESIAN_POINT ( 'NONE',  ( 22.59275855922847498, 34.81751292744058190, -6.180339887498951690 ) ) ;
#91768 = CARTESIAN_POINT ( 'NONE',  ( 85.06235871598175891, 48.90491807502699828, 12.39955041771802691 ) ) ;
#91769 = CARTESIAN_POINT ( 'NONE',  ( 170.3679664779006373, 270.9046122409516215, -17.49121570188935593 ) ) ;
#91771 = VECTOR ( 'NONE', #45657, 1000.000000000000114 ) ;
#91770 = PLANE ( 'NONE',  #8007 ) ;
#91772 = CARTESIAN_POINT ( 'NONE',  ( 150.1492354317374236, 276.5066157258622752, 3.807244489742962035 ) ) ;
#91773 = CARTESIAN_POINT ( 'NONE',  ( 177.8716437711887863, 254.8016637181727617, -3.895127477326730148 ) ) ;
#91774 = CARTESIAN_POINT ( 'NONE',  ( 191.0543065984834925, 261.4893840380978531, -1.560471719009105973 ) ) ;
#91776 = CARTESIAN_POINT ( 'NONE',  ( 182.9811911498659924, 295.6553585014947316, 1.023933121683335390 ) ) ;
#91775 = AXIS2_PLACEMENT_3D ( 'NONE', #92617, #86540, #47961 ) ;
#91777 = CARTESIAN_POINT ( 'NONE',  ( 58.91185237153150211, 191.4865022471901455, 1.119607411625061291E-15 ) ) ;
#91778 = LINE ( 'NONE', #22837, #34511 ) ;
#91779 = CARTESIAN_POINT ( 'NONE',  ( 147.9710862514405960, 274.3535558917855042, 7.785500222159708272 ) ) ;
#91780 = CARTESIAN_POINT ( 'NONE',  ( 20.41882739113040302, 182.5958772461660544, -9.188101187500095079 ) ) ;
#91781 = CARTESIAN_POINT ( 'NONE',  ( 72.60008616680404714, 70.69752196365911345, -7.958780822297746305 ) ) ;
#91782 = CARTESIAN_POINT ( 'NONE',  ( 72.58458169156800466, 71.41452113280901415, 5.739636480442070088 ) ) ;
#91783 = CARTESIAN_POINT ( 'NONE',  ( 38.30461122658549300, 34.06628583063844928, -9.188101187500006262 ) ) ;
#91784 = CARTESIAN_POINT ( 'NONE',  ( -19.65312891409030271, 93.06504152958497400, -10.00000000000000888 ) ) ;
#91785 = CARTESIAN_POINT ( 'NONE',  ( 164.9404048476745004, 244.9618339132846074, -2.801285734921658666 ) ) ;
#91786 = CARTESIAN_POINT ( 'NONE',  ( 185.2395268517200293, 266.6953418153134407, 13.39566909832231723 ) ) ;
#91787 = CARTESIAN_POINT ( 'NONE',  ( 79.14312167556931854, 57.64441083166269664, 0.000000000000000000 ) ) ;
#91788 = CARTESIAN_POINT ( 'NONE',  ( 164.0173503523412251, 281.8225298789022872, 9.954678856299715051 ) ) ;
#91789 = APPLICATION_PROTOCOL_DEFINITION ( 'draft international standard', 'automotive_design', 1998, #5503 ) ;
#91790 = CARTESIAN_POINT ( 'NONE',  ( 24.50893013558248157, 16.01110640527292261, 2.839279412974134775 ) ) ;
#91791 = CARTESIAN_POINT ( 'NONE',  ( 147.6220714307702622, 274.9580672937808572, 8.392894244419288441 ) ) ;
#91792 = CARTESIAN_POINT ( 'NONE',  ( 72.02510489751692546, 59.23144522310215621, 15.35746550185032255 ) ) ;
#91793 = ADVANCED_FACE ( 'NONE', ( #63677 ), #79427, .T. ) ;
#91794 = CARTESIAN_POINT ( 'NONE',  ( 155.5888570658010508, 261.1591898008976500, 17.34682632352454945 ) ) ;
#91795 = ORIENTED_EDGE ( 'NONE', *, *, #10271, .F. ) ;
#91796 = VECTOR ( 'NONE', #23481, 1000.000000000000000 ) ;
#91797 = CARTESIAN_POINT ( 'NONE',  ( 185.4839599128850693, 290.9053401448446152, 12.29227739265569674 ) ) ;
#91798 = CARTESIAN_POINT ( 'NONE',  ( 81.10000394050406669, 45.98558232817099878, -12.37583392106304458 ) ) ;
#91799 = CARTESIAN_POINT ( 'NONE',  ( 75.36487073175837281, 53.53173320265494795, -16.04382577248123809 ) ) ;
#91800 = CARTESIAN_POINT ( 'NONE',  ( 81.71275118201126020, 42.05154519778324129, 7.556033175796731172 ) ) ;
#91801 = PLANE ( 'NONE',  #86690 ) ;
#91802 = EDGE_CURVE ( 'NONE', #52500, #25226, #61646, .T. ) ;
#91803 = EDGE_LOOP ( 'NONE', ( #17212, #82598, #87517, #59393 ) ) ;
#91804 = DIRECTION ( 'NONE',  ( 0.2347357813929421555, -0.4065742997269585213, 0.8829475928589297640 ) ) ;
#91805 = CARTESIAN_POINT ( 'NONE',  ( 72.39195994751899832, 71.88450172447629427, -5.391213119607743742 ) ) ;
#91806 = CARTESIAN_POINT ( 'NONE',  ( 77.20977722794761178, 63.51083823537270945, 15.08832032918205357 ) ) ;
#91807 = CARTESIAN_POINT ( 'NONE',  ( 202.8535267948003593, 279.2943804273081696, -15.36804658072946062 ) ) ;
#91808 = ORIENTED_EDGE ( 'NONE', *, *, #96460, .F. ) ;
#91809 = ORIENTED_EDGE ( 'NONE', *, *, #17165, .T. ) ;
#91810 = CIRCLE ( 'NONE', #67545, 17.82106496071138224 ) ;
#91812 = CARTESIAN_POINT ( 'NONE',  ( 87.85430303351097336, 43.89859490532884223, 0.3596698246726173775 ) ) ;
#91811 = CARTESIAN_POINT ( 'NONE',  ( 74.93017357788674815, 189.2419560658248940, 5.188172501216619860E-14 ) ) ;
#91813 = B_SPLINE_CURVE_WITH_KNOTS ( 'NONE', 3,
 ( #34315, #20125, #26718, #34799, #73329, #88580, #4929, #19142, #65701, #96655, #27225, #58108, #50499, #50016, #57098, #81453 ),
 .UNSPECIFIED., .F., .F.,
 ( 4, 1, 2, 2, 2, 1, 2, 2, 4 ),
 ( 0.000000000000000000, 0.1250000000000047462, 0.1875000000000061062, 0.2500000000000074940, 0.5000000000000091038, 0.6250000000000103251, 0.6875000000000094369, 0.7500000000000085487, 1.000000000000000000 ),
 .UNSPECIFIED. ) ;
#91814 = ORIENTED_EDGE ( 'NONE', *, *, #35525, .T. ) ;
#91815 = CARTESIAN_POINT ( 'NONE',  ( 153.4542976351440302, 264.8563551865710224, -17.11782692037292009 ) ) ;
#91816 = CARTESIAN_POINT ( 'NONE',  ( 26.31557204471864253, 27.14441083166262203, 10.00000000000000533 ) ) ;
#91817 = CARTESIAN_POINT ( 'NONE',  ( 80.07172880487748046, 57.71088839156738715, 16.60216399474093762 ) ) ;
#91818 = CARTESIAN_POINT ( 'NONE',  ( 159.0906380018002153, 259.2649656523443582, -17.57712761084927067 ) ) ;
#91820 = EDGE_CURVE ( 'NONE', #8542, #54050, #63044, .T. ) ;
#91819 = ORIENTED_EDGE ( 'NONE', *, *, #30539, .F. ) ;
#91821 = CARTESIAN_POINT ( 'NONE',  ( 190.0515794655415789, 301.4680036374047063, -1.296825456579539626 ) ) ;
#91822 = CARTESIAN_POINT ( 'NONE',  ( 149.3801359649374092, 271.9130101976182914, -11.41245530317637424 ) ) ;
#91823 = ORIENTED_EDGE ( 'NONE', *, *, #9513, .T. ) ;
#91824 = CARTESIAN_POINT ( 'NONE',  ( 205.8610808625997208, 274.0851439753691920, 10.38803237360972531 ) ) ;
#91825 = DIRECTION ( 'NONE',  ( -1.000000000000000000, 0.000000000000000000, 0.000000000000000000 ) ) ;
#91826 = EDGE_LOOP ( 'NONE', ( #83891, #21797, #76468, #92261, #82873, #3829, #65618, #39229, #55502, #63807, #4063, #28257, #90477, #98537, #35814, #4328, #97937, #73242, #701, #31098, #64519, #60720, #50681, #36173, #81716, #32831, #22030, #45570, #29925, #40315, #80065, #27817, #70526, #70698, #97476, #69423, #72543, #23355, #34821, #90185, #84630, #8320, #40309, #25518 ) ) ;
#91827 = CARTESIAN_POINT ( 'NONE',  ( 190.7222376050763444, 300.3063896652212179, 3.365789908110941475 ) ) ;
#91828 = CARTESIAN_POINT ( 'NONE',  ( 78.37926235792471630, 47.32821374589490659, -14.23582365648701575 ) ) ;
#91829 = ORIENTED_EDGE ( 'NONE', *, *, #35429, .F. ) ;
#91830 = CARTESIAN_POINT ( 'NONE',  ( -17.01447213259276126, 75.00420231477963284, 13.39782861781775480 ) ) ;
#91831 = ADVANCED_FACE ( 'NONE', ( #27890 ), #80766, .F. ) ;
#91832 = CARTESIAN_POINT ( 'NONE',  ( 42.14088959202413776, 24.73415679381825427, -6.890680421881970419E-14 ) ) ;
#91833 = PLANE ( 'NONE',  #6201 ) ;
#91834 = CARTESIAN_POINT ( 'NONE',  ( 185.9406580756425171, 265.4572926502605128, 14.02042132963198817 ) ) ;
#91835 = ORIENTED_EDGE ( 'NONE', *, *, #17165, .F. ) ;
#91836 = VERTEX_POINT ( 'NONE', #86517 ) ;
#91837 = CARTESIAN_POINT ( 'NONE',  ( 156.4389512583130681, 266.4418172495878139, -16.23539328966390727 ) ) ;
#91838 = CARTESIAN_POINT ( 'NONE',  ( 88.22316733864592209, 44.26875609612613971, 2.029272769359137474 ) ) ;
#91839 = CARTESIAN_POINT ( 'NONE',  ( 50.33970617970973649, 92.06352491358971690, -10.00000000000000000 ) ) ;
#91840 = CARTESIAN_POINT ( 'NONE',  ( 82.35193903712398367, 53.76144841737798430, 15.84691369965402963 ) ) ;
#91841 = CARTESIAN_POINT ( 'NONE',  ( 149.6676065383367416, 271.4150965588098074, 11.80358707172367261 ) ) ;
#91842 = CARTESIAN_POINT ( 'NONE',  ( 170.8444319527499999, 275.3490660935767096, -16.15441094210034478 ) ) ;
#91843 = B_SPLINE_CURVE_WITH_KNOTS ( 'NONE', 3,
 ( #38744, #38233, #46332, #1263 ),
 .UNSPECIFIED., .F., .F.,
 ( 4, 4 ),
 ( 0.04153493918636062820, 0.04887066958154935581 ),
 .UNSPECIFIED. ) ;
#91844 = CARTESIAN_POINT ( 'NONE',  ( 191.3733179707528791, 299.1786853920590374, 9.861994297794856479 ) ) ;
#91845 = CARTESIAN_POINT ( 'NONE',  ( 147.2937583206075942, 275.5267222813735088, 0.1877253132609109920 ) ) ;
#91846 = CARTESIAN_POINT ( 'NONE',  ( 163.4180467003458261, 257.8218550979400447, 15.55521868025378218 ) ) ;
#91847 = B_SPLINE_CURVE_WITH_KNOTS ( 'NONE', 3,
 ( #19833, #29415, #97837, #6108, #28926, #90769, #58793, #52197, #67914, #50705, #83146, #37004, #98834, #51203, #12743, #43607, #28406, #59286, #14211, #29904, #7100, #6616, #85664, #47095 ),
 .UNSPECIFIED., .F., .F.,
 ( 4, 2, 2, 2, 2, 2, 2, 2, 2, 2, 2, 4 ),
 ( 0.000000000000000000, 0.1250000000000033029, 0.2500000000000066058, 0.3750000000000098810, 0.4375000000000053291, 0.5000000000000007772, 0.5624999999999962252, 0.6249999999999916733, 0.6874999999999871214, 0.7499999999999824585, 0.8749999999999912292, 1.000000000000000000 ),
 .UNSPECIFIED. ) ;
#91848 = VECTOR ( 'NONE', #43082, 1000.000000000000000 ) ;
#91849 = CARTESIAN_POINT ( 'NONE',  ( 69.91676562038409770, 67.50422961795942456, 9.414007674835353612 ) ) ;
#91851 = CARTESIAN_POINT ( 'NONE',  ( -13.51183432020139819, 142.4280072687214442, 0.000000000000000000 ) ) ;
#91850 = CARTESIAN_POINT ( 'NONE',  ( 149.6564118588553924, 271.4344863124460971, -11.76165597393390172 ) ) ;
#91852 = DIRECTION ( 'NONE',  ( -0.9606745773021526658, 0.2776767122488494333, 0.000000000000000000 ) ) ;
#91853 = CARTESIAN_POINT ( 'NONE',  ( 168.1067394590192521, 286.6168014624556122, 3.602430751267735598 ) ) ;
#91854 = CARTESIAN_POINT ( 'NONE',  ( 78.13762852215380406, 47.61987223718105611, 14.45360562616755828 ) ) ;
#91855 = AXIS2_PLACEMENT_3D ( 'NONE', #86997, #17525, #28616 ) ;
#91856 = ORIENTED_EDGE ( 'NONE', *, *, #72937, .T. ) ;
#91857 = CARTESIAN_POINT ( 'NONE',  ( 190.4558984197548170, 300.7677026662446451, -4.819771570275049655 ) ) ;
#91858 = EDGE_CURVE ( 'NONE', #24595, #78857, #39955, .T. ) ;
#91859 = CARTESIAN_POINT ( 'NONE',  ( 74.94274948198699349, 54.56384823593326416, -16.13558687890323995 ) ) ;
#91860 = EDGE_CURVE ( 'NONE', #37942, #61780, #23767, .T. ) ;
#91861 = CARTESIAN_POINT ( 'NONE',  ( 203.0126454322200402, 278.3859261051122189, 14.97126004913892139 ) ) ;
#91862 = CARTESIAN_POINT ( 'NONE',  ( 79.56664545794562571, 45.84018632621341283, 12.91967758877038897 ) ) ;
#91863 = CARTESIAN_POINT ( 'NONE',  ( 191.5873934714740301, 298.0279652477457262, -9.452854836254962478 ) ) ;
#91864 = CARTESIAN_POINT ( 'NONE',  ( 189.8449610424057425, 301.8258772440559028, -0.9803210874536477659 ) ) ;
#91865 = CARTESIAN_POINT ( 'NONE',  ( 166.2025478939213770, 283.6845846615859159, -8.127517485801055486 ) ) ;
#91866 = VERTEX_POINT ( 'NONE', #31732 ) ;
#91868 = EDGE_CURVE ( 'NONE', #23610, #26987, #40832, .T. ) ;
#91867 = CARTESIAN_POINT ( 'NONE',  ( 162.7070706717508699, 248.8300821762643693, -9.986337079333621247 ) ) ;
#91869 = VECTOR ( 'NONE', #98469, 1000.000000000000000 ) ;
#91870 = LINE ( 'NONE', #53316, #35474 ) ;
#91871 = CARTESIAN_POINT ( 'NONE',  ( 72.56680254073343406, 71.38637538794350235, 5.777867564336604644 ) ) ;
#91872 = CARTESIAN_POINT ( 'NONE',  ( 45.83126033165611091, 187.2677522451417929, -5.000000000000041744 ) ) ;
#91873 = CARTESIAN_POINT ( 'NONE',  ( 116.0331843058823296, 246.9869531367911293, 4.594050593750046652 ) ) ;
#91874 = CARTESIAN_POINT ( 'NONE',  ( 199.2205425252482200, 285.5868937652708155, -18.05012564782189344 ) ) ;
#91875 = EDGE_CURVE ( 'NONE', #85355, #52772, #25555, .T. ) ;
#91876 = AXIS2_PLACEMENT_3D ( 'NONE', #14039, #24995, #99147 ) ;
#91877 = DIRECTION ( 'NONE',  ( 0.5000000000000013323, -0.8660254037844378194, 0.000000000000000000 ) ) ;
#91878 = CARTESIAN_POINT ( 'NONE',  ( 157.8562613713738472, 257.2319303423452652, 17.81420683562559404 ) ) ;
#91879 = CARTESIAN_POINT ( 'NONE',  ( 172.8923325490025036, 251.6825938466021455, -3.947792175603512810 ) ) ;
#91880 = CARTESIAN_POINT ( 'NONE',  ( 33.40920844789697952, 190.0958772461660544, -9.188101187500095079 ) ) ;
#91881 = CARTESIAN_POINT ( 'NONE',  ( 147.8527080755910958, 276.5585929068648170, -2.411454450074328903 ) ) ;
#91882 = ORIENTED_EDGE ( 'NONE', *, *, #35886, .F. ) ;
#91884 = EDGE_CURVE ( 'NONE', #9692, #45778, #95764, .T. ) ;
#91883 = FACE_OUTER_BOUND ( 'NONE', #49460, .T. ) ;
#91885 = FACE_OUTER_BOUND ( 'NONE', #70147, .T. ) ;
#91886 = ADVANCED_FACE ( 'NONE', ( #18070 ), #2886, .F. ) ;
#91887 = LINE ( 'NONE', #62414, #64338 ) ;
#91888 = CARTESIAN_POINT ( 'NONE',  ( 147.5498377207569263, 275.0831797495432056, 4.097967709737811326 ) ) ;
#91889 = CARTESIAN_POINT ( 'NONE',  ( 81.86592541406376711, 41.15561125584435587, -5.581452205721086024 ) ) ;
#91890 = FACE_OUTER_BOUND ( 'NONE', #69515, .T. ) ;
#91891 = CARTESIAN_POINT ( 'NONE',  ( 68.55042658866229033, 64.21781301378140938, -12.45171015595362540 ) ) ;
#91892 = VECTOR ( 'NONE', #24554, 1000.000000000000000 ) ;
#91893 = CARTESIAN_POINT ( 'NONE',  ( 110.7831656154890254, 224.7677522451417929, -5.000000000000041744 ) ) ;
#91894 = CARTESIAN_POINT ( 'NONE',  ( 194.3452430042056847, 293.4673175397701357, -14.50972866970454866 ) ) ;
#91895 = ORIENTED_EDGE ( 'NONE', *, *, #21395, .T. ) ;
#91896 = FACE_OUTER_BOUND ( 'NONE', #47240, .T. ) ;
#91897 = CARTESIAN_POINT ( 'NONE',  ( 78.60735446187601383, 47.91558663937575346, -14.46554739992949834 ) ) ;
#91898 = CARTESIAN_POINT ( 'NONE',  ( 15.70964071017000663, 186.0024278399160949, -9.188101187500093303 ) ) ;
#91899 = CARTESIAN_POINT ( 'NONE',  ( 6.588875291771465470, 26.73705186507752174, -3.090169943749475845 ) ) ;
#91900 = CARTESIAN_POINT ( 'NONE',  ( 196.2097543372840391, 273.6352822109456611, 15.01336023606802783 ) ) ;
#91901 = CARTESIAN_POINT ( 'NONE',  ( 71.49043722402748813, 59.12641653362435079, -15.80154365645430836 ) ) ;
#91902 = FACE_OUTER_BOUND ( 'NONE', #41036, .T. ) ;
#91904 = CARTESIAN_POINT ( 'NONE',  ( 72.54290492928882372, 206.5643266524159571, -9.188101187500093303 ) ) ;
#91903 = CARTESIAN_POINT ( 'NONE',  ( 175.1643429085319497, 286.5391626044407190, 10.49485163562685663 ) ) ;
#91905 = CYLINDRICAL_SURFACE ( 'NONE', #60290, 10.00000000000010658 ) ;
#91906 = CARTESIAN_POINT ( 'NONE',  ( 73.58947491971605359, 55.55901669400043374, 16.10573162174744155 ) ) ;
#91907 = CARTESIAN_POINT ( 'NONE',  ( -30.02137776312446960, 96.47624038658500467, 44.61044380647359731 ) ) ;
#91909 = B_SPLINE_CURVE_WITH_KNOTS ( 'NONE', 3,
 ( #66743, #73862, #66258, #81496, #27760, #12065, #59119, #98172, #28750, #65741 ),
 .UNSPECIFIED., .F., .F.,
 ( 4, 2, 2, 2, 4 ),
 ( 0.000000000000000000, 0.2500000000000000000, 0.5000000000000000000, 0.7500000000000000000, 1.000000000000000000 ),
 .UNSPECIFIED. ) ;
#91908 = CARTESIAN_POINT ( 'NONE',  ( 66.31978875953279839, 68.10230444367267921, -4.579799779162929241 ) ) ;
#91910 = ORIENTED_EDGE ( 'NONE', *, *, #67686, .T. ) ;
#91911 = CARTESIAN_POINT ( 'NONE',  ( 18.28082717731156848, 171.3615022471901739, 5.000000000000051514 ) ) ;
#91912 = CARTESIAN_POINT ( 'NONE',  ( 164.4698008747318738, 245.7769439046653019, -6.272955660526681854 ) ) ;
#91913 = AXIS2_PLACEMENT_3D ( 'NONE', #20099, #3889, #12498 ) ;
#91914 = CARTESIAN_POINT ( 'NONE',  ( 136.0871718362070339, 255.5024278399161233, 9.188101187500095079 ) ) ;
#91915 = CARTESIAN_POINT ( 'NONE',  ( 28.07469292777547309, 37.18502408145594273, 5.678558825948277544 ) ) ;
#91916 = CARTESIAN_POINT ( 'NONE',  ( 167.7336762235300682, 262.4260227015225269, -16.94079744808321664 ) ) ;
#91917 = CARTESIAN_POINT ( 'NONE',  ( 66.43953443436691941, 68.06212878376058484, -4.898982275787033380 ) ) ;
#91918 = CARTESIAN_POINT ( 'NONE',  ( 198.4753670019441643, 282.2770161063888281, -17.61508457932132288 ) ) ;
#91920 = CARTESIAN_POINT ( 'NONE',  ( 110.0000000000000000, 15.00000000000003908, 59.99999999999999289 ) ) ;
#91919 = CARTESIAN_POINT ( 'NONE',  ( -76.23101443460923576, 54.01191295053621388, -10.00000000000000000 ) ) ;
#91921 = CARTESIAN_POINT ( 'NONE',  ( -63.30067564770008914, 39.94154026010144065, -10.00000000000000000 ) ) ;
#91922 = ORIENTED_EDGE ( 'NONE', *, *, #15013, .T. ) ;
#91923 = CARTESIAN_POINT ( 'NONE',  ( 60.12067949409930634, 205.5177522451418497, -10.00000000000009592 ) ) ;
#91924 = DIRECTION ( 'NONE',  ( 0.000000000000000000, 0.000000000000000000, 1.000000000000000000 ) ) ;
#91925 = CIRCLE ( 'NONE', #48206, 70.00000000000001421 ) ;
#91926 = CARTESIAN_POINT ( 'NONE',  ( 181.2434141109869756, 287.9121743413131185, 13.99700062213659280 ) ) ;
#91927 = CARTESIAN_POINT ( 'NONE',  ( 156.6019793714546893, 280.4068591911544672, -5.433895450329538690 ) ) ;
#91928 = CARTESIAN_POINT ( 'NONE',  ( -17.42236680055705023, 149.2012482093457777, 0.000000000000000000 ) ) ;
#91929 = ORIENTED_EDGE ( 'NONE', *, *, #57812, .F. ) ;
#91930 = CARTESIAN_POINT ( 'NONE',  ( 160.1554125499368411, 253.2496836867922809, 14.66957084865053140 ) ) ;
#91931 = ADVANCED_FACE ( 'NONE', ( #78881 ), #48966, .F. ) ;
#91932 = VECTOR ( 'NONE', #34723, 1000.000000000000114 ) ;
#91933 = CARTESIAN_POINT ( 'NONE',  ( 168.0402147318401944, 281.8818710449446598, -11.04375926519547768 ) ) ;
#91934 = B_SPLINE_CURVE_WITH_KNOTS ( 'NONE', 3,
 ( #87908, #60269, #4743, #34144, #3749, #2759, #18451, #56919, #41722, #26547, #34626, #35121, #96475, #89392, #11849, #91223, #27044, #57925, #50324, #66032, #35627, #81276, #73639, #4222, #21791, #19943, #81767, #54162, #38473, #93731, #8097, #47081, #70383, #31871, #24290, #490, #85124, #99309, #84143, #84625, #62773, #22288, #37473, #6599, #46066, #990, #69385, #91723, #92723, #77505, #30888, #55167 ),
 .UNSPECIFIED., .F., .F.,
 ( 4, 2, 2, 2, 2, 2, 2, 2, 2, 2, 2, 2, 2, 2, 2, 2, 2, 2, 2, 2, 2, 2, 2, 2, 2, 4 ),
 ( 0.0002653169772839772465, 0.0007391932915139334034, 0.001213069605743889723, 0.001450007762858867774, 0.001568476841416391711, 0.001686945919973915865, 0.001805414998531439802, 0.001923884077088963739, 0.002160822234204006192, 0.002634698548434018673, 0.003108574862664031588, 0.004056327491123986294, 0.005004080119583941000, 0.005477956433813918787, 0.005714894590928907246, 0.005833363669486404078, 0.005892598208765155096, 0.005951832748043906114, 0.006011067287322656265, 0.006070301826601406416, 0.006188770905158779215, 0.006425709062273484047, 0.006899585376502746260, 0.007136523533617395582, 0.007373461690732044035, 0.007847338004961328800 ),
 .UNSPECIFIED. ) ;
#91935 = EDGE_CURVE ( 'NONE', #65525, #72951, #62588, .T. ) ;
#91936 = DIRECTION ( 'NONE',  ( -0.9839629614562445115, 0.1783728972749415165, 0.000000000000000000 ) ) ;
#91937 = FACE_OUTER_BOUND ( 'NONE', #54378, .T. ) ;
#91938 = CARTESIAN_POINT ( 'NONE',  ( 89.99855592466239784, 232.7677522451419065, -5.000000000000047962 ) ) ;
#91939 = CARTESIAN_POINT ( 'NONE',  ( 207.9328781051891042, 270.4966858882232259, -0.8820402142964423042 ) ) ;
#91940 = CARTESIAN_POINT ( 'NONE',  ( 153.3939648708017387, 264.9608545997728015, -16.49556533540763681 ) ) ;
#91941 = VECTOR ( 'NONE', #42010, 1000.000000000000000 ) ;
#91942 =( BOUNDED_CURVE ( )  B_SPLINE_CURVE ( 2, ( #65867, #82634, #26888, #19314, #97307, #59243, #96825, #4076, #36463 ),
 .UNSPECIFIED., .F., .T. ) 
 B_SPLINE_CURVE_WITH_KNOTS ( ( 3, 2, 2, 2, 3 ),
 ( 0.2701612903225806273, 0.2715053763440860024, 0.2741935483870967527, 0.2768817204301075030, 0.2782258064516128782 ),
 .UNSPECIFIED. ) 
 CURVE ( )  GEOMETRIC_REPRESENTATION_ITEM ( )  RATIONAL_B_SPLINE_CURVE ( ( 0.9330127018922194093, 0.9330127018922194093, 1.000000000000000000, 0.8660254037844387076, 1.000000000000000000, 0.8660254037844387076, 1.000000000000000000, 0.9330127018922194093, 0.9330127018922194093 ) ) 
 REPRESENTATION_ITEM ( '' )  );
#91943 = CARTESIAN_POINT ( 'NONE',  ( -19.65312891409030271, 93.06504152958497400, 177.5919119679930134 ) ) ;
#91944 = CARTESIAN_POINT ( 'NONE',  ( 18.14948940725119897, 10.28848085856230377, 1.475505719884397138E-15 ) ) ;
#91945 = CARTESIAN_POINT ( 'NONE',  ( 86.46048006423903587, 47.32182001325401899, 10.26516935212321258 ) ) ;
#91946 = ORIENTED_EDGE ( 'NONE', *, *, #83257, .F. ) ;
#91947 = CARTESIAN_POINT ( 'NONE',  ( 149.5633513747893346, 271.5956717990251832, 12.83777201928511325 ) ) ;
#91948 = CARTESIAN_POINT ( 'NONE',  ( 86.46734690923850053, 47.05374834302038067, -10.53985889464876458 ) ) ;
#91949 = CARTESIAN_POINT ( 'NONE',  ( 80.52777769245514605, 45.62452705624884430, -11.72524612028085222 ) ) ;
#91951 = EDGE_CURVE ( 'NONE', #29135, #22165, #98053, .T. ) ;
#91950 = ORIENTED_EDGE ( 'NONE', *, *, #49755, .F. ) ;
#91952 = CARTESIAN_POINT ( 'NONE',  ( 147.2180753513904961, 275.6578090293250511, 0.4909717733184589261 ) ) ;
#91953 = FACE_OUTER_BOUND ( 'NONE', #18692, .T. ) ;
#91954 = AXIS2_PLACEMENT_3D ( 'NONE', #48329, #54394, #9327 ) ;
#91955 = CARTESIAN_POINT ( 'NONE',  ( 164.4936379324916516, 245.7356569095223051, 6.719479797016231437 ) ) ;
#91956 = CARTESIAN_POINT ( 'NONE',  ( 74.92809311542137607, 53.46823265460128738, -16.53855748461180752 ) ) ;
#91957 = CARTESIAN_POINT ( 'NONE',  ( 69.40575591891894192, 62.79509274011370223, 13.16381358185486405 ) ) ;
#91958 = VERTEX_POINT ( 'NONE', #24649 ) ;
#91959 = CARTESIAN_POINT ( 'NONE',  ( 95.14032143958276322, 234.9244531367911009, -4.594050593750046652 ) ) ;
#91960 = CARTESIAN_POINT ( 'NONE',  ( 155.7926064421430112, 260.8062855290629045, 17.74927770606829469 ) ) ;
#91961 = CARTESIAN_POINT ( 'NONE',  ( 73.32155222933093341, 69.66094733087366819, -9.921889652296787432 ) ) ;
#91962 = CARTESIAN_POINT ( 'NONE',  ( 81.80835978698212330, 42.34965515190965846, -7.954336405571433843 ) ) ;
#91963 = B_SPLINE_SURFACE_WITH_KNOTS ( 'NONE', 3, 1, ( 
 ( #72582, #73559 ),
 ( #65943, #57341 ),
 ( #58336, #10764 ),
 ( #5151, #42140 ),
 ( #34548, #73072 ),
 ( #95415, #49752 ),
 ( #41639, #66446 ),
 ( #89312, #20360 ),
 ( #58822, #34071 ),
 ( #80704, #25971 ),
 ( #89784, #95907 ),
 ( #50733, #81688 ),
 ( #3670, #65446 ),
 ( #57839, #88819 ),
 ( #13737, #66932 ),
 ( #28433, #39385 ),
 ( #44617, #29440 ),
 ( #16604, #53234 ),
 ( #21837, #83682 ),
 ( #93649, #60810 ),
 ( #21346, #14243 ),
 ( #8516, #90794 ),
 ( #24214, #75552 ),
 ( #9009, #55095 ),
 ( #47503, #20864 ),
 ( #75060, #52722 ),
 ( #37522, #67942 ),
 ( #83175, #59315 ),
 ( #86082, #60314 ),
 ( #84186, #29933 ),
 ( #62693, #45129 ) ),
 .UNSPECIFIED., .F., .F., .F.,
 ( 4, 3, 3, 3, 3, 3, 3, 3, 3, 3, 4 ),
 ( 2, 2 ),
 ( 0.000000000000000000, 0.1333490885032340423, 0.3007194338854312643, 0.4699862290245129803, 0.5844252810809342780, 0.6686540514502644639, 0.7354980260655447077, 0.8028463152565625816, 0.8633854507757121599, 0.9437142632667110398, 1.000000000000000000 ),
 ( 0.000000000000000000, 1.000000000000000000 ),
 .UNSPECIFIED. ) ;
#91964 = ORIENTED_EDGE ( 'NONE', *, *, #23322, .F. ) ;
#91965 = EDGE_CURVE ( 'NONE', #49112, #19562, #70205, .T. ) ;
#91966 = ORIENTED_EDGE ( 'NONE', *, *, #75286, .F. ) ;
#91967 = EDGE_CURVE ( 'NONE', #10047, #8803, #35250, .T. ) ;
#91968 = EDGE_LOOP ( 'NONE', ( #30755, #85386, #92827, #69363 ) ) ;
#91969 = CARTESIAN_POINT ( 'NONE',  ( 81.27747349237425567, 49.50046732535272298, 14.00627724909530691 ) ) ;
#91970 = ORIENTED_EDGE ( 'NONE', *, *, #77413, .T. ) ;
#91971 = CARTESIAN_POINT ( 'NONE',  ( 68.17307502523176765, 68.36170032566508326, 6.558107242125284841 ) ) ;
#91972 = VERTEX_POINT ( 'NONE', #11487 ) ;
#91973 = CARTESIAN_POINT ( 'NONE',  ( 164.0179800784044915, 246.5595204798204065, -5.772998092557310557 ) ) ;
#91974 = AXIS2_PLACEMENT_3D ( 'NONE', #36635, #97482, #13848 ) ;
#91975 = CARTESIAN_POINT ( 'NONE',  ( 80.66987298107778770, 24.99999999999998579, -10.00000000000000178 ) ) ;
#91976 = CARTESIAN_POINT ( 'NONE',  ( 192.3926678149021825, 295.4131196713046847, -13.42882169270698256 ) ) ;
#91977 = CARTESIAN_POINT ( 'NONE',  ( 17.48697055717582316, 174.2365022471902023, -10.00000000000009237 ) ) ;
#91978 = CARTESIAN_POINT ( 'NONE',  ( 70.30291785998953458, 68.43742151735528978, -8.517849549379890917 ) ) ;
#91980 = CARTESIAN_POINT ( 'NONE',  ( 80.07214027775873433, 55.25082771389860170, -16.41292865798596878 ) ) ;
#91979 = B_SPLINE_CURVE_WITH_KNOTS ( 'NONE', 3,
 ( #56807, #96860, #18334, #65903, #49228, #88277 ),
 .UNSPECIFIED., .F., .F.,
 ( 4, 2, 4 ),
 ( 0.02208471075069790360, 0.02668293858277623332, 0.03128116641485456650 ),
 .UNSPECIFIED. ) ;
#91981 = CARTESIAN_POINT ( 'NONE',  ( 21.59269996301512862, 13.26216523072493914, -2.296566073217252530E-15 ) ) ;
#91982 = CARTESIAN_POINT ( 'NONE',  ( 163.4341025207368716, 282.8476932499685859, 9.116081536633066307 ) ) ;
#91983 = FACE_OUTER_BOUND ( 'NONE', #36312, .T. ) ;
#91985 = ORIENTED_EDGE ( 'NONE', *, *, #40345, .F. ) ;
#91984 = CARTESIAN_POINT ( 'NONE',  ( 74.14312167556930433, 66.30466486950707861, 1.224646799147354045E-15 ) ) ;
#91986 = ADVANCED_FACE ( 'NONE', ( #66649 ), #3386, .T. ) ;
#91987 = CARTESIAN_POINT ( 'NONE',  ( 163.4004183463084416, 247.6291687766210146, 10.19167732382099345 ) ) ;
#91988 = CARTESIAN_POINT ( 'NONE',  ( 187.5027153640760105, 260.3852002302687083, 2.859512323897527963 ) ) ;
#91989 = CARTESIAN_POINT ( 'NONE',  ( 48.21858077004885246, 104.0489273421469818, -10.00000000000000000 ) ) ;
#91990 = CARTESIAN_POINT ( 'NONE',  ( 81.43726257051942241, 46.06824199903791595, -11.66015455581693061 ) ) ;
#91991 = CARTESIAN_POINT ( 'NONE',  ( 171.7256454430782924, 255.0603003222375378, 10.96627809234114359 ) ) ;
#91992 = CARTESIAN_POINT ( 'NONE',  ( 158.8074424692007938, 281.4784585291520784, 2.074645808957411575 ) ) ;
#91993 = VERTEX_POINT ( 'NONE', #13466 ) ;
#91995 = EDGE_CURVE ( 'NONE', #130, #61735, #36486, .T. ) ;
#91994 = CARTESIAN_POINT ( 'NONE',  ( 41.10966550219804816, 207.8207943907112565, -18.47570218321542868 ) ) ;
#91996 = CARTESIAN_POINT ( 'NONE',  ( 74.79855439552166274, 62.33245921625753994, -14.96095770982128847 ) ) ;
#91997 = AXIS2_PLACEMENT_3D ( 'NONE', #66027, #75136, #89862 ) ;
#91998 = DIRECTION ( 'NONE',  ( -0.04056776950001317328, 0.9991767892008870389, 0.000000000000000000 ) ) ;
#91999 = CARTESIAN_POINT ( 'NONE',  ( -1.439292958244568821, 176.6427522451419065, 10.00000000000009237 ) ) ;
#92000 = CARTESIAN_POINT ( 'NONE',  ( 82.83316871194540454, 53.40219886645672176, -15.30257817068320847 ) ) ;
#92001 = VECTOR ( 'NONE', #11664, 1000.000000000000000 ) ;
#92002 = EDGE_CURVE ( 'NONE', #56559, #2820, #28054, .T. ) ;
#92003 = CARTESIAN_POINT ( 'NONE',  ( 174.9330555342984610, 281.7317282589606862, -14.07090496212465069 ) ) ;
#92004 = CARTESIAN_POINT ( 'NONE',  ( 193.8848781386269309, 267.1185884883711879, -11.59377028749509364 ) ) ;
#92005 = CARTESIAN_POINT ( 'NONE',  ( 72.08719088798999053, 72.32551850972336638, 0.8194835739893685522 ) ) ;
#92006 = CIRCLE ( 'NONE', #90341, 2.471954595299370006 ) ;
#92007 = CARTESIAN_POINT ( 'NONE',  ( 162.2842013956643825, 250.7983415291583071, -12.77801933371535448 ) ) ;
#92009 = FACE_OUTER_BOUND ( 'NONE', #27504, .T. ) ;
#92008 = CARTESIAN_POINT ( 'NONE',  ( 0.5816933075168655431, 161.9548013555410080, -4.594050593750042211 ) ) ;
#92010 = CARTESIAN_POINT ( 'NONE',  ( 16.79905537663784898, 192.0530062829863311, -4.648177544792955347E-16 ) ) ;
#92011 = ORIENTED_EDGE ( 'NONE', *, *, #64033, .F. ) ;
#92012 = VECTOR ( 'NONE', #61764, 1000.000000000000000 ) ;
#92013 = EDGE_CURVE ( 'NONE', #4221, #81160, #78829, .T. ) ;
#92014 = VERTEX_POINT ( 'NONE', #88521 ) ;
#92015 = CARTESIAN_POINT ( 'NONE',  ( 49.74924850768366724, 83.93760989710260390, 177.5919119679930134 ) ) ;
#92016 = FACE_OUTER_BOUND ( 'NONE', #8928, .T. ) ;
#92017 = CARTESIAN_POINT ( 'NONE',  ( 152.7122812589697958, 277.9324518551267147, 6.933031942251369983 ) ) ;
#92018 = LINE ( 'NONE', #76287, #63103 ) ;
#92019 = CARTESIAN_POINT ( 'NONE',  ( 162.9923277572749214, 248.3360024109179847, -11.73806682979623695 ) ) ;
#92020 = VECTOR ( 'NONE', #182, 1000.000000000000114 ) ;
#92021 = CARTESIAN_POINT ( 'NONE',  ( 153.4490520802545177, 279.2845403698434552, 3.866127127660768714 ) ) ;
#92022 = CARTESIAN_POINT ( 'NONE',  ( 20.90579313287664220, 189.0024278399160949, -9.188101187500093303 ) ) ;
#92023 = CARTESIAN_POINT ( 'NONE',  ( 119.6601863278771845, 230.7048013555409796, 4.594050593750051981 ) ) ;
#92024 = CARTESIAN_POINT ( 'NONE',  ( 179.8548388294205438, 292.4099480123907142, -6.160154682680708760 ) ) ;
#92025 = CARTESIAN_POINT ( 'NONE',  ( 170.4037115821164434, 284.7129311807937029, 11.70618658742957940 ) ) ;
#92026 = CARTESIAN_POINT ( 'NONE',  ( 149.9807464961409664, 271.6463072190915682, -11.70746914540981010 ) ) ;
#92027 = CARTESIAN_POINT ( 'NONE',  ( 178.3812519316271903, 283.9015146232569009, -15.02767978356603962 ) ) ;
#92028 = CARTESIAN_POINT ( 'NONE',  ( 78.82139251731592822, 54.02149238465010939, -15.89892391852131048 ) ) ;
#92029 = FACE_OUTER_BOUND ( 'NONE', #27329, .T. ) ;
#92030 = CARTESIAN_POINT ( 'NONE',  ( 154.9455285025717615, 262.2734675583710100, 18.28470720339922551 ) ) ;
#92031 = CARTESIAN_POINT ( 'NONE',  ( 184.2649791758939273, 274.6463348420198258, 16.49567768463042583 ) ) ;
#92032 = CARTESIAN_POINT ( 'NONE',  ( 190.1045438606958271, 284.8339252823208199, 16.91879847483513188 ) ) ;
#92033 = CARTESIAN_POINT ( 'NONE',  ( 167.8099627665611706, 278.1935700092135448, 14.45340646069998947 ) ) ;
#92034 = CARTESIAN_POINT ( 'NONE',  ( 196.5944846034172713, 266.5326877703075752, 8.237093742074783620 ) ) ;
#92035 = CARTESIAN_POINT ( 'NONE',  ( 70.32692526124142773, 70.56678268892162009, 4.342815048252711918 ) ) ;
#92036 = CARTESIAN_POINT ( 'NONE',  ( 70.54960841692590634, 71.60126540147106766, 2.719701375183281034 ) ) ;
#92037 = CARTESIAN_POINT ( 'NONE',  ( 162.8014500637598871, 250.9066623883947216, -12.97690139725125746 ) ) ;
#92038 = EDGE_LOOP ( 'NONE', ( #73716, #72175, #44556, #58889 ) ) ;
#92039 = CARTESIAN_POINT ( 'NONE',  ( 164.0771906360838273, 283.2204635009451863, -9.130928687893741014 ) ) ;
#92040 = CARTESIAN_POINT ( 'NONE',  ( 207.5195222358739784, 271.2126392554839640, 2.810970398613041432 ) ) ;
#92041 = CARTESIAN_POINT ( 'NONE',  ( 181.3746470502182149, 267.9051538131957955, 15.02264890925958696 ) ) ;
#92042 = EDGE_CURVE ( 'NONE', #46359, #98253, #4355, .T. ) ;
#92043 = CARTESIAN_POINT ( 'NONE',  ( 102.5829875751790468, 230.0333772461660828, 9.188101187500095079 ) ) ;
#92044 = CARTESIAN_POINT ( 'NONE',  ( 3.278110179240818045, 23.93396525600387648, 2.839279412974139660 ) ) ;
#92045 = B_SPLINE_CURVE_WITH_KNOTS ( 'NONE', 3,
 ( #15056, #69764, #78387, #54541 ),
 .UNSPECIFIED., .F., .F.,
 ( 4, 4 ),
 ( 0.02560006208908528064, 0.03484442351368802898 ),
 .UNSPECIFIED. ) ;
#92046 = CARTESIAN_POINT ( 'NONE',  ( 151.0036289208911171, 269.1010379121764799, 14.24595189915657478 ) ) ;
#92047 = FACE_OUTER_BOUND ( 'NONE', #77502, .T. ) ;
#92049 = CARTESIAN_POINT ( 'NONE',  ( 105.0818317072414061, 238.1427522451419065, 10.00000000000009415 ) ) ;
#92048 = CARTESIAN_POINT ( 'NONE',  ( 143.3312870410541677, 246.8927522451417929, -10.00000000000009237 ) ) ;
#92050 = CARTESIAN_POINT ( 'NONE',  ( 149.3318355652811817, 271.9966689438488743, 13.09533505091524397 ) ) ;
#92051 = CARTESIAN_POINT ( 'NONE',  ( 198.5201458116119397, 286.8000164587433005, -18.30276554821096013 ) ) ;
#92052 = AXIS2_PLACEMENT_3D ( 'NONE', #9762, #46342, #15443 ) ;
#92053 = CARTESIAN_POINT ( 'NONE',  ( 36.29711636232130445, 39.14336893147758900, 7.433330006724141015 ) ) ;
#92054 = CARTESIAN_POINT ( 'NONE',  ( 33.00691499580853616, 42.55466486950702887, 7.012934429366973338E-14 ) ) ;
#92055 = DIRECTION ( 'NONE',  ( 0.4999999999999998890, -0.8660254037844385966, 0.000000000000000000 ) ) ;
#92056 = VERTEX_POINT ( 'NONE', #3862 ) ;
#92057 = CARTESIAN_POINT ( 'NONE',  ( 34.04181514241641082, 20.44966523072496756, -2.296566073217252530E-15 ) ) ;
#92058 = CARTESIAN_POINT ( 'NONE',  ( 74.41527144631503177, 63.48680199517529843, -14.86167820946030815 ) ) ;
#92059 = CARTESIAN_POINT ( 'NONE',  ( 147.2089949622447875, 275.6735367246781720, -3.633014386235353221 ) ) ;
#92060 = CARTESIAN_POINT ( 'NONE',  ( 149.1939152435731728, 272.2355539484436235, -11.44223522189843933 ) ) ;
#92061 = VERTEX_POINT ( 'NONE', #5357 ) ;
#92062 = CARTESIAN_POINT ( 'NONE',  ( 84.55094438110296551, 49.89265462440669552, -13.67900519688966021 ) ) ;
#92063 = CARTESIAN_POINT ( 'NONE',  ( 76.01570425163725986, 65.59347775405139203, -14.29814048726880316 ) ) ;
#92064 = CARTESIAN_POINT ( 'NONE',  ( 183.5859071331518351, 264.2830035368942276, -13.62284648814853050 ) ) ;
#92065 = CARTESIAN_POINT ( 'NONE',  ( 169.3267103143955410, 252.0916492433576934, -8.716375534122970947 ) ) ;
#92066 = CARTESIAN_POINT ( 'NONE',  ( 75.07854663334262568, 53.00102994419008695, -16.48764564530848631 ) ) ;
#92067 = CARTESIAN_POINT ( 'NONE',  ( 152.9262073036446168, 265.7710344717137900, 16.19159804214501008 ) ) ;
#92068 = ORIENTED_EDGE ( 'NONE', *, *, #61063, .T. ) ;
#92069 = CARTESIAN_POINT ( 'NONE',  ( 187.1950062442360831, 278.7691670715128112, 17.33431566565705495 ) ) ;
#92070 = VECTOR ( 'NONE', #71166, 999.9999999999998863 ) ;
#92071 = CARTESIAN_POINT ( 'NONE',  ( 37.04286019156342746, 27.10170272979929607, -7.433330006724141015 ) ) ;
#92072 = ORIENTED_EDGE ( 'NONE', *, *, #61818, .F. ) ;
#92073 = CARTESIAN_POINT ( 'NONE',  ( 167.8000401002150568, 249.6086421576515306, 6.575756818014385274 ) ) ;
#92074 = DIRECTION ( 'NONE',  ( 0.4999999999999992784, -0.8660254037844390407, 0.000000000000000000 ) ) ;
#92076 = EDGE_CURVE ( 'NONE', #87476, #93085, #56937, .T. ) ;
#92075 = ORIENTED_EDGE ( 'NONE', *, *, #14721, .F. ) ;
#92077 = AXIS2_PLACEMENT_3D ( 'NONE', #96516, #43251, #27591 ) ;
#92078 = CARTESIAN_POINT ( 'NONE',  ( 86.50941216119214516, 47.42513861390694530, -10.35655363221832737 ) ) ;
#92079 = CARTESIAN_POINT ( 'NONE',  ( 206.0571735407143592, 273.7455014938826707, 12.27159782092593332 ) ) ;
#92080 = CARTESIAN_POINT ( 'NONE',  ( 190.8789531733649483, 278.0110512791312090, -17.17207137177770448 ) ) ;
#92081 = CARTESIAN_POINT ( 'NONE',  ( 153.9709862450691560, 263.9614242624880376, -16.70428749416571890 ) ) ;
#92082 = CARTESIAN_POINT ( 'NONE',  ( 201.0356089830534643, 282.4431064412383989, -18.18835788025466371 ) ) ;
#92083 = VECTOR ( 'NONE', #27155, 1000.000000000000000 ) ;
#92084 = AXIS2_PLACEMENT_3D ( 'NONE', #97175, #2972, #79980 ) ;
#92085 = CARTESIAN_POINT ( 'NONE',  ( 31.21403501649406209, 38.99752408145594273, 5.678558825948276656 ) ) ;
#92086 = CYLINDRICAL_SURFACE ( 'NONE', #94772, 10.00000000000001066 ) ;
#92088 = EDGE_CURVE ( 'NONE', #71618, #4371, #10161, .T. ) ;
#92087 = CARTESIAN_POINT ( 'NONE',  ( 152.3360070569975449, 270.2436951681156643, -14.78697292633622951 ) ) ;
#92089 = ORIENTED_EDGE ( 'NONE', *, *, #81003, .T. ) ;
#92090 = B_SPLINE_CURVE_WITH_KNOTS ( 'NONE', 3,
 ( #54017, #46939, #835, #9444 ),
 .UNSPECIFIED., .F., .F.,
 ( 4, 4 ),
 ( 0.01228877948971598445, 0.01655137231517712568 ),
 .UNSPECIFIED. ) ;
#92091 = CARTESIAN_POINT ( 'NONE',  ( 162.7054358649808705, 249.4575268515429798, 10.87536955962176499 ) ) ;
#92092 = ADVANCED_FACE ( 'NONE', ( #45811 ), #237, .F. ) ;
#92093 = ORIENTED_EDGE ( 'NONE', *, *, #11543, .T. ) ;
#92094 = VERTEX_POINT ( 'NONE', #21552 ) ;
#92095 = CARTESIAN_POINT ( 'NONE',  ( 72.12409258116959165, 72.31950243486284080, -1.088631527110781594 ) ) ;
#92096 = CARTESIAN_POINT ( 'NONE',  ( 161.5600482970121163, 274.5147329235393840, 15.37191611340452724 ) ) ;
#92097 = AXIS2_PLACEMENT_3D ( 'NONE', #65491, #4703, #52278 ) ;
#92099 = PLANE ( 'NONE',  #66968 ) ;
#92098 = CARTESIAN_POINT ( 'NONE',  ( 204.8523313866422484, 275.8323493198358847, 14.65426965484541100 ) ) ;
#92100 = CARTESIAN_POINT ( 'NONE',  ( 165.0831640657340529, 244.7145676943567878, -1.661138566959525775 ) ) ;
#92101 = CARTESIAN_POINT ( 'NONE',  ( 200.3018037382982470, 274.6393581797076990, -13.69157862092785116 ) ) ;
#92102 = CARTESIAN_POINT ( 'NONE',  ( -24.92793671336084671, 23.00358903956173862, 10.00000000000000000 ) ) ;
#92103 = CARTESIAN_POINT ( 'NONE',  ( 189.8763472015711216, 301.7715148217271803, -0.1184663095182975079 ) ) ;
#92104 = CARTESIAN_POINT ( 'NONE',  ( 171.5969307849138659, 250.8838870372819372, -5.657895903504599922 ) ) ;
#92105 = CARTESIAN_POINT ( 'NONE',  ( 77.19405137238244663, 62.95358206284149105, -15.28408875821778423 ) ) ;
#92106 = CARTESIAN_POINT ( 'NONE',  ( 178.2870251902395466, 255.0132465080435225, 5.857099106615994089 ) ) ;
#92107 = CARTESIAN_POINT ( 'NONE',  ( 114.4640339051705666, 227.7048013555410080, 4.594050593750051981 ) ) ;
#92108 = EDGE_LOOP ( 'NONE', ( #20638, #79844, #90511 ) ) ;
#92109 = CARTESIAN_POINT ( 'NONE',  ( 185.1790142135946837, 260.5378326486920741, -9.806357480331048038 ) ) ;
#92110 = CARTESIAN_POINT ( 'NONE',  ( 161.0764005243388226, 283.8056199075659265, 2.187379043674367196 ) ) ;
#92111 = CARTESIAN_POINT ( 'NONE',  ( 187.9439182355510809, 273.9003972453228926, 16.19719593720451911 ) ) ;
#92112 = ORIENTED_EDGE ( 'NONE', *, *, #30810, .T. ) ;
#92113 = CARTESIAN_POINT ( 'NONE',  ( 162.8594194046838197, 248.9559446593948167, -10.02318146003397636 ) ) ;
#92114 = CARTESIAN_POINT ( 'NONE',  ( 180.4686966669306969, 294.6099987018001229, -1.982722432560759973 ) ) ;
#92115 = CARTESIAN_POINT ( 'NONE',  ( 192.0571890000333042, 297.9941860235205127, 11.61994745305988275 ) ) ;
#92116 = CARTESIAN_POINT ( 'NONE',  ( 206.7408728089182546, 272.5612996242556960, -10.63134519248043475 ) ) ;
#92117 = CARTESIAN_POINT ( 'NONE',  ( 92.75901190277325270, 224.3615022471902591, -10.00000000000009592 ) ) ;
#92118 = ORIENTED_EDGE ( 'NONE', *, *, #67667, .T. ) ;
#92119 = CARTESIAN_POINT ( 'NONE',  ( 195.4838507530383254, 292.0590337669632390, 15.61368894501154259 ) ) ;
#92120 = ORIENTED_EDGE ( 'NONE', *, *, #29455, .T. ) ;
#92122 = ADVANCED_FACE ( 'NONE', ( #85382 ), #44333, .T. ) ;
#92121 = CARTESIAN_POINT ( 'NONE',  ( 51.46042545625488174, 210.5177522451419065, 5.000000000000046185 ) ) ;
#92123 = DIRECTION ( 'NONE',  ( 0.7278481391575630788, -0.6857383512134002101, 0.000000000000000000 ) ) ;
#92124 = VERTEX_POINT ( 'NONE', #36734 ) ;
#92125 = CARTESIAN_POINT ( 'NONE',  ( 188.6360227007297112, 264.9932382472330232, -12.30697744625317291 ) ) ;
#92126 = CARTESIAN_POINT ( 'NONE',  ( 195.8318599711807053, 265.1596923740410716, 4.002729224306967204 ) ) ;
#92127 = DIRECTION ( 'NONE',  ( 0.000000000000000000, 0.000000000000000000, 1.000000000000000000 ) ) ;
#92128 = CARTESIAN_POINT ( 'NONE',  ( 81.69252017841917279, 43.53081715963432430, 8.862045408265887048 ) ) ;
#92130 = CARTESIAN_POINT ( 'NONE',  ( 69.66079769549185130, 63.13740578632653921, -13.62281212579674161 ) ) ;
#92129 = CARTESIAN_POINT ( 'NONE',  ( 184.2754218782066289, 288.8003507295421741, -13.20763826220184178 ) ) ;
#92131 = CARTESIAN_POINT ( 'NONE',  ( 201.4617167010348737, 281.7050662241970826, -17.43131506460443703 ) ) ;
#92132 = VERTEX_POINT ( 'NONE', #91474 ) ;
#92133 = CARTESIAN_POINT ( 'NONE',  ( 190.8957779480239765, 300.0058089740729770, -4.541438514207768229 ) ) ;
#92134 = CARTESIAN_POINT ( 'NONE',  ( 72.02948279518248853, 64.51453867759187233, 13.07310271355176390 ) ) ;
#92135 = CARTESIAN_POINT ( 'NONE',  ( 82.62760750629610129, 40.94168765461595427, -3.622589341579083300 ) ) ;
#92136 = EDGE_CURVE ( 'NONE', #35311, #97187, #14923, .T. ) ;
#92137 = PLANE ( 'NONE',  #64121 ) ;
#92138 = CARTESIAN_POINT ( 'NONE',  ( -57.04299263576977097, 30.72821847190685673, -10.00000000000000000 ) ) ;
#92139 = CARTESIAN_POINT ( 'NONE',  ( 82.63082945135448654, 42.48621489691582553, 6.270187774756061039 ) ) ;
#92140 = CARTESIAN_POINT ( 'NONE',  ( 196.4164021072083983, 270.5621661862001019, 13.33908636140236936 ) ) ;
#92141 = CARTESIAN_POINT ( 'NONE',  ( 194.5051734451974426, 293.7541525883582381, 14.61790433731063921 ) ) ;
#92142 = CARTESIAN_POINT ( 'NONE',  ( 34.63963837367094811, 179.2592609112380160, 2.679491924311254714 ) ) ;
#92143 = CARTESIAN_POINT ( 'NONE',  ( 82.51639823017981712, 53.47659673923356394, -15.74004163755323304 ) ) ;
#92144 = AXIS2_PLACEMENT_3D ( 'NONE', #56855, #89206, #19753 ) ;
#92145 = CARTESIAN_POINT ( 'NONE',  ( 77.73871025623044773, 221.8149278399160949, -9.188101187500095079 ) ) ;
#92146 = CARTESIAN_POINT ( 'NONE',  ( 159.5895502557670795, 254.2297859303815244, -16.92708575547316485 ) ) ;
#92147 = CARTESIAN_POINT ( 'NONE',  ( 192.8301672656986341, 296.6553483942417415, -13.40355799340913556 ) ) ;
#92148 = CARTESIAN_POINT ( 'NONE',  ( 163.0056347026689707, 248.3129541054019569, -11.27842346302751508 ) ) ;
#92150 = CARTESIAN_POINT ( 'NONE',  ( 19.98788723728717898, 104.4047874917408336, -22.49999999999983302 ) ) ;
#92149 = VECTOR ( 'NONE', #56397, 1000.000000000000000 ) ;
#92151 = VECTOR ( 'NONE', #61040, 1000.000000000000000 ) ;
#92152 = CARTESIAN_POINT ( 'NONE',  ( 207.6357208050208101, 271.0113774299547913, -6.790259683043212036 ) ) ;
#92153 = CARTESIAN_POINT ( 'NONE',  ( 194.5758046545716411, 288.3945151952651713, 17.23224542525024816 ) ) ;
#92154 = CARTESIAN_POINT ( 'NONE',  ( -19.65312891409030271, 93.06504152958497400, -10.00000000000000888 ) ) ;
#92155 = CARTESIAN_POINT ( 'NONE',  ( 188.9516232634142909, 259.5449388965931234, 2.625812016075142807 ) ) ;
#92156 = CARTESIAN_POINT ( 'NONE',  ( 42.57599984984017993, 32.78052372038644791, -10.00000000000000355 ) ) ;
#92157 = CARTESIAN_POINT ( 'NONE',  ( 161.7489939963169263, 252.0668770259760265, 14.13598244775917934 ) ) ;
#92158 = CARTESIAN_POINT ( 'NONE',  ( 157.5710319558766344, 257.7259621817996162, 18.28704422422941533 ) ) ;
#92159 = CARTESIAN_POINT ( 'NONE',  ( 71.83668398922712583, 71.91439960379638308, 2.874141227818668654 ) ) ;
#92160 = EDGE_CURVE ( 'NONE', #62531, #23462, #29645, .T. ) ;
#92161 = CARTESIAN_POINT ( 'NONE',  ( 26.48065812185646806, 198.3464784336661637, 1.353441290958777327E-15 ) ) ;
#92162 = EDGE_CURVE ( 'NONE', #95962, #99249, #99308, .T. ) ;
#92163 = CARTESIAN_POINT ( 'NONE',  ( 54.51857766514267212, 202.2833772461660828, -9.188101187500095079 ) ) ;
#92164 = CARTESIAN_POINT ( 'NONE',  ( 196.2609093297512857, 290.7131288316392670, 16.03897268885959448 ) ) ;
#92165 = PLANE ( 'NONE',  #81630 ) ;
#92166 = CARTESIAN_POINT ( 'NONE',  ( 82.36450559414066674, 49.91219489361158423, -13.90160499203291522 ) ) ;
#92167 = CARTESIAN_POINT ( 'NONE',  ( 149.7817191771959244, 245.0327760586659451, 1.948934522072303157E-15 ) ) ;
#92168 = CARTESIAN_POINT ( 'NONE',  ( 48.45674693441662129, 186.5327760586659451, 1.948934522072302763E-15 ) ) ;
#92169 = CONICAL_SURFACE ( 'NONE', #30661, 2.749999999999999112, 0.7853981633974463916 ) ;
#92170 = CARTESIAN_POINT ( 'NONE',  ( 22.39019813391814751, 21.43085787977763701, -9.188101187500008038 ) ) ;
#92171 = CARTESIAN_POINT ( 'NONE',  ( 150.9363692955544991, 269.2175350005573478, -14.27857383982596140 ) ) ;
#92172 = CARTESIAN_POINT ( 'NONE',  ( 196.9728329903666122, 289.4800408803428695, -17.53478045286815856 ) ) ;
#92173 = CARTESIAN_POINT ( 'NONE',  ( 14.98925625915878079, 9.449665230724930254, -2.296566073217252530E-15 ) ) ;
#92174 = CARTESIAN_POINT ( 'NONE',  ( 24.67121952831112353, 36.01751292744057764, 6.180339887498949913 ) ) ;
#92175 = CARTESIAN_POINT ( 'NONE',  ( 77.03033377257250436, 63.66679109869721742, 15.37730549896620147 ) ) ;
#92176 = CARTESIAN_POINT ( 'NONE',  ( -14.09755945733355276, 105.0466235773165096, 43.88975835780059498 ) ) ;
#92177 = CARTESIAN_POINT ( 'NONE',  ( 198.0792648159935538, 287.5636447432459022, 17.04758482866669667 ) ) ;
#92178 = CARTESIAN_POINT ( 'NONE',  ( 182.1968425487349919, 281.0285068568209113, -17.15452853389480126 ) ) ;
#92179 = CARTESIAN_POINT ( 'NONE',  ( 201.3491118187633901, 281.9001036014715282, 16.71671293284840587 ) ) ;
#92180 = DIRECTION ( 'NONE',  ( 0.000000000000000000, 0.000000000000000000, 1.000000000000000000 ) ) ;
#92181 = CARTESIAN_POINT ( 'NONE',  ( 117.9459173961707137, 232.2365022471902307, 10.00000000000009592 ) ) ;
#92182 = DIRECTION ( 'NONE',  ( -0.8660254037844387076, -0.4999999999999998890, -0.000000000000000000 ) ) ;
#92183 = CARTESIAN_POINT ( 'NONE',  ( 166.7087160314272296, 287.6354326016939353, -0.3369197202164816995 ) ) ;
#92184 = VERTEX_POINT ( 'NONE', #44830 ) ;
#92185 = CARTESIAN_POINT ( 'NONE',  ( 77.23115344012272487, 49.25751081205777382, 15.36283045010027948 ) ) ;
#92186 = ORIENTED_EDGE ( 'NONE', *, *, #11475, .T. ) ;
#92187 = CARTESIAN_POINT ( 'NONE',  ( 206.6268150440956504, 272.7588534679261443, -10.76664753678610609 ) ) ;
#92188 = CARTESIAN_POINT ( 'NONE',  ( 190.1333673262456330, 279.2923110579273498, -17.65696406450081213 ) ) ;
#92189 = CARTESIAN_POINT ( 'NONE',  ( 47.92671612011951510, 80.40884667711614497, 10.00000000000000000 ) ) ;
#92190 = ORIENTED_EDGE ( 'NONE', *, *, #43057, .T. ) ;
#92191 = CARTESIAN_POINT ( 'NONE',  ( 59.94571803450949687, 216.9637435831425023, 2.679491924311251605 ) ) ;
#92192 = CARTESIAN_POINT ( 'NONE',  ( 79.08118623426810245, 45.97885358038440273, -12.60247831142608987 ) ) ;
#92193 = CARTESIAN_POINT ( 'NONE',  ( 194.6310785344323904, 293.5360785768717165, -14.54510914272505495 ) ) ;
#92194 = CARTESIAN_POINT ( 'NONE',  ( 73.09164847706512091, 70.51859621836145209, -7.974784385355167871 ) ) ;
#92195 = PLANE ( 'NONE',  #38530 ) ;
#92196 = ORIENTED_EDGE ( 'NONE', *, *, #22653, .F. ) ;
#92197 = CARTESIAN_POINT ( 'NONE',  ( 15.62557774837418023, 29.99752408145591431, 5.678558825948276656 ) ) ;
#92198 = CARTESIAN_POINT ( 'NONE',  ( 23.67544375150414737, 191.1427522451419350, -10.00000000000009592 ) ) ;
#92199 = DIRECTION ( 'NONE',  ( 0.4999999999999992784, -0.8660254037844390407, 0.000000000000000000 ) ) ;
#92200 = ORIENTED_EDGE ( 'NONE', *, *, #11030, .F. ) ;
#92202 = EDGE_CURVE ( 'NONE', #25358, #184, #69128, .T. ) ;
#92201 = CARTESIAN_POINT ( 'NONE',  ( 185.2391986358457530, 295.7873944733689768, 8.585680893828113724 ) ) ;
#92203 = DIRECTION ( 'NONE',  ( 0.000000000000000000, 0.000000000000000000, 1.000000000000000000 ) ) ;
#92204 = ADVANCED_FACE ( 'NONE', ( #68135 ), #67640, .T. ) ;
#92205 = ORIENTED_EDGE ( 'NONE', *, *, #36678, .T. ) ;
#92206 = CARTESIAN_POINT ( 'NONE',  ( 174.0013662709156108, 285.8605094670047606, 10.49998161009456155 ) ) ;
#92208 = CARTESIAN_POINT ( 'NONE',  ( 68.06446806950627604, 66.09146943954503683, -10.51449895684611491 ) ) ;
#92207 = CARTESIAN_POINT ( 'NONE',  ( 163.1953264782998758, 283.8895661455310915, -7.125257539458086598 ) ) ;
#92209 = CARTESIAN_POINT ( 'NONE',  ( 207.6555576926778883, 270.9770189326688410, -1.235081510489080436 ) ) ;
#92210 = CARTESIAN_POINT ( 'NONE',  ( 164.4990934228277411, 245.7262077230798809, 6.470820838822735510 ) ) ;
#92211 = EDGE_CURVE ( 'NONE', #52319, #86732, #69138, .T. ) ;
#92212 = CARTESIAN_POINT ( 'NONE',  ( 159.7897726928491409, 253.8829904965402875, 16.83923858130328810 ) ) ;
#92213 = CARTESIAN_POINT ( 'NONE',  ( 161.1999634265268924, 263.0548667757333874, -17.77828691421615304 ) ) ;
#92214 = ADVANCED_FACE ( 'NONE', ( #99551 ), #60027, .F. ) ;
#92215 = CARTESIAN_POINT ( 'NONE',  ( 132.4608640057421667, 247.2833772461660544, -9.188101187500095079 ) ) ;
#92216 = VECTOR ( 'NONE', #86011, 1000.000000000000000 ) ;
#92217 = CARTESIAN_POINT ( 'NONE',  ( 203.0744322039535632, 268.2681989120735011, 2.496359996990924923 ) ) ;
#92218 = CARTESIAN_POINT ( 'NONE',  ( 179.0724974991984766, 257.7164609560927033, 10.12017508776513530 ) ) ;
#92219 = CARTESIAN_POINT ( 'NONE',  ( 69.94448162217048548, 217.3149278399160949, -9.188101187500095079 ) ) ;
#92220 = EDGE_LOOP ( 'NONE', ( #39494, #22999, #31707, #69392, #30537 ) ) ;
#92221 = CARTESIAN_POINT ( 'NONE',  ( 173.2165366525584602, 265.2663209395350918, 16.02481246879085575 ) ) ;
#92222 = CYLINDRICAL_SURFACE ( 'NONE', #30159, 17.82106496071139645 ) ;
#92223 = CARTESIAN_POINT ( 'NONE',  ( 79.46553399343461876, 45.78194281441977864, 12.91977081584364662 ) ) ;
#92224 = ORIENTED_EDGE ( 'NONE', *, *, #46771, .T. ) ;
#92225 = CIRCLE ( 'NONE', #32287, 70.00000000000001421 ) ;
#92226 = CARTESIAN_POINT ( 'NONE',  ( 163.9961211234992788, 256.9275610305372766, 16.20495027727189807 ) ) ;
#92227 = ORIENTED_EDGE ( 'NONE', *, *, #9947, .T. ) ;
#92228 = CARTESIAN_POINT ( 'NONE',  ( -107.5954152546897262, 65.38554960527366688, 21.50000000000000000 ) ) ;
#92229 = CARTESIAN_POINT ( 'NONE',  ( 66.96658208328462081, 68.04499853430465350, 6.922779954623445420 ) ) ;
#92230 = CARTESIAN_POINT ( 'NONE',  ( 194.1605905766382136, 284.7225647929109300, 17.53772805858957184 ) ) ;
#92231 = CARTESIAN_POINT ( 'NONE',  ( 90.04477061917849312, 44.76220097505219542, 0.000000000000000000 ) ) ;
#92232 = CARTESIAN_POINT ( 'NONE',  ( 81.17013726474981183, 56.17602725108039152, 16.10664853823880804 ) ) ;
#92233 = CARTESIAN_POINT ( 'NONE',  ( 155.0898745997320134, 262.0234527842152374, 17.05457557403769542 ) ) ;
#92234 = CARTESIAN_POINT ( 'NONE',  ( 71.55041901307521357, 67.02176819343763725, 10.94176416068171953 ) ) ;
#92235 = CARTESIAN_POINT ( 'NONE',  ( 78.92949518643405327, 222.5024278399160949, 9.188101187500095079 ) ) ;
#92236 = ORIENTED_EDGE ( 'NONE', *, *, #18696, .T. ) ;
#92237 = ADVANCED_FACE ( 'NONE', ( #62508 ), #55906, .T. ) ;
#92238 = B_SPLINE_SURFACE_WITH_KNOTS ( 'NONE', 3, 1, ( 
 ( #63749, #86114 ),
 ( #40428, #54623 ),
 ( #71362, #25240 ),
 ( #1953, #56125 ),
 ( #87121, #71868 ),
 ( #33346, #64245 ),
 ( #95195, #25767 ),
 ( #56642, #87625 ),
 ( #18154, #49053 ),
 ( #79989, #10557 ),
 ( #78341, #69718 ),
 ( #8923, #54498 ),
 ( #8426, #62102 ),
 ( #93049, #78847 ),
 ( #70212, #63622 ),
 ( #17521, #94559 ),
 ( #48428, #79376 ),
 ( #48933, #79872 ),
 ( #10432, #64635 ),
 ( #72249, #4840 ),
 ( #80883, #95587 ),
 ( #34717, #49925 ),
 ( #10943, #66121 ),
 ( #65616, #41306 ),
 ( #80372, #35220 ),
 ( #11452, #42308 ),
 ( #4317, #35720 ),
 ( #58506, #97070 ),
 ( #73239, #3832 ),
 ( #96573, #57513 ),
 ( #66618, #97548 ) ),
 .UNSPECIFIED., .F., .F., .F.,
 ( 4, 3, 3, 3, 3, 3, 3, 3, 3, 3, 4 ),
 ( 2, 2 ),
 ( 0.000000000000000000, 0.1333490885032359574, 0.3007194338854340954, 0.4699862290245186980, 0.5844252810809413834, 0.6686540514502794519, 0.7354980260655689106, 0.8028463152565833427, 0.8633854507757432462, 0.9437142632667659958, 1.000000000000000000 ),
 ( 0.000000000000000000, 1.000000000000000000 ),
 .UNSPECIFIED. ) ;
#92239 = CARTESIAN_POINT ( 'NONE',  ( 200.5016309952337394, 283.3679834462653844, -16.85167051214465772 ) ) ;
#92240 = ORIENTED_EDGE ( 'NONE', *, *, #19225, .T. ) ;
#92241 = CARTESIAN_POINT ( 'NONE',  ( 163.7196345835096452, 261.0355710201180841, -16.91880463402510060 ) ) ;
#92242 = CARTESIAN_POINT ( 'NONE',  ( 76.20470709868462222, 65.28062994224386273, -14.10576654135921437 ) ) ;
#92243 = CIRCLE ( 'NONE', #93826, 0.1418229129680828593 ) ;
#92244 = CARTESIAN_POINT ( 'NONE',  ( -32.46306855948172654, 93.78642701249712843, 43.90667800897207940 ) ) ;
#92245 = CARTESIAN_POINT ( 'NONE',  ( 197.4614820106550326, 280.4067882521826505, 16.54892308915801991 ) ) ;
#92246 = CARTESIAN_POINT ( 'NONE',  ( 161.6101421750211671, 260.8786438988923351, 16.75479683814266707 ) ) ;
#92247 = ORIENTED_EDGE ( 'NONE', *, *, #25483, .T. ) ;
#92248 = CARTESIAN_POINT ( 'NONE',  ( 87.82600437409995209, 44.28008912978396694, 4.743525404917310340 ) ) ;
#92249 = CARTESIAN_POINT ( 'NONE',  ( 156.7582088183394546, 274.2853207512858944, 13.68792815068864854 ) ) ;
#92250 = DIRECTION ( 'NONE',  ( -0.000000000000000000, 0.000000000000000000, -1.000000000000000000 ) ) ;
#92251 = CARTESIAN_POINT ( 'NONE',  ( 201.2535035105529744, 282.0657020489176716, -18.08976065250591958 ) ) ;
#92252 =( BOUNDED_CURVE ( )  B_SPLINE_CURVE ( 2, ( #92054, #53488, #70181, #84440, #15477, #69690, #15995, #77818, #47388, #22600, #38279, #93535, #8893 ),
 .UNSPECIFIED., .F., .T. ) 
 B_SPLINE_CURVE_WITH_KNOTS ( ( 3, 2, 2, 2, 2, 2, 3 ),
 ( 0.9125000000000000888, 0.9150000000000000355, 0.9200000000000000400, 0.9250000000000000444, 0.9300000000000000488, 0.9350000000000000533, 0.9375000000000000000 ),
 .UNSPECIFIED. ) 
 CURVE ( )  GEOMETRIC_REPRESENTATION_ITEM ( )  RATIONAL_B_SPLINE_CURVE ( ( 0.9755282581475767101, 0.9755282581475772652, 1.000000000000000000, 0.9510565162951535312, 1.000000000000000000, 0.9510565162951535312, 1.000000000000000000, 0.9510565162951535312, 1.000000000000000000, 0.9510565162951535312, 1.000000000000000000, 0.9755282581475768211, 0.9755282581475768211 ) ) 
 REPRESENTATION_ITEM ( '' )  );
#92253 = CARTESIAN_POINT ( 'NONE',  ( 73.06677152903225192, 70.63173304288399379, 7.751455205043641605 ) ) ;
#92254 = CARTESIAN_POINT ( 'NONE',  ( 69.73018707955242235, 67.40416580934164870, -9.399663619568531914 ) ) ;
#92255 = ORIENTED_EDGE ( 'NONE', *, *, #72657, .F. ) ;
#92256 = CARTESIAN_POINT ( 'NONE',  ( 195.6998486595285840, 265.4147343413312115, 4.643485329879461609 ) ) ;
#92257 = CARTESIAN_POINT ( 'NONE',  ( 87.85384634344086408, 209.9824982072973683, 3.021315404115420679E-15 ) ) ;
#92258 = PLANE ( 'NONE',  #41408 ) ;
#92259 = CARTESIAN_POINT ( 'NONE',  ( 80.80154134310006953, 50.59177401893971648, 14.61214521119545751 ) ) ;
#92260 = FACE_OUTER_BOUND ( 'NONE', #59114, .T. ) ;
#92261 = ORIENTED_EDGE ( 'NONE', *, *, #46073, .F. ) ;
#92262 = CARTESIAN_POINT ( 'NONE',  ( 147.5634954182374372, 275.0595239235922236, 4.682022975662822439 ) ) ;
#92263 = CARTESIAN_POINT ( 'NONE',  ( -13.82959147685579104, 104.2312461070085021, 43.93259070532315036 ) ) ;
#92264 = EDGE_CURVE ( 'NONE', #19562, #72450, #8339, .T. ) ;
#92265 = CARTESIAN_POINT ( 'NONE',  ( 207.6007741873543750, 271.0719067473055475, 7.587922723682903658 ) ) ;
#92267 = CARTESIAN_POINT ( 'NONE',  ( 73.87609383058843093, 55.21511341151430230, 16.12190632378065303 ) ) ;
#92266 = CARTESIAN_POINT ( 'NONE',  ( 155.0929244053699847, 262.0181703658971628, 18.51426604808664678 ) ) ;
#92268 = CARTESIAN_POINT ( 'NONE',  ( 24.58352123714976045, 26.14441083166261848, 10.00000000000000533 ) ) ;
#92269 = CARTESIAN_POINT ( 'NONE',  ( 19.28110618420672395, 193.4860189848785126, -2.679491924311252493 ) ) ;
#92270 = CARTESIAN_POINT ( 'NONE',  ( 163.3652774841088444, 283.7749973649284811, -3.153219606719814827 ) ) ;
#92271 = DIRECTION ( 'NONE',  ( -0.8660254037844382635, -0.5000000000000005551, 0.000000000000000000 ) ) ;
#92272 = CARTESIAN_POINT ( 'NONE',  ( 159.8416255366773839, 253.7931787365127434, 16.77980437810719394 ) ) ;
#92273 = CARTESIAN_POINT ( 'NONE',  ( -15.08856125979659346, 174.3464784336661353, 1.353441290958777327E-15 ) ) ;
#92274 = CARTESIAN_POINT ( 'NONE',  ( 82.77371932451866599, 207.0494855054051584, -2.679491924311248496 ) ) ;
#92275 = ORIENTED_EDGE ( 'NONE', *, *, #52362, .F. ) ;
#92276 = VECTOR ( 'NONE', #50683, 1000.000000000000000 ) ;
#92277 = CARTESIAN_POINT ( 'NONE',  ( 178.6997720573820061, 256.4289685822167257, 8.737427515670157518 ) ) ;
#92278 = CARTESIAN_POINT ( 'NONE',  ( 72.49337063691618255, 70.67504402769610294, -7.896386945446492334 ) ) ;
#92279 = CARTESIAN_POINT ( 'NONE',  ( 81.60564328118654487, 41.73995806223437199, 5.932757990861635022 ) ) ;
#92280 = CARTESIAN_POINT ( 'NONE',  ( 15.06046875309669630, 173.3768266524159856, -9.188101187500093303 ) ) ;
#92281 = CARTESIAN_POINT ( 'NONE',  ( 23.90938336746022586, 36.73705186507755371, -3.090169943749475845 ) ) ;
#92282 = CARTESIAN_POINT ( 'NONE',  ( 85.20962068992432137, 42.51169701653922317, -1.264518624749869868 ) ) ;
#92283 = CARTESIAN_POINT ( 'NONE',  ( 64.01779381112923772, 217.7677522451419065, -5.000000000000047962 ) ) ;
#92284 = CARTESIAN_POINT ( 'NONE',  ( 49.09245556086620610, 93.56363653685789927, -10.00000000000000000 ) ) ;
#92285 = DIRECTION ( 'NONE',  ( -0.4999999999999974465, 0.8660254037844402619, 0.000000000000000000 ) ) ;
#92286 = CARTESIAN_POINT ( 'NONE',  ( 190.8432295316381442, 261.8533477349316740, -1.278961237959173491 ) ) ;
#92287 = CARTESIAN_POINT ( 'NONE',  ( 75.87151652897675547, 204.6115022471901739, -5.000000000000041744 ) ) ;
#92288 = CARTESIAN_POINT ( 'NONE',  ( 34.47489329363036603, 42.83705186507756935, 3.090169943749475401 ) ) ;
#92289 = CARTESIAN_POINT ( 'NONE',  ( 147.6088797830324779, 274.9809158978982850, 8.531536684623960198 ) ) ;
#92290 = CARTESIAN_POINT ( 'NONE',  ( 34.43744006700849525, 196.8149278399160664, 9.188101187500093303 ) ) ;
#92291 = CARTESIAN_POINT ( 'NONE',  ( 72.54816569808836846, 70.68207713539274550, -7.935695741106854051 ) ) ;
#92292 = CARTESIAN_POINT ( 'NONE',  ( 36.94473716931751284, 21.73415679381824361, -6.890680421881970419E-14 ) ) ;
#92293 = CARTESIAN_POINT ( 'NONE',  ( 43.88624854525928498, 27.19860640527296169, 2.839279412974134775 ) ) ;
#92294 = CARTESIAN_POINT ( 'NONE',  ( 151.3681950933278983, 268.4695907787949523, -15.50699599486383917 ) ) ;
#92295 = CARTESIAN_POINT ( 'NONE',  ( 206.9059968923335475, 272.2752963222270068, 6.902135944297345560 ) ) ;
#92296 = CARTESIAN_POINT ( 'NONE',  ( 188.2139646732387348, 267.9741926252710300, 13.43593211841361779 ) ) ;
#92297 = CARTESIAN_POINT ( 'NONE',  ( 162.9658701564373189, 281.1729661104742490, -10.32510856000857125 ) ) ;
#92298 = B_SPLINE_CURVE_WITH_KNOTS ( 'NONE', 3,
 ( #81951, #52012, #68195, #20624 ),
 .UNSPECIFIED., .F., .F.,
 ( 4, 4 ),
 ( 0.008917401783766700993, 0.01511162993189288720 ),
 .UNSPECIFIED. ) ;
#92299 = CARTESIAN_POINT ( 'NONE',  ( 161.4425099228864440, 280.3143438959959894, 8.996476011744888979 ) ) ;
#92300 = APPLICATION_PROTOCOL_DEFINITION ( 'draft international standard', 'automotive_design', 1998, #67032 ) ;
#92301 = CARTESIAN_POINT ( 'NONE',  ( 23.18645373101242413, 19.10170272979927120, -7.433330006724141015 ) ) ;
#92302 = CARTESIAN_POINT ( 'NONE',  ( 148.3930300673291640, 273.6227277647267897, 8.375036249079425232 ) ) ;
#92303 = CARTESIAN_POINT ( 'NONE',  ( 72.03863647653309954, 59.27131230149748831, 15.84878527872051279 ) ) ;
#92304 = CARTESIAN_POINT ( 'NONE',  ( 155.0898745997320134, 262.0234527842152374, 17.05457557403769542 ) ) ;
#92305 = ORIENTED_EDGE ( 'NONE', *, *, #92211, .T. ) ;
#92306 = CARTESIAN_POINT ( 'NONE',  ( 79.57426776854913442, 46.24084366570346560, -13.18946159588284139 ) ) ;
#92307 = CARTESIAN_POINT ( 'NONE',  ( 148.7305541605275607, 275.0381188865328568, -8.045727261058747359 ) ) ;
#92308 = CARTESIAN_POINT ( 'NONE',  ( 81.82544566900152461, 42.13177917682811824, 7.581690138153514447 ) ) ;
#92309 = EDGE_LOOP ( 'NONE', ( #32222, #95592, #29624, #13559 ) ) ;
#92310 = CARTESIAN_POINT ( 'NONE',  ( 196.1972786361653789, 290.1674837226785826, -16.31932546841715137 ) ) ;
#92312 = ADVANCED_FACE ( 'NONE', ( #46833 ), #72158, .F. ) ;
#92311 = CARTESIAN_POINT ( 'NONE',  ( 72.37288529989473318, 71.73372848700918780, -5.731447342215284735 ) ) ;
#92313 = CARTESIAN_POINT ( 'NONE',  ( 76.59502500117768875, 63.79608208629903032, 14.86840811388221439 ) ) ;
#92314 = CARTESIAN_POINT ( 'NONE',  ( 203.3041373168503299, 278.5139001086923827, -16.61929732091214973 ) ) ;
#92315 = EDGE_CURVE ( 'NONE', #55159, #9356, #71651, .T. ) ;
#92316 = ORIENTED_EDGE ( 'NONE', *, *, #2129, .F. ) ;
#92317 = EDGE_LOOP ( 'NONE', ( #40759, #66959, #87701, #84355 ) ) ;
#92318 = B_SPLINE_CURVE_WITH_KNOTS ( 'NONE', 3,
 ( #18228, #42493, #34898, #19250, #65798, #73426, #10628, #11142, #40990, #87196 ),
 .UNSPECIFIED., .F., .F.,
 ( 4, 2, 2, 2, 4 ),
 ( 0.000000000000000000, 0.2500000000000000000, 0.5000000000000000000, 0.7500000000000000000, 1.000000000000000000 ),
 .UNSPECIFIED. ) ;
#92319 = CARTESIAN_POINT ( 'NONE',  ( 202.2560213337884250, 279.9099699780790615, 15.68235421671478669 ) ) ;
#92320 = ORIENTED_EDGE ( 'NONE', *, *, #38847, .T. ) ;
#92321 = CARTESIAN_POINT ( 'NONE',  ( 150.8888667059421209, 269.2998118992572927, 15.79021133717968617 ) ) ;
#92322 = CARTESIAN_POINT ( 'NONE',  ( 71.81093420572706520, 69.41658505044310346, 9.148441192301559610 ) ) ;
#92323 = CARTESIAN_POINT ( 'NONE',  ( -22.42236680055709641, 157.8615022471902591, 0.000000000000000000 ) ) ;
#92324 = CARTESIAN_POINT ( 'NONE',  ( 71.59204759908475069, 69.79570777427565531, -8.447857603145788374 ) ) ;
#92325 = ORIENTED_EDGE ( 'NONE', *, *, #34417, .F. ) ;
#92327 = ADVANCED_FACE ( 'NONE', ( #77755 ), #39208, .F. ) ;
#92326 = CARTESIAN_POINT ( 'NONE',  ( 190.5444288681022442, 300.6143634316900943, -1.000014190476072873 ) ) ;
#92328 = ORIENTED_EDGE ( 'NONE', *, *, #90000, .F. ) ;
#92329 = CARTESIAN_POINT ( 'NONE',  ( 195.6974783896144174, 291.6890198465123945, 16.70600479393688431 ) ) ;
#92330 = CARTESIAN_POINT ( 'NONE',  ( 74.90805568670471359, 65.07985694792712650, 13.78103290621842270 ) ) ;
#92331 = ORIENTED_EDGE ( 'NONE', *, *, #27017, .F. ) ;
#92332 = FACE_OUTER_BOUND ( 'NONE', #75636, .T. ) ;
#92333 = CARTESIAN_POINT ( 'NONE',  ( 78.19421406511375494, 47.63508073124027220, -14.44498547994805016 ) ) ;
#92334 = ORIENTED_EDGE ( 'NONE', *, *, #64053, .T. ) ;
#92335 = DIRECTION ( 'NONE',  ( -0.8660254037844384856, -0.5000000000000002220, -3.252519625699449945E-16 ) ) ;
#92336 = CARTESIAN_POINT ( 'NONE',  ( 24.56850397818812226, 63.80763720866956845, 59.99999999999999289 ) ) ;
#92337 = CARTESIAN_POINT ( 'NONE',  ( 41.50110961350213046, 24.36477965099642873, 1.583844403245330712 ) ) ;
#92338 = EDGE_LOOP ( 'NONE', ( #85621, #52031, #66894, #9421 ) ) ;
#92339 = ORIENTED_EDGE ( 'NONE', *, *, #77199, .T. ) ;
#92340 = CARTESIAN_POINT ( 'NONE',  ( -19.70352899468211660, 93.19760687392162879, 59.99999999999999289 ) ) ;
#92341 = LINE ( 'NONE', #47680, #55747 ) ;
#92342 = CARTESIAN_POINT ( 'NONE',  ( 147.6220714307702622, 274.9580672937808572, 8.392894244419288441 ) ) ;
#92343 = CARTESIAN_POINT ( 'NONE',  ( 149.2511585606875428, 272.1364056148075292, 11.40684181024752242 ) ) ;
#92344 = CARTESIAN_POINT ( 'NONE',  ( 171.8663912998340777, 275.8233464154953936, -15.83653131706603112 ) ) ;
#92345 = CARTESIAN_POINT ( 'NONE',  ( 147.2650827261924746, 275.5763898678378041, 0.3422986961735832168 ) ) ;
#92346 = CARTESIAN_POINT ( 'NONE',  ( 146.5865263025993954, 276.7516840693029962, 0.4918294119671828835 ) ) ;
#92347 = CARTESIAN_POINT ( 'NONE',  ( 162.9808515016160300, 257.5771916527201029, 15.58578234508959781 ) ) ;
#92348 = CARTESIAN_POINT ( 'NONE',  ( 71.02066284800852713, 69.66031639842336176, 7.328838084737518521 ) ) ;
#92350 = LINE ( 'NONE', #91346, #61193 ) ;
#92349 = CARTESIAN_POINT ( 'NONE',  ( 196.5806080813426888, 290.1593943507663766, -16.31912166233602690 ) ) ;
#92351 = CARTESIAN_POINT ( 'NONE',  ( 67.01638591644868370, 66.89576277548633243, 8.813849967855754031 ) ) ;
#92352 = CARTESIAN_POINT ( 'NONE',  ( 189.7791324398369852, 300.5155985523547884, 1.795207924923805987 ) ) ;
#92353 = CARTESIAN_POINT ( 'NONE',  ( 78.53005147510766903, 47.90408355870507506, 13.93219832960360094 ) ) ;
#92354 = PRODUCT_RELATED_PRODUCT_CATEGORY ( 'part', '', ( #74307 ) ) ;
#92355 = EDGE_LOOP ( 'NONE', ( #48540, #20821, #4726, #17925 ) ) ;
#92356 = CARTESIAN_POINT ( 'NONE',  ( 149.6144381846877991, 271.5071868486843414, -11.67527394954620590 ) ) ;
#92357 = CARTESIAN_POINT ( 'NONE',  ( 83.62483622648333892, 41.61889388988494431, -1.100529281121362501 ) ) ;
#92358 = CARTESIAN_POINT ( 'NONE',  ( 87.77948443791279942, 45.22530890134208903, -6.970560438077714416 ) ) ;
#92359 = CARTESIAN_POINT ( 'NONE',  ( 79.29099298814826113, 45.77971119220809015, 12.98826949500056926 ) ) ;
#92360 = CARTESIAN_POINT ( 'NONE',  ( 191.9248140970461804, 297.5186077601156285, -10.25883709677317945 ) ) ;
#92361 = CARTESIAN_POINT ( 'NONE',  ( 189.8679201377346999, 301.7861109244506679, -1.065287660593647434 ) ) ;
#92362 = AXIS2_PLACEMENT_3D ( 'NONE', #10805, #79741, #32078 ) ;
#92363 = CARTESIAN_POINT ( 'NONE',  ( 165.3821918710930845, 283.7844301331062979, -8.403629075564190032 ) ) ;
#92364 = ORIENTED_EDGE ( 'NONE', *, *, #74921, .T. ) ;
#92365 = CARTESIAN_POINT ( 'NONE',  ( 207.5886452961740076, 271.0929146030698007, -1.661373005306138184 ) ) ;
#92366 = CARTESIAN_POINT ( 'NONE',  ( 149.8622666665893632, 273.0779353264732663, 11.47145096717591528 ) ) ;
#92367 = CARTESIAN_POINT ( 'NONE',  ( 54.85235828774403899, 189.1427522451417644, 1.119607411625061291E-15 ) ) ;
#92368 = CARTESIAN_POINT ( 'NONE',  ( 126.7777458412893168, 237.8768266524159856, -9.188101187500093303 ) ) ;
#92369 = CARTESIAN_POINT ( 'NONE',  ( 151.1126408083691501, 268.9122237844355254, -15.82705194100464396 ) ) ;
#92370 = CARTESIAN_POINT ( 'NONE',  ( 2.487887237287232711, 134.7156766241960497, -21.50000000000002487 ) ) ;
#92371 = CARTESIAN_POINT ( 'NONE',  ( 187.3902638176308244, 281.3068701335633364, -17.14294349842597498 ) ) ;
#92372 = CARTESIAN_POINT ( 'NONE',  ( 175.9466766006847536, 252.7179606613870249, -4.818959155576430398 ) ) ;
#92373 = CARTESIAN_POINT ( 'NONE',  ( 48.83545950068980090, 192.8768266524159856, -9.188101187500091527 ) ) ;
#92374 = ADVANCED_FACE ( 'NONE', ( #25543 ), #78251, .T. ) ;
#92375 = CARTESIAN_POINT ( 'NONE',  ( 183.1426684129219780, 267.5694331394444703, -16.03671021927237206 ) ) ;
#92376 = CARTESIAN_POINT ( 'NONE',  ( 85.74825148587619594, 48.61567592689142003, -12.33318615817162645 ) ) ;
#92377 = VERTEX_POINT ( 'NONE', #54926 ) ;
#92378 = LINE ( 'NONE', #31027, #65641 ) ;
#92379 = CARTESIAN_POINT ( 'NONE',  ( 74.14452735224477919, 67.86235095172764886, -11.65459263701698234 ) ) ;
#92380 = CARTESIAN_POINT ( 'NONE',  ( 26.07505581137152006, 175.8615022471901739, 5.000000000000051514 ) ) ;
#92381 = CARTESIAN_POINT ( 'NONE',  ( 164.4344613858980608, 251.5011570344067877, -12.86682041478359295 ) ) ;
#92382 = FACE_OUTER_BOUND ( 'NONE', #84001, .T. ) ;
#92383 = ADVANCED_FACE ( 'NONE', ( #17954 ), #70629, .T. ) ;
#92384 = CARTESIAN_POINT ( 'NONE',  ( 154.4765043762321000, 276.8026792959899467, -10.28524050916173138 ) ) ;
#92385 = CARTESIAN_POINT ( 'NONE',  ( 182.2623503800200240, 262.6690854021607606, 12.85806171487328875 ) ) ;
#92386 = B_SPLINE_CURVE_WITH_KNOTS ( 'NONE', 3,
 ( #81450, #66699, #90045, #5902, #52005, #97634, #66214, #74337, #5413, #91044 ),
 .UNSPECIFIED., .F., .F.,
 ( 4, 2, 2, 2, 4 ),
 ( 0.000000000000000000, 0.0002622400424272520970, 0.0005244800848545041940, 0.0007867201272817562910, 0.001048960169709008388 ),
 .UNSPECIFIED. ) ;
#92387 = CARTESIAN_POINT ( 'NONE',  ( 114.6802799325189284, 237.0177522451418497, -10.00000000000009592 ) ) ;
#92388 = CARTESIAN_POINT ( 'NONE',  ( 192.9518127100452034, 296.0217619941561793, -12.12386602825073645 ) ) ;
#92389 = EDGE_LOOP ( 'NONE', ( #64055, #24625, #3493 ) ) ;
#92390 = ADVANCED_FACE ( 'NONE', ( #25025 ), #87426, .F. ) ;
#92391 = CARTESIAN_POINT ( 'NONE',  ( 163.1008115941903895, 248.1481028935802442, 11.25332017433677834 ) ) ;
#92392 = CARTESIAN_POINT ( 'NONE',  ( 163.3409975114459485, 247.7320886816312111, -10.96358124877083640 ) ) ;
#92393 = CARTESIAN_POINT ( 'NONE',  ( 25.39882055865593458, 173.2202760586659736, -5.415160957724236172E-17 ) ) ;
#92394 = CARTESIAN_POINT ( 'NONE',  ( 73.03321427718370273, 68.50884256177610609, -10.98349909054766549 ) ) ;
#92395 = CARTESIAN_POINT ( 'NONE',  ( -14.77590589997254611, 105.6530250111700013, 43.95880336568158242 ) ) ;
#92396 = CARTESIAN_POINT ( 'NONE',  ( 31.70422093597028734, 199.1115022471903160, -5.000000000000047962 ) ) ;
#92397 = CARTESIAN_POINT ( 'NONE',  ( -39.78121323716017343, 66.61922423961890161, -10.00000000000000000 ) ) ;
#92399 = CARTESIAN_POINT ( 'NONE',  ( 60.74296170696083408, 212.0024278399160949, 9.188101187500095079 ) ) ;
#92398 = CARTESIAN_POINT ( 'NONE',  ( 174.7354935756264638, 286.3370388987765409, 10.43770612672979503 ) ) ;
#92400 = CARTESIAN_POINT ( 'NONE',  ( 164.4989226152910646, 245.7265035704120351, -6.575810094723514965 ) ) ;
#92401 = CARTESIAN_POINT ( 'NONE',  ( 72.90605544040717234, 57.09015056262271059, 16.39620496795493665 ) ) ;
#92402 = CARTESIAN_POINT ( 'NONE',  ( -29.37075727991403440, 94.88921800892813962, 44.57229221387616036 ) ) ;
#92403 = CARTESIAN_POINT ( 'NONE',  ( 66.42322958073232542, 68.80919999086530936, -4.344013851444929131 ) ) ;
#92404 = ORIENTED_EDGE ( 'NONE', *, *, #56831, .T. ) ;
#92405 = CARTESIAN_POINT ( 'NONE',  ( 20.08504676852914272, 175.7365022471902307, -10.00000000000009059 ) ) ;
#92406 = CARTESIAN_POINT ( 'NONE',  ( 208.2777459429579210, 269.8993572713111462, 3.129643751043610589 ) ) ;
#92407 = CARTESIAN_POINT ( 'NONE',  ( 142.6909626358283560, 247.0643266524159856, -9.188101187500093303 ) ) ;
#92408 = CARTESIAN_POINT ( 'NONE',  ( 33.90351810284484202, 25.28920272979928896, -7.433330006724141015 ) ) ;
#92409 = CARTESIAN_POINT ( 'NONE',  ( 164.3421951250510631, 260.7081190328407843, -16.15447616004134446 ) ) ;
#92410 = CARTESIAN_POINT ( 'NONE',  ( 21.99520779934447745, 195.0530062829863311, -4.648177544792955347E-16 ) ) ;
#92411 = CARTESIAN_POINT ( 'NONE',  ( 194.9528736489464791, 280.9848362485358280, -17.70191856674237840 ) ) ;
#92413 = CARTESIAN_POINT ( 'NONE',  ( 185.4588683995272902, 277.6883572167094485, -17.52057745498484920 ) ) ;
#92412 = CARTESIAN_POINT ( 'NONE',  ( 68.98401675473516548, 68.40627949866706103, 8.275036679873185363 ) ) ;
#92414 = CARTESIAN_POINT ( 'NONE',  ( 68.56394572365037732, 64.18846526882273906, 11.84148672416030124 ) ) ;
#92415 = ORIENTED_EDGE ( 'NONE', *, *, #9594, .T. ) ;
#92416 = CARTESIAN_POINT ( 'NONE',  ( 150.8359915840788688, 269.3913942967808453, 15.73449616766854575 ) ) ;
#92417 = CARTESIAN_POINT ( 'NONE',  ( 177.8086748658496674, 286.5436072803887555, 13.62650167180037641 ) ) ;
#92418 = CARTESIAN_POINT ( 'NONE',  ( 156.6086985941140313, 280.0481763786762599, -5.331284326237024196 ) ) ;
#92419 = CARTESIAN_POINT ( 'NONE',  ( 14.85095921958720666, 14.28920272979925699, -7.433330006724141015 ) ) ;
#92420 = ORIENTED_EDGE ( 'NONE', *, *, #33722, .T. ) ;
#92421 = CARTESIAN_POINT ( 'NONE',  ( 160.3024851031978528, 252.9949465521450520, 16.22879458631637561 ) ) ;
#92422 = DIRECTION ( 'NONE',  ( -1.000000000000000000, 0.000000000000000000, 0.000000000000000000 ) ) ;
#92423 = CARTESIAN_POINT ( 'NONE',  ( 69.69525977227351632, 62.53367147251394442, 13.41414775225847755 ) ) ;
#92424 = EDGE_CURVE ( 'NONE', #77091, #100075, #1756, .T. ) ;
#92425 = CARTESIAN_POINT ( 'NONE',  ( 71.71459329694582152, 72.12586688595882833, 0.6178152589126062466 ) ) ;
#92426 = LINE ( 'NONE', #21501, #10147 ) ;
#92427 = LINE ( 'NONE', #71106, #9975 ) ;
#92428 = CARTESIAN_POINT ( 'NONE',  ( 149.6779600888696677, 272.0038180561006698, 11.37632069153431580 ) ) ;
#92429 = CARTESIAN_POINT ( 'NONE',  ( 162.8223739550644211, 248.6303710312858186, -11.16939803179192658 ) ) ;
#92430 = VECTOR ( 'NONE', #8398, 1000.000000000000000 ) ;
#92431 = CARTESIAN_POINT ( 'NONE',  ( 200.6583719735737645, 283.0965001081523269, -17.35266956530146132 ) ) ;
#92432 = ORIENTED_EDGE ( 'NONE', *, *, #93892, .T. ) ;
#92433 = CARTESIAN_POINT ( 'NONE',  ( 192.4947987708966650, 281.8339256886280282, 16.78223888497653604 ) ) ;
#92434 = CYLINDRICAL_SURFACE ( 'NONE', #28838, 70.00000000000002842 ) ;
#92435 = ORIENTED_EDGE ( 'NONE', *, *, #63166, .T. ) ;
#92436 = CARTESIAN_POINT ( 'NONE',  ( 190.6893905452545823, 300.3632824417117604, 3.294993852933539191 ) ) ;
#92437 = CARTESIAN_POINT ( 'NONE',  ( 16.81940930487741426, 170.5177522451417929, 5.000000000000051514 ) ) ;
#92438 = CARTESIAN_POINT ( 'NONE',  ( 81.37277742391516711, 45.49914513073889566, -11.21303457981032103 ) ) ;
#92439 = VERTEX_POINT ( 'NONE', #63032 ) ;
#92441 = EDGE_CURVE ( 'NONE', #11925, #50507, #48999, .T. ) ;
#92440 = CARTESIAN_POINT ( 'NONE',  ( 146.6138605399200117, 276.7043397814778132, -0.5394499176159462950 ) ) ;
#92442 = DIRECTION ( 'NONE',  ( -1.000000000000000000, 0.000000000000000000, 0.000000000000000000 ) ) ;
#92443 = CARTESIAN_POINT ( 'NONE',  ( 196.6317700900902139, 290.0707791521982131, -17.91116578096951883 ) ) ;
#92444 = DIRECTION ( 'NONE',  ( 0.000000000000000000, 0.000000000000000000, 1.000000000000000000 ) ) ;
#92445 = CARTESIAN_POINT ( 'NONE',  ( 69.41441713838028704, 62.72891755904008448, 13.20643227790562335 ) ) ;
#92446 = EDGE_LOOP ( 'NONE', ( #69949, #78349, #58596 ) ) ;
#92447 = CARTESIAN_POINT ( 'NONE',  ( 108.5372593219620683, 221.2202760586659167, -5.415160957724236172E-17 ) ) ;
#92448 = CARTESIAN_POINT ( 'NONE',  ( 155.7819252383450248, 260.8247859167269667, 17.61512984275023896 ) ) ;
#92449 = CARTESIAN_POINT ( 'NONE',  ( 150.6533415055477008, 269.7077535128032082, 14.84621632544246062 ) ) ;
#92450 = CARTESIAN_POINT ( 'NONE',  ( 81.68042570781203437, 42.31879938090973070, -8.022231220700685839 ) ) ;
#92451 = ORIENTED_EDGE ( 'NONE', *, *, #33282, .T. ) ;
#92452 = ORIENTED_EDGE ( 'NONE', *, *, #33636, .F. ) ;
#92453 = ORIENTED_EDGE ( 'NONE', *, *, #62772, .F. ) ;
#92454 = CARTESIAN_POINT ( 'NONE',  ( 73.95930103172710801, 63.91830289297120515, 14.08246017068975142 ) ) ;
#92455 = B_SPLINE_CURVE_WITH_KNOTS ( 'NONE', 3,
 ( #98886, #6165, #13293, #59858 ),
 .UNSPECIFIED., .F., .F.,
 ( 4, 4 ),
 ( 0.009316165907098234583, 0.01506860168139122214 ),
 .UNSPECIFIED. ) ;
#92456 = EDGE_LOOP ( 'NONE', ( #20059, #59126, #42414, #14785 ) ) ;
#92457 = CARTESIAN_POINT ( 'NONE',  ( 67.75555162469370885, 67.74667152934745218, 7.221070002596457371 ) ) ;
#92458 = ORIENTED_EDGE ( 'NONE', *, *, #77797, .F. ) ;
#92459 = CARTESIAN_POINT ( 'NONE',  ( 207.5290616128274337, 271.1961165699281651, 2.604679844609484984 ) ) ;
#92460 = CARTESIAN_POINT ( 'NONE',  ( 81.98865867772765625, 45.57652215286253750, 10.94910104189580657 ) ) ;
#92461 = CARTESIAN_POINT ( 'NONE',  ( -71.61465314115659453, 63.06504152958490295, 60.00000000000000000 ) ) ;
#92462 = CARTESIAN_POINT ( 'NONE',  ( 194.6310785344323904, 293.5360785768717165, -14.54510914272505495 ) ) ;
#92463 = CARTESIAN_POINT ( 'NONE',  ( 82.53793375827495993, 54.22719885510827709, -15.94096427280454442 ) ) ;
#92464 = DIRECTION ( 'NONE',  ( -0.8321961394790272637, 0.5544813661758195567, 0.000000000000000000 ) ) ;
#92465 = CARTESIAN_POINT ( 'NONE',  ( 17.47068606603513530, 15.80170272979925628, 7.433330006724137462 ) ) ;
#92466 = FACE_OUTER_BOUND ( 'NONE', #4975, .T. ) ;
#92467 = CARTESIAN_POINT ( 'NONE',  ( 78.75297625639956323, 47.66336229257159118, 14.29739783539339371 ) ) ;
#92469 = VERTEX_POINT ( 'NONE', #10350 ) ;
#92468 = CARTESIAN_POINT ( 'NONE',  ( 79.14312167556931854, 57.64441083166269664, 0.000000000000000000 ) ) ;
#92470 = CARTESIAN_POINT ( 'NONE',  ( 163.1484656051875106, 248.0655637253488806, 9.714247672444804138 ) ) ;
#92471 = CARTESIAN_POINT ( 'NONE',  ( 206.7893622945242385, 272.4773133715531230, -10.52881283832460291 ) ) ;
#92472 = CARTESIAN_POINT ( 'NONE',  ( 165.9091197491159164, 246.2627970730538323, -2.747640711776688338 ) ) ;
#92473 = CARTESIAN_POINT ( 'NONE',  ( 79.48876273271771709, 46.38894273206648222, -12.71961528548989406 ) ) ;
#92474 = CARTESIAN_POINT ( 'NONE',  ( 171.4611298474229386, 255.5042682504870584, 11.10224729584274428 ) ) ;
#92475 = CARTESIAN_POINT ( 'NONE',  ( 158.0103319884112523, 281.0314316241064603, 2.028691772727660769 ) ) ;
#92476 = ORIENTED_EDGE ( 'NONE', *, *, #33121, .T. ) ;
#92477 = CARTESIAN_POINT ( 'NONE',  ( 194.6195663601007766, 293.5560182477196918, -14.78158780203209233 ) ) ;
#92478 = CARTESIAN_POINT ( 'NONE',  ( 72.59700804457577306, 63.00543003063684466, -14.10603509414891654 ) ) ;
#92479 = LINE ( 'NONE', #62518, #80802 ) ;
#92480 = CARTESIAN_POINT ( 'NONE',  ( 2.890834060677703210, 159.1427522451417644, 1.119607411625061291E-15 ) ) ;
#92481 = CARTESIAN_POINT ( 'NONE',  ( 196.1299550548953050, 269.6200306317458057, -11.66289591416585480 ) ) ;
#92482 = CARTESIAN_POINT ( 'NONE',  ( 144.6270795744234476, 268.7413018095040798, -2.761272660171008000E-15 ) ) ;
#92483 = CARTESIAN_POINT ( 'NONE',  ( 169.6888855313890474, 280.6163284094095047, -14.28460871240806540 ) ) ;
#92484 = DIRECTION ( 'NONE',  ( 1.000000000000000000, 0.000000000000000000, 0.000000000000000000 ) ) ;
#92486 = CARTESIAN_POINT ( 'NONE',  ( 115.2960263294082068, 225.8262482093458061, 3.021315404115420679E-15 ) ) ;
#92485 = CARTESIAN_POINT ( 'NONE',  ( -0.5279885150232012103, 164.3768266524160140, -9.188101187500091527 ) ) ;
#92487 = EDGE_CURVE ( 'NONE', #35590, #22676, #85904, .T. ) ;
#92488 = CARTESIAN_POINT ( 'NONE',  ( 17.68543470866176648, 191.0177522451419065, 5.000000000000046185 ) ) ;
#92489 = ORIENTED_EDGE ( 'NONE', *, *, #34876, .F. ) ;
#92490 = ORIENTED_EDGE ( 'NONE', *, *, #95250, .F. ) ;
#92491 = DIRECTION ( 'NONE',  ( -0.7957378174433876739, 0.6056412518070690698, 0.000000000000000000 ) ) ;
#92492 = EDGE_CURVE ( 'NONE', #4349, #48417, #41217, .T. ) ;
#92493 = CARTESIAN_POINT ( 'NONE',  ( 83.03036255845053404, 46.46437440478001690, -11.26726318583448183 ) ) ;
#92494 = CYLINDRICAL_SURFACE ( 'NONE', #11374, 1.449999999999993072 ) ;
#92495 = VECTOR ( 'NONE', #94292, 1000.000000000000114 ) ;
#92496 = DIRECTION ( 'NONE',  ( -0.5000000000000006661, 0.8660254037844382635, -1.877843081442120958E-16 ) ) ;
#92497 = CARTESIAN_POINT ( 'NONE',  ( 82.03292314450337130, 42.28330721560684680, 6.570821834211296952 ) ) ;
#92498 = CARTESIAN_POINT ( 'NONE',  ( 153.1046550690079187, 278.4315285291231135, 3.738693302458024448 ) ) ;
#92499 = CARTESIAN_POINT ( 'NONE',  ( 8.294124642383250645, 187.8464784336662206, 1.353441290958777525E-15 ) ) ;
#92500 = CARTESIAN_POINT ( 'NONE',  ( 115.2486091055264410, 237.3458772461660544, 9.188101187500095079 ) ) ;
#92501 = CARTESIAN_POINT ( 'NONE',  ( 179.1786855675093477, 291.9707536515992956, -6.147306910137406710 ) ) ;
#92502 = CARTESIAN_POINT ( 'NONE',  ( 195.9340754144258199, 275.1539484599448997, 15.83571573274672417 ) ) ;
#92503 = EDGE_CURVE ( 'NONE', #86106, #9838, #23198, .T. ) ;
#92504 = CARTESIAN_POINT ( 'NONE',  ( 150.0488362022254023, 271.5008970094041842, -11.96187989116652162 ) ) ;
#92505 = CARTESIAN_POINT ( 'NONE',  ( 178.4764170025789554, 283.7516055304348583, -14.72289439906822217 ) ) ;
#92506 = CARTESIAN_POINT ( 'NONE',  ( 76.56057136519696371, 54.76627436849224750, -16.10539304684806083 ) ) ;
#92507 = CARTESIAN_POINT ( 'NONE',  ( 195.6986305151803549, 291.6870243064952888, 16.84182339398051909 ) ) ;
#92508 = CARTESIAN_POINT ( 'NONE',  ( 194.4459411895494725, 293.8567458645873103, 14.31012567920753042 ) ) ;
#92509 = CARTESIAN_POINT ( 'NONE',  ( 207.1572261440131797, 271.8401544939704877, -5.633070628900782140 ) ) ;
#92510 = CARTESIAN_POINT ( 'NONE',  ( 190.1357066293690536, 284.8999334207817924, 17.11029449594927243 ) ) ;
#92511 = EDGE_CURVE ( 'NONE', #5086, #43088, #32122, .T. ) ;
#92512 = CARTESIAN_POINT ( 'NONE',  ( 189.2284142613084157, 262.6620465936063056, 8.058909338376276210 ) ) ;
#92513 = CARTESIAN_POINT ( 'NONE',  ( 171.5551119485164975, 279.8722202788326285, 13.93221665515422991 ) ) ;
#92514 = CARTESIAN_POINT ( 'NONE',  ( 192.5337445403046104, 265.2601942734702902, 7.958587396316798568 ) ) ;
#92515 = CARTESIAN_POINT ( 'NONE',  ( 191.5521510896938935, 298.8689373439769952, -9.847378829740700112 ) ) ;
#92516 = CARTESIAN_POINT ( 'NONE',  ( 189.9925954911225290, 301.5701668779311717, 0.1154287172046158938 ) ) ;
#92517 = CARTESIAN_POINT ( 'NONE',  ( 180.7798174273501388, 266.8764815076470995, -14.74666571146830307 ) ) ;
#92518 = ADVANCED_FACE ( 'NONE', ( #32634 ), #63531, .F. ) ;
#92519 = ORIENTED_EDGE ( 'NONE', *, *, #96333, .F. ) ;
#92520 = CARTESIAN_POINT ( 'NONE',  ( 154.0199539993881217, 276.0341879782693582, -10.88229598812187682 ) ) ;
#92521 =( BOUNDED_CURVE ( )  B_SPLINE_CURVE ( 2, ( #75045, #13249, #91256, #91754, #50717, #44106, #12754, #43617, #90778 ),
 .UNSPECIFIED., .F., .T. ) 
 B_SPLINE_CURVE_WITH_KNOTS ( ( 3, 2, 2, 2, 3 ),
 ( 0.5443548387096773800, 0.5456989247311827551, 0.5483870967741935054, 0.5510752688172042557, 0.5524193548387096309 ),
 .UNSPECIFIED. ) 
 CURVE ( )  GEOMETRIC_REPRESENTATION_ITEM ( )  RATIONAL_B_SPLINE_CURVE ( ( 0.9330127018922194093, 0.9330127018922194093, 1.000000000000000000, 0.8660254037844387076, 1.000000000000000000, 0.8660254037844387076, 1.000000000000000000, 0.9330127018922194093, 0.9330127018922194093 ) ) 
 REPRESENTATION_ITEM ( '' )  );
#92522 = CARTESIAN_POINT ( 'NONE',  ( 163.7587049410067266, 247.0085981909329576, -6.137518685179130351 ) ) ;
#92523 = CARTESIAN_POINT ( 'NONE',  ( -52.33464467766007289, 32.58262665401804270, -10.00000000000000000 ) ) ;
#92524 = CARTESIAN_POINT ( 'NONE',  ( 98.52366704282199805, 221.5643266524159856, -9.188101187500093303 ) ) ;
#92525 = CARTESIAN_POINT ( 'NONE',  ( 9.022134044517839513, 26.18502408145589655, 5.678558825948277544 ) ) ;
#92526 = CARTESIAN_POINT ( 'NONE',  ( 191.5766842709549280, 298.8264446275616137, 8.039910086100929831 ) ) ;
#92527 = CARTESIAN_POINT ( 'NONE',  ( 81.30975366074838462, 56.24313983998633404, -16.44754541364716971 ) ) ;
#92529 = CARTESIAN_POINT ( 'NONE',  ( 86.80939509573987323, 43.35552860557069010, -0.1859311002499181298 ) ) ;
#92528 = DIRECTION ( 'NONE',  ( 0.4999999999999992784, -0.8660254037844390407, 0.000000000000000000 ) ) ;
#92530 = CARTESIAN_POINT ( 'NONE',  ( 149.2285814192496218, 272.1755103708678121, 13.04936292285073485 ) ) ;
#92531 = B_SPLINE_CURVE_WITH_KNOTS ( 'NONE', 3,
 ( #52121, #36925, #97756, #20753, #90178, #74952, #52615, #45020, #99245, #60702, #22226, #84084, #14635, #37907, #68817, #99744, #61219, #22736, #77396, #7474, #84528, #91618, #38873, #92622, #75407, #69280, #45475, #21694, #68777, #69778, #387, #62163, #100206, #53573, #67793, #52576, #53083, #31275, #93112, #37376, #15072, #14596, #45961, #76878, #37867, #30793, #38369, #98719, #83530, #84037, #23664, #54556 ),
 .UNSPECIFIED., .F., .F.,
 ( 4, 2, 2, 2, 2, 2, 2, 2, 2, 2, 2, 2, 2, 2, 2, 2, 2, 2, 2, 2, 2, 2, 2, 2, 2, 4 ),
 ( 0.0008597875087230317853, 0.001056026466501868441, 0.001154145945391277283, 0.001252265424280685907, 0.001448504382059393435, 0.001644743339838100745, 0.002037221255395451399, 0.002429699170952801836, 0.003214655002067501408, 0.003999610833182200113, 0.004784566664296898385, 0.005177044579854248388, 0.005373283537632888261, 0.005471403016522252000, 0.005520462755966851036, 0.005569522495411450939, 0.005618582234856050843, 0.005667641974300649879, 0.005765761453189883513, 0.005962000410968388946, 0.006158239368746893511, 0.006354478326525398076, 0.006550717284303903508, 0.006746956242082408073, 0.006943195199860913505, 0.007139434157639417203 ),
 .UNSPECIFIED. ) ;
#92532 = CARTESIAN_POINT ( 'NONE',  ( 150.8168331730346949, 269.4245776381016526, -15.71017957295074652 ) ) ;
#92533 = CARTESIAN_POINT ( 'NONE',  ( 149.8554569740625197, 271.5993192349010315, -11.69353262999953103 ) ) ;
#92534 = CARTESIAN_POINT ( 'NONE',  ( 58.13834967963523326, 192.8262482093458061, 3.021315404115420679E-15 ) ) ;
#92535 = DIRECTION ( 'NONE',  ( 0.000000000000000000, 0.000000000000000000, 1.000000000000000000 ) ) ;
#92536 = CARTESIAN_POINT ( 'NONE',  ( -8.406493707509316238, 25.24382671950691304, 10.00000000000000000 ) ) ;
#92537 = EDGE_LOOP ( 'NONE', ( #50271, #2967, #57121, #93880 ) ) ;
#92538 = CARTESIAN_POINT ( 'NONE',  ( 25.99623195869281744, 35.98502408145594700, -5.678558825948271327 ) ) ;
#92539 = CARTESIAN_POINT ( 'NONE',  ( 71.96639307748559133, 71.49757472301891426, -5.734781593071442529 ) ) ;
#92540 = CARTESIAN_POINT ( 'NONE',  ( 196.5802072422632421, 267.8039352643175448, 9.492349405241153448 ) ) ;
#92541 = CARTESIAN_POINT ( 'NONE',  ( 196.6317700900902139, 290.0707791521982131, -17.91116578096951883 ) ) ;
#92542 = ADVANCED_FACE ( 'NONE', ( #88909 ), #18958, .F. ) ;
#92543 = VERTEX_POINT ( 'NONE', #80794 ) ;
#92544 = B_SPLINE_SURFACE_WITH_KNOTS ( 'NONE', 3, 1, ( 
 ( #59993, #75728 ),
 ( #99524, #45300 ),
 ( #61494, #6808 ),
 ( #69096, #91957 ),
 ( #68105, #14895 ),
 ( #37204, #92445 ),
 ( #22990, #62477 ),
 ( #8309, #30107 ),
 ( #47291, #100023 ),
 ( #77723, #38180 ),
 ( #53882, #69599 ),
 ( #37690, #29613 ),
 ( #54893, #204 ),
 ( #76234, #30609 ),
 ( #15380, #99026 ),
 ( #16400, #77203 ),
 ( #78217, #70090 ),
 ( #23995, #84842 ),
 ( #91444, #700 ),
 ( #76705, #83852 ),
 ( #46277, #14418 ),
 ( #7808, #45784 ),
 ( #68600, #22505 ),
 ( #61977, #85347 ),
 ( #31090, #85873 ),
 ( #92931, #7299 ),
 ( #23483, #84348 ),
 ( #60990, #38694 ),
 ( #53399, #54373 ),
 ( #93442, #39173 ),
 ( #15894, #60485 ) ),
 .UNSPECIFIED., .F., .F., .F.,
 ( 4, 3, 3, 3, 3, 3, 3, 3, 3, 3, 4 ),
 ( 2, 2 ),
 ( 0.000000000000000000, 0.1122669598086646486, 0.2243161639709356503, 0.3396355846218876984, 0.4553962076585064134, 0.5677860799922357371, 0.6749047109689600976, 0.7773884377078469354, 0.8775581155834195624, 0.9782364162377885641, 1.000000000000000000 ),
 ( 0.000000000000000000, 1.000000000000000000 ),
 .UNSPECIFIED. ) ;
#92545 = CARTESIAN_POINT ( 'NONE',  ( 84.44631528110988938, 49.90853024617071299, -13.72425691458318475 ) ) ;
#92546 = CARTESIAN_POINT ( 'NONE',  ( 85.51825389741982519, 45.42935502215924259, 9.290761976430086833 ) ) ;
#92547 = FACE_OUTER_BOUND ( 'NONE', #94334, .T. ) ;
#92548 = CARTESIAN_POINT ( 'NONE',  ( 173.1432744218939774, 253.4296248983395401, -9.251738304191658102 ) ) ;
#92549 = CARTESIAN_POINT ( 'NONE',  ( 192.2431834237441706, 297.6720342317289578, 11.07782187406058938 ) ) ;
#92550 = EDGE_CURVE ( 'NONE', #5319, #34942, #54586, .T. ) ;
#92551 = ORIENTED_EDGE ( 'NONE', *, *, #14832, .F. ) ;
#92552 = CARTESIAN_POINT ( 'NONE',  ( 187.5872943901169378, 278.9980123648381891, 16.95840433791729396 ) ) ;
#92553 = CARTESIAN_POINT ( 'NONE',  ( 38.16387531507685793, 24.96004757982092315, -5.678558825948276656 ) ) ;
#92554 = VERTEX_POINT ( 'NONE', #5235 ) ;
#92555 = CARTESIAN_POINT ( 'NONE',  ( 66.52662661294374402, 68.71800325113713370, 4.800704629298682136 ) ) ;
#92557 = EDGE_CURVE ( 'NONE', #73949, #48810, #57928, .T. ) ;
#92556 = LINE ( 'NONE', #317, #67738 ) ;
#92558 = ORIENTED_EDGE ( 'NONE', *, *, #60442, .F. ) ;
#92560 = EDGE_CURVE ( 'NONE', #90346, #63237, #49589, .T. ) ;
#92559 = CARTESIAN_POINT ( 'NONE',  ( 86.55235766077406367, 47.22292317728852140, -10.66532192617879637 ) ) ;
#92561 = CARTESIAN_POINT ( 'NONE',  ( 206.2925202860113245, 273.3378689736323963, 11.27730907742713384 ) ) ;
#92562 = CARTESIAN_POINT ( 'NONE',  ( 85.05685448785742153, 49.86430017123296210, 13.48384481714161787 ) ) ;
#92563 = CARTESIAN_POINT ( 'NONE',  ( 154.0425198334700099, 263.8375244529303245, -16.86014285715240035 ) ) ;
#92564 = CARTESIAN_POINT ( 'NONE',  ( 201.1679199471075492, 282.2139371290980989, -16.62385308864941535 ) ) ;
#92565 = EDGE_CURVE ( 'NONE', #53210, #20188, #81770, .T. ) ;
#92566 = DIRECTION ( 'NONE',  ( 0.4999999999999992784, -0.8660254037844390407, 0.000000000000000000 ) ) ;
#92567 = DIRECTION ( 'NONE',  ( 0.5000000000000013323, -0.8660254037844378194, 0.000000000000000000 ) ) ;
#92568 = EDGE_CURVE ( 'NONE', #75209, #34863, #95898, .T. ) ;
#92569 = DIRECTION ( 'NONE',  ( 0.000000000000000000, 0.000000000000000000, 1.000000000000000000 ) ) ;
#92570 = VERTEX_POINT ( 'NONE', #58900 ) ;
#92571 = CARTESIAN_POINT ( 'NONE',  ( 176.0924988190274121, 258.7481610597934605, 13.20100988338283088 ) ) ;
#92572 = ORIENTED_EDGE ( 'NONE', *, *, #88248, .T. ) ;
#92573 = ORIENTED_EDGE ( 'NONE', *, *, #88127, .F. ) ;
#92574 = CARTESIAN_POINT ( 'NONE',  ( 172.8345891994052579, 271.0481249001369406, 16.42822092899199049 ) ) ;
#92575 = CARTESIAN_POINT ( 'NONE',  ( 79.81870009848962866, 57.67573475680517703, 16.25934251437179512 ) ) ;
#92576 = ORIENTED_EDGE ( 'NONE', *, *, #83409, .F. ) ;
#92578 = CARTESIAN_POINT ( 'NONE',  ( 164.4200829731848046, 246.2493134173791418, 2.172245655849200485 ) ) ;
#92577 = CARTESIAN_POINT ( 'NONE',  ( 0.005075371086064872639, 27.18819441265828019, 10.00000000000000000 ) ) ;
#92579 = DIRECTION ( 'NONE',  ( 0.4999999999999992784, -0.8660254037844390407, 0.000000000000000000 ) ) ;
#92580 = CARTESIAN_POINT ( 'NONE',  ( 200.4204578720470522, 274.6855620619879232, -13.71762816491924220 ) ) ;
#92581 = CARTESIAN_POINT ( 'NONE',  ( 15.77038241084232517, 34.14663330942826747, -10.00000000000000000 ) ) ;
#92582 = CARTESIAN_POINT ( 'NONE',  ( 147.0314375879888757, 275.9810751181479986, -5.168577011192616588 ) ) ;
#92583 = CARTESIAN_POINT ( 'NONE',  ( 171.4353610529350078, 250.3536029180922640, -5.787908394485046237 ) ) ;
#92584 = DIRECTION ( 'NONE',  ( -1.000000000000000000, 0.000000000000000000, 0.000000000000000000 ) ) ;
#92585 = CARTESIAN_POINT ( 'NONE',  ( 178.0362726450289017, 255.4666490453336678, 5.105776653552220878 ) ) ;
#92586 = CARTESIAN_POINT ( 'NONE',  ( 70.43138065582230922, 60.95397308647202550, -14.95463465097626354 ) ) ;
#92587 = CARTESIAN_POINT ( 'NONE',  ( 37.18479240120036167, 39.65586893147759895, -7.433330006724137462 ) ) ;
#92588 = CARTESIAN_POINT ( 'NONE',  ( 188.1412547211656943, 273.5593357346770063, 17.08033167198486879 ) ) ;
#92589 = ORIENTED_EDGE ( 'NONE', *, *, #22519, .F. ) ;
#92590 = CARTESIAN_POINT ( 'NONE',  ( 86.81792973151222270, 45.86417987983289635, -8.215134288092611925 ) ) ;
#92591 = CARTESIAN_POINT ( 'NONE',  ( 74.16718187723988365, 63.24922278397193764, -14.42629137139557827 ) ) ;
#92592 = DIRECTION ( 'NONE',  ( -0.8660254037844378194, -0.5000000000000013323, -0.000000000000000000 ) ) ;
#92593 = CARTESIAN_POINT ( 'NONE',  ( 192.0519773745460554, 298.0032128236547351, 11.68523422658327249 ) ) ;
#92594 = CARTESIAN_POINT ( 'NONE',  ( 72.00815872078212010, 61.71914051830567161, 14.51550446260311134 ) ) ;
#92595 = CARTESIAN_POINT ( 'NONE',  ( 201.1755594471486859, 282.2007051268825535, -18.15567516623250910 ) ) ;
#92596 = FACE_OUTER_BOUND ( 'NONE', #1617, .T. ) ;
#92597 = VERTEX_POINT ( 'NONE', #3752 ) ;
#92598 = CARTESIAN_POINT ( 'NONE',  ( 195.0715819075916215, 292.7731043536545030, 16.72244352212509710 ) ) ;
#92599 = ORIENTED_EDGE ( 'NONE', *, *, #11465, .F. ) ;
#92600 = CARTESIAN_POINT ( 'NONE',  ( 194.8432095198904221, 293.1686569321988145, -14.74101036184996616 ) ) ;
#92601 = CARTESIAN_POINT ( 'NONE',  ( -19.65312891409028850, 79.99999999999991473, 54.99999999999999289 ) ) ;
#92602 = ORIENTED_EDGE ( 'NONE', *, *, #13227, .T. ) ;
#92603 = CARTESIAN_POINT ( 'NONE',  ( 190.3065890357339356, 267.3458242085297911, -11.97292556197838209 ) ) ;
#92604 = B_SPLINE_CURVE_WITH_KNOTS ( 'NONE', 3,
 ( #65718, #64232, #34817, #55609 ),
 .UNSPECIFIED., .F., .F.,
 ( 4, 4 ),
 ( 0.02515406699106021923, 0.03440006065807557634 ),
 .UNSPECIFIED. ) ;
#92605 = CARTESIAN_POINT ( 'NONE',  ( 190.8715817853789645, 283.7415510105400926, -16.63753925581049486 ) ) ;
#92606 = CARTESIAN_POINT ( 'NONE',  ( 192.3743113064165584, 262.7446559956477472, 4.590962410021210971 ) ) ;
#92607 = CARTESIAN_POINT ( 'NONE',  ( -10.09954699608895901, 171.6427522451419350, -10.00000000000009592 ) ) ;
#92608 = CARTESIAN_POINT ( 'NONE',  ( 204.8008807586744524, 272.7600038595665524, -10.89009281376315741 ) ) ;
#92610 = CARTESIAN_POINT ( 'NONE',  ( 160.7842430252816541, 281.5629877887335510, 5.625797120217996827 ) ) ;
#92609 = CARTESIAN_POINT ( 'NONE',  ( 184.3834185992925825, 288.5535061363751765, -13.68474095756436881 ) ) ;
#92611 = CIRCLE ( 'NONE', #82925, 17.82106496071138935 ) ;
#92612 = CARTESIAN_POINT ( 'NONE',  ( 153.3506059258413643, 265.0359544954067132, -16.39100908615009899 ) ) ;
#92613 = ORIENTED_EDGE ( 'NONE', *, *, #45378, .F. ) ;
#92614 = DIRECTION ( 'NONE',  ( 0.000000000000000000, 0.000000000000000000, -1.000000000000000000 ) ) ;
#92615 = PLANE ( 'NONE',  #98294 ) ;
#92616 = CARTESIAN_POINT ( 'NONE',  ( 186.9340657304752540, 262.8988569655599576, -9.024534070206733816 ) ) ;
#92617 = CARTESIAN_POINT ( 'NONE',  ( 198.2505066714982149, 285.2670451491296149, 0.000000000000000000 ) ) ;
#92618 = CARTESIAN_POINT ( 'NONE',  ( 192.6739937146571151, 271.4875022964622531, -15.03443561379086191 ) ) ;
#92619 = CARTESIAN_POINT ( 'NONE',  ( 3.924699723655708627, 184.6199935810940929, 2.679491924311251605 ) ) ;
#92620 = CARTESIAN_POINT ( 'NONE',  ( 82.21690911714624406, 41.97360749678824732, 5.658590786372603709 ) ) ;
#92621 = CARTESIAN_POINT ( 'NONE',  ( 39.64431452495993824, 58.26521502737223557, -10.00000000000000000 ) ) ;
#92622 = CARTESIAN_POINT ( 'NONE',  ( 191.3994361718305015, 283.5433174942932624, -16.59339826374022309 ) ) ;
#92623 = CARTESIAN_POINT ( 'NONE',  ( 72.17187393125894346, 66.23161324361963409, -12.52721847853723247 ) ) ;
#92624 = CARTESIAN_POINT ( 'NONE',  ( 66.23672358827711548, 218.2369531367911293, -4.594050593750048428 ) ) ;
#92625 = LINE ( 'NONE', #390, #67042 ) ;
#92626 = CARTESIAN_POINT ( 'NONE',  ( 147.4323331177958494, 275.2867036919951147, -5.064030047414062707 ) ) ;
#92627 = CARTESIAN_POINT ( 'NONE',  ( 163.1369207721744772, 248.0855599626920593, -11.24692769914530110 ) ) ;
#92628 = EDGE_CURVE ( 'NONE', #91687, #48146, #81279, .T. ) ;
#92629 = CARTESIAN_POINT ( 'NONE',  ( 154.9067123643522734, 262.3406990819208886, -18.18534662427576265 ) ) ;
#92630 = CARTESIAN_POINT ( 'NONE',  ( 207.7836085030675690, 270.7552284231231852, -5.468305433308493058 ) ) ;
#92631 = CARTESIAN_POINT ( 'NONE',  ( 202.8499463704053198, 279.3005819042728604, 17.04674939340617001 ) ) ;
#92632 = CARTESIAN_POINT ( 'NONE',  ( 162.8513067182543921, 284.1523628685703216, 6.041541777105626565 ) ) ;
#92634 = CARTESIAN_POINT ( 'NONE',  ( 76.43143940513256496, 51.47447208219396231, 15.62944959062109440 ) ) ;
#92633 = CARTESIAN_POINT ( 'NONE',  ( 73.48070833180072725, 69.95435187952867295, -9.683457271946362965 ) ) ;
#92635 = CARTESIAN_POINT ( 'NONE',  ( 185.7372650184451857, 257.4645284076796656, -2.264991511946413505E-12 ) ) ;
#92636 = EDGE_CURVE ( 'NONE', #12691, #58645, #91054, .T. ) ;
#92637 = CARTESIAN_POINT ( 'NONE',  ( 169.2563262549492151, 252.1410605716396560, -8.850704283268973072 ) ) ;
#92638 = CARTESIAN_POINT ( 'NONE',  ( 205.1068273514435703, 275.3915493784789419, -12.24197861934597142 ) ) ;
#92639 = CARTESIAN_POINT ( 'NONE',  ( 195.7291534503633272, 291.6341570319625021, 16.44925029361851543 ) ) ;
#92640 = DIRECTION ( 'NONE',  ( -0.000000000000000000, -0.000000000000000000, 1.000000000000000000 ) ) ;
#92641 = EDGE_CURVE ( 'NONE', #6854, #84457, #50328, .T. ) ;
#92642 = CARTESIAN_POINT ( 'NONE',  ( 35.30381256655795852, 185.0643266524160140, 9.188101187500095079 ) ) ;
#92643 = CARTESIAN_POINT ( 'NONE',  ( 52.46142023538963173, 213.3464784336661637, 1.353441290958777327E-15 ) ) ;
#92644 = CARTESIAN_POINT ( 'NONE',  ( 164.1172920531512318, 247.2548588590273368, -6.812855435237894497 ) ) ;
#92645 = CARTESIAN_POINT ( 'NONE',  ( 88.10161777267849459, 43.64076697146427364, 0.1132407729617423420 ) ) ;
#92646 = CARTESIAN_POINT ( 'NONE',  ( 82.09089402055167284, 49.99296431688566145, -14.01874078344520669 ) ) ;
#92647 = CARTESIAN_POINT ( 'NONE',  ( 138.9828575061699496, 260.2369531367911009, -4.594050593750048428 ) ) ;
#92648 = CARTESIAN_POINT ( 'NONE',  ( 38.04107491472451841, 53.42442038713603125, 177.5919119679930134 ) ) ;
#92649 = CARTESIAN_POINT ( 'NONE',  ( 197.9229657308372907, 270.3857085654402113, -10.89782717189174654 ) ) ;
#92650 = CARTESIAN_POINT ( 'NONE',  ( 25.00689474275853286, 16.29860640527292759, -2.839279412974138328 ) ) ;
#92651 = CARTESIAN_POINT ( 'NONE',  ( -15.39849209473666569, 173.4637435831425307, 2.679491924311255158 ) ) ;
#92652 = LINE ( 'NONE', #13630, #13495 ) ;
#92653 = CARTESIAN_POINT ( 'NONE',  ( 14.85095921958720666, 14.28920272979925699, -7.433330006724141015 ) ) ;
#92654 = CARTESIAN_POINT ( 'NONE',  ( 56.27743144475606130, 212.4869531367911009, 4.594050593750046652 ) ) ;
#92655 = CARTESIAN_POINT ( 'NONE',  ( 158.8209852333526158, 256.8487328634645337, -16.76518060723513415 ) ) ;
#92656 = CARTESIAN_POINT ( 'NONE',  ( 42.87900647455834502, 24.75620593066997444, -1.732050807568748407 ) ) ;
#92657 = CARTESIAN_POINT ( 'NONE',  ( 159.4230536986738400, 254.5181664265525683, 16.83068086755798376 ) ) ;
#92658 = CARTESIAN_POINT ( 'NONE',  ( 53.62548896571601631, 201.7677522451418781, 10.00000000000009592 ) ) ;
#92659 = CARTESIAN_POINT ( 'NONE',  ( 151.4592217034740997, 275.9376209827681237, 7.243053434427960013 ) ) ;
#92660 = CARTESIAN_POINT ( 'NONE',  ( 112.2445834879230944, 245.6115022471903160, -5.000000000000047962 ) ) ;
#92661 = CARTESIAN_POINT ( 'NONE',  ( 200.3134965941964651, 283.6938417875134064, 18.29802468362849766 ) ) ;
#92662 = EDGE_CURVE ( 'NONE', #19580, #71349, #40059, .T. ) ;
#92663 = CARTESIAN_POINT ( 'NONE',  ( 165.0437781805843258, 244.7827860485373606, -2.050141714668513693 ) ) ;
#92664 = VERTEX_POINT ( 'NONE', #20444 ) ;
#92665 = CARTESIAN_POINT ( 'NONE',  ( 77.09205440684367261, 49.43085972797705097, 15.45120731324600349 ) ) ;
#92666 = CARTESIAN_POINT ( 'NONE',  ( 41.10245927640360719, 127.8322459559854138, 177.5919119679930134 ) ) ;
#92667 = ORIENTED_EDGE ( 'NONE', *, *, #38296, .T. ) ;
#92668 = CARTESIAN_POINT ( 'NONE',  ( 160.0081047537594543, 253.5048282741223602, -16.11956848123596941 ) ) ;
#92669 = CARTESIAN_POINT ( 'NONE',  ( 193.7981402883559099, 293.2477674331528874, 15.14322874797242768 ) ) ;
#92670 = CARTESIAN_POINT ( 'NONE',  ( 71.37166012509962343, 68.88869991590640041, -8.754280617899828698 ) ) ;
#92671 = ORIENTED_EDGE ( 'NONE', *, *, #73547, .F. ) ;
#92672 = ORIENTED_EDGE ( 'NONE', *, *, #15139, .T. ) ;
#92674 = ADVANCED_FACE ( 'NONE', ( #12856 ), #88880, .T. ) ;
#92673 = CARTESIAN_POINT ( 'NONE',  ( 165.0437781805843258, 244.7827860485373606, -2.050141714668513693 ) ) ;
#92675 = CARTESIAN_POINT ( 'NONE',  ( 147.7467138384290308, 274.7421803109381813, -9.190172068879620682 ) ) ;
#92676 = CARTESIAN_POINT ( 'NONE',  ( -22.42236680055709641, 157.8615022471902591, 0.000000000000000000 ) ) ;
#92678 = ORIENTED_EDGE ( 'NONE', *, *, #97239, .F. ) ;
#92677 = CIRCLE ( 'NONE', #52205, 70.00000000000001421 ) ;
#92679 = CARTESIAN_POINT ( 'NONE',  ( 23.56475526289127842, 35.64646525600391413, -2.839279412974133887 ) ) ;
#92680 = CARTESIAN_POINT ( 'NONE',  ( 27.68909066282341058, 16.39040679176984128, 1.333680081654574804E-15 ) ) ;
#92681 = DIRECTION ( 'NONE',  ( -1.000000000000000000, 0.000000000000000000, 0.000000000000000000 ) ) ;
#92682 = CARTESIAN_POINT ( 'NONE',  ( 75.03771487841179066, 67.29470115673240116, -12.93936238812017514 ) ) ;
#92683 = EDGE_CURVE ( 'NONE', #76358, #56880, #75633, .T. ) ;
#92684 = VECTOR ( 'NONE', #35195, 1000.000000000000000 ) ;
#92685 = ORIENTED_EDGE ( 'NONE', *, *, #94357, .T. ) ;
#92686 = PLANE ( 'NONE',  #83850 ) ;
#92687 = CARTESIAN_POINT ( 'NONE',  ( 172.2853610648057838, 258.8912576570302235, 14.85002519649902908 ) ) ;
#92688 = ORIENTED_EDGE ( 'NONE', *, *, #21816, .F. ) ;
#92689 = FACE_OUTER_BOUND ( 'NONE', #19475, .T. ) ;
#92691 = CARTESIAN_POINT ( 'NONE',  ( 67.97241529915037006, 65.50463755924691611, -10.32544819515218038 ) ) ;
#92690 = CARTESIAN_POINT ( 'NONE',  ( 67.64135108386106765, 65.79995805064302772, 10.56434706573462634 ) ) ;
#92692 = CARTESIAN_POINT ( 'NONE',  ( 207.5920568422024814, 271.0870056320159165, -1.586464549033245186 ) ) ;
#92693 = CARTESIAN_POINT ( 'NONE',  ( 163.9587364689194260, 246.6621334214722481, 5.816126667419880825 ) ) ;
#92694 = CARTESIAN_POINT ( 'NONE',  ( 188.3275099133877006, 294.7511660258297184, -11.02676022468676287 ) ) ;
#92695 = CARTESIAN_POINT ( 'NONE',  ( 205.0716081116550527, 275.4525508911965517, -12.57761053684872188 ) ) ;
#92696 = CARTESIAN_POINT ( 'NONE',  ( 140.7695555451228984, 242.8923013555409796, 4.594050593750050204 ) ) ;
#92697 = CARTESIAN_POINT ( 'NONE',  ( 160.1046160203818545, 254.1427746626272324, -15.31471876624168793 ) ) ;
#92698 = VECTOR ( 'NONE', #70117, 1000.000000000000000 ) ;
#92699 = CARTESIAN_POINT ( 'NONE',  ( 180.5113990821174355, 259.4917306361832061, 9.538867622362561249 ) ) ;
#92700 = CARTESIAN_POINT ( 'NONE',  ( 72.38035161819672680, 212.5958772461660544, -9.188101187500095079 ) ) ;
#92701 = VERTEX_POINT ( 'NONE', #37603 ) ;
#92702 = CARTESIAN_POINT ( 'NONE',  ( 150.6533415055477008, 269.7077535128032082, 14.84621632544246062 ) ) ;
#92703 = CARTESIAN_POINT ( 'NONE',  ( -72.30469571560091424, 48.86078274006646183, 10.00000000000000000 ) ) ;
#92704 = ORIENTED_EDGE ( 'NONE', *, *, #67685, .F. ) ;
#92705 = CARTESIAN_POINT ( 'NONE',  ( 157.3026460594630294, 258.1908201904226985, -16.97013930368657242 ) ) ;
#92706 = ORIENTED_EDGE ( 'NONE', *, *, #40455, .F. ) ;
#92707 = ORIENTED_EDGE ( 'NONE', *, *, #21595, .T. ) ;
#92708 = CARTESIAN_POINT ( 'NONE',  ( 66.69662207783855479, 67.50385436546183371, 6.505031878347596219 ) ) ;
#92709 = CARTESIAN_POINT ( 'NONE',  ( 194.5843950310221828, 284.9301011135724480, 17.17984868612067118 ) ) ;
#92710 = CARTESIAN_POINT ( 'NONE',  ( 147.2229325088103735, 275.6493961858936927, -0.4918294119671829390 ) ) ;
#92711 = DIRECTION ( 'NONE',  ( -0.5169068966820336009, 0.8560416229147678191, 0.000000000000000000 ) ) ;
#92712 = CARTESIAN_POINT ( 'NONE',  ( 193.7118145980225279, 295.1282904202991517, 14.61271143546694162 ) ) ;
#92713 = CARTESIAN_POINT ( 'NONE',  ( 72.10474246843376989, 68.41231093896740845, 9.878068674442724628 ) ) ;
#92714 = CARTESIAN_POINT ( 'NONE',  ( 84.04489159724214176, 210.1423013555409796, -4.594050593750043987 ) ) ;
#92715 = ORIENTED_EDGE ( 'NONE', *, *, #17964, .F. ) ;
#92716 = ORIENTED_EDGE ( 'NONE', *, *, #42846, .T. ) ;
#92717 = CARTESIAN_POINT ( 'NONE',  ( 15.84452179826556417, 32.08080186712592763, -3.090169943749475845 ) ) ;
#92718 = CARTESIAN_POINT ( 'NONE',  ( 161.4285303944317036, 251.0445788961045537, -12.80520346941578502 ) ) ;
#92719 = VERTEX_POINT ( 'NONE', #14324 ) ;
#92720 = EDGE_CURVE ( 'NONE', #21922, #48026, #45211, .T. ) ;
#92721 = CARTESIAN_POINT ( 'NONE',  ( 18.12000580879176326, 26.16454794089041513, -10.00000000000000355 ) ) ;
#92722 = B_SPLINE_CURVE_WITH_KNOTS ( 'NONE', 3,
 ( #76215, #74229, #30090, #59975 ),
 .UNSPECIFIED., .F., .F.,
 ( 4, 4 ),
 ( 2.823925224926892107E-17, 0.003590681989198405560 ),
 .UNSPECIFIED. ) ;
#92723 = CARTESIAN_POINT ( 'NONE',  ( 183.6537928361365175, 275.7188707068767144, 17.33434013053200928 ) ) ;
#92724 = CARTESIAN_POINT ( 'NONE',  ( -30.99490618150352006, 93.26309149566453982, 44.14155221573258103 ) ) ;
#92725 = CARTESIAN_POINT ( 'NONE',  ( 207.0624025450594843, 270.0043937851150417, -2.644299678167422840 ) ) ;
#92726 = CARTESIAN_POINT ( 'NONE',  ( 162.7006039569504594, 261.3497057169571463, 17.57720365097131676 ) ) ;
#92727 = ORIENTED_EDGE ( 'NONE', *, *, #35728, .F. ) ;
#92728 = CARTESIAN_POINT ( 'NONE',  ( 191.2234062282808509, 295.9205195230730965, 11.25357184734625626 ) ) ;
#92729 = CARTESIAN_POINT ( 'NONE',  ( 42.94622797204061726, 25.76426979415093044, 3.090169943749476733 ) ) ;
#92730 = CARTESIAN_POINT ( 'NONE',  ( 201.4520623681621316, 281.7217880192456505, -17.56577389517433119 ) ) ;
#92731 = CARTESIAN_POINT ( 'NONE',  ( 72.57700935610729687, 70.89248372566723333, 7.619130926959992500 ) ) ;
#92732 = DIRECTION ( 'NONE',  ( 1.000000000000000000, 0.000000000000000000, 0.000000000000000000 ) ) ;
#92733 = ORIENTED_EDGE ( 'NONE', *, *, #29323, .T. ) ;
#92734 = CARTESIAN_POINT ( 'NONE',  ( 195.7006838637995827, 265.4149546518947318, 4.607653087064138120 ) ) ;
#92735 = CARTESIAN_POINT ( 'NONE',  ( 181.6234035976268615, 291.8979964657406754, 10.50546202400086671 ) ) ;
#92736 = FACE_OUTER_BOUND ( 'NONE', #30489, .T. ) ;
#92737 = CARTESIAN_POINT ( 'NONE',  ( 188.0529924718924519, 265.9906442623397993, -13.09709986203515797 ) ) ;
#92738 = CARTESIAN_POINT ( 'NONE',  ( 83.61138909378800577, 52.00041238365411544, 15.00249647689079424 ) ) ;
#92739 = DIRECTION ( 'NONE',  ( -0.8660254037844387076, -0.4999999999999998890, -0.000000000000000000 ) ) ;
#92740 = ORIENTED_EDGE ( 'NONE', *, *, #3657, .T. ) ;
#92741 = EDGE_CURVE ( 'NONE', #40803, #90112, #1640, .T. ) ;
#92742 = CARTESIAN_POINT ( 'NONE',  ( 162.7644741734472120, 248.7306563947940958, 9.865755277559742353 ) ) ;
#92743 = DIRECTION ( 'NONE',  ( -0.6544109481086124447, -0.7561390817803210762, 0.000000000000000000 ) ) ;
#92745 = CARTESIAN_POINT ( 'NONE',  ( 73.66703090666727860, 55.44584689847431491, 16.58622807595889270 ) ) ;
#92744 = CARTESIAN_POINT ( 'NONE',  ( 194.4263876777154394, 293.8906135405502482, 15.23185943445137802 ) ) ;
#92746 = AXIS2_PLACEMENT_3D ( 'NONE', #8766, #10776, #54857 ) ;
#92747 = ADVANCED_FACE ( 'NONE', ( #31501 ), #15806, .F. ) ;
#92748 = CARTESIAN_POINT ( 'NONE',  ( 24.60437102317565206, 29.90829794293881960, 10.00000000000000355 ) ) ;
#92749 = CARTESIAN_POINT ( 'NONE',  ( 48.91560817564824504, 80.00000000000000000, -54.99999999999999289 ) ) ;
#92750 = CARTESIAN_POINT ( 'NONE',  ( 87.35668359673078953, 44.84080960044052944, -6.701380392922970053 ) ) ;
#92751 = CARTESIAN_POINT ( 'NONE',  ( 15.54467260552930341, 34.00295985972733348, -10.00000000000000000 ) ) ;
#92752 = CARTESIAN_POINT ( 'NONE',  ( 190.3922147189167902, 261.8887683268970932, 2.888942485245276526 ) ) ;
#92753 = ADVANCED_FACE ( 'NONE', ( #10227 ), #3072, .F. ) ;
#92754 = CARTESIAN_POINT ( 'NONE',  ( -12.00317221093202136, 170.0024278399160949, 9.188101187500095079 ) ) ;
#92755 = CARTESIAN_POINT ( 'NONE',  ( 80.97745796857455503, 210.8927522451417929, -10.00000000000009237 ) ) ;
#92756 = EDGE_LOOP ( 'NONE', ( #81406, #39119, #62039, #22529 ) ) ;
#92758 = CARTESIAN_POINT ( 'NONE',  ( 66.74743652013738426, 67.50578830241221340, -6.557104418870829399 ) ) ;
#92757 = VECTOR ( 'NONE', #38158, 1000.000000000000000 ) ;
#92759 = CARTESIAN_POINT ( 'NONE',  ( 73.05894514279327723, 70.71455386244217323, -7.616028886072077064 ) ) ;
#92760 = CARTESIAN_POINT ( 'NONE',  ( 163.2669474939272902, 273.3144560705613912, 16.33214292347920349 ) ) ;
#92761 = CARTESIAN_POINT ( 'NONE',  ( 26.12944271915780448, 176.7048013555409796, 4.594050593750051981 ) ) ;
#92762 = CARTESIAN_POINT ( 'NONE',  ( -19.65312891409030271, 93.06504152958497400, -25.00000000000000000 ) ) ;
#92763 = CARTESIAN_POINT ( 'NONE',  ( 35.77580382318486585, 22.78380873178790011, -6.180339887498949025 ) ) ;
#92764 = CARTESIAN_POINT ( 'NONE',  ( 83.57802576903957004, 41.91920785109143566, -3.213770064112233982 ) ) ;
#92765 = CARTESIAN_POINT ( 'NONE',  ( 157.8043799545718286, 257.3217915922150496, -17.97575562758749257 ) ) ;
#92766 = DIRECTION ( 'NONE',  ( 0.4996954135095463823, -0.8654978445076774163, -0.03489949670249753444 ) ) ;
#92767 = B_SPLINE_SURFACE_WITH_KNOTS ( 'NONE', 3, 1, ( 
 ( #32173, #70674 ),
 ( #62556, #54970 ),
 ( #85428, #39745 ),
 ( #31166, #48388 ),
 ( #24572, #8877 ),
 ( #63077, #1289 ),
 ( #24076, #85948 ),
 ( #15976, #78294 ),
 ( #54451, #78796 ),
 ( #94021, #55457 ),
 ( #16476, #8386 ),
 ( #23064, #32677 ),
 ( #39253, #47371 ),
 ( #9900, #47858 ),
 ( #86442, #55950 ),
 ( #15459, #9383 ),
 ( #62055, #773 ),
 ( #16969, #46877 ),
 ( #69673, #279 ),
 ( #77802, #2301 ),
 ( #40261, #71709 ),
 ( #71201, #70164 ),
 ( #86946, #93006 ),
 ( #53959, #17479 ),
 ( #79332, #1794 ),
 ( #63576, #84916 ),
 ( #94520, #61568 ),
 ( #92516, #38769 ),
 ( #46357, #77282 ),
 ( #7892, #81324 ),
 ( #87465, #34672 ),
 ( #73687, #65574 ),
 ( #74203, #81817 ),
 ( #56965, #72717 ) ),
 .UNSPECIFIED., .T., .F., .F.,
 ( 4, 2, 2, 2, 2, 2, 2, 2, 2, 2, 2, 2, 2, 2, 2, 2, 4 ),
 ( 2, 2 ),
 ( 0.000000000000000000, 0.06250000000000000000, 0.1250000000000000000, 0.1875000000000000000, 0.2500000000000000000, 0.3125000000000000000, 0.3750000000000000000, 0.4375000000000000000, 0.5000000000000000000, 0.5625000000000000000, 0.6250000000000000000, 0.6875000000000000000, 0.7500000000000000000, 0.8125000000000000000, 0.8750000000000000000, 0.9375000000000000000, 1.000000000000000000 ),
 ( 0.000000000000000000, 1.000000000000000000 ),
 .UNSPECIFIED. ) ;
#92768 = CARTESIAN_POINT ( 'NONE',  ( 82.86808232639344851, 43.79884615191943453, 9.160507364924834306 ) ) ;
#92769 = CARTESIAN_POINT ( 'NONE',  ( 190.4498225699937564, 261.8013334372093937, -0.7578904268681307954 ) ) ;
#92770 = CARTESIAN_POINT ( 'NONE',  ( 182.8250716288524131, 295.5606410807013162, 1.016483728176388324 ) ) ;
#92771 = CARTESIAN_POINT ( 'NONE',  ( 66.85041857288875633, 222.7365022471903160, 2.944929066748280225E-16 ) ) ;
#92772 = CARTESIAN_POINT ( 'NONE',  ( 82.09598787739267323, 41.22586304043770866, 5.427194921701099517 ) ) ;
#92773 = EDGE_CURVE ( 'NONE', #86172, #23023, #67702, .T. ) ;
#92774 = CARTESIAN_POINT ( 'NONE',  ( 203.4957782983326524, 270.1299432202798698, 6.025416085054049908 ) ) ;
#92775 = CARTESIAN_POINT ( 'NONE',  ( 40.17520546284541894, 187.8768266524160140, 9.188101187500098632 ) ) ;
#92776 = CARTESIAN_POINT ( 'NONE',  ( 167.1385956060480282, 251.2337521017574602, -11.14139130086932639 ) ) ;
#92777 = CARTESIAN_POINT ( 'NONE',  ( 33.91574581199579086, 27.78052372038643369, -10.00000000000000355 ) ) ;
#92778 = CARTESIAN_POINT ( 'NONE',  ( 65.02584505343169496, 219.8967562850346837, -4.648177544792955347E-16 ) ) ;
#92779 = CARTESIAN_POINT ( 'NONE',  ( 85.68485941944550177, 48.66523437743575187, 11.91861461389294163 ) ) ;
#92780 = CARTESIAN_POINT ( 'NONE',  ( 164.2723164851102808, 246.1189969011916503, -1.993789335506892302 ) ) ;
#92781 = DIRECTION ( 'NONE',  ( -0.9532659690011937581, 0.2314883312386630254, -0.1941575258509295188 ) ) ;
#92782 = CARTESIAN_POINT ( 'NONE',  ( 161.8432519094067175, 279.7467170949879574, -9.831637663153189877 ) ) ;
#92783 = CARTESIAN_POINT ( 'NONE',  ( 158.7942145198741741, 261.8960026634072733, 17.81789268137834625 ) ) ;
#92784 = CARTESIAN_POINT ( 'NONE',  ( 21.37261828447143586, 20.84335787977763133, 9.188101187500006262 ) ) ;
#92785 = CARTESIAN_POINT ( 'NONE',  ( 189.9462859318020946, 301.6503773875500087, -1.164147598593831656 ) ) ;
#92786 = CARTESIAN_POINT ( 'NONE',  ( 72.04273812837081437, 59.28583566120335036, 15.34548535902080246 ) ) ;
#92787 = CARTESIAN_POINT ( 'NONE',  ( 188.8678792399009581, 270.1696821249879576, -14.21866136085443877 ) ) ;
#92788 = ORIENTED_EDGE ( 'NONE', *, *, #92002, .T. ) ;
#92789 = CARTESIAN_POINT ( 'NONE',  ( 185.5458178329047882, 290.8126708647759529, 12.98563741746813349 ) ) ;
#92790 = CARTESIAN_POINT ( 'NONE',  ( 178.6782777294722848, 260.6412425082613709, 13.57969907341511551 ) ) ;
#92791 = LINE ( 'NONE', #47149, #50099 ) ;
#92792 = CARTESIAN_POINT ( 'NONE',  ( 81.89600004460587002, 42.20886894945997625, 7.642739303376051119 ) ) ;
#92793 = DIRECTION ( 'NONE',  ( -0.5280678506503699854, -0.8492021815265776707, 0.000000000000000000 ) ) ;
#92794 = ORIENTED_EDGE ( 'NONE', *, *, #13650, .T. ) ;
#92795 = DIRECTION ( 'NONE',  ( 5.984665299743594308E-16, 0.000000000000000000, 1.000000000000000000 ) ) ;
#92796 = CARTESIAN_POINT ( 'NONE',  ( 72.40857565946932084, 71.84120774512069829, -5.522868224832428119 ) ) ;
#92797 = CARTESIAN_POINT ( 'NONE',  ( 73.09176899391452764, 57.17258086466325295, 16.39964270276630742 ) ) ;
#92798 = CARTESIAN_POINT ( 'NONE',  ( 181.1390130125879807, 257.6774870082531379, -7.540388427927620540 ) ) ;
#92799 = VERTEX_POINT ( 'NONE', #3633 ) ;
#92800 =( BOUNDED_CURVE ( )  B_SPLINE_CURVE ( 2, ( #83884, #99549, #22538, #85380, #62007, #54404, #25023, #47812, #9337 ),
 .UNSPECIFIED., .F., .F. ) 
 B_SPLINE_CURVE_WITH_KNOTS ( ( 3, 2, 2, 2, 3 ),
 ( 0.4395161290322580627, 0.4408602150537634379, 0.4435483870967741882, 0.4462365591397849385, 0.4475806451612903136 ),
 .UNSPECIFIED. ) 
 CURVE ( )  GEOMETRIC_REPRESENTATION_ITEM ( )  RATIONAL_B_SPLINE_CURVE ( ( 0.9330127018922194093, 0.9330127018922194093, 1.000000000000000000, 0.8660254037844387076, 1.000000000000000000, 0.8660254037844387076, 1.000000000000000000, 0.9330127018922194093, 0.9330127018922194093 ) ) 
 REPRESENTATION_ITEM ( '' )  );
#92801 = ORIENTED_EDGE ( 'NONE', *, *, #75470, .F. ) ;
#92803 = CARTESIAN_POINT ( 'NONE',  ( 84.69548858147219050, 42.71338583940531208, -3.895673258569514630 ) ) ;
#92802 = CARTESIAN_POINT ( 'NONE',  ( -32.04500338604974985, 25.44370296803430520, 10.00000000000000000 ) ) ;
#92804 = ORIENTED_EDGE ( 'NONE', *, *, #18984, .T. ) ;
#92805 = CARTESIAN_POINT ( 'NONE',  ( 151.0099717111976076, 269.0900518771037468, 15.84752309685681659 ) ) ;
#92806 = PLANE ( 'NONE',  #85276 ) ;
#92807 = CYLINDRICAL_SURFACE ( 'NONE', #12729, 16.60714546451156792 ) ;
#92808 = CARTESIAN_POINT ( 'NONE',  ( 76.85865272105424140, 63.69649487134743282, 15.33129195839047298 ) ) ;
#92809 = ORIENTED_EDGE ( 'NONE', *, *, #18319, .F. ) ;
#92810 = CARTESIAN_POINT ( 'NONE',  ( 189.8238368927809745, 301.8624653444729802, -0.3620111495846872751 ) ) ;
#92811 = EDGE_CURVE ( 'NONE', #28762, #97214, #64119, .T. ) ;
#92812 = VECTOR ( 'NONE', #34802, 1000.000000000000227 ) ;
#92813 = ORIENTED_EDGE ( 'NONE', *, *, #71582, .F. ) ;
#92814 = FACE_OUTER_BOUND ( 'NONE', #65220, .T. ) ;
#92815 = LINE ( 'NONE', #16279, #88299 ) ;
#92816 = ORIENTED_EDGE ( 'NONE', *, *, #47497, .T. ) ;
#92817 = CARTESIAN_POINT ( 'NONE',  ( 31.61033844661487180, 20.11110640527293825, -2.839279412974138328 ) ) ;
#92818 = CARTESIAN_POINT ( 'NONE',  ( -16.99542894172669705, 24.36904009834037765, -10.00000000000000000 ) ) ;
#92819 = LINE ( 'NONE', #46162, #72535 ) ;
#92820 = EDGE_LOOP ( 'NONE', ( #68754, #41438, #63374, #33604 ) ) ;
#92821 = CARTESIAN_POINT ( 'NONE',  ( -16.31071837694740623, 74.13583127143270701, 13.48478556928571948 ) ) ;
#92822 =( BOUNDED_CURVE ( )  B_SPLINE_CURVE ( 2, ( #46449, #84023, #32264, #70259, #45947, #23650, #47462, #867, #37853 ),
 .UNSPECIFIED., .F., .T. ) 
 B_SPLINE_CURVE_WITH_KNOTS ( ( 3, 2, 2, 2, 3 ),
 ( 0.1411290322580645296, 0.1424731182795699047, 0.1451612903225806550, 0.1478494623655914053, 0.1491935483870967805 ),
 .UNSPECIFIED. ) 
 CURVE ( )  GEOMETRIC_REPRESENTATION_ITEM ( )  RATIONAL_B_SPLINE_CURVE ( ( 0.9330127018922194093, 0.9330127018922200755, 1.000000000000000000, 0.8660254037844387076, 1.000000000000000000, 0.8660254037844387076, 1.000000000000000000, 0.9330127018922194093, 0.9330127018922194093 ) ) 
 REPRESENTATION_ITEM ( '' )  );
#92823 = CARTESIAN_POINT ( 'NONE',  ( 190.7851866479434761, 300.1973587246873194, 7.931162401707728016 ) ) ;
#92824 = CARTESIAN_POINT ( 'NONE',  ( 66.15274061880275269, 50.14441083166266822, 0.000000000000000000 ) ) ;
#92825 = LINE ( 'NONE', #23378, #38231 ) ;
#92826 = ORIENTED_EDGE ( 'NONE', *, *, #68263, .T. ) ;
#92827 = ORIENTED_EDGE ( 'NONE', *, *, #95017, .T. ) ;
#92828 = CARTESIAN_POINT ( 'NONE',  ( -22.42236680055709641, 157.8615022471902591, 0.000000000000000000 ) ) ;
#92830 = VECTOR ( 'NONE', #14967, 1000.000000000000000 ) ;
#92829 = CARTESIAN_POINT ( 'NONE',  ( 82.36003205642018088, 42.70002867508654276, -6.979109086437436105 ) ) ;
#92831 = CARTESIAN_POINT ( 'NONE',  ( 190.1696443193688708, 301.2635093119881162, -4.804312979389741223 ) ) ;
#92832 = CARTESIAN_POINT ( 'NONE',  ( 190.1158090214649405, 301.3567547831981983, -1.340987185199551845 ) ) ;
#92833 = ORIENTED_EDGE ( 'NONE', *, *, #71015, .F. ) ;
#92834 = CARTESIAN_POINT ( 'NONE',  ( 190.8187029736043883, 300.1393067457597681, 3.941064102378585954 ) ) ;
#92835 = CARTESIAN_POINT ( 'NONE',  ( 171.6872963709983821, 276.1252452772627635, -16.94555118095737711 ) ) ;
#92836 = DIRECTION ( 'NONE',  ( 0.000000000000000000, 0.000000000000000000, 1.000000000000000000 ) ) ;
#92837 = FACE_OUTER_BOUND ( 'NONE', #71292, .T. ) ;
#92838 = CARTESIAN_POINT ( 'NONE',  ( 148.9230895364621574, 272.7046378331555161, 12.20434325797056019 ) ) ;
#92839 = CARTESIAN_POINT ( 'NONE',  ( 20.94669640352213236, 37.57748520232517109, -10.00000000000000000 ) ) ;
#92840 = CARTESIAN_POINT ( 'NONE',  ( 94.56323149399085537, 218.7365022471901739, 10.00000000000009948 ) ) ;
#92841 = CARTESIAN_POINT ( 'NONE',  ( 75.92693672788908543, 65.58256616235577496, 13.87764565375856662 ) ) ;
#92842 = CARTESIAN_POINT ( 'NONE',  ( 154.6387566766715054, 264.1588125162423353, -17.13921758461861700 ) ) ;
#92843 = CARTESIAN_POINT ( 'NONE',  ( 78.55383125624311447, 47.44943004927687014, 14.24641143436689816 ) ) ;
#92844 = CARTESIAN_POINT ( 'NONE',  ( 107.5083335113205578, 239.0024278399160949, 9.188101187500095079 ) ) ;
#92845 = ORIENTED_EDGE ( 'NONE', *, *, #24098, .F. ) ;
#92846 = CARTESIAN_POINT ( 'NONE',  ( 146.8859094598974480, 276.2331372299326517, -0.7994986043261681496 ) ) ;
#92847 = CARTESIAN_POINT ( 'NONE',  ( 70.26774927589852382, 65.27959088349479089, 11.79268299559660349 ) ) ;
#92848 = DIRECTION ( 'NONE',  ( 0.5637708215276955315, -0.8259312688075124420, 0.000000000000000000 ) ) ;
#92849 = CARTESIAN_POINT ( 'NONE',  ( 202.7602807045765019, 279.4558873931827065, -15.90558713185497020 ) ) ;
#92850 = CARTESIAN_POINT ( 'NONE',  ( 182.0697224992034648, 283.9259822107836158, -15.01725063203069865 ) ) ;
#92851 = CARTESIAN_POINT ( 'NONE',  ( 83.76909922093737748, 51.72725043056325234, -14.84865573977556075 ) ) ;
#92852 = CARTESIAN_POINT ( 'NONE',  ( 165.7172767540421319, 283.5836649089671937, -8.214104100105947381 ) ) ;
#92853 = ORIENTED_EDGE ( 'NONE', *, *, #25121, .T. ) ;
#92854 = CARTESIAN_POINT ( 'NONE',  ( 208.3764315856425640, 269.7284287242038658, -1.833640725398759441 ) ) ;
#92855 = CARTESIAN_POINT ( 'NONE',  ( 72.45582997685151838, 71.59006409230265433, 5.171701996141663926 ) ) ;
#92856 = CARTESIAN_POINT ( 'NONE',  ( 49.72837464868604940, 199.5177522451418781, -10.00000000000009592 ) ) ;
#92857 = CARTESIAN_POINT ( 'NONE',  ( 131.1078728602114722, 240.3768266524160424, 9.188101187500096856 ) ) ;
#92858 = CARTESIAN_POINT ( 'NONE',  ( 150.7133245577828689, 269.6038598187387834, -14.58664962216439598 ) ) ;
#92859 = LINE ( 'NONE', #44712, #56146 ) ;
#92860 = CARTESIAN_POINT ( 'NONE',  ( 196.4982648257524147, 290.3020170531091821, 16.69353242256149628 ) ) ;
#92861 = LINE ( 'NONE', #33026, #77354 ) ;
#92862 = CARTESIAN_POINT ( 'NONE',  ( 46.91405240998433612, 188.7048013555409796, 4.594050593750051981 ) ) ;
#92863 = CARTESIAN_POINT ( 'NONE',  ( 85.70408377067469985, 48.42330189018957043, -11.73456542461740604 ) ) ;
#92864 = ORIENTED_EDGE ( 'NONE', *, *, #41701, .T. ) ;
#92865 = CARTESIAN_POINT ( 'NONE',  ( 71.45374252289430217, 64.76739115956998205, 12.70080691706103515 ) ) ;
#92866 = CARTESIAN_POINT ( 'NONE',  ( 88.07442723472371426, 44.71957171711925838, -4.374393210843437352 ) ) ;
#92867 = ADVANCED_FACE ( 'NONE', ( #50211 ), #4108, .T. ) ;
#92868 = CARTESIAN_POINT ( 'NONE',  ( -6.542761065016642341, 25.57183462804972507, 10.00000000000000000 ) ) ;
#92869 = CARTESIAN_POINT ( 'NONE',  ( 190.1693911629507738, 301.2639477917662703, -5.112716700269980485 ) ) ;
#92870 = CARTESIAN_POINT ( 'NONE',  ( 82.08809084460519045, 41.85377707259943492, -5.545080802233028905 ) ) ;
#92871 = CARTESIAN_POINT ( 'NONE',  ( 10.49025449741314375, 29.55466486950698624, -1.111400068045478839E-16 ) ) ;
#92872 = EDGE_CURVE ( 'NONE', #4561, #54647, #57801, .T. ) ;
#92873 = CARTESIAN_POINT ( 'NONE',  ( 178.5272579798314894, 261.1979847487124289, 12.22333219613103239 ) ) ;
#92874 = CARTESIAN_POINT ( 'NONE',  ( 106.8860512984590088, 232.5177522451418781, -10.00000000000009592 ) ) ;
#92875 = EDGE_CURVE ( 'NONE', #67111, #98668, #89474, .T. ) ;
#92876 = CARTESIAN_POINT ( 'NONE',  ( 15.42233441037273423, 31.83705186507753382, 3.090169943749475401 ) ) ;
#92877 = ORIENTED_EDGE ( 'NONE', *, *, #70534, .T. ) ;
#92878 = EDGE_CURVE ( 'NONE', #19564, #38181, #35002, .T. ) ;
#92879 = CARTESIAN_POINT ( 'NONE',  ( 189.9052851100924215, 301.7213928939034986, -1.077181946533001256 ) ) ;
#92880 = DIRECTION ( 'NONE',  ( 0.4999999999999992784, -0.8660254037844390407, 0.000000000000000000 ) ) ;
#92881 = CARTESIAN_POINT ( 'NONE',  ( 20.74358691754956396, 182.7833772461660544, -9.188101187500095079 ) ) ;
#92882 = CARTESIAN_POINT ( 'NONE',  ( 16.70795526530605457, 14.81029122506293483, 8.090169943749479842 ) ) ;
#92883 = CARTESIAN_POINT ( 'NONE',  ( 192.9465561454275928, 272.3177685425281993, 14.20360320959197686 ) ) ;
#92884 = CARTESIAN_POINT ( 'NONE',  ( 160.3733185927383715, 282.5102941377067509, 6.606729549618552078 ) ) ;
#92885 = CARTESIAN_POINT ( 'NONE',  ( 73.06502562637749065, 69.62150218382535627, 9.203196011093488949 ) ) ;
#92887 = CARTESIAN_POINT ( 'NONE',  ( 69.15955932604958889, 219.9244531367911293, -4.594050593750046652 ) ) ;
#92886 = CARTESIAN_POINT ( 'NONE',  ( 197.8951961584970149, 277.1396171073823211, -15.32953000722216430 ) ) ;
#92888 = CARTESIAN_POINT ( 'NONE',  ( 208.3152833949211526, 269.8343404973242059, 2.763633873278860342 ) ) ;
#92889 = CARTESIAN_POINT ( 'NONE',  ( 72.61312054461893695, 57.22205865948716763, 15.86921491991221522 ) ) ;
#92890 = DIRECTION ( 'NONE',  ( 0.2588190451025306205, 0.9659258262890656477, 0.000000000000000000 ) ) ;
#92891 = CARTESIAN_POINT ( 'NONE',  ( 66.76842575320728201, 68.41059621743521291, -4.427724692764615888 ) ) ;
#92892 = ORIENTED_EDGE ( 'NONE', *, *, #38725, .F. ) ;
#92893 = COLOUR_RGB ( '',0.7921568627450980005, 0.8196078431372548767, 0.9333333333333333481 ) ;
#92894 = CARTESIAN_POINT ( 'NONE',  ( 25.28119919123569304, 198.7365022471903444, 2.944929066748280225E-16 ) ) ;
#92895 = CARTESIAN_POINT ( 'NONE',  ( 207.6471633721571379, 270.9915583223058206, 2.196965492132801678 ) ) ;
#92896 = CARTESIAN_POINT ( 'NONE',  ( -15.41332078621576329, 174.1589784336661637, -6.496448406907675876E-16 ) ) ;
#92897 = CARTESIAN_POINT ( 'NONE',  ( 30.51038259252555207, 29.56628583063842441, 9.188101187500006262 ) ) ;
#92898 = CARTESIAN_POINT ( 'NONE',  ( 167.5778442440516471, 262.4579367844059448, -16.54578138360918160 ) ) ;
#92899 = CARTESIAN_POINT ( 'NONE',  ( 186.0023642507784416, 260.7041546637453848, 6.337017704808292962 ) ) ;
#92900 = CARTESIAN_POINT ( 'NONE',  ( 206.1215120922853146, 273.6340638536760821, 10.12238414215620885 ) ) ;
#92901 = AXIS2_PLACEMENT_3D ( 'NONE', #47410, #87502, #78336 ) ;
#92902 = CARTESIAN_POINT ( 'NONE',  ( 48.61286661847091040, 84.94359857078811160, 10.00000000000000000 ) ) ;
#92903 = CARTESIAN_POINT ( 'NONE',  ( 66.43068645214782464, 68.73212257389783986, 2.345923867857303335 ) ) ;
#92904 = VERTEX_POINT ( 'NONE', #57307 ) ;
#92905 = DIRECTION ( 'NONE',  ( -0.6758705274779386318, -0.2489746672676196315, -0.6936934806855771241 ) ) ;
#92906 = CARTESIAN_POINT ( 'NONE',  ( 164.0943423276914643, 246.4272571842752484, 8.509643519936494371 ) ) ;
#92907 = CARTESIAN_POINT ( 'NONE',  ( 178.5527154611763763, 285.5147197797991794, 13.02099474314520400 ) ) ;
#92908 = PLANE ( 'NONE',  #80749 ) ;
#92909 = CARTESIAN_POINT ( 'NONE',  ( 18.45335787429653251, 11.44966523072493558, -2.296566073217252530E-15 ) ) ;
#92910 = VERTEX_POINT ( 'NONE', #72546 ) ;
#92911 = DIRECTION ( 'NONE',  ( -0.8660254037844387076, -0.4999999999999998890, -0.000000000000000000 ) ) ;
#92912 = CARTESIAN_POINT ( 'NONE',  ( 157.1965120183049578, 258.3746497421212780, -18.06591467563559306 ) ) ;
#92913 = CARTESIAN_POINT ( 'NONE',  ( 23.90938336746022586, 36.73705186507755371, -3.090169943749475845 ) ) ;
#92914 = CARTESIAN_POINT ( 'NONE',  ( -13.85019419761653836, 104.3865186021088078, 43.91809099165308083 ) ) ;
#92915 = CARTESIAN_POINT ( 'NONE',  ( 41.08847453908118297, 182.9824982072973967, 3.021315404115420679E-15 ) ) ;
#92916 = CARTESIAN_POINT ( 'NONE',  ( 163.3939361803663246, 247.6403962173759226, -10.78041711314006790 ) ) ;
#92917 = CARTESIAN_POINT ( 'NONE',  ( 200.8147387322574957, 282.8256649374973790, -18.02438097732020239 ) ) ;
#92918 = ORIENTED_EDGE ( 'NONE', *, *, #31217, .F. ) ;
#92919 = ORIENTED_EDGE ( 'NONE', *, *, #47722, .T. ) ;
#92920 = CARTESIAN_POINT ( 'NONE',  ( 190.7147070850360819, 281.1586976679043346, 16.70495451513169272 ) ) ;
#92921 = LINE ( 'NONE', #46795, #46607 ) ;
#92922 = ORIENTED_EDGE ( 'NONE', *, *, #18760, .F. ) ;
#92923 = CARTESIAN_POINT ( 'NONE',  ( 71.17064988840769502, 70.28013413260883624, 7.276424097237452315 ) ) ;
#92924 = CARTESIAN_POINT ( 'NONE',  ( 87.14288108606291416, 44.98988116358240319, -6.378897604470720850 ) ) ;
#92925 = ORIENTED_EDGE ( 'NONE', *, *, #98793, .T. ) ;
#92926 = DIRECTION ( 'NONE',  ( -0.000000000000000000, -0.000000000000000000, -1.000000000000000000 ) ) ;
#92927 = CARTESIAN_POINT ( 'NONE',  ( 186.2798660816079632, 264.0713031700501006, -12.82791401631097550 ) ) ;
#92928 = CARTESIAN_POINT ( 'NONE',  ( 17.13867093926436169, 10.86426979415088567, -3.090169943749474069 ) ) ;
#92929 = CARTESIAN_POINT ( 'NONE',  ( 86.13879346367242817, 46.95025718893441535, -10.63009676298478823 ) ) ;
#92930 = EDGE_CURVE ( 'NONE', #93753, #89224, #95382, .T. ) ;
#92931 = CARTESIAN_POINT ( 'NONE',  ( 69.91735932814472676, 62.82170394719442896, 13.89425379104851999 ) ) ;
#92932 = ORIENTED_EDGE ( 'NONE', *, *, #22663, .T. ) ;
#92933 = CARTESIAN_POINT ( 'NONE',  ( 200.1385401540174769, 283.9968752310148830, 17.30012534137638625 ) ) ;
#92934 = CARTESIAN_POINT ( 'NONE',  ( 49.10122569834316408, 93.29622288527660601, -10.00000000000000000 ) ) ;
#92935 = CARTESIAN_POINT ( 'NONE',  ( 172.6505904036989136, 280.8448313155626579, -15.39888677054324440 ) ) ;
#92936 = ORIENTED_EDGE ( 'NONE', *, *, #20140, .T. ) ;
#92937 = ORIENTED_EDGE ( 'NONE', *, *, #40732, .F. ) ;
#92938 = ORIENTED_EDGE ( 'NONE', *, *, #36360, .T. ) ;
#92939 = CARTESIAN_POINT ( 'NONE',  ( 160.0767744118185476, 268.8186339879788989, -17.09306701113738569 ) ) ;
#92940 = ORIENTED_EDGE ( 'NONE', *, *, #92487, .T. ) ;
#92941 = CARTESIAN_POINT ( 'NONE',  ( 68.42993948008529514, 68.72088526677468678, 6.145480275798111514 ) ) ;
#92942 = ORIENTED_EDGE ( 'NONE', *, *, #78554, .F. ) ;
#92943 = CARTESIAN_POINT ( 'NONE',  ( 163.9354095869165633, 246.7025367662834014, -7.289870401565430313 ) ) ;
#92944 = CARTESIAN_POINT ( 'NONE',  ( 83.59982691654131770, 50.63482651926307909, 13.94564167549828504 ) ) ;
#92946 = EDGE_CURVE ( 'NONE', #58975, #18309, #91979, .T. ) ;
#92945 = CARTESIAN_POINT ( 'NONE',  ( 167.4568069247567905, 281.4715426663276503, 11.40307132674027457 ) ) ;
#92947 = CARTESIAN_POINT ( 'NONE',  ( 148.3629184514745987, 273.6748826132846375, -8.219814532462343948 ) ) ;
#92948 = CARTESIAN_POINT ( 'NONE',  ( 82.75828967192548191, 53.74568045750391576, -15.77735475420663924 ) ) ;
#92949 = CARTESIAN_POINT ( 'NONE',  ( -68.29659580619643577, 42.72804590294295224, 10.00000000000000000 ) ) ;
#92950 = ORIENTED_EDGE ( 'NONE', *, *, #95434, .F. ) ;
#92951 = CARTESIAN_POINT ( 'NONE',  ( -10.80656490723494123, 24.88181024604956804, -10.00000000000000000 ) ) ;
#92952 = CARTESIAN_POINT ( 'NONE',  ( 19.48598279363274344, 13.11110640527291693, -2.839279412974138328 ) ) ;
#92953 = DIRECTION ( 'NONE',  ( -0.8660254037844387076, -0.4999999999999998890, -0.000000000000000000 ) ) ;
#92954 = CARTESIAN_POINT ( 'NONE',  ( 80.73437012277888414, 57.38180594535329249, 16.57560423861647081 ) ) ;
#92956 = ORIENTED_EDGE ( 'NONE', *, *, #78877, .F. ) ;
#92955 = CARTESIAN_POINT ( 'NONE',  ( 206.8495915765685140, 270.6470149864544510, 5.005496931752787759 ) ) ;
#92957 = CARTESIAN_POINT ( 'NONE',  ( 147.2851682955343620, 275.5416006412388583, -4.045222947525739521 ) ) ;
#92958 = CARTESIAN_POINT ( 'NONE',  ( 168.6819343819337575, 257.4928200986727234, -14.24392100367956893 ) ) ;
#92959 = CARTESIAN_POINT ( 'NONE',  ( 206.8791291248445532, 272.3218326606039454, -10.16823074922856840 ) ) ;
#92960 = CARTESIAN_POINT ( 'NONE',  ( 77.14944321224352564, 49.32060529837239926, -15.40190492294266278 ) ) ;
#92961 = B_SPLINE_CURVE_WITH_KNOTS ( 'NONE', 3,
 ( #27360, #42048, #97283, #4547, #19770, #66350, #50153, #65352, #90191, #65835, #74966, #57736, #43023, #5548, #26860, #20767, #81105, #18768, #49645, #82099, #58242, #43540, #72982, #74481 ),
 .UNSPECIFIED., .F., .F.,
 ( 4, 2, 2, 2, 2, 2, 2, 2, 2, 2, 2, 4 ),
 ( 0.000000000000000000, 0.1250000000000053568, 0.2500000000000107137, 0.3750000000000160982, 0.4375000000000109912, 0.5000000000000058842, 0.5625000000000007772, 0.6249999999999956701, 0.6874999999999905631, 0.7499999999999854561, 0.8749999999999927836, 1.000000000000000000 ),
 .UNSPECIFIED. ) ;
#92962 = CARTESIAN_POINT ( 'NONE',  ( 83.79436218315080964, 45.74912830802215780, -10.11333493852419707 ) ) ;
#92963 = AXIS2_PLACEMENT_3D ( 'NONE', #67190, #90551, #74827 ) ;
#92964 = CARTESIAN_POINT ( 'NONE',  ( 171.3137948708142062, 255.5715404926284862, 11.21645684402445831 ) ) ;
#92965 = CARTESIAN_POINT ( 'NONE',  ( 161.2178929573049402, 283.3531530028743077, 2.129142326282500886 ) ) ;
#92966 = VERTEX_POINT ( 'NONE', #49710 ) ;
#92967 = CARTESIAN_POINT ( 'NONE',  ( 194.5442727646457399, 293.6864305805324307, -14.41394159254472029 ) ) ;
#92968 = CARTESIAN_POINT ( 'NONE',  ( 74.84872400778057511, 66.80276697526575447, -13.19923776164384499 ) ) ;
#92969 = CARTESIAN_POINT ( 'NONE',  ( 162.1461328301699609, 255.8963067295628662, -16.22074050756077668 ) ) ;
#92970 = CARTESIAN_POINT ( 'NONE',  ( -4.037369169597886831, 175.1427522451419350, 10.00000000000009237 ) ) ;
#92971 = CARTESIAN_POINT ( 'NONE',  ( 89.61940949045693117, 231.7369531367911009, -4.594050593750048428 ) ) ;
#92972 = CARTESIAN_POINT ( 'NONE',  ( 82.87432691701982890, 53.54933337481561750, -15.33804591960182861 ) ) ;
#92973 = CARTESIAN_POINT ( 'NONE',  ( 15.58658660100807580, 11.12755873383624561, -6.180339887498949025 ) ) ;
#92974 = CARTESIAN_POINT ( 'NONE',  ( 163.5897630428932246, 247.3012141419924603, -7.420471801261374623 ) ) ;
#92975 = DIRECTION ( 'NONE',  ( 0.9659258262890674240, -0.2588190451025239036, 8.659560562355041327E-17 ) ) ;
#92977 = CARTESIAN_POINT ( 'NONE',  ( 75.58214075417596689, 65.23491603964201602, 14.35294216029143755 ) ) ;
#92976 = CARTESIAN_POINT ( 'NONE',  ( 10.97399815293012892, 167.9548013555409796, -4.594050593750042211 ) ) ;
#92978 = CARTESIAN_POINT ( 'NONE',  ( 161.1990332043106946, 251.4420796895884394, 14.26998817770995487 ) ) ;
#92979 = ORIENTED_EDGE ( 'NONE', *, *, #88763, .T. ) ;
#92980 = ORIENTED_EDGE ( 'NONE', *, *, #48161, .T. ) ;
#92981 = B_SPLINE_CURVE_WITH_KNOTS ( 'NONE', 3,
 ( #23029, #78262, #15425, #24041 ),
 .UNSPECIFIED., .F., .F.,
 ( 4, 4 ),
 ( 0.006441154778305856546, 0.01214362524711681476 ),
 .UNSPECIFIED. ) ;
#92982 = CARTESIAN_POINT ( 'NONE',  ( 188.9125033604726411, 260.9492661745924238, -6.201642747674654288 ) ) ;
#92983 = EDGE_CURVE ( 'NONE', #57886, #79592, #80666, .T. ) ;
#92984 = CARTESIAN_POINT ( 'NONE',  ( 105.0000000000000000, 4.999999999999999112, 54.99999999999999289 ) ) ;
#92985 = CARTESIAN_POINT ( 'NONE',  ( 205.1300674467857164, 275.3512963525735131, -12.60245643603069610 ) ) ;
#92986 = CARTESIAN_POINT ( 'NONE',  ( 201.9828021040781891, 280.8025198310436394, -16.96692439557026688 ) ) ;
#92987 = CARTESIAN_POINT ( 'NONE',  ( 185.5309115041763164, 286.5403957835872006, 16.01510129901755164 ) ) ;
#92988 = CARTESIAN_POINT ( 'NONE',  ( 74.02653709664873816, 68.32631449583556105, -11.67658431812981412 ) ) ;
#92989 = CARTESIAN_POINT ( 'NONE',  ( 29.56604717072103483, 194.0024278399160949, 9.188101187500095079 ) ) ;
#92990 = CARTESIAN_POINT ( 'NONE',  ( 125.6409139509397050, 243.3458772461660544, 9.188101187500095079 ) ) ;
#92991 = CARTESIAN_POINT ( 'NONE',  ( 182.8698629865610030, 257.6187957884557136, -2.313844758695299042 ) ) ;
#92992 = EDGE_LOOP ( 'NONE', ( #95081, #35981, #84646, #58693 ) ) ;
#92993 = CARTESIAN_POINT ( 'NONE',  ( 153.4632062653391529, 273.9939398201073004, -11.95209943642215933 ) ) ;
#92994 = EDGE_CURVE ( 'NONE', #74626, #51127, #30192, .T. ) ;
#92995 = CARTESIAN_POINT ( 'NONE',  ( -15.10528209597770299, 24.46087392797018722, -10.00000000000000000 ) ) ;
#92996 = CARTESIAN_POINT ( 'NONE',  ( 38.51867309874058520, 23.20801979619931643, -3.090169943749474069 ) ) ;
#92997 = CARTESIAN_POINT ( 'NONE',  ( 197.5443661845914107, 266.8897665035560181, 8.689862809994204795 ) ) ;
#92998 = CARTESIAN_POINT ( 'NONE',  ( 154.9910882912764123, 262.1945556895526579, 18.38052604520346023 ) ) ;
#92999 = CARTESIAN_POINT ( 'NONE',  ( 161.5757715694810770, 250.7895496999525449, -14.51803553215175135 ) ) ;
#93000 = CARTESIAN_POINT ( 'NONE',  ( 82.31162263179685112, 47.02075270482669112, 12.63320473991187676 ) ) ;
#93001 = CARTESIAN_POINT ( 'NONE',  ( 148.3025927079438304, 273.7793698660844939, -8.046026357031887954 ) ) ;
#93002 = CARTESIAN_POINT ( 'NONE',  ( 72.12483444493729223, 64.99830324756513278, 13.36562007551493281 ) ) ;
#93003 = CARTESIAN_POINT ( 'NONE',  ( 164.6664072718354532, 249.8410913454628144, -10.49978785697552119 ) ) ;
#93004 = CARTESIAN_POINT ( 'NONE',  ( 192.8633186137653865, 264.6749303248840306, 8.942253059790195024 ) ) ;
#93005 = CARTESIAN_POINT ( 'NONE',  ( 69.77287440015896891, 69.89897948854762433, 5.259387334649119339 ) ) ;
#93006 = CARTESIAN_POINT ( 'NONE',  ( 148.1634546024981205, 274.0203641339852538, 9.324875965062235039 ) ) ;
#93007 = CARTESIAN_POINT ( 'NONE',  ( 149.4596969528118393, 273.7752065243203106, 10.43958276706939614 ) ) ;
#93008 = ORIENTED_EDGE ( 'NONE', *, *, #76643, .T. ) ;
#93009 = LINE ( 'NONE', #30691, #14147 ) ;
#93010 = CARTESIAN_POINT ( 'NONE',  ( 182.9346993922109448, 268.7180793606257794, 15.07033917878656837 ) ) ;
#93011 = CARTESIAN_POINT ( 'NONE',  ( 111.1353355333153843, 222.7202760586659167, -5.415160957724236172E-17 ) ) ;
#93012 = CARTESIAN_POINT ( 'NONE',  ( 8.675723883004062387, 25.98502408145591147, -5.678558825948271327 ) ) ;
#93013 = CARTESIAN_POINT ( 'NONE',  ( 190.8623743139412454, 300.0636657654615647, 8.577953960666059530 ) ) ;
#93014 = CARTESIAN_POINT ( 'NONE',  ( 79.86306577577953192, 56.87384565298960126, -16.58767780902013911 ) ) ;
#93016 = CARTESIAN_POINT ( 'NONE',  ( 195.0461724950329767, 279.0680765902233134, 16.30667399101714921 ) ) ;
#93015 = CARTESIAN_POINT ( 'NONE',  ( 19.29290913472606661, 12.10801979619928126, 3.090169943749476733 ) ) ;
#93017 = CARTESIAN_POINT ( 'NONE',  ( 191.2176534171005926, 299.4483043079223421, -6.603228034478700437 ) ) ;
#93018 = CARTESIAN_POINT ( 'NONE',  ( 191.2557879401978198, 261.3776189723048446, -4.694998167070893125 ) ) ;
#93019 = FACE_OUTER_BOUND ( 'NONE', #5750, .T. ) ;
#93020 = PLANE ( 'NONE',  #91168 ) ;
#93021 = CARTESIAN_POINT ( 'NONE',  ( 192.4663556654298588, 297.2854885702906245, -12.98646995774174684 ) ) ;
#93022 = PLANE ( 'NONE',  #79908 ) ;
#93023 = ORIENTED_EDGE ( 'NONE', *, *, #33309, .T. ) ;
#93024 = CARTESIAN_POINT ( 'NONE',  ( 193.0322577453413260, 267.1504813846829620, 11.29149517974427042 ) ) ;
#93025 = CARTESIAN_POINT ( 'NONE',  ( 69.28997898220227114, 64.65901494164410224, -12.44462553223597823 ) ) ;
#93026 = CARTESIAN_POINT ( 'NONE',  ( 200.5156711751714909, 269.2042492623063481, 9.044317516942950164 ) ) ;
#93027 = CARTESIAN_POINT ( 'NONE',  ( 149.7072529793668707, 271.3464269086063041, -11.98883662638834657 ) ) ;
#93028 = ORIENTED_EDGE ( 'NONE', *, *, #35761, .F. ) ;
#93029 = CARTESIAN_POINT ( 'NONE',  ( 79.21012467913614330, 50.17711341405016867, 14.78417737531875886 ) ) ;
#93030 = MECHANICAL_DESIGN_GEOMETRIC_PRESENTATION_REPRESENTATION (  '', ( #99461 ), #68698 ) ;
#93031 = FACE_OUTER_BOUND ( 'NONE', #80021, .T. ) ;
#93032 = CARTESIAN_POINT ( 'NONE',  ( 77.08943580299947484, 49.61595851769167353, 15.51385818994994459 ) ) ;
#93033 = CARTESIAN_POINT ( 'NONE',  ( 74.95739461836087969, 53.28572374827752611, -16.04297136957062264 ) ) ;
#93034 = DIRECTION ( 'NONE',  ( -0.000000000000000000, -0.000000000000000000, 1.000000000000000000 ) ) ;
#93035 = ORIENTED_EDGE ( 'NONE', *, *, #88325, .F. ) ;
#93036 = CARTESIAN_POINT ( 'NONE',  ( 73.53729735990698657, 69.85633680769765874, 9.839233502311348190 ) ) ;
#93037 = CARTESIAN_POINT ( 'NONE',  ( 34.67813663163181559, 40.99752408145594273, 5.678558825948277544 ) ) ;
#93038 = VERTEX_POINT ( 'NONE', #43519 ) ;
#93039 = CARTESIAN_POINT ( 'NONE',  ( 167.5352006701565415, 249.8483303177359858, 6.949831534123834587 ) ) ;
#93040 = DIRECTION ( 'NONE',  ( -1.000000000000000000, -0.000000000000000000, -0.000000000000000000 ) ) ;
#93042 = EDGE_LOOP ( 'NONE', ( #29230, #38555, #85789, #10089 ) ) ;
#93041 = VECTOR ( 'NONE', #20626, 1000.000000000000227 ) ;
#93043 = CARTESIAN_POINT ( 'NONE',  ( 86.13879346367242817, 46.95025718893440825, -10.63009676298480422 ) ) ;
#93044 = LINE ( 'NONE', #22125, #65322 ) ;
#93045 = CARTESIAN_POINT ( 'NONE',  ( -19.65312891409030271, 93.06504152958497400, 59.99999999999999289 ) ) ;
#93046 = CARTESIAN_POINT ( 'NONE',  ( 85.87384404189388931, 44.42517650707678456, -7.508811624228250103 ) ) ;
#93047 = EDGE_CURVE ( 'NONE', #91263, #11929, #51116, .T. ) ;
#93048 = CARTESIAN_POINT ( 'NONE',  ( 112.8760603413013399, 242.6427522451419350, 10.00000000000009415 ) ) ;
#93049 = CARTESIAN_POINT ( 'NONE',  ( 84.81216594078708226, 50.08139507223255293, -13.70157583983569971 ) ) ;
#93050 = CARTESIAN_POINT ( 'NONE',  ( 16.62988887134222438, 56.19058022948441788, 59.99999999999999289 ) ) ;
#93051 = EDGE_CURVE ( 'NONE', #29881, #38656, #35426, .T. ) ;
#93052 = VERTEX_POINT ( 'NONE', #19749 ) ;
#93053 = CARTESIAN_POINT ( 'NONE',  ( 175.0972523130546676, 258.5006466257072475, 12.88669541573133159 ) ) ;
#93054 = ORIENTED_EDGE ( 'NONE', *, *, #28525, .F. ) ;
#93055 = CARTESIAN_POINT ( 'NONE',  ( 77.23449085028160255, 49.20386544400301432, -14.82971331545884652 ) ) ;
#93056 = ORIENTED_EDGE ( 'NONE', *, *, #45138, .T. ) ;
#93057 = CARTESIAN_POINT ( 'NONE',  ( 156.5497824763685912, 272.6770023486104719, 14.78669166138748814 ) ) ;
#93058 = EDGE_LOOP ( 'NONE', ( #3837, #28620, #85484, #18548, #69199, #48870 ) ) ;
#93059 = CARTESIAN_POINT ( 'NONE',  ( 165.5525849530957885, 274.9503981232618912, -15.45021171627992906 ) ) ;
#93060 = CARTESIAN_POINT ( 'NONE',  ( 36.34934470066777834, 21.39040679176985194, 1.333680081654574804E-15 ) ) ;
#93061 = CARTESIAN_POINT ( 'NONE',  ( 190.6281757562097710, 300.4693095665120381, 3.199750815899911505 ) ) ;
#93062 = CARTESIAN_POINT ( 'NONE',  ( 70.22362515028090968, 62.13392031687246941, -13.81625945947303080 ) ) ;
#93063 = CARTESIAN_POINT ( 'NONE',  ( 147.1603453755519695, 275.7578002805973370, -5.230822882238410187 ) ) ;
#93065 = EDGE_CURVE ( 'NONE', #8119, #51824, #58016, .T. ) ;
#93064 = CARTESIAN_POINT ( 'NONE',  ( 167.7603581743459813, 248.9573463932346158, -5.085697366910332029 ) ) ;
#93066 = DIRECTION ( 'NONE',  ( 0.000000000000000000, 0.000000000000000000, -1.000000000000000000 ) ) ;
#93067 = CARTESIAN_POINT ( 'NONE',  ( 183.4229765504979923, 284.5723098315226025, -15.06534290927836572 ) ) ;
#93068 = CARTESIAN_POINT ( 'NONE',  ( 119.3079296378835181, 245.8149278399160949, -9.188101187500095079 ) ) ;
#93069 = CARTESIAN_POINT ( 'NONE',  ( 70.39572275625086206, 61.09682404813923995, -14.88543345152358022 ) ) ;
#93070 = CARTESIAN_POINT ( 'NONE',  ( 34.67813663163181559, 40.99752408145594273, 5.678558825948277544 ) ) ;
#93071 = CARTESIAN_POINT ( 'NONE',  ( 180.3975999145519324, 291.6145726629062551, -9.903595297598538849 ) ) ;
#93072 = ORIENTED_EDGE ( 'NONE', *, *, #57154, .F. ) ;
#93073 = VECTOR ( 'NONE', #11318, 1000.000000000000114 ) ;
#93074 = CARTESIAN_POINT ( 'NONE',  ( -86.81108781737714253, 4.999999999999999112, 14.21260523776213347 ) ) ;
#93075 = CARTESIAN_POINT ( 'NONE',  ( 180.4159519357722274, 256.0394304848937281, 1.308251353306819187 ) ) ;
#93076 = CARTESIAN_POINT ( 'NONE',  ( 171.0865663407766704, 287.7261751874844435, -4.922011468251167088 ) ) ;
#93077 = CARTESIAN_POINT ( 'NONE',  ( 146.7826225510319489, 276.4120354038443566, 2.803222021035590927 ) ) ;
#93078 = CARTESIAN_POINT ( 'NONE',  ( 72.08687029594609896, 62.01746031163174422, 14.40919635732520021 ) ) ;
#93079 = CARTESIAN_POINT ( 'NONE',  ( 66.27017796984547715, 68.16393141397755073, 4.308032648087416483 ) ) ;
#93080 = DIRECTION ( 'NONE',  ( -0.9303772761487891785, -0.3666034970181814012, 0.000000000000000000 ) ) ;
#93081 = EDGE_CURVE ( 'NONE', #55233, #60043, #50614, .T. ) ;
#93082 = ORIENTED_EDGE ( 'NONE', *, *, #65455, .T. ) ;
#93083 = CARTESIAN_POINT ( 'NONE',  ( 148.2681081336820057, 273.8390989007832559, 10.43132051060321963 ) ) ;
#93084 = CARTESIAN_POINT ( 'NONE',  ( 74.85238693809837685, 54.71601908059493269, -16.61539935277903268 ) ) ;
#93085 = VERTEX_POINT ( 'NONE', #12650 ) ;
#93086 = CARTESIAN_POINT ( 'NONE',  ( 83.37296956034946049, 51.74080471427829053, 14.95189368521467976 ) ) ;
#93087 = CARTESIAN_POINT ( 'NONE',  ( 65.98272894656351184, 68.67277586300092196, -0.2982986715729523119 ) ) ;
#93088 = ORIENTED_EDGE ( 'NONE', *, *, #5832, .T. ) ;
#93089 = CARTESIAN_POINT ( 'NONE',  ( 188.1067865297412709, 265.9162154355072971, -11.65400840555840567 ) ) ;
#93090 = CARTESIAN_POINT ( 'NONE',  ( 156.8527937823772902, 276.5847309089942883, 10.20935908917872581 ) ) ;
#93091 = CARTESIAN_POINT ( 'NONE',  ( 192.3892185349728265, 262.7068694540994898, 4.602004816464169146 ) ) ;
#93092 = LINE ( 'NONE', #24662, #52686 ) ;
#93093 = CARTESIAN_POINT ( 'NONE',  ( 204.6659862557271481, 272.9955293577589259, -9.800396827976472380 ) ) ;
#93095 = CARTESIAN_POINT ( 'NONE',  ( 157.9099320729108342, 280.2816496675481517, 5.725259973247741385 ) ) ;
#93094 = CARTESIAN_POINT ( 'NONE',  ( 164.5092017753200935, 284.2060207574768356, -6.958017126009926834 ) ) ;
#93096 = CARTESIAN_POINT ( 'NONE',  ( 201.0732166862245549, 282.3779679885897167, -18.18766936363638820 ) ) ;
#93097 = ORIENTED_EDGE ( 'NONE', *, *, #81227, .F. ) ;
#93098 = CARTESIAN_POINT ( 'NONE',  ( 204.6905575775918464, 272.9566935833489083, -9.732807054487977894 ) ) ;
#93099 = DIRECTION ( 'NONE',  ( 0.000000000000000000, 1.000000000000000000, 0.000000000000000000 ) ) ;
#93100 = EDGE_CURVE ( 'NONE', #89249, #92701, #96271, .T. ) ;
#93101 = CARTESIAN_POINT ( 'NONE',  ( 72.47507403108335211, 60.92439914301793635, 15.41744962056277224 ) ) ;
#93102 = CARTESIAN_POINT ( 'NONE',  ( -59.29375005653867703, 35.37083770076973366, -10.00000000000000000 ) ) ;
#93103 = CARTESIAN_POINT ( 'NONE',  ( 143.1652255295228997, 257.3466091724133094, -10.00000000000009770 ) ) ;
#93104 = EDGE_CURVE ( 'NONE', #30963, #90765, #73939, .T. ) ;
#93105 = CARTESIAN_POINT ( 'NONE',  ( 188.5830972050926846, 298.6249682447369196, -4.133896775017286807 ) ) ;
#93106 = AXIS2_PLACEMENT_3D ( 'NONE', #75602, #98909, #91825 ) ;
#93107 = CARTESIAN_POINT ( 'NONE',  ( 85.30910355950469182, 47.43175382727999079, 10.99938408205740004 ) ) ;
#93108 = PLANE ( 'NONE',  #9012 ) ;
#93109 = EDGE_CURVE ( 'NONE', #19580, #99795, #4923, .T. ) ;
#93110 =( BOUNDED_CURVE ( )  B_SPLINE_CURVE ( 2, ( #12755, #7113, #14719, #53221, #83666, #84172, #75536, #90278, #6630, #6121, #21821, #74559, #37017 ),
 .UNSPECIFIED., .F., .T. ) 
 B_SPLINE_CURVE_WITH_KNOTS ( ( 3, 2, 2, 2, 2, 2, 3 ),
 ( 0.4124999999999999778, 0.4149999999999999800, 0.4199999999999999845, 0.4249999999999999889, 0.4299999999999999933, 0.4349999999999999978, 0.4375000000000000000 ),
 .UNSPECIFIED. ) 
 CURVE ( )  GEOMETRIC_REPRESENTATION_ITEM ( )  RATIONAL_B_SPLINE_CURVE ( ( 0.9755282581475768211, 0.9755282581475768211, 1.000000000000000000, 0.9510565162951535312, 1.000000000000000000, 0.9510565162951535312, 1.000000000000000000, 0.9510565162951535312, 1.000000000000000000, 0.9510565162951535312, 1.000000000000000000, 0.9755282581475768211, 0.9755282581475768211 ) ) 
 REPRESENTATION_ITEM ( '' )  );
#93111 = CARTESIAN_POINT ( 'NONE',  ( 194.2764122224708103, 294.1503786489221284, 15.46903869661980835 ) ) ;
#93112 = CARTESIAN_POINT ( 'NONE',  ( 191.2589732073035975, 283.0812871616826669, -16.69315749097196289 ) ) ;
#93113 = CARTESIAN_POINT ( 'NONE',  ( 69.66464655795641647, 66.64923878050555572, -10.89182121580662432 ) ) ;
#93114 = CARTESIAN_POINT ( 'NONE',  ( 75.92590343676303632, 205.4548013555409796, -4.594050593750042211 ) ) ;
#93115 = CARTESIAN_POINT ( 'NONE',  ( 37.23771458502426412, 180.7592609112380444, 2.679491924311254714 ) ) ;
#93116 = CARTESIAN_POINT ( 'NONE',  ( 147.5851099763508216, 275.0220864107570264, -4.372720440640867956 ) ) ;
#93117 = DIRECTION ( 'NONE',  ( 0.6303371332823493045, 0.7763215174174871169, 0.000000000000000000 ) ) ;
#93118 = EDGE_CURVE ( 'NONE', #86364, #90974, #53165, .T. ) ;
#93119 = CARTESIAN_POINT ( 'NONE',  ( 84.99999999999997158, 27.49999999999999645, 59.99999999999999289 ) ) ;
#93120 = EDGE_CURVE ( 'NONE', #61384, #37680, #31435, .T. ) ;
#93121 = CARTESIAN_POINT ( 'NONE',  ( 78.60047569677259105, 58.74348153791917326, 16.19982007990188322 ) ) ;
#93122 = CARTESIAN_POINT ( 'NONE',  ( 84.78559661328758068, 49.87520375107067849, -13.17027106718964902 ) ) ;
#93123 = B_SPLINE_CURVE_WITH_KNOTS ( 'NONE', 3,
 ( #16647, #69349, #55130, #40433 ),
 .UNSPECIFIED., .F., .F.,
 ( 4, 4 ),
 ( 0.01401868009846423541, 0.02031335532182578993 ),
 .UNSPECIFIED. ) ;
#93124 = CARTESIAN_POINT ( 'NONE',  ( 78.31490237461567006, 61.48931456610748825, 15.81469504661664516 ) ) ;
#93126 = CARTESIAN_POINT ( 'NONE',  ( 76.16734681154976272, 51.14571779461076773, 16.08280053340072868 ) ) ;
#93125 = CARTESIAN_POINT ( 'NONE',  ( 73.44801800142467130, 69.18349203779057177, -9.987627434106716606 ) ) ;
#93127 = EDGE_CURVE ( 'NONE', #36969, #79746, #37901, .T. ) ;
#93128 = CARTESIAN_POINT ( 'NONE',  ( 193.3641403297651777, 293.0000335917870871, 15.29877003740085861 ) ) ;
#93129 = ADVANCED_FACE ( 'NONE', ( #99738 ), #45509, .T. ) ;
#93130 = CARTESIAN_POINT ( 'NONE',  ( -0.4807448425718762741, 158.9824982072973683, 3.021315404115420679E-15 ) ) ;
#93131 = CARTESIAN_POINT ( 'NONE',  ( 164.0223914878876883, 246.5518796944625421, -5.434886772145694600 ) ) ;
#93132 = CARTESIAN_POINT ( 'NONE',  ( 157.4177733328310467, 257.9914139036126812, 18.29188238796808363 ) ) ;
#93133 = CARTESIAN_POINT ( 'NONE',  ( 170.8926691088181542, 251.4534695730977774, 8.613095916456943613 ) ) ;
#93134 = CARTESIAN_POINT ( 'NONE',  ( 161.8153478334749877, 250.3745914384277285, -14.21120979595050215 ) ) ;
#93135 = CARTESIAN_POINT ( 'NONE',  ( 39.44458330234355969, 184.3923013555410080, 4.594050593750050204 ) ) ;
#93136 = CARTESIAN_POINT ( 'NONE',  ( 55.54680928425421627, 209.0024278399160949, 9.188101187500095079 ) ) ;
#93137 = CARTESIAN_POINT ( 'NONE',  ( 82.21410988452117863, 40.73976263626466476, 3.762362152834610729 ) ) ;
#93138 = CARTESIAN_POINT ( 'NONE',  ( 88.24973202300745356, 44.12735596345137168, 0.4777715347392412215 ) ) ;
#93139 = CARTESIAN_POINT ( 'NONE',  ( 83.93511005065496988, 49.44454015237737821, -13.15056953514552518 ) ) ;
#93140 = CARTESIAN_POINT ( 'NONE',  ( -12.46307465703604400, 163.6115022471902591, 10.00000000000009592 ) ) ;
#93141 = CARTESIAN_POINT ( 'NONE',  ( 197.4342445231449119, 270.1541731842395961, -10.85943118219619485 ) ) ;
#93142 = VECTOR ( 'NONE', #28283, 1000.000000000000000 ) ;
#93143 = CARTESIAN_POINT ( 'NONE',  ( 25.38519627463738715, 32.84336893147757053, -7.433330006724137462 ) ) ;
#93144 = CARTESIAN_POINT ( 'NONE',  ( 150.8168331730346949, 269.4245776381016526, -15.71017957295074652 ) ) ;
#93145 = CARTESIAN_POINT ( 'NONE',  ( 82.94087190812932420, 47.09133877588998018, -11.82568837119483085 ) ) ;
#93146 = CARTESIAN_POINT ( 'NONE',  ( 12.59929316974766955, 12.98920272979924739, 7.433330006724137462 ) ) ;
#93147 = CARTESIAN_POINT ( 'NONE',  ( 69.62006919151632189, 204.8768266524159856, -9.188101187500093303 ) ) ;
#93148 = CARTESIAN_POINT ( 'NONE',  ( 77.16076033720362659, 63.58031483167507503, 15.43380074518343825 ) ) ;
#93149 = CARTESIAN_POINT ( 'NONE',  ( 43.54657591670569872, 62.36930841191391295, 10.00000000000000000 ) ) ;
#93150 = CARTESIAN_POINT ( 'NONE',  ( 159.2876523829509665, 254.7526883847961017, 15.64395448151312351 ) ) ;
#93151 = CARTESIAN_POINT ( 'NONE',  ( 59.27500801855438795, 193.4824982072973683, 3.021315404115420679E-15 ) ) ;
#93152 = CARTESIAN_POINT ( 'NONE',  ( 149.1655084001637022, 275.4698895707030601, 7.593777017023739973 ) ) ;
#93153 = B_SPLINE_CURVE_WITH_KNOTS ( 'NONE', 3,
 ( #50624, #81091, #80589, #19756, #35925, #19272, #88202, #11657, #12657, #57722 ),
 .UNSPECIFIED., .F., .F.,
 ( 4, 2, 2, 2, 4 ),
 ( 0.000000000000000000, 0.0002622400424272852736, 0.0005244800848545705472, 0.0007867201272818558208, 0.001048960169709141094 ),
 .UNSPECIFIED. ) ;
#93154 = AXIS2_PLACEMENT_3D ( 'NONE', #52559, #53067, #13586 ) ;
#93155 = CARTESIAN_POINT ( 'NONE',  ( 75.50969905168113883, 56.69343460978081595, -16.12022845293416751 ) ) ;
#93156 = CARTESIAN_POINT ( 'NONE',  ( 87.51070308547132015, 44.87157588833125033, -6.586006751413206572 ) ) ;
#93157 = CARTESIAN_POINT ( 'NONE',  ( 111.7394020023821781, 241.9865022471903160, 10.00000000000009237 ) ) ;
#93158 = FACE_OUTER_BOUND ( 'NONE', #22804, .T. ) ;
#93159 = CARTESIAN_POINT ( 'NONE',  ( 164.4858674010174298, 245.7491158648375347, -2.958464974013825355 ) ) ;
#93160 = ORIENTED_EDGE ( 'NONE', *, *, #2012, .T. ) ;
#93161 = CARTESIAN_POINT ( 'NONE',  ( 77.12302860632740931, 49.36369884983294298, 15.42198964217536528 ) ) ;
#93162 = CARTESIAN_POINT ( 'NONE',  ( 184.6846741228996507, 271.1466850869315977, 16.33319160510210111 ) ) ;
#93163 = EDGE_LOOP ( 'NONE', ( #22743, #3964, #79378, #92451, #32099 ) ) ;
#93164 = CARTESIAN_POINT ( 'NONE',  ( 159.8597520197352537, 253.7617827468940277, -16.74905990210778839 ) ) ;
#93165 = CARTESIAN_POINT ( 'NONE',  ( 190.3814439774240554, 278.7562814661916946, -16.51409031520932302 ) ) ;
#93166 = CARTESIAN_POINT ( 'NONE',  ( 67.84800455489335036, 68.64766278059737203, -5.501624410574179613 ) ) ;
#93167 = ORIENTED_EDGE ( 'NONE', *, *, #13148, .T. ) ;
#93168 = CARTESIAN_POINT ( 'NONE',  ( 176.7695020951789218, 253.2860360199555316, -0.2578646269232350852 ) ) ;
#93169 = EDGE_LOOP ( 'NONE', ( #4578, #57932 ) ) ;
#93170 = CARTESIAN_POINT ( 'NONE',  ( 79.36831560114676165, 46.38765329515769764, -12.76462913186217030 ) ) ;
#93171 = CARTESIAN_POINT ( 'NONE',  ( 194.8598199529639317, 293.1398868181796615, -15.91766051364927570 ) ) ;
#93172 = CARTESIAN_POINT ( 'NONE',  ( 82.52530459147394026, 45.85050490410911550, 11.59675866233544106 ) ) ;
#93173 = ORIENTED_EDGE ( 'NONE', *, *, #92002, .F. ) ;
#93174 = CARTESIAN_POINT ( 'NONE',  ( 31.61033844661487180, 20.11110640527293825, -2.839279412974138328 ) ) ;
#93175 = CARTESIAN_POINT ( 'NONE',  ( 75.38962278209211831, 56.66636018296492239, 16.13016272302565213 ) ) ;
#93176 = CARTESIAN_POINT ( 'NONE',  ( -61.39381520214497101, 38.43978098112751951, 10.00000000000000000 ) ) ;
#93177 = CARTESIAN_POINT ( 'NONE',  ( 74.68932948184824738, 66.80812537921997318, -13.13442079021221609 ) ) ;
#93178 = ORIENTED_EDGE ( 'NONE', *, *, #21160, .F. ) ;
#93179 = CARTESIAN_POINT ( 'NONE',  ( 156.9440562780969231, 274.4750137900673508, 13.77464823823377316 ) ) ;
#93180 = DIRECTION ( 'NONE',  ( 0.000000000000000000, 1.000000000000000000, 0.000000000000000000 ) ) ;
#93181 = ORIENTED_EDGE ( 'NONE', *, *, #34434, .T. ) ;
#93182 = CARTESIAN_POINT ( 'NONE',  ( 174.6666250183130842, 286.3799292530254093, 11.61780681835062445 ) ) ;
#93184 = CARTESIAN_POINT ( 'NONE',  ( 68.01698362341183213, 65.55827135151169216, -10.29583288777463679 ) ) ;
#93183 = CARTESIAN_POINT ( 'NONE',  ( 67.90965126688126929, 65.44846603141178321, 10.34735008748251595 ) ) ;
#93185 = CARTESIAN_POINT ( 'NONE',  ( 163.2000388741132895, 247.9762362032568035, -11.19676374274550312 ) ) ;
#93186 = CARTESIAN_POINT ( 'NONE',  ( 204.9608076533459950, 275.6444629144898499, 14.31488288944633069 ) ) ;
#93187 = CARTESIAN_POINT ( 'NONE',  ( 162.1260167985288376, 266.6785162637209510, 17.71249957499354366 ) ) ;
#93188 = CARTESIAN_POINT ( 'NONE',  ( 204.6075833744878878, 276.2562653119390461, -13.34672481898815910 ) ) ;
#93191 = EDGE_CURVE ( 'NONE', #76006, #89530, #94290, .T. ) ;
#93190 = CARTESIAN_POINT ( 'NONE',  ( 179.6160012257981862, 295.0481727651569486, 1.085779272287555663 ) ) ;
#93189 =( GEOMETRIC_REPRESENTATION_CONTEXT ( 3 ) GLOBAL_UNCERTAINTY_ASSIGNED_CONTEXT ( ( #16944 ) ) GLOBAL_UNIT_ASSIGNED_CONTEXT ( ( #67455, #20380, #65471 ) ) REPRESENTATION_CONTEXT ( 'NONE', 'WORKASPACE' ) );
#93192 = DIRECTION ( 'NONE',  ( 0.000000000000000000, 0.000000000000000000, 1.000000000000000000 ) ) ;
#93193 = CARTESIAN_POINT ( 'NONE',  ( 195.6684633869053016, 291.3492540482502022, -15.70191374158172160 ) ) ;
#93194 = CARTESIAN_POINT ( 'NONE',  ( 74.03095222233704931, 222.7369531367911293, -4.594050593750048428 ) ) ;
#93195 = ORIENTED_EDGE ( 'NONE', *, *, #60113, .T. ) ;
#93196 = CARTESIAN_POINT ( 'NONE',  ( 151.2648146047323507, 268.6486510375538614, 15.71323890031163550 ) ) ;
#93197 = CARTESIAN_POINT ( 'NONE',  ( -54.25663331465118233, 31.91744790946455979, 10.00000000000000000 ) ) ;
#93198 = VERTEX_POINT ( 'NONE', #48532 ) ;
#93199 = CARTESIAN_POINT ( 'NONE',  ( 157.3433393808201117, 258.1203372903034960, -18.24816514480781393 ) ) ;
#93200 = ORIENTED_EDGE ( 'NONE', *, *, #32915, .T. ) ;
#93201 = ORIENTED_EDGE ( 'NONE', *, *, #30664, .T. ) ;
#93202 = CARTESIAN_POINT ( 'NONE',  ( 66.69106175333467945, 67.85483539735206193, 6.981201250520606472 ) ) ;
#93203 = CARTESIAN_POINT ( 'NONE',  ( 47.03029105687463840, 114.3563895605556269, 177.5919119679930134 ) ) ;
#93204 = EDGE_CURVE ( 'NONE', #47298, #14902, #19857, .T. ) ;
#93205 = CARTESIAN_POINT ( 'NONE',  ( 147.2937583206075942, 275.5267222813735088, 0.1877253132609109920 ) ) ;
#93206 = CARTESIAN_POINT ( 'NONE',  ( 81.29827136372979624, 55.78681482234479461, 16.38844377500790017 ) ) ;
#93207 = CARTESIAN_POINT ( 'NONE',  ( -66.55019942848203129, 42.78701949053055387, 10.00000000000000000 ) ) ;
#93208 = LINE ( 'NONE', #54657, #41496 ) ;
#93209 = ADVANCED_FACE ( 'NONE', ( #16123 ), #926, .F. ) ;
#93210 = CARTESIAN_POINT ( 'NONE',  ( 83.09741599002914825, 218.7833772461660544, -9.188101187500095079 ) ) ;
#93211 = ORIENTED_EDGE ( 'NONE', *, *, #24012, .T. ) ;
#93212 = ORIENTED_EDGE ( 'NONE', *, *, #86491, .T. ) ;
#93213 = DIRECTION ( 'NONE',  ( 1.000000000000000000, 0.000000000000000000, 0.000000000000000000 ) ) ;
#93214 = DIRECTION ( 'NONE',  ( -0.9825427565607363078, 0.1860369090530953895, 0.000000000000000000 ) ) ;
#93215 = ORIENTED_EDGE ( 'NONE', *, *, #65624, .F. ) ;
#93216 = CARTESIAN_POINT ( 'NONE',  ( 21.19599769036394932, 20.43677371833801359, -10.00000000000000355 ) ) ;
#93217 = CARTESIAN_POINT ( 'NONE',  ( 76.26204961069845467, 64.89063096657046970, -14.31995487015190172 ) ) ;
#93218 = CARTESIAN_POINT ( 'NONE',  ( 164.5348324038273518, 245.6643059921780718, 1.473102934610569958 ) ) ;
#93219 = CIRCLE ( 'NONE', #62425, 70.00000000000001421 ) ;
#93220 = CARTESIAN_POINT ( 'NONE',  ( 161.6936156625698970, 283.9059814617143047, 0.5218588777158598146 ) ) ;
#93221 = CARTESIAN_POINT ( 'NONE',  ( 107.5536125507574354, 226.2365022471902876, 10.00000000000009948 ) ) ;
#93222 = CARTESIAN_POINT ( 'NONE',  ( 188.2735287570237688, 299.1710073388255751, -5.251721556916531419 ) ) ;
#93223 = VERTEX_POINT ( 'NONE', #24714 ) ;
#93224 = CARTESIAN_POINT ( 'NONE',  ( 84.94358975746530405, 43.75860775811098335, -6.241023248769397291 ) ) ;
#93225 = CARTESIAN_POINT ( 'NONE',  ( 39.55573625059403753, 31.03677371833805054, 10.00000000000000533 ) ) ;
#93226 = CARTESIAN_POINT ( 'NONE',  ( 29.10553579016685077, 39.73705186507756082, -3.090169943749475845 ) ) ;
#93227 = CARTESIAN_POINT ( 'NONE',  ( 201.2139346379346705, 282.1342373466909521, -16.65315141107179286 ) ) ;
#93228 = VECTOR ( 'NONE', #35009, 1000.000000000000000 ) ;
#93229 = CARTESIAN_POINT ( 'NONE',  ( 72.56545876662167416, 70.71212947315848396, 7.162847399348136079 ) ) ;
#93230 = CARTESIAN_POINT ( 'NONE',  ( 71.98158595747280231, 67.14350720622732638, -11.10114360595152050 ) ) ;
#93231 = ORIENTED_EDGE ( 'NONE', *, *, #7828, .F. ) ;
#93232 = DIRECTION ( 'NONE',  ( -0.8660254037844387076, -0.4999999999999998890, -0.000000000000000000 ) ) ;
#93233 = EDGE_CURVE ( 'NONE', #50517, #58741, #58658, .T. ) ;
#93234 = DIRECTION ( 'NONE',  ( -0.000000000000000000, -0.000000000000000000, -1.000000000000000000 ) ) ;
#93235 = CARTESIAN_POINT ( 'NONE',  ( 29.10614472461704949, 177.6115022471902023, -5.000000000000041744 ) ) ;
#93236 = CARTESIAN_POINT ( 'NONE',  ( 171.6377315803280794, 251.4568186439958879, 7.258662687126358648 ) ) ;
#93237 = CARTESIAN_POINT ( 'NONE',  ( 83.40084016564935609, 52.41263683630168657, 14.84168028052237176 ) ) ;
#93238 = CARTESIAN_POINT ( 'NONE',  ( 156.3322239406982703, 272.0717997662977155, 14.16949642306787815 ) ) ;
#93239 = EDGE_CURVE ( 'NONE', #50293, #56647, #16916, .T. ) ;
#93240 = ORIENTED_EDGE ( 'NONE', *, *, #80679, .F. ) ;
#93241 = EDGE_CURVE ( 'NONE', #40956, #52454, #15603, .T. ) ;
#93242 = CARTESIAN_POINT ( 'NONE',  ( -14.65437209019651732, 102.4994735386711397, 44.28570614930890059 ) ) ;
#93243 = ADVANCED_FACE ( 'NONE', ( #32818 ), #86580, .F. ) ;
#93244 = CIRCLE ( 'NONE', #75437, 3.299999999999978950 ) ;
#93245 = CARTESIAN_POINT ( 'NONE',  ( 207.6727254509676186, 270.9472835030587703, 7.315149605389819953 ) ) ;
#93247 = CARTESIAN_POINT ( 'NONE',  ( 73.77213256992256163, 55.19446632860606883, 16.59757308087127825 ) ) ;
#93246 = CARTESIAN_POINT ( 'NONE',  ( 178.8595466249924755, 265.0989930076032124, -16.03772641351113748 ) ) ;
#93248 = CARTESIAN_POINT ( 'NONE',  ( 61.50992858288473286, 212.9865022471902876, -10.00000000000009592 ) ) ;
#93249 = EDGE_CURVE ( 'NONE', #96074, #2731, #37538, .T. ) ;
#93250 = CARTESIAN_POINT ( 'NONE',  ( 32.18369500442690878, 26.78052372038641948, -10.00000000000000355 ) ) ;
#93251 = CARTESIAN_POINT ( 'NONE',  ( 168.5245981071017809, 273.3323447180702033, 16.01708071253985111 ) ) ;
#93252 = CARTESIAN_POINT ( 'NONE',  ( 166.4096179326797937, 285.9983886822901127, -3.191241580084798191 ) ) ;
#93253 = LINE ( 'NONE', #8128, #97100 ) ;
#93254 = CARTESIAN_POINT ( 'NONE',  ( 188.4600153102442732, 260.9481083049865902, 2.870696243003649339 ) ) ;
#93255 = CARTESIAN_POINT ( 'NONE',  ( 207.3646600298985447, 271.4808684644054324, -5.284084612275558257 ) ) ;
#93256 = CARTESIAN_POINT ( 'NONE',  ( 7.753205860782987457, 175.2833772461660544, -9.188101187500095079 ) ) ;
#93257 = DIRECTION ( 'NONE',  ( -0.8660254037844387076, -0.4999999999999998890, -0.000000000000000000 ) ) ;
#93258 = ORIENTED_EDGE ( 'NONE', *, *, #92315, .T. ) ;
#93259 = CARTESIAN_POINT ( 'NONE',  ( 174.8608349436526055, 255.3260918886272179, 8.528007662106622533 ) ) ;
#93260 = CARTESIAN_POINT ( 'NONE',  ( 37.96661208706053969, 52.86061180733513964, -10.00000000000000000 ) ) ;
#93261 = CARTESIAN_POINT ( 'NONE',  ( 81.57802524835842917, 41.68064318211084185, 5.833990239057619931 ) ) ;
#93262 = CARTESIAN_POINT ( 'NONE',  ( 23.55782238408398044, 196.6589784336661353, -6.496448406907676862E-16 ) ) ;
#93263 = CARTESIAN_POINT ( 'NONE',  ( 25.74102936209481385, 30.56454794089042437, 10.00000000000000355 ) ) ;
#93264 = CARTESIAN_POINT ( 'NONE',  ( 36.19122982252199705, 21.86426979415092120, -3.090169943749474069 ) ) ;
#93265 = CARTESIAN_POINT ( 'NONE',  ( 76.61888230025124358, 51.35972145274618583, 16.07233720520855158 ) ) ;
#93266 = CARTESIAN_POINT ( 'NONE',  ( 103.1513167481865310, 230.3615022471902591, -10.00000000000009592 ) ) ;
#93267 = CARTESIAN_POINT ( 'NONE',  ( 134.1658515176688127, 258.2677522451419350, -5.000000000000047962 ) ) ;
#93268 = PLANE ( 'NONE',  #45686 ) ;
#93269 = CARTESIAN_POINT ( 'NONE',  ( 188.3805762680232192, 260.4081077799571631, -0.7596527320232882019 ) ) ;
#93270 = CARTESIAN_POINT ( 'NONE',  ( 64.18017357788677657, 207.8615022471902307, -10.00000000000009592 ) ) ;
#93271 = CARTESIAN_POINT ( 'NONE',  ( 67.86202049053581220, 66.83700393428978259, -8.676109968774889936 ) ) ;
#93272 = CARTESIAN_POINT ( 'NONE',  ( 206.5545904789651388, 271.4197609012314274, 6.179362329135090981 ) ) ;
#93273 = CARTESIAN_POINT ( 'NONE',  ( 35.84507844392322085, 185.3768266524159856, -9.188101187500091527 ) ) ;
#93274 = CARTESIAN_POINT ( 'NONE',  ( 72.12013178652179590, 70.28500072208976235, -8.194891429308611919 ) ) ;
#93275 = EDGE_CURVE ( 'NONE', #23755, #45951, #2143, .T. ) ;
#93276 = DIRECTION ( 'NONE',  ( 0.4803199113995043623, -0.8770933717188679202, 0.000000000000000000 ) ) ;
#93277 = CARTESIAN_POINT ( 'NONE',  ( 203.9116033662877783, 270.5127528292231318, -6.455590966117181750 ) ) ;
#93278 = B_SPLINE_CURVE_WITH_KNOTS ( 'NONE', 3,
 ( #97535, #28104, #70080, #61970, #14887, #92923, #76698, #86356, #54886, #23476, #77717, #45776, #63495, #1202, #77194, #85866 ),
 .UNSPECIFIED., .F., .F.,
 ( 4, 1, 2, 2, 2, 1, 2, 2, 4 ),
 ( 0.000000000000000000, 0.1250000000000013600, 0.1875000000000028866, 0.2500000000000043854, 0.4999999999999998890, 0.6249999999999976685, 0.6874999999999965583, 0.7499999999999954481, 1.000000000000000000 ),
 .UNSPECIFIED. ) ;
#93279 = CARTESIAN_POINT ( 'NONE',  ( 151.1230807375396807, 268.8941412966845519, -14.26613110909109849 ) ) ;
#93280 = CARTESIAN_POINT ( 'NONE',  ( 67.32971676510786097, 66.39089803301675374, -8.864210629079892101 ) ) ;
#93281 = DIRECTION ( 'NONE',  ( 0.000000000000000000, 0.000000000000000000, -1.000000000000000000 ) ) ;
#93282 = CARTESIAN_POINT ( 'NONE',  ( 159.9029087581434396, 278.3966458521681488, -10.39982288579484582 ) ) ;
#93283 = CARTESIAN_POINT ( 'NONE',  ( 44.95821123098110661, 116.5722627105190270, 10.00000000000000000 ) ) ;
#93284 = CARTESIAN_POINT ( 'NONE',  ( 16.26188567080226477, 32.49540643055187417, 3.479690158560446702E-15 ) ) ;
#93285 = CARTESIAN_POINT ( 'NONE',  ( 189.9052851100924215, 301.7213928939034986, -1.077181946533001256 ) ) ;
#93286 = CARTESIAN_POINT ( 'NONE',  ( 72.03863647653309954, 59.27131230149748831, 15.34878527849881458 ) ) ;
#93287 = VECTOR ( 'NONE', #78091, 1000.000000000000227 ) ;
#93288 = CARTESIAN_POINT ( 'NONE',  ( 174.7028696250029043, 256.5417377999049222, 12.02695302890117546 ) ) ;
#93289 = ORIENTED_EDGE ( 'NONE', *, *, #37013, .F. ) ;
#93290 = CARTESIAN_POINT ( 'NONE',  ( 37.76795716069911890, 37.50829794293884589, -10.00000000000000355 ) ) ;
#93291 = AXIS2_PLACEMENT_3D ( 'NONE', #59018, #89988, #88519 ) ;
#93292 = CARTESIAN_POINT ( 'NONE',  ( 8.697374518098676788, 25.99752408145590366, 5.678558825948276656 ) ) ;
#93293 = CARTESIAN_POINT ( 'NONE',  ( 73.37087704974057090, 59.79349537656993618, -15.44674116277980147 ) ) ;
#93294 = CARTESIAN_POINT ( 'NONE',  ( 81.89248010131869648, 42.20395449353005546, 7.637921802679397132 ) ) ;
#93295 = ORIENTED_EDGE ( 'NONE', *, *, #54975, .T. ) ;
#93296 = CARTESIAN_POINT ( 'NONE',  ( -12.95261720355844126, 24.63757726406876003, -10.00000000000000000 ) ) ;
#93297 = CARTESIAN_POINT ( 'NONE',  ( 69.27156750288784792, 70.56227451142774498, -1.298478209937802719 ) ) ;
#93298 = VECTOR ( 'NONE', #92464, 1000.000000000000114 ) ;
#93299 = CARTESIAN_POINT ( 'NONE',  ( 150.6453220160077251, 269.7216436761371483, 14.94145576020818034 ) ) ;
#93300 = CARTESIAN_POINT ( 'NONE',  ( 172.5992896740868616, 281.6695515350652954, -14.94842763437895350 ) ) ;
#93301 = VERTEX_POINT ( 'NONE', #48011 ) ;
#93302 = ORIENTED_EDGE ( 'NONE', *, *, #26826, .T. ) ;
#93304 = CARTESIAN_POINT ( 'NONE',  ( 87.13830015243127036, 43.52866481668240084, -0.7691705554832481972 ) ) ;
#93303 = CARTESIAN_POINT ( 'NONE',  ( 186.5384767560921091, 272.2703538590346852, -15.99658917633080613 ) ) ;
#93305 = ORIENTED_EDGE ( 'NONE', *, *, #78804, .T. ) ;
#93306 = CARTESIAN_POINT ( 'NONE',  ( 201.4520623681621316, 281.7217880192456505, -17.56577389517433119 ) ) ;
#93307 = CARTESIAN_POINT ( 'NONE',  ( 71.94697066620052794, 72.20377774097838142, -3.624262489285473343 ) ) ;
#93308 = CARTESIAN_POINT ( 'NONE',  ( 80.01979875032591849, 57.54866692369599690, 16.59896302490742315 ) ) ;
#93309 = CARTESIAN_POINT ( 'NONE',  ( 77.24238159045749796, 63.47610639771342278, 15.48509222746617553 ) ) ;
#93310 = CARTESIAN_POINT ( 'NONE',  ( 189.8763472015711216, 301.7715148217271803, -0.1184663095182975079 ) ) ;
#93311 = EDGE_CURVE ( 'NONE', #75967, #8895, #91636, .T. ) ;
#93312 = CARTESIAN_POINT ( 'NONE',  ( 196.4501996009505831, 290.3852684645433442, -17.82325615854289680 ) ) ;
#93313 = VERTEX_POINT ( 'NONE', #423 ) ;
#93314 = AXIS2_PLACEMENT_3D ( 'NONE', #90413, #18610, #1907 ) ;
#93315 = CARTESIAN_POINT ( 'NONE',  ( 156.5497824763685912, 272.6770023486104719, 14.78669166138748814 ) ) ;
#93316 = VECTOR ( 'NONE', #10466, 1000.000000000000227 ) ;
#93317 = CARTESIAN_POINT ( 'NONE',  ( 162.0238244467804805, 266.8515061766926237, 16.62455803315057068 ) ) ;
#93318 = ORIENTED_EDGE ( 'NONE', *, *, #46570, .T. ) ;
#93319 = CARTESIAN_POINT ( 'NONE',  ( 31.84670776885679899, 24.10170272979928541, -7.433330006724141015 ) ) ;
#93320 = CARTESIAN_POINT ( 'NONE',  ( 190.3572031550745294, 300.9386478791372497, 3.093832330100951378 ) ) ;
#93321 = CARTESIAN_POINT ( 'NONE',  ( 78.19070433545205390, 47.56140015029151868, -14.40966192187991624 ) ) ;
#93322 = VERTEX_POINT ( 'NONE', #31312 ) ;
#93323 = EDGE_CURVE ( 'NONE', #99384, #29626, #83538, .T. ) ;
#93324 = CARTESIAN_POINT ( 'NONE',  ( 44.35815684012577265, 67.96982248125696913, -10.00000000000000000 ) ) ;
#93325 = CARTESIAN_POINT ( 'NONE',  ( 25.26661199696083671, 36.36126292948896577, 6.180339887498949913 ) ) ;
#93326 = CARTESIAN_POINT ( 'NONE',  ( 150.3774144590728952, 270.1856731764797814, 13.91914410364283938 ) ) ;
#93327 = CARTESIAN_POINT ( 'NONE',  ( 40.62554608437772430, 25.58380873178790083, 6.180339887498953466 ) ) ;
#93328 = ORIENTED_EDGE ( 'NONE', *, *, #79163, .T. ) ;
#93329 = EDGE_CURVE ( 'NONE', #27171, #23113, #80975, .T. ) ;
#93330 = ORIENTED_EDGE ( 'NONE', *, *, #6391, .F. ) ;
#93331 = CARTESIAN_POINT ( 'NONE',  ( 185.5036743169331430, 269.5266205919543268, -16.28606374402843571 ) ) ;
#93332 = CARTESIAN_POINT ( 'NONE',  ( 147.3023124603499809, 275.5119060767245287, 5.196938859334171212 ) ) ;
#93333 = CARTESIAN_POINT ( 'NONE',  ( 190.6071113721798156, 300.5057941498820924, -0.4754021072632813594 ) ) ;
#93334 = ORIENTED_EDGE ( 'NONE', *, *, #92773, .T. ) ;
#93335 = CARTESIAN_POINT ( 'NONE',  ( 149.0802055316563326, 272.4325049467973940, 12.84384348890831085 ) ) ;
#93336 = CARTESIAN_POINT ( 'NONE',  ( 174.1990609491486737, 253.0008501898304871, 8.022018053261177783 ) ) ;
#93337 = CARTESIAN_POINT ( 'NONE',  ( 48.91227514082039107, 78.96591507484178862, -10.00000000000000000 ) ) ;
#93338 = CARTESIAN_POINT ( 'NONE',  ( 192.4335622838504207, 297.3422883733380786, -12.83044365323471325 ) ) ;
#93339 = CARTESIAN_POINT ( 'NONE',  ( 163.9961211234992788, 256.9275610305372766, 16.20495027727189807 ) ) ;
#93340 = CARTESIAN_POINT ( 'NONE',  ( 68.70434024268674023, 64.76539896931275564, 11.44226853676074995 ) ) ;
#93341 = CARTESIAN_POINT ( 'NONE',  ( 164.3754245770190039, 245.9404084473339083, 1.667926061651832992 ) ) ;
#93342 = CARTESIAN_POINT ( 'NONE',  ( 67.44483578933650847, 66.62155022141699590, 8.635578642564382790 ) ) ;
#93343 = CARTESIAN_POINT ( 'NONE',  ( 73.51625129091058852, 64.84468117635124429, -13.42585287280998330 ) ) ;
#93344 = CARTESIAN_POINT ( 'NONE',  ( 78.56500620533599033, 47.97831951877432743, 13.95998044843349817 ) ) ;
#93345 = CARTESIAN_POINT ( 'NONE',  ( 100.7694865641816051, 238.1744531367911293, 4.594050593750047540 ) ) ;
#93346 = ORIENTED_EDGE ( 'NONE', *, *, #75481, .F. ) ;
#93347 = CARTESIAN_POINT ( 'NONE',  ( 191.6723191112861855, 298.6608002251342100, -9.737039817265848995 ) ) ;
#93348 = CARTESIAN_POINT ( 'NONE',  ( 82.81954554793986745, 41.27561870364412755, -2.050892944899044945 ) ) ;
#93349 = LINE ( 'NONE', #3021, #91631 ) ;
#93350 = CARTESIAN_POINT ( 'NONE',  ( 203.5080190724872011, 278.1607665491929993, -15.47044080916498743 ) ) ;
#93351 = B_SPLINE_CURVE_WITH_KNOTS ( 'NONE', 3,
 ( #65191, #89546, #59054, #12504, #43375, #20107, #74320, #96635, #89071, #80950 ),
 .UNSPECIFIED., .F., .F.,
 ( 4, 2, 2, 2, 4 ),
 ( 0.000000000000000000, 0.2499999999999991118, 0.4999999999999982236, 0.7499999999999991118, 1.000000000000000000 ),
 .UNSPECIFIED. ) ;
#93352 = CARTESIAN_POINT ( 'NONE',  ( 163.9704062730716032, 246.6419207277664327, 7.317582738093436845 ) ) ;
#93353 = CARTESIAN_POINT ( 'NONE',  ( 83.83681109075200766, 51.55721269723052558, -14.37373883924508000 ) ) ;
#93354 = CARTESIAN_POINT ( 'NONE',  ( 70.15619903503488786, 64.92682878892891551, -12.01717930017344038 ) ) ;
#93355 = ORIENTED_EDGE ( 'NONE', *, *, #69288, .F. ) ;
#93356 = CARTESIAN_POINT ( 'NONE',  ( 208.1612901671020381, 270.1010645919285480, -2.401583477149568768 ) ) ;
#93357 = EDGE_CURVE ( 'NONE', #24937, #92554, #34448, .T. ) ;
#93358 = CARTESIAN_POINT ( 'NONE',  ( 72.48128350488923388, 71.72257018173657173, 5.902110541236717189 ) ) ;
#93359 = CARTESIAN_POINT ( 'NONE',  ( 206.1542244435759983, 272.8725460781796528, 8.903176382340632244 ) ) ;
#93360 = CARTESIAN_POINT ( 'NONE',  ( 127.1021582719434662, 250.3149278399160949, -9.188101187500095079 ) ) ;
#93361 = CARTESIAN_POINT ( 'NONE',  ( 156.6812872898450735, 261.2670451491295012, 0.000000000000000000 ) ) ;
#93362 = CARTESIAN_POINT ( 'NONE',  ( 186.0639839519483019, 296.8412207699221881, 4.661798123928299731 ) ) ;
#93363 = CARTESIAN_POINT ( 'NONE',  ( 157.5520850189458884, 257.7587792392113215, 16.71892742266126319 ) ) ;
#93364 = DIRECTION ( 'NONE',  ( -0.8660254037844392627, -0.4999999999999987232, 0.000000000000000000 ) ) ;
#93365 = CARTESIAN_POINT ( 'NONE',  ( 54.19381813872350762, 202.0958772461660544, -9.188101187500095079 ) ) ;
#93366 = AXIS2_PLACEMENT_3D ( 'NONE', #61754, #54141, #84123 ) ;
#93368 = CARTESIAN_POINT ( 'NONE',  ( 67.41248320326423027, 66.37693208286884783, -8.946798147498746800 ) ) ;
#93367 = AXIS2_PLACEMENT_3D ( 'NONE', #78469, #39424, #84591 ) ;
#93369 = VERTEX_POINT ( 'NONE', #89567 ) ;
#93370 = CARTESIAN_POINT ( 'NONE',  ( 72.47029212360676809, 67.90129717547449673, 10.67585825917434761 ) ) ;
#93372 = DIRECTION ( 'NONE',  ( 1.000000000000000000, 0.000000000000000000, -0.000000000000000000 ) ) ;
#93371 = B_SPLINE_CURVE_WITH_KNOTS ( 'NONE', 3,
 ( #75152, #96485, #36617, #58908, #4233, #67525, #59918, #13830, #3758, #98455 ),
 .UNSPECIFIED., .F., .F.,
 ( 4, 2, 2, 2, 4 ),
 ( 3.453764301715650149E-15, 0.0004337349686803219548, 0.0008674699373571900752, 0.001301204906034058358, 0.001734939874710926533 ),
 .UNSPECIFIED. ) ;
#93373 = EDGE_CURVE ( 'NONE', #99290, #11051, #31256, .T. ) ;
#93374 = B_SPLINE_SURFACE_WITH_KNOTS ( 'NONE', 3, 1, ( 
 ( #26052, #64543 ),
 ( #56925, #87913 ),
 ( #47327, #18456 ),
 ( #10852, #72672 ),
 ( #3265, #50329 ),
 ( #81280, #28026 ),
 ( #74659, #49838 ),
 ( #36115, #96480 ),
 ( #75146, #80795 ),
 ( #88404, #11372 ),
 ( #97458, #11854 ),
 ( #96983, #73161 ),
 ( #50823, #67019 ),
 ( #42223, #81773 ),
 ( #57425, #97946 ),
 ( #58901, #43212 ),
 ( #82779, #89871 ),
 ( #51839, #12857 ),
 ( #43715, #20446 ),
 ( #89396, #57930 ),
 ( #3753, #26551 ),
 ( #27554, #12346 ),
 ( #51315, #66532 ),
 ( #34631, #28519 ),
 ( #90379, #82284 ),
 ( #44211, #19947 ),
 ( #65531, #58420 ),
 ( #27048, #59402 ),
 ( #5237, #88912 ),
 ( #19472, #95989 ),
 ( #42711, #73645 ),
 ( #4226, #35126 ),
 ( #66036, #74155 ),
 ( #4747, #20956 ) ),
 .UNSPECIFIED., .T., .F., .F.,
 ( 4, 2, 2, 2, 2, 2, 2, 2, 2, 2, 2, 2, 2, 2, 2, 2, 4 ),
 ( 2, 2 ),
 ( 0.000000000000000000, 0.06250000000000000000, 0.1250000000000000000, 0.1875000000000000000, 0.2500000000000000000, 0.3125000000000000000, 0.3750000000000000000, 0.4375000000000000000, 0.5000000000000000000, 0.5625000000000000000, 0.6250000000000000000, 0.6875000000000000000, 0.7500000000000000000, 0.8125000000000000000, 0.8750000000000000000, 0.9375000000000000000, 1.000000000000000000 ),
 ( 0.000000000000000000, 1.000000000000000000 ),
 .UNSPECIFIED. ) ;
#93375 = DIRECTION ( 'NONE',  ( 0.000000000000000000, 0.000000000000000000, 1.000000000000000000 ) ) ;
#93376 = CARTESIAN_POINT ( 'NONE',  ( 174.6105168250273323, 262.0571681988877799, 14.27631620660720735 ) ) ;
#93377 = CARTESIAN_POINT ( 'NONE',  ( 82.09393458893232776, 41.85502508557050305, -5.540192124174895483 ) ) ;
#93378 = CARTESIAN_POINT ( 'NONE',  ( 203.4357368910538355, 278.2859629599173559, -16.45855118664066197 ) ) ;
#93379 = CARTESIAN_POINT ( 'NONE',  ( 153.6187353439852075, 269.2963960243311021, -15.64461193481829504 ) ) ;
#93380 = VECTOR ( 'NONE', #93590, 1000.000000000000000 ) ;
#93381 = CARTESIAN_POINT ( 'NONE',  ( 108.1850894041357094, 223.2677522451417929, -5.000000000000041744 ) ) ;
#93382 = CARTESIAN_POINT ( 'NONE',  ( 194.2385081474906769, 292.6568478422810244, -15.46372919447845362 ) ) ;
#93383 = ORIENTED_EDGE ( 'NONE', *, *, #85122, .F. ) ;
#93384 = CARTESIAN_POINT ( 'NONE',  ( 162.8789161433191452, 248.5324370884573568, 9.731756914259689140 ) ) ;
#93385 = DIRECTION ( 'NONE',  ( -0.8660254037844387076, -0.4999999999999998890, -0.000000000000000000 ) ) ;
#93386 = ADVANCED_FACE ( 'NONE', ( #10531 ), #12029, .T. ) ;
#93387 = CARTESIAN_POINT ( 'NONE',  ( 27.99689677000926125, 174.7202760586659736, -5.415160957724236172E-17 ) ) ;
#93388 = CARTESIAN_POINT ( 'NONE',  ( 19.28614774617036787, 10.94473085651391386, 1.475505719884397138E-15 ) ) ;
#93389 = VECTOR ( 'NONE', #41198, 1000.000000000000000 ) ;
#93390 = FACE_OUTER_BOUND ( 'NONE', #17042, .T. ) ;
#93391 = CARTESIAN_POINT ( 'NONE',  ( 26.02075121854041839, 117.3566028095996643, 59.99999999999999289 ) ) ;
#93392 = CARTESIAN_POINT ( 'NONE',  ( 72.24325681757291306, 72.08904859244903207, 3.121326503868123492 ) ) ;
#93394 = CARTESIAN_POINT ( 'NONE',  ( 68.53719034102077501, 216.5024278399160664, 9.188101187500095079 ) ) ;
#93393 = CARTESIAN_POINT ( 'NONE',  ( 198.2212904662371500, 277.5279118919263510, -15.45398242064391781 ) ) ;
#93395 = CARTESIAN_POINT ( 'NONE',  ( 161.3193951073452581, 251.2336067582368742, 13.01220207292984377 ) ) ;
#93396 = CARTESIAN_POINT ( 'NONE',  ( 174.5315600938332921, 289.3520206179668435, 7.862896886311159683 ) ) ;
#93397 = CARTESIAN_POINT ( 'NONE',  ( -31.80880183691780871, 96.77778971401760089, 44.36020821963600724 ) ) ;
#93398 = CARTESIAN_POINT ( 'NONE',  ( 10.48369258086752787, 24.79103043416547791, 8.090169943749478065 ) ) ;
#93399 = ORIENTED_EDGE ( 'NONE', *, *, #24354, .T. ) ;
#93400 = B_SPLINE_CURVE_WITH_KNOTS ( 'NONE', 3,
 ( #39588, #16313, #26296, #87665 ),
 .UNSPECIFIED., .F., .F.,
 ( 4, 4 ),
 ( 0.01540896664962445803, 0.02418941936981118535 ),
 .UNSPECIFIED. ) ;
#93401 =( BOUNDED_CURVE ( )  B_SPLINE_CURVE ( 2, ( #49859, #80309, #2795, #18989, #66556, #80825, #50849, #43240, #3291 ),
 .UNSPECIFIED., .F., .T. ) 
 B_SPLINE_CURVE_WITH_KNOTS ( ( 3, 2, 2, 2, 3 ),
 ( 0.7137096774193548709, 0.7150537634408602461, 0.7177419354838709964, 0.7204301075268817467, 0.7217741935483871218 ),
 .UNSPECIFIED. ) 
 CURVE ( )  GEOMETRIC_REPRESENTATION_ITEM ( )  RATIONAL_B_SPLINE_CURVE ( ( 0.9330127018922194093, 0.9330127018922194093, 1.000000000000000000, 0.8660254037844387076, 1.000000000000000000, 0.8660254037844387076, 1.000000000000000000, 0.9330127018922194093, 0.9330127018922194093 ) ) 
 REPRESENTATION_ITEM ( '' )  );
#93402 = CARTESIAN_POINT ( 'NONE',  ( 163.2842962196203302, 267.9677010721593433, 16.49754710497367682 ) ) ;
#93403 = CARTESIAN_POINT ( 'NONE',  ( 23.40481081636943017, 190.9865022471903160, 10.00000000000009237 ) ) ;
#93404 = CARTESIAN_POINT ( 'NONE',  ( 34.06774859691741142, 197.1427522451419350, -10.00000000000009592 ) ) ;
#93405 = VECTOR ( 'NONE', #38251, 1000.000000000000000 ) ;
#93406 = CARTESIAN_POINT ( 'NONE',  ( 162.9466247808429102, 248.4151622881552441, 11.25765811906727443 ) ) ;
#93407 = CARTESIAN_POINT ( 'NONE',  ( -3.126064726376516667, 162.8768266524159856, -9.188101187500091527 ) ) ;
#93408 = CARTESIAN_POINT ( 'NONE',  ( 28.93108252874724684, 32.10171378149919974, 9.188101187500008038 ) ) ;
#93410 = EDGE_CURVE ( 'NONE', #24841, #51452, #79469, .T. ) ;
#93409 = CARTESIAN_POINT ( 'NONE',  ( 168.6534459294139481, 262.6503232764572431, 15.96541089746672171 ) ) ;
#93411 = CARTESIAN_POINT ( 'NONE',  ( 185.3010781374966882, 260.3148984547196960, 6.941109534206622911 ) ) ;
#93412 = CARTESIAN_POINT ( 'NONE',  ( 205.7639495959071212, 274.2533802642843170, 10.79039487422292432 ) ) ;
#93413 = CARTESIAN_POINT ( 'NONE',  ( 183.1769575194604158, 257.7542008109865037, -2.146814141465986481 ) ) ;
#93414 = B_SPLINE_CURVE_WITH_KNOTS ( 'NONE', 3,
 ( #69365, #98292, #44552, #37452, #91205, #53169, #92223, #8080, #83609, #75486 ),
 .UNSPECIFIED., .F., .F.,
 ( 4, 2, 2, 2, 4 ),
 ( 0.000000000000000000, 0.0002622400424272794731, 0.0005244800848545589462, 0.0007867201272818383651, 0.001048960169709117892 ),
 .UNSPECIFIED. ) ;
#93415 = CARTESIAN_POINT ( 'NONE',  ( 66.14637081899437021, 69.08478385240519515, 2.576720762024273359 ) ) ;
#93416 = ORIENTED_EDGE ( 'NONE', *, *, #19468, .T. ) ;
#93417 = CARTESIAN_POINT ( 'NONE',  ( 176.2544971312975974, 263.4220703943961439, 15.96855061784746610 ) ) ;
#93418 = CARTESIAN_POINT ( 'NONE',  ( 178.5167212123578224, 285.5003866454536023, 13.01602787300356923 ) ) ;
#93419 = CARTESIAN_POINT ( 'NONE',  ( 156.1933712160320908, 280.4387541887718953, -5.510142736702231758 ) ) ;
#93420 = CARTESIAN_POINT ( 'NONE',  ( 14.33134397731654630, 13.98920272979924917, 7.433330006724137462 ) ) ;
#93421 = ORIENTED_EDGE ( 'NONE', *, *, #45650, .F. ) ;
#93422 = CARTESIAN_POINT ( 'NONE',  ( 159.9681198662056545, 253.5740841309004452, 14.91312641984554688 ) ) ;
#93423 = CARTESIAN_POINT ( 'NONE',  ( 157.7847820078105201, 257.3557362317297361, -18.02899742403477035 ) ) ;
#93424 = FACE_OUTER_BOUND ( 'NONE', #77719, .T. ) ;
#93425 = CARTESIAN_POINT ( 'NONE',  ( 32.72712820738424000, 19.86426979415091054, -3.090169943749474069 ) ) ;
#93426 = CARTESIAN_POINT ( 'NONE',  ( -13.83735209449856640, 104.3088569339948180, 43.92483008768037678 ) ) ;
#93427 = DIRECTION ( 'NONE',  ( -0.000000000000000000, -0.000000000000000000, -1.000000000000000000 ) ) ;
#93428 = CARTESIAN_POINT ( 'NONE',  ( 207.8136982414359579, 270.7031114674828700, -0.9536989003868096004 ) ) ;
#93429 = CARTESIAN_POINT ( 'NONE',  ( 152.6692142062575499, 266.2161595735824449, -16.77985299603479419 ) ) ;
#93430 = ORIENTED_EDGE ( 'NONE', *, *, #22591, .T. ) ;
#93431 = ORIENTED_EDGE ( 'NONE', *, *, #26811, .F. ) ;
#93432 = CARTESIAN_POINT ( 'NONE',  ( 24.55112987542764458, 40.41347472807388641, -10.00000000000000000 ) ) ;
#93433 = CARTESIAN_POINT ( 'NONE',  ( 72.79448081417055505, 70.83012470017415296, 7.186594751207691978 ) ) ;
#93434 = ORIENTED_EDGE ( 'NONE', *, *, #17115, .F. ) ;
#93435 = FACE_OUTER_BOUND ( 'NONE', #46837, .T. ) ;
#93436 = PLANE ( 'NONE',  #28991 ) ;
#93437 = ORIENTED_EDGE ( 'NONE', *, *, #26945, .F. ) ;
#93438 = CARTESIAN_POINT ( 'NONE',  ( 32.74483707338229266, 117.8038484974524351, 59.99999999999999289 ) ) ;
#93439 = CARTESIAN_POINT ( 'NONE',  ( 79.16081066472990813, 59.09338877662139566, -16.21814646735712273 ) ) ;
#93440 = CARTESIAN_POINT ( 'NONE',  ( 30.69616969366791537, 176.9824982072973967, 3.021315404115420679E-15 ) ) ;
#93441 = CARTESIAN_POINT ( 'NONE',  ( 85.84005213714648619, 47.01912803749855385, -10.88097575854029309 ) ) ;
#93442 = CARTESIAN_POINT ( 'NONE',  ( 69.95297458392498413, 62.89479584344802277, 13.86435754852248969 ) ) ;
#93443 = VERTEX_POINT ( 'NONE', #10033 ) ;
#93444 = CARTESIAN_POINT ( 'NONE',  ( 203.3278261089206183, 278.4728699172566735, 16.54899263865330994 ) ) ;
#93445 = VECTOR ( 'NONE', #76827, 1000.000000000000114 ) ;
#93446 = CARTESIAN_POINT ( 'NONE',  ( 150.6453220160077251, 269.7216436761371483, 14.94145576020818034 ) ) ;
#93447 = CARTESIAN_POINT ( 'NONE',  ( 40.36445127458296867, 23.70852965304482041, 1.583844403245330712 ) ) ;
#93448 = EDGE_LOOP ( 'NONE', ( #11192, #40543, #35481, #59386 ) ) ;
#93449 = ORIENTED_EDGE ( 'NONE', *, *, #87184, .T. ) ;
#93450 = EDGE_CURVE ( 'NONE', #85874, #27025, #87602, .T. ) ;
#93451 = CARTESIAN_POINT ( 'NONE',  ( 160.2402339746914777, 268.8803885730948195, -16.99231777190169623 ) ) ;
#93452 = VERTEX_POINT ( 'NONE', #73822 ) ;
#93453 = EDGE_CURVE ( 'NONE', #100173, #35725, #18636, .T. ) ;
#93454 = CARTESIAN_POINT ( 'NONE',  ( 42.25626477193290498, 60.39660150822810891, 10.00000000000000000 ) ) ;
#93455 = ORIENTED_EDGE ( 'NONE', *, *, #3560, .F. ) ;
#93456 = CARTESIAN_POINT ( 'NONE',  ( 163.8947349411736525, 246.7729873192901664, -5.868803394723933309 ) ) ;
#93457 = VECTOR ( 'NONE', #33731, 1000.000000000000114 ) ;
#93458 = CARTESIAN_POINT ( 'NONE',  ( 83.56215914360431896, 50.45755031246686428, 13.86092672225745837 ) ) ;
#93459 = ADVANCED_FACE ( 'NONE', ( #64220 ), #35428, .F. ) ;
#93460 = CARTESIAN_POINT ( 'NONE',  ( 165.3974121193675160, 271.2591920438384818, 17.13699628004796693 ) ) ;
#93461 = FACE_OUTER_BOUND ( 'NONE', #37147, .T. ) ;
#93462 = EDGE_CURVE ( 'NONE', #50507, #16411, #43900, .T. ) ;
#93463 = CARTESIAN_POINT ( 'NONE',  ( 147.9311236323648870, 274.4227731784279172, -7.799459659034405412 ) ) ;
#93464 = DIRECTION ( 'NONE',  ( -0.8660254037844387076, -0.4999999999999998890, -0.000000000000000000 ) ) ;
#93465 = DIRECTION ( 'NONE',  ( -0.8660254037844387076, -0.4999999999999998890, -0.000000000000000000 ) ) ;
#93466 = CARTESIAN_POINT ( 'NONE',  ( 166.3150859005863254, 247.0070523979024983, 1.903668903753348518 ) ) ;
#93467 = CARTESIAN_POINT ( 'NONE',  ( 15.07770630580378501, 30.74646525600389424, 2.839279412974139660 ) ) ;
#93468 = CARTESIAN_POINT ( 'NONE',  ( 178.0302064638906074, 292.4640037680099454, 7.106335582765731296 ) ) ;
#93469 = CARTESIAN_POINT ( 'NONE',  ( 80.56456852273207403, 57.68474611512090888, 16.59351620786970116 ) ) ;
#93471 = ORIENTED_EDGE ( 'NONE', *, *, #56926, .T. ) ;
#93470 = CARTESIAN_POINT ( 'NONE',  ( 159.2554912534056939, 254.8083930951974878, 16.49944922174842432 ) ) ;
#93472 = AXIS2_PLACEMENT_3D ( 'NONE', #16426, #86392, #94469 ) ;
#93473 = DIRECTION ( 'NONE',  ( -0.8660254037844387076, -0.4999999999999998890, -0.000000000000000000 ) ) ;
#93474 = CARTESIAN_POINT ( 'NONE',  ( 160.0061168334508750, 253.5082714530983026, -16.02306982074888708 ) ) ;
#93475 = DIRECTION ( 'NONE',  ( 0.000000000000000000, 0.000000000000000000, 1.000000000000000000 ) ) ;
#93476 = CARTESIAN_POINT ( 'NONE',  ( 79.68797162431192760, 46.35385572848484514, -12.62015847980756611 ) ) ;
#93477 = CARTESIAN_POINT ( 'NONE',  ( 200.7523954295751594, 282.9336467052548869, 18.23634913067694185 ) ) ;
#93478 = VERTEX_POINT ( 'NONE', #74840 ) ;
#93479 = CARTESIAN_POINT ( 'NONE',  ( 155.1126062595885458, 261.9840803944032359, -18.37531408727430104 ) ) ;
#93480 = CARTESIAN_POINT ( 'NONE',  ( 134.1658515176688411, 248.2677522451418497, 10.00000000000009592 ) ) ;
#93481 = CARTESIAN_POINT ( 'NONE',  ( 179.9645220515723167, 295.2954571389396392, -0.1274745643057336175 ) ) ;
#93482 = CARTESIAN_POINT ( 'NONE',  ( 25.04665064082957926, 175.2677522451417929, -5.000000000000041744 ) ) ;
#93483 = CARTESIAN_POINT ( 'NONE',  ( 90.02596631606968458, 210.5327760586659451, 1.948934522072302763E-15 ) ) ;
#93484 = CARTESIAN_POINT ( 'NONE',  ( 196.4287751515431921, 269.1031666285815618, -12.09581130873691279 ) ) ;
#93485 = CARTESIAN_POINT ( 'NONE',  ( 174.5193869908134445, 282.4549705599221170, -14.99235812395697920 ) ) ;
#93486 = CARTESIAN_POINT ( 'NONE',  ( 166.9537089176444624, 278.1996852497881605, -13.41525378165041182 ) ) ;
#93487 = CARTESIAN_POINT ( 'NONE',  ( 1.754175721758462148, 178.4865022471903728, -10.00000000000009592 ) ) ;
#93489 = CARTESIAN_POINT ( 'NONE',  ( 48.16808589598787904, 104.3116767361652535, 10.00000000000000000 ) ) ;
#93488 = CARTESIAN_POINT ( 'NONE',  ( 9.512059640396367755, 185.4869531367911293, 4.594050593750046652 ) ) ;
#93490 = CARTESIAN_POINT ( 'NONE',  ( 200.2316334480823912, 283.8356329158505105, 17.02791935830326508 ) ) ;
#93491 = VERTEX_POINT ( 'NONE', #98129 ) ;
#93492 = ORIENTED_EDGE ( 'NONE', *, *, #60881, .T. ) ;
#93493 = PLANE ( 'NONE',  #19380 ) ;
#93494 = CARTESIAN_POINT ( 'NONE',  ( 200.9031254216535842, 267.7938560626140543, -2.960348916509118578 ) ) ;
#93495 = PRODUCT_RELATED_PRODUCT_CATEGORY ( 'part', '', ( #29009 ) ) ;
#93496 = CARTESIAN_POINT ( 'NONE',  ( 81.94645434516804983, 46.66819754834421730, -11.94275014213957675 ) ) ;
#93497 = CARTESIAN_POINT ( 'NONE',  ( 161.1061647010182583, 251.6029326557136585, -13.56144933775657613 ) ) ;
#93498 = CARTESIAN_POINT ( 'NONE',  ( 82.81707834093893439, 43.43219480169420876, 7.813715050472316292 ) ) ;
#93499 = CARTESIAN_POINT ( 'NONE',  ( 74.46912172204532965, 68.18838830983000321, -11.53105533885364231 ) ) ;
#93500 = CARTESIAN_POINT ( 'NONE',  ( 33.19304919271588972, 177.7202760586659451, -5.415160957724236172E-17 ) ) ;
#93501 = AXIS2_PLACEMENT_3D ( 'NONE', #43477, #26799, #27303 ) ;
#93502 = CARTESIAN_POINT ( 'NONE',  ( 196.1313296246206619, 275.4698387032307778, 15.47109719661084704 ) ) ;
#93503 = ORIENTED_EDGE ( 'NONE', *, *, #74823, .T. ) ;
#93504 = CARTESIAN_POINT ( 'NONE',  ( 153.3327503926682596, 274.2549037607562354, -12.22769268488517902 ) ) ;
#93505 = CARTESIAN_POINT ( 'NONE',  ( 182.5206069704653089, 260.8428654270882134, -10.69627834319913795 ) ) ;
#93507 = EDGE_CURVE ( 'NONE', #53063, #83615, #35029, .T. ) ;
#93506 = AXIS2_PLACEMENT_3D ( 'NONE', #4468, #81027, #97207 ) ;
#93508 = CARTESIAN_POINT ( 'NONE',  ( -16.57695564860984661, 170.4244531367911293, -4.594050593750046652 ) ) ;
#93509 = CARTESIAN_POINT ( 'NONE',  ( 196.0051728737935832, 265.8263463907475170, 8.406970388261065352 ) ) ;
#93510 = AXIS2_PLACEMENT_3D ( 'NONE', #88495, #4326, #43312 ) ;
#93511 = CARTESIAN_POINT ( 'NONE',  ( 194.2199708651012600, 294.2481379475345875, 15.50834247347371253 ) ) ;
#93512 = CARTESIAN_POINT ( 'NONE',  ( 161.2133744761260061, 251.4172398781588811, -14.30368667312104058 ) ) ;
#93513 = FACE_OUTER_BOUND ( 'NONE', #65762, .T. ) ;
#93514 = CARTESIAN_POINT ( 'NONE',  ( 194.9455394410084921, 292.9914163096879065, -15.01116663483170655 ) ) ;
#93515 = CARTESIAN_POINT ( 'NONE',  ( 189.3832291599495079, 300.6256203239445313, 1.753828516883770838 ) ) ;
#93516 = CARTESIAN_POINT ( 'NONE',  ( 84.13204908911602331, 50.42604040346918737, 13.71367173376235371 ) ) ;
#93517 = CARTESIAN_POINT ( 'NONE',  ( 193.0126352936363503, 264.4189281174865869, 8.906082567666748773 ) ) ;
#93518 = CARTESIAN_POINT ( 'NONE',  ( 71.88630063891508826, 72.11467658586039420, 1.680795692104123162 ) ) ;
#93519 = CARTESIAN_POINT ( 'NONE',  ( 75.87525401958798454, 64.72722897157592570, -14.29033900848947169 ) ) ;
#93520 = CARTESIAN_POINT ( 'NONE',  ( 181.4735074999749145, 292.1586133693310785, 10.55809797880889001 ) ) ;
#93521 = VECTOR ( 'NONE', #5020, 1000.000000000000000 ) ;
#93522 = CARTESIAN_POINT ( 'NONE',  ( 173.9008529106967558, 272.4049662731551962, -17.79092985220220058 ) ) ;
#93523 = EDGE_CURVE ( 'NONE', #86318, #82867, #73810, .T. ) ;
#93524 = CARTESIAN_POINT ( 'NONE',  ( 114.2743305262689404, 236.7833772461660544, -9.188101187500095079 ) ) ;
#93525 = CARTESIAN_POINT ( 'NONE',  ( 15.46199490364264406, 17.43085787977761925, -9.188101187500008038 ) ) ;
#93526 = CARTESIAN_POINT ( 'NONE',  ( 150.8888667059421209, 269.2998118992572927, 15.79021133717968617 ) ) ;
#93527 = CARTESIAN_POINT ( 'NONE',  ( 71.88281838930642209, 59.56282477439597045, -15.74156321294393024 ) ) ;
#93528 = VECTOR ( 'NONE', #45042, 1000.000000000000114 ) ;
#93530 = CARTESIAN_POINT ( 'NONE',  ( 86.98157820904661719, 43.44862423325045597, 0.06000229279370256075 ) ) ;
#93529 = DIRECTION ( 'NONE',  ( 0.8660254037844378194, 0.5000000000000015543, -0.000000000000000000 ) ) ;
#93531 = CARTESIAN_POINT ( 'NONE',  ( 151.0170062819612440, 269.0778676431315830, -14.83004665419763946 ) ) ;
#93532 = CARTESIAN_POINT ( 'NONE',  ( 190.8403443996919293, 262.5132785920529273, -4.370171634604190558 ) ) ;
#93533 = CARTESIAN_POINT ( 'NONE',  ( -19.65312891409030271, 93.06504152958497400, -10.00000000000000888 ) ) ;
#93534 = DIRECTION ( 'NONE',  ( -0.9404163354663408469, -0.3400251696390412803, 0.000000000000000000 ) ) ;
#93535 = CARTESIAN_POINT ( 'NONE',  ( 43.82855288972071151, 25.70852965304483462, 1.583844403245364907 ) ) ;
#93536 = CARTESIAN_POINT ( 'NONE',  ( 86.26520568890161655, 47.67615905960597900, 10.76369269717137733 ) ) ;
#93537 = ORIENTED_EDGE ( 'NONE', *, *, #18318, .T. ) ;
#93538 = CARTESIAN_POINT ( 'NONE',  ( 191.8538237116409846, 266.9476526621388643, 10.93440350035595365 ) ) ;
#93539 = CARTESIAN_POINT ( 'NONE',  ( 68.91022223105564137, 64.71151235087043574, -12.22836756590942464 ) ) ;
#93540 = CARTESIAN_POINT ( 'NONE',  ( 200.4850423784957343, 269.2554961546323398, 9.006584850389378616 ) ) ;
#93541 = B_SPLINE_CURVE_WITH_KNOTS ( 'NONE', 3,
 ( #97507, #28078, #58949, #39642, #62966, #15347, #22959, #70055, #85314, #54862, #69567, #70563, #85841, #47262, #23451, #84807, #15860, #7771, #16370, #46767, #77693, #71092, #54343, #53847, #8276, #47751, #92899, #38145, #86327, #39143, #671, #46243, #78184, #55349, #175, #31554, #14863, #77168, #62443, #38664, #61461, #93916, #93411, #31058, #24469, #55838, #61948, #16865, #23960, #8772, #1180, #32055 ),
 .UNSPECIFIED., .F., .F.,
 ( 4, 2, 2, 2, 2, 2, 2, 2, 2, 2, 2, 2, 2, 2, 2, 2, 2, 2, 2, 2, 2, 2, 2, 2, 2, 4 ),
 ( 0.0001062343114664006984, 0.001128839385260167923, 0.001384490653708566167, 0.001640141922156964412, 0.001767967556381141525, 0.001895793190605319072, 0.002023618824829496402, 0.002151444459053673732, 0.002407095727502028826, 0.002662746995950384787, 0.003174049532847176506, 0.004196654606640761245, 0.005219259680434346418, 0.005730562217331175434, 0.005986213485779591677, 0.006114039120003762935, 0.006241864754227933326, 0.006305777571339981659, 0.006369690388452029124, 0.006497516022676135330, 0.006753167291124355549, 0.007008818559572576636, 0.007264469828020798589, 0.007520121096469019675, 0.007775772364917239894, 0.008287074901813495584 ),
 .UNSPECIFIED. ) ;
#93542 = CARTESIAN_POINT ( 'NONE',  ( 78.98404269576303705, 49.35947893415648480, 14.50012733305994139 ) ) ;
#93543 = CARTESIAN_POINT ( 'NONE',  ( 180.3992865667702574, 261.8415815662849013, -12.99249967246676718 ) ) ;
#93544 = CARTESIAN_POINT ( 'NONE',  ( 168.8668831836475590, 259.3240382218725131, -16.04453771237437110 ) ) ;
#93545 = DIRECTION ( 'NONE',  ( -0.9042435392811322137, -0.4270171210482451296, 0.000000000000000000 ) ) ;
#93546 = ORIENTED_EDGE ( 'NONE', *, *, #19671, .T. ) ;
#93547 = CARTESIAN_POINT ( 'NONE',  ( 73.13555747811004437, 69.81939941050913490, 9.605153593488003239 ) ) ;
#93548 = CARTESIAN_POINT ( 'NONE',  ( 42.37730965384162829, 25.26216523072498532, -2.296566073217252530E-15 ) ) ;
#93549 = ORIENTED_EDGE ( 'NONE', *, *, #51096, .F. ) ;
#93550 = CARTESIAN_POINT ( 'NONE',  ( 167.4359517046813437, 249.7873561267534512, 6.955981803495778770 ) ) ;
#93551 = CARTESIAN_POINT ( 'NONE',  ( 148.5272680744187141, 275.3902207161408455, -7.185975151065171929 ) ) ;
#93552 = CARTESIAN_POINT ( 'NONE',  ( 80.96157657440146238, 44.13459223731847914, -10.82752981140125925 ) ) ;
#93553 = ORIENTED_EDGE ( 'NONE', *, *, #16780, .T. ) ;
#93554 = CARTESIAN_POINT ( 'NONE',  ( 79.41525598906244454, 59.66657864593240390, 16.17364996136696931 ) ) ;
#93555 = CARTESIAN_POINT ( 'NONE',  ( 159.1045919238213457, 255.0697584008655383, 17.12809966849329513 ) ) ;
#93556 = DIRECTION ( 'NONE',  ( -0.8660254037844387076, -0.4999999999999998890, -0.000000000000000000 ) ) ;
#93557 = CARTESIAN_POINT ( 'NONE',  ( 88.33748333995926316, 44.07075497373335793, -2.898134731201833070 ) ) ;
#93558 = CARTESIAN_POINT ( 'NONE',  ( 83.42026165063415988, 45.10053359704732401, -10.33714611788759896 ) ) ;
#93559 = FACE_OUTER_BOUND ( 'NONE', #56629, .T. ) ;
#93560 = ORIENTED_EDGE ( 'NONE', *, *, #88565, .T. ) ;
#93561 = EDGE_LOOP ( 'NONE', ( #50191, #36191, #58715, #54899 ) ) ;
#93562 = CARTESIAN_POINT ( 'NONE',  ( 167.6502826215564994, 287.3877002845107995, 4.891367078714356609 ) ) ;
#93563 = ORIENTED_EDGE ( 'NONE', *, *, #36832, .F. ) ;
#93564 = CARTESIAN_POINT ( 'NONE',  ( 77.18698849263780914, 49.25976772916404656, -14.85955674287117922 ) ) ;
#93565 = ORIENTED_EDGE ( 'NONE', *, *, #19237, .F. ) ;
#93566 = CARTESIAN_POINT ( 'NONE',  ( 170.9560043375414864, 269.9813116362016103, 16.58206790160089383 ) ) ;
#93567 = CARTESIAN_POINT ( 'NONE',  ( 78.33316717312801813, 49.42570397860901465, 14.68581309318566497 ) ) ;
#93568 = VERTEX_POINT ( 'NONE', #16989 ) ;
#93569 = CARTESIAN_POINT ( 'NONE',  ( 3.434913740874227628, 106.3949291714904462, 36.50000000000000000 ) ) ;
#93570 = CARTESIAN_POINT ( 'NONE',  ( 206.6672608846700427, 272.6887992170966299, -10.88770374553082121 ) ) ;
#93571 = CARTESIAN_POINT ( 'NONE',  ( 147.9415534642045884, 274.4047081797672263, -6.588256216760665751 ) ) ;
#93572 = CARTESIAN_POINT ( 'NONE',  ( 148.9230895364621574, 272.7046378331555161, 12.20434325797056019 ) ) ;
#93573 = CARTESIAN_POINT ( 'NONE',  ( 82.75615910393362640, 40.58425042732405785, 0.9307152221985128815 ) ) ;
#93574 = VECTOR ( 'NONE', #97608, 1000.000000000000000 ) ;
#93575 = CARTESIAN_POINT ( 'NONE',  ( -61.39381520214497101, 38.43978098112751951, -10.00000000000000000 ) ) ;
#93576 = EDGE_CURVE ( 'NONE', #64387, #48406, #84445, .T. ) ;
#93577 = LINE ( 'NONE', #55029, #92216 ) ;
#93578 = CARTESIAN_POINT ( 'NONE',  ( 157.9640733854634789, 281.0222844342897588, 2.394995417900620982 ) ) ;
#93579 = CARTESIAN_POINT ( 'NONE',  ( 124.5040820605901217, 248.8149278399161233, -9.188101187500095079 ) ) ;
#93580 = CARTESIAN_POINT ( 'NONE',  ( 70.64661241052995422, 60.59469274283073048, -14.62924882204517729 ) ) ;
#93581 = CARTESIAN_POINT ( 'NONE',  ( 38.84587710395076954, 34.37878583063844218, 9.188101187500006262 ) ) ;
#93582 = ORIENTED_EDGE ( 'NONE', *, *, #75984, .F. ) ;
#93583 = AXIS2_PLACEMENT_3D ( 'NONE', #40458, #87654, #9596 ) ;
#93584 = CARTESIAN_POINT ( 'NONE',  ( 28.83231091828818649, 21.81029122506295792, 8.090169943749479842 ) ) ;
#93585 = CARTESIAN_POINT ( 'NONE',  ( -47.54945751754587491, 75.00082604429731248, -10.00000000000000000 ) ) ;
#93586 = FACE_OUTER_BOUND ( 'NONE', #71096, .T. ) ;
#93587 = CARTESIAN_POINT ( 'NONE',  ( 173.3788830315178870, 289.3113284895608217, -4.680553739743101183 ) ) ;
#93588 = CARTESIAN_POINT ( 'NONE',  ( 192.2557068912079501, 297.6503429497950037, 11.10070071572538275 ) ) ;
#93589 = FACE_BOUND ( 'NONE', #33448, .T. ) ;
#93590 = DIRECTION ( 'NONE',  ( 0.000000000000000000, 0.000000000000000000, 1.000000000000000000 ) ) ;
#93591 = CARTESIAN_POINT ( 'NONE',  ( 173.3932497502476906, 287.2264128176810800, -9.697408833419370211 ) ) ;
#93593 = CARTESIAN_POINT ( 'NONE',  ( 173.8830265265375772, 282.0958691128189457, 14.99492924356757584 ) ) ;
#93592 = B_SPLINE_CURVE_WITH_KNOTS ( 'NONE', 3,
 ( #34838, #28243, #80503, #12064, #89126, #97676, #97192, #72888, #88617, #57641, #65251, #19185, #3955, #81013, #81993, #12566, #73861, #50539, #4448, #41442, #43441, #11077, #42921, #3480 ),
 .UNSPECIFIED., .F., .F.,
 ( 4, 2, 2, 2, 2, 2, 2, 2, 2, 2, 2, 4 ),
 ( 0.000000000000000000, 0.1249999999999925060, 0.2499999999999850120, 0.3749999999999775180, 0.4374999999999797384, 0.4999999999999820144, 0.5624999999999842348, 0.6249999999999864553, 0.6874999999999887867, 0.7499999999999910072, 0.8749999999999954481, 1.000000000000000000 ),
 .UNSPECIFIED. ) ;
#93594 = CARTESIAN_POINT ( 'NONE',  ( 194.5253693406981483, 291.7191722712467481, 16.18900132190417551 ) ) ;
#93595 = AXIS2_PLACEMENT_3D ( 'NONE', #32906, #89183, #96755 ) ;
#93596 = ORIENTED_EDGE ( 'NONE', *, *, #8317, .F. ) ;
#93597 = CARTESIAN_POINT ( 'NONE',  ( 148.0637215040603394, 274.1931069276759558, -7.795633835291665648 ) ) ;
#93598 = CARTESIAN_POINT ( 'NONE',  ( 4.262040950002970341, 183.2677522451419065, -5.000000000000047962 ) ) ;
#93599 = VERTEX_POINT ( 'NONE', #78820 ) ;
#93600 = CARTESIAN_POINT ( 'NONE',  ( 188.0563983182514960, 266.0109151943670440, -11.70562387175789532 ) ) ;
#93601 = CARTESIAN_POINT ( 'NONE',  ( -70.89022602266993545, 47.22876919346843749, 10.00000000000000000 ) ) ;
#93602 = CARTESIAN_POINT ( 'NONE',  ( 152.4236611112960986, 266.6414700100113464, -15.70435633784547669 ) ) ;
#93603 = CARTESIAN_POINT ( 'NONE',  ( -70.92467617367974242, 45.40763453331954480, 177.5919119679930134 ) ) ;
#93605 = CARTESIAN_POINT ( 'NONE',  ( 154.8984264370756136, 277.3990238811145446, -8.847142293553330816 ) ) ;
#93604 = CARTESIAN_POINT ( 'NONE',  ( 153.4476745504623239, 270.0653357872154174, 15.15442168775317278 ) ) ;
#93606 = CARTESIAN_POINT ( 'NONE',  ( 152.7295469705997277, 266.1116601603806657, -17.40211458100010589 ) ) ;
#93607 = ORIENTED_EDGE ( 'NONE', *, *, #27443, .F. ) ;
#93608 = CARTESIAN_POINT ( 'NONE',  ( 146.8195026170398023, 276.3481572557323034, 4.765869558735466249 ) ) ;
#93610 = DIRECTION ( 'NONE',  ( -0.000000000000000000, -0.000000000000000000, -1.000000000000000000 ) ) ;
#93609 = B_SPLINE_SURFACE_WITH_KNOTS ( 'NONE', 3, 1, ( 
 ( #702, #23997 ),
 ( #39176, #32090 ),
 ( #77725, #31586 ),
 ( #16894, #54895 ),
 ( #46280, #85875 ),
 ( #63003, #93947 ),
 ( #47294, #24501 ),
 ( #9308, #22994 ),
 ( #47785, #71122 ),
 ( #31092, #38696 ),
 ( #60993, #61979 ),
 ( #92933, #22508 ),
 ( #53402, #84351 ),
 ( #45787, #23485 ),
 ( #38183, #54375 ),
 ( #40688, #96446 ),
 ( #71628, #17921 ),
 ( #72122, #34119 ),
 ( #2223, #10316 ),
 ( #49802, #42193 ),
 ( #65012, #80763 ),
 ( #73128, #27013 ),
 ( #64001, #11822 ),
 ( #63502, #33104 ),
 ( #48819, #95956 ),
 ( #3721, #72635 ),
 ( #94942, #11334 ),
 ( #34599, #10816 ),
 ( #57897, #2727 ),
 ( #25506, #94440 ),
 ( #65498, #88877 ),
 ( #79752, #24994 ),
 ( #41692, #41185 ),
 ( #1726, #50294 ) ),
 .UNSPECIFIED., .T., .F., .F.,
 ( 4, 2, 2, 2, 2, 2, 2, 2, 2, 2, 2, 2, 2, 2, 2, 2, 4 ),
 ( 2, 2 ),
 ( 0.000000000000000000, 0.06250000000000000000, 0.1250000000000000000, 0.1875000000000000000, 0.2500000000000000000, 0.3125000000000000000, 0.3750000000000000000, 0.4375000000000000000, 0.5000000000000000000, 0.5625000000000000000, 0.6250000000000000000, 0.6875000000000000000, 0.7500000000000000000, 0.8125000000000000000, 0.8750000000000000000, 0.9375000000000000000, 1.000000000000000000 ),
 ( 0.000000000000000000, 1.000000000000000000 ),
 .UNSPECIFIED. ) ;
#93611 = CARTESIAN_POINT ( 'NONE',  ( 72.89767165371587510, 62.52605430883413362, 14.90584116256920133 ) ) ;
#93612 = CARTESIAN_POINT ( 'NONE',  ( 190.7945136500361230, 274.8346541966113818, -15.71499985172781066 ) ) ;
#93613 = CARTESIAN_POINT ( 'NONE',  ( 39.80235952159635815, 84.99999999999998579, -59.99999999999999289 ) ) ;
#93614 = CARTESIAN_POINT ( 'NONE',  ( 184.6334634352423905, 296.8755821276896540, -4.397454188638743489 ) ) ;
#93615 = CARTESIAN_POINT ( 'NONE',  ( 198.1679321590325458, 277.6257778925182720, -16.56331389466651061 ) ) ;
#93616 = CARTESIAN_POINT ( 'NONE',  ( 73.85129109314340212, 68.53037146055885387, 11.40305250113367741 ) ) ;
#93617 = CARTESIAN_POINT ( 'NONE',  ( 154.9910882912764123, 262.1945556895526579, 18.38052604520346023 ) ) ;
#93618 = FACE_OUTER_BOUND ( 'NONE', #83112, .T. ) ;
#93619 = AXIS2_PLACEMENT_3D ( 'NONE', #79183, #26938, #88801 ) ;
#93620 = CARTESIAN_POINT ( 'NONE',  ( -5.751638101304356709, 176.6744531367911293, 4.594050593750047540 ) ) ;
#93621 = CARTESIAN_POINT ( 'NONE',  ( 89.61940949045693117, 231.7369531367911009, -4.594050593750048428 ) ) ;
#93622 = CARTESIAN_POINT ( 'NONE',  ( 203.3349860717029571, 278.4604684979374838, -16.59553970625579566 ) ) ;
#93623 = CARTESIAN_POINT ( 'NONE',  ( 192.7705129102570822, 296.7586727687594816, -13.39629674907774692 ) ) ;
#93624 = CARTESIAN_POINT ( 'NONE',  ( 183.0282842160764574, 294.7209337947608674, -8.144370267713933131 ) ) ;
#93625 = CARTESIAN_POINT ( 'NONE',  ( 78.14015596324891533, 47.79605781560270117, 14.53813849190288465 ) ) ;
#93627 = EDGE_CURVE ( 'NONE', #57243, #45703, #77403, .T. ) ;
#93626 = CIRCLE ( 'NONE', #24020, 16.60714546451156082 ) ;
#93628 = CARTESIAN_POINT ( 'NONE',  ( 77.89337869297911254, 54.04621959010322740, 15.98457785149147092 ) ) ;
#93629 = CARTESIAN_POINT ( 'NONE',  ( 202.0661878422603763, 279.1895584290143120, -16.02388874507808225 ) ) ;
#93630 = DIRECTION ( 'NONE',  ( 0.5000000000000012212, -0.8660254037844380415, -0.000000000000000000 ) ) ;
#93632 = CARTESIAN_POINT ( 'NONE',  ( 76.45858476847112684, 51.15202837745678721, 16.04606878625051536 ) ) ;
#93631 = CARTESIAN_POINT ( 'NONE',  ( 23.64814127513154673, 118.0650415295851019, 20.00000000000000355 ) ) ;
#93633 = CARTESIAN_POINT ( 'NONE',  ( 161.5907339951948245, 250.7636340184123469, 12.67682986482127028 ) ) ;
#93634 = CARTESIAN_POINT ( 'NONE',  ( 166.0167935002967283, 249.2348392641485191, -9.295598770875054484 ) ) ;
#93635 = CARTESIAN_POINT ( 'NONE',  ( 204.8371018956013074, 275.8587275720924481, -12.67884532777024198 ) ) ;
#93636 = CARTESIAN_POINT ( 'NONE',  ( 196.0727848089514964, 291.0389700598140621, 17.56388901715066808 ) ) ;
#93637 = CARTESIAN_POINT ( 'NONE',  ( -73.83803415018344651, 50.74234351129840093, -10.00000000000000000 ) ) ;
#93638 = EDGE_CURVE ( 'NONE', #44012, #16902, #95975, .T. ) ;
#93639 = CARTESIAN_POINT ( 'NONE',  ( 207.6357208050208101, 271.0113774299547913, -6.790259683043212036 ) ) ;
#93640 = B_SPLINE_CURVE_WITH_KNOTS ( 'NONE', 3,
 ( #39072, #49211, #80143, #10708 ),
 .UNSPECIFIED., .F., .F.,
 ( 4, 4 ),
 ( 0.008487571838833373600, 0.009484744147854903482 ),
 .UNSPECIFIED. ) ;
#93641 = CARTESIAN_POINT ( 'NONE',  ( 31.29809797828990270, 195.0024278399160664, -9.188101187500093303 ) ) ;
#93642 = CIRCLE ( 'NONE', #20812, 60.00000000000002132 ) ;
#93643 = EDGE_CURVE ( 'NONE', #64147, #31573, #45968, .T. ) ;
#93644 = CARTESIAN_POINT ( 'NONE',  ( 67.50895872190925218, 209.7833772461660544, -9.188101187500095079 ) ) ;
#93645 = CARTESIAN_POINT ( 'NONE',  ( 190.8429499865819707, 278.0757709512191695, -17.64141544901220371 ) ) ;
#93646 = CARTESIAN_POINT ( 'NONE',  ( 88.50685567279400345, 43.87431988399859506, -0.03150979628302791324 ) ) ;
#93647 = CARTESIAN_POINT ( 'NONE',  ( 107.5017976953482446, 221.3262482093458061, 3.021315404115420679E-15 ) ) ;
#93648 = CARTESIAN_POINT ( 'NONE',  ( 140.9585647324944659, 258.3149278399160380, 9.188101187500093303 ) ) ;
#93650 = DIRECTION ( 'NONE',  ( -0.000000000000000000, 0.000000000000000000, 1.000000000000000000 ) ) ;
#93649 = CARTESIAN_POINT ( 'NONE',  ( 71.87942950353104266, 72.15877716270880171, -3.647418342425857052 ) ) ;
#93651 = VECTOR ( 'NONE', #92836, 1000.000000000000000 ) ;
#93652 = CARTESIAN_POINT ( 'NONE',  ( 198.1689325269066444, 270.4971866185222780, -10.92086016236654444 ) ) ;
#93653 = CARTESIAN_POINT ( 'NONE',  ( 24.06271987006732616, 35.93396525600390845, 2.839279412974139660 ) ) ;
#93654 = CARTESIAN_POINT ( 'NONE',  ( 198.8194531333411419, 286.2816009704309863, -17.01510935557533344 ) ) ;
#93655 = CARTESIAN_POINT ( 'NONE',  ( 149.2223635749290622, 272.1862799931444670, -12.97307652490353647 ) ) ;
#93656 = CARTESIAN_POINT ( 'NONE',  ( 16.72130706672765754, 10.44966523072493203, -2.296566073217252530E-15 ) ) ;
#93657 = CARTESIAN_POINT ( 'NONE',  ( 67.18419919549008057, 209.5958772461660544, -9.188101187500095079 ) ) ;
#93658 = CARTESIAN_POINT ( 'NONE',  ( 158.7800074345649648, 256.0125694611146514, -16.06375889119701483 ) ) ;
#93659 = CARTESIAN_POINT ( 'NONE',  ( 202.7676489560256528, 279.4431252073101746, -16.04062356091568020 ) ) ;
#93660 = VECTOR ( 'NONE', #96820, 999.9999999999998863 ) ;
#93661 = CARTESIAN_POINT ( 'NONE',  ( 159.3528137482544196, 254.6398255893999476, 16.73628156321660398 ) ) ;
#93662 = CARTESIAN_POINT ( 'NONE',  ( 74.31686216695912606, 67.90482052775791999, 11.67503013858854466 ) ) ;
#93663 = LINE ( 'NONE', #24227, #88241 ) ;
#93664 = CARTESIAN_POINT ( 'NONE',  ( 82.21393801928418554, 54.22668391568882384, -15.61295444237038232 ) ) ;
#93665 = VECTOR ( 'NONE', #41663, 1000.000000000000000 ) ;
#93666 = CARTESIAN_POINT ( 'NONE',  ( 118.6676052326577633, 225.9865022471901455, 1.119607411625061291E-15 ) ) ;
#93667 = CARTESIAN_POINT ( 'NONE',  ( -0.1936345643149539608, 38.48607693945955077, 59.99999999999999289 ) ) ;
#93668 = CARTESIAN_POINT ( 'NONE',  ( 207.6860335175200589, 270.9242332556395922, 6.913225035677485586 ) ) ;
#93669 = ORIENTED_EDGE ( 'NONE', *, *, #96063, .F. ) ;
#93670 = CARTESIAN_POINT ( 'NONE',  ( 77.10732452059650655, 49.39774977627229191, 15.43680315855346663 ) ) ;
#93671 = CARTESIAN_POINT ( 'NONE',  ( 185.4348243712239821, 271.7623222876268301, 15.85896177974588639 ) ) ;
#93672 = ORIENTED_EDGE ( 'NONE', *, *, #12122, .F. ) ;
#93673 = CARTESIAN_POINT ( 'NONE',  ( 159.2651917302844993, 254.7915913763855258, -16.53922207549818424 ) ) ;
#93674 = CARTESIAN_POINT ( 'NONE',  ( 193.9893413146322132, 294.1401140054277334, 13.97219244730923471 ) ) ;
#93675 = CARTESIAN_POINT ( 'NONE',  ( 68.54420489956650897, 68.75802437611594087, -6.174013142999687176 ) ) ;
#93676 = EDGE_LOOP ( 'NONE', ( #2756, #76640, #7274, #49666 ) ) ;
#93677 = CARTESIAN_POINT ( 'NONE',  ( 173.7058431582960054, 250.9251529220507564, 0.5223538383735283341 ) ) ;
#93678 = ORIENTED_EDGE ( 'NONE', *, *, #38121, .F. ) ;
#93679 = DIRECTION ( 'NONE',  ( 0.000000000000000000, -0.000000000000000000, -1.000000000000000000 ) ) ;
#93680 = CARTESIAN_POINT ( 'NONE',  ( 148.4083960970861256, 273.5961130204771052, -8.574185186226726429 ) ) ;
#93681 = CARTESIAN_POINT ( 'NONE',  ( 148.4820959031164023, 274.3664125831473939, 7.729347682778947792 ) ) ;
#93682 = CONICAL_SURFACE ( 'NONE', #25688, 16.60714546451156082, 0.7853981633974407295 ) ;
#93683 = VERTEX_POINT ( 'NONE', #18516 ) ;
#93684 = CARTESIAN_POINT ( 'NONE',  ( 24.44940106416278169, 29.51421378149920116, -9.188101187500004485 ) ) ;
#93685 = CARTESIAN_POINT ( 'NONE',  ( 79.74649121193665735, 44.83324031607526194, 11.42014051431522681 ) ) ;
#93686 = CYLINDRICAL_SURFACE ( 'NONE', #66228, 70.00000000000002842 ) ;
#93687 = CARTESIAN_POINT ( 'NONE',  ( 74.87331927037789114, 66.80950769484921636, -13.20416362156882961 ) ) ;
#93688 = EDGE_CURVE ( 'NONE', #29382, #73834, #82298, .T. ) ;
#93689 = ORIENTED_EDGE ( 'NONE', *, *, #43755, .F. ) ;
#93690 = LINE ( 'NONE', #16148, #93528 ) ;
#93691 = CARTESIAN_POINT ( 'NONE',  ( 206.7408728089182546, 272.5612996242556960, -10.63134519248043475 ) ) ;
#93692 = ORIENTED_EDGE ( 'NONE', *, *, #14645, .T. ) ;
#93693 = CARTESIAN_POINT ( 'NONE',  ( -19.65312891409030271, 93.06504152958497400, 177.5919119679930134 ) ) ;
#93695 = CARTESIAN_POINT ( 'NONE',  ( 67.93406655831707042, 65.27944798580912789, -10.53696878470477571 ) ) ;
#93694 = CARTESIAN_POINT ( 'NONE',  ( 67.93934924601143166, 65.44133490301047118, 10.37202260051014058 ) ) ;
#93696 = CARTESIAN_POINT ( 'NONE',  ( 81.47677896408023912, 55.16251862595696309, -15.92532667734195329 ) ) ;
#93697 = CARTESIAN_POINT ( 'NONE',  ( 178.0302064638906074, 292.4640037680099454, 7.106335582765731296 ) ) ;
#93698 = CARTESIAN_POINT ( 'NONE',  ( 32.98506340464172837, 40.81751292744058901, -6.180339887498951690 ) ) ;
#93699 = CARTESIAN_POINT ( 'NONE',  ( 204.7764732025852084, 275.9637395487929439, -14.02287343454361412 ) ) ;
#93700 = CARTESIAN_POINT ( 'NONE',  ( 207.9607810208533749, 270.4483566206134242, -3.700399523436301408 ) ) ;
#93701 = EDGE_CURVE ( 'NONE', #79632, #96562, #86967, .T. ) ;
#93702 = CARTESIAN_POINT ( 'NONE',  ( 206.4545408510063567, 270.6145640749817289, 2.451115620848321797 ) ) ;
#93703 = CARTESIAN_POINT ( 'NONE',  ( 180.7872516664550915, 259.6763394889495089, 9.523190573527278602 ) ) ;
#93704 = CARTESIAN_POINT ( 'NONE',  ( 91.51436070488293240, 214.4548013555409796, -4.594050593750042211 ) ) ;
#93705 = ORIENTED_EDGE ( 'NONE', *, *, #23458, .F. ) ;
#93706 = CARTESIAN_POINT ( 'NONE',  ( 150.6931560952953646, 269.6387926204777727, 14.65021044537114037 ) ) ;
#93707 = CARTESIAN_POINT ( 'NONE',  ( 156.6168467568483891, 276.9391697405689001, 11.51099842983860633 ) ) ;
#93708 = CARTESIAN_POINT ( 'NONE',  ( -110.0000000000000142, 10.00000000000000178, 14.21260523776214590 ) ) ;
#93709 = EDGE_LOOP ( 'NONE', ( #2462, #35877, #31184, #51523 ) ) ;
#93710 = CARTESIAN_POINT ( 'NONE',  ( 156.9736299494965408, 258.7606928093932197, -16.87440706565485016 ) ) ;
#93711 = VERTEX_POINT ( 'NONE', #50889 ) ;
#93712 = ORIENTED_EDGE ( 'NONE', *, *, #46504, .T. ) ;
#93713 = EDGE_CURVE ( 'NONE', #42456, #48590, #95584, .T. ) ;
#93714 = CARTESIAN_POINT ( 'NONE',  ( 80.43640818173928153, 44.73695621425903113, -11.66065100600888549 ) ) ;
#93715 = EDGE_CURVE ( 'NONE', #1197, #39666, #76213, .T. ) ;
#93716 = CARTESIAN_POINT ( 'NONE',  ( 67.12382456020034738, 67.68358546754156180, 6.632048820649145249 ) ) ;
#93717 = CARTESIAN_POINT ( 'NONE',  ( 191.5324528500417216, 298.9030556958743432, -8.286652526617016790 ) ) ;
#93718 = CARTESIAN_POINT ( 'NONE',  ( 81.06903993398350394, 56.12834176912372186, 16.10816894976702685 ) ) ;
#93719 = CARTESIAN_POINT ( 'NONE',  ( 78.77411331422680973, 48.77619312070567759, -14.30298268893856140 ) ) ;
#93720 = CARTESIAN_POINT ( 'NONE',  ( 162.9529104326093716, 248.4042752199367214, 11.77079043123004176 ) ) ;
#93721 = CARTESIAN_POINT ( 'NONE',  ( 71.13526655237410523, 218.0024278399160664, 9.188101187500095079 ) ) ;
#93722 = B_SPLINE_CURVE_WITH_KNOTS ( 'NONE', 3,
 ( #92306, #52261, #5668, #91798, #22855, #38547, #84213, #45158, #44153, #44645, #60341, #6670, #68453, #76569, #7150, #84699 ),
 .UNSPECIFIED., .F., .F.,
 ( 4, 1, 2, 2, 2, 1, 2, 2, 4 ),
 ( 0.000000000000000000, 0.1250000000000017764, 0.1875000000000028033, 0.2500000000000038303, 0.5000000000000042188, 0.6250000000000029976, 0.6875000000000041078, 0.7500000000000052180, 1.000000000000000000 ),
 .UNSPECIFIED. ) ;
#93723 = ORIENTED_EDGE ( 'NONE', *, *, #13674, .F. ) ;
#93724 =( BOUNDED_CURVE ( )  B_SPLINE_CURVE ( 2, ( #59563, #6387, #52471, #14486, #36772, #6870, #76299, #37761, #37273 ),
 .UNSPECIFIED., .F., .T. ) 
 B_SPLINE_CURVE_WITH_KNOTS ( ( 3, 2, 2, 2, 3 ),
 ( 0.4798387096774193727, 0.4811827956989247479, 0.4838709677419354982, 0.4865591397849462485, 0.4879032258064516236 ),
 .UNSPECIFIED. ) 
 CURVE ( )  GEOMETRIC_REPRESENTATION_ITEM ( )  RATIONAL_B_SPLINE_CURVE ( ( 0.9330127018922194093, 0.9330127018922194093, 1.000000000000000000, 0.8660254037844387076, 1.000000000000000000, 0.8660254037844387076, 1.000000000000000000, 0.9330127018922194093, 0.9330127018922194093 ) ) 
 REPRESENTATION_ITEM ( '' )  );
#93725 = ORIENTED_EDGE ( 'NONE', *, *, #45931, .T. ) ;
#93726 = CARTESIAN_POINT ( 'NONE',  ( 201.0201945934902028, 282.4698049471293757, -18.03844186250218229 ) ) ;
#93727 = VECTOR ( 'NONE', #55416, 1000.000000000000000 ) ;
#93728 = VERTEX_POINT ( 'NONE', #37184 ) ;
#93729 = CARTESIAN_POINT ( 'NONE',  ( 15.09101445147005727, 32.21091486745859811, -1.111400068045478839E-16 ) ) ;
#93730 = VECTOR ( 'NONE', #65232, 1000.000000000000000 ) ;
#93731 = CARTESIAN_POINT ( 'NONE',  ( 184.2134048493523721, 275.2594305566963726, 16.37148162228643145 ) ) ;
#93732 = AXIS2_PLACEMENT_3D ( 'NONE', #1516, #79548, #79030 ) ;
#93733 = CARTESIAN_POINT ( 'NONE',  ( -30.31876249839593385, 93.46524241893469309, 44.28731163467956833 ) ) ;
#93734 = CARTESIAN_POINT ( 'NONE',  ( 207.4188537709976572, 270.9991043259717571, -1.591865268704130587 ) ) ;
#93735 = CARTESIAN_POINT ( 'NONE',  ( 87.73298548431469612, 44.18903561216111342, 4.633618514853093728 ) ) ;
#93736 = ORIENTED_EDGE ( 'NONE', *, *, #34950, .F. ) ;
#93737 = CARTESIAN_POINT ( 'NONE',  ( 82.53511752467487383, 43.65719814951889077, -8.367179187669531615 ) ) ;
#93738 = CARTESIAN_POINT ( 'NONE',  ( -26.53413439647355787, 34.79436034334068495, 59.99999999999999289 ) ) ;
#93739 = CARTESIAN_POINT ( 'NONE',  ( 206.1062572280473546, 273.6604860535989587, -9.773577984388410300 ) ) ;
#93740 = CARTESIAN_POINT ( 'NONE',  ( 147.7314489675487152, 275.2273187821839429, -4.041098034711884779 ) ) ;
#93741 = CARTESIAN_POINT ( 'NONE',  ( 175.6685219133858311, 284.7759717101654928, 14.09206119860363415 ) ) ;
#93742 = B_SPLINE_CURVE_WITH_KNOTS ( 'NONE', 3,
 ( #30163, #5876, #53452, #98091, #83407, #84403, #74805, #99579, #21100, #90018, #20590, #22066, #76760, #38239, #82440, #67672 ),
 .UNSPECIFIED., .F., .F.,
 ( 4, 1, 2, 2, 2, 1, 2, 2, 4 ),
 ( 0.000000000000000000, 0.1250000000000024980, 0.1875000000000030254, 0.2500000000000035527, 0.5000000000000019984, 0.6250000000000015543, 0.6875000000000027756, 0.7500000000000038858, 1.000000000000000000 ),
 .UNSPECIFIED. ) ;
#93743 = CARTESIAN_POINT ( 'NONE',  ( 198.9782931523127445, 285.5098555092977222, -17.06882919058305603 ) ) ;
#93744 = LINE ( 'NONE', #86657, #76153 ) ;
#93745 = VERTEX_POINT ( 'NONE', #6789 ) ;
#93746 = CARTESIAN_POINT ( 'NONE',  ( 21.15788363470973366, 37.74176219324819215, 10.00000000000000000 ) ) ;
#93747 = VECTOR ( 'NONE', #199, 1000.000000000000114 ) ;
#93748 = CARTESIAN_POINT ( 'NONE',  ( 161.3644539559160478, 251.1555625431813894, 12.97746593258196413 ) ) ;
#93749 = CARTESIAN_POINT ( 'NONE',  ( 86.49003203920455007, 46.12064888256469430, 8.834558565304289957 ) ) ;
#93750 = CARTESIAN_POINT ( 'NONE',  ( 187.0949703139557130, 265.6442697474142278, -11.84038648041589070 ) ) ;
#93751 = CARTESIAN_POINT ( 'NONE',  ( 83.71675958367757175, 52.25485864705834160, 14.69809135895772201 ) ) ;
#93752 = FACE_OUTER_BOUND ( 'NONE', #89719, .T. ) ;
#93753 = VERTEX_POINT ( 'NONE', #82354 ) ;
#93754 = CARTESIAN_POINT ( 'NONE',  ( -16.79610892523035659, 102.6363712329456916, 44.61266935656895072 ) ) ;
#93755 = VECTOR ( 'NONE', #52865, 1000.000000000000114 ) ;
#93756 = EDGE_CURVE ( 'NONE', #10181, #97433, #4815, .T. ) ;
#93757 = CARTESIAN_POINT ( 'NONE',  ( 207.6727254509676186, 270.9472835030587703, 7.315149605389819953 ) ) ;
#93759 = CARTESIAN_POINT ( 'NONE',  ( 73.67134723356205939, 55.40687185882725174, 16.58795594256350725 ) ) ;
#93758 = PLANE ( 'NONE',  #22448 ) ;
#93760 = CARTESIAN_POINT ( 'NONE',  ( 199.3295071964006979, 281.4960670786311425, -16.63318914033289886 ) ) ;
#93761 = EDGE_CURVE ( 'NONE', #100075, #82380, #28092, .T. ) ;
#93762 = CARTESIAN_POINT ( 'NONE',  ( 27.18159744850307291, 27.64441083166262203, -10.00000000000000533 ) ) ;
#93763 = DIRECTION ( 'NONE',  ( -0.8660254037844387076, -0.4999999999999998890, -0.000000000000000000 ) ) ;
#93764 = CARTESIAN_POINT ( 'NONE',  ( 131.8023238567217561, 240.2365022471901739, -10.00000000000009237 ) ) ;
#93765 = CARTESIAN_POINT ( 'NONE',  ( 188.2455483746452671, 260.8383077707633220, 2.948178099069697300 ) ) ;
#93766 = CARTESIAN_POINT ( 'NONE',  ( -15.31269525828471068, 104.2312461070085021, 43.89948692389422291 ) ) ;
#93767 = CARTESIAN_POINT ( 'NONE',  ( -0.2032289886040369309, 164.5643266524160140, -9.188101187500093303 ) ) ;
#93768 = PLANE ( 'NONE',  #97068 ) ;
#93769 = ORIENTED_EDGE ( 'NONE', *, *, #44612, .F. ) ;
#93770 = EDGE_CURVE ( 'NONE', #43945, #13446, #18345, .T. ) ;
#93771 = CARTESIAN_POINT ( 'NONE',  ( 160.7608406066382258, 253.1279765243780275, -14.70232046160609229 ) ) ;
#93772 = CARTESIAN_POINT ( 'NONE',  ( 13.35896364390118052, 31.21091486745859811, -1.111400068045478839E-16 ) ) ;
#93773 = DIRECTION ( 'NONE',  ( -0.8660254037844387076, -0.4999999999999998890, -0.000000000000000000 ) ) ;
#93774 = CARTESIAN_POINT ( 'NONE',  ( 22.85469738715664434, 177.8768266524159856, -9.188101187500093303 ) ) ;
#93775 = CARTESIAN_POINT ( 'NONE',  ( 62.42776884207837895, 218.3967562850346837, -4.648177544792955347E-16 ) ) ;
#93776 = CARTESIAN_POINT ( 'NONE',  ( 26.05686017436622137, 36.81751292744056769, -6.180339887498951690 ) ) ;
#93777 = CARTESIAN_POINT ( 'NONE',  ( 78.35917589421563889, 60.43990711353329459, 16.37966976287263421 ) ) ;
#93778 = CARTESIAN_POINT ( 'NONE',  ( 146.7373254022577100, 276.4904923669593586, -0.7242168585908188572 ) ) ;
#93779 = CARTESIAN_POINT ( 'NONE',  ( 81.07801343454443099, 56.14216831447085099, 16.10939811578601066 ) ) ;
#93780 = DIRECTION ( 'NONE',  ( -0.5346708562974007428, -0.8450603975019799208, 0.000000000000000000 ) ) ;
#93781 = EDGE_CURVE ( 'NONE', #86588, #75472, #75705, .T. ) ;
#93782 = CARTESIAN_POINT ( 'NONE',  ( 187.8880901142922824, 259.9596066364514400, -0.7662718320385906168 ) ) ;
#93783 = ADVANCED_FACE ( 'NONE', ( #58481 ), #27615, .T. ) ;
#93784 = CARTESIAN_POINT ( 'NONE',  ( 69.30415721694475906, 197.4865022471901455, 1.119607411625061291E-15 ) ) ;
#93785 = CARTESIAN_POINT ( 'NONE',  ( 71.83360485995035560, 66.53127591888950576, -11.52825921822993038 ) ) ;
#93786 = CARTESIAN_POINT ( 'NONE',  ( 203.6370189927176284, 270.2020975153263862, 6.025740961596683931 ) ) ;
#93787 = CARTESIAN_POINT ( 'NONE',  ( 33.24700223256990483, 183.8768266524160140, -9.188101187500091527 ) ) ;
#93788 = CARTESIAN_POINT ( 'NONE',  ( 72.76037481019558584, 70.79492043649185007, -7.951079947203126608 ) ) ;
#93789 = FILL_AREA_STYLE ('',( #15732 ) ) ;
#93790 = CARTESIAN_POINT ( 'NONE',  ( 203.0474655300526763, 270.0767168047294149, -6.426262563393472682 ) ) ;
#93791 = CARTESIAN_POINT ( 'NONE',  ( 151.3898985249405200, 268.4319993325432847, -14.65018536945715510 ) ) ;
#93793 = CARTESIAN_POINT ( 'NONE',  ( 79.14312167556931854, 57.64441083166269664, 0.000000000000000000 ) ) ;
#93792 = CIRCLE ( 'NONE', #95407, 0.1418229129680863287 ) ;
#93794 = CARTESIAN_POINT ( 'NONE',  ( 78.90260544222221029, 226.3615022471903160, 5.000000000000046185 ) ) ;
#93795 = CARTESIAN_POINT ( 'NONE',  ( 202.3402481470395742, 279.2721451994542576, -15.68818295843871624 ) ) ;
#93796 = CARTESIAN_POINT ( 'NONE',  ( 205.7253228364901645, 269.4700910448960940, -1.329327177517085845 ) ) ;
#93797 = CARTESIAN_POINT ( 'NONE',  ( 19.79331822069313418, 23.37878583063840665, 9.188101187500006262 ) ) ;
#93798 = CARTESIAN_POINT ( 'NONE',  ( 162.6220573360242270, 248.9773295930640131, 10.49878733418918486 ) ) ;
#93799 = CARTESIAN_POINT ( 'NONE',  ( 196.9319848161575806, 289.5507919934690335, -17.64330560362266453 ) ) ;
#93800 = CARTESIAN_POINT ( 'NONE',  ( 175.2944853640667873, 257.1826618528377253, 11.78886922157304085 ) ) ;
#93801 = ORIENTED_EDGE ( 'NONE', *, *, #64750, .F. ) ;
#93802 = AXIS2_PLACEMENT_3D ( 'NONE', #99344, #93257, #60797 ) ;
#93803 = CARTESIAN_POINT ( 'NONE',  ( 7.739928672529463149, 22.65586893147754211, -7.433330006724137462 ) ) ;
#93804 = FACE_OUTER_BOUND ( 'NONE', #42845, .T. ) ;
#93805 = CARTESIAN_POINT ( 'NONE',  ( 72.08846993314111273, 60.16552014367059797, -15.10313558536819123 ) ) ;
#93806 = CARTESIAN_POINT ( 'NONE',  ( 88.10649794555163794, 44.30893306230427697, 2.763757158845316475 ) ) ;
#93807 = EDGE_CURVE ( 'NONE', #65437, #39666, #52385, .T. ) ;
#93808 = VERTEX_POINT ( 'NONE', #91422 ) ;
#93809 = CARTESIAN_POINT ( 'NONE',  ( 16.79905537663784898, 192.0530062829863311, -4.648177544792955347E-16 ) ) ;
#93810 = CARTESIAN_POINT ( 'NONE',  ( 70.74702872844959245, 71.14896229169289654, -3.171960569837653399 ) ) ;
#93811 = CARTESIAN_POINT ( 'NONE',  ( 190.8094645593471341, 300.1553081486349015, 8.399847186519689757 ) ) ;
#93812 = CARTESIAN_POINT ( 'NONE',  ( 180.1993755460965758, 257.5231556457691795, -7.374963718432667292 ) ) ;
#93813 = ORIENTED_EDGE ( 'NONE', *, *, #68341, .T. ) ;
#93814 = ORIENTED_EDGE ( 'NONE', *, *, #12143, .F. ) ;
#93815 = EDGE_CURVE ( 'NONE', #21, #63881, #32536, .T. ) ;
#93817 = CARTESIAN_POINT ( 'NONE',  ( 85.17596481923946783, 42.83503000546589590, -3.343520128603064023 ) ) ;
#93816 = CARTESIAN_POINT ( 'NONE',  ( 189.4970640320313748, 274.7204259376300683, -16.57914224039128470 ) ) ;
#93818 = ORIENTED_EDGE ( 'NONE', *, *, #98262, .T. ) ;
#93819 = CARTESIAN_POINT ( 'NONE',  ( 200.7694952279801157, 282.9040289856181403, -17.94628235092568502 ) ) ;
#93820 = CYLINDRICAL_SURFACE ( 'NONE', #18953, 70.00000000000002842 ) ;
#93821 = CARTESIAN_POINT ( 'NONE',  ( 80.09463153584134432, 58.13915816355183352, 16.26729705550203420 ) ) ;
#93822 = CARTESIAN_POINT ( 'NONE',  ( 76.80413851785759505, 63.68367294747309870, 15.32454931363362149 ) ) ;
#93823 = CARTESIAN_POINT ( 'NONE',  ( 190.1063449786324213, 301.3731469862293011, 0.2163967485516588019 ) ) ;
#93824 = EDGE_CURVE ( 'NONE', #24620, #91836, #56238, .T. ) ;
#93825 = CARTESIAN_POINT ( 'NONE',  ( 196.3286486926436680, 290.5958008134369948, -16.58330917766970458 ) ) ;
#93826 = AXIS2_PLACEMENT_3D ( 'NONE', #63985, #41675, #72619 ) ;
#93827 = CARTESIAN_POINT ( 'NONE',  ( 183.9298583336507136, 289.3229830586321327, -13.00965999724257749 ) ) ;
#93828 = ADVANCED_FACE ( 'NONE', ( #87231 ), #70969, .T. ) ;
#93829 = VERTEX_POINT ( 'NONE', #80096 ) ;
#93830 = CARTESIAN_POINT ( 'NONE',  ( 157.1606030646430554, 258.4368458743103361, 17.96998724893680688 ) ) ;
#93831 = CARTESIAN_POINT ( 'NONE',  ( 161.9337977053698694, 266.9980763431651667, 16.53593164407537941 ) ) ;
#93832 = ORIENTED_EDGE ( 'NONE', *, *, #4718, .T. ) ;
#93833 = EDGE_CURVE ( 'NONE', #49158, #33261, #2063, .T. ) ;
#93834 = CARTESIAN_POINT ( 'NONE',  ( 29.64555348686941016, 32.51421378149920827, -9.188101187500004485 ) ) ;
#93835 = CARTESIAN_POINT ( 'NONE',  ( 198.1230806404959139, 287.4877535090322453, 17.00698319228197164 ) ) ;
#93836 = CARTESIAN_POINT ( 'NONE',  ( 154.4986966408730211, 266.8510081643221952, -16.80735267183326087 ) ) ;
#93838 = CIRCLE ( 'NONE', #26838, 0.1418229129680828593 ) ;
#93837 = CARTESIAN_POINT ( 'NONE',  ( 57.63111678181675757, 194.8923013555409796, 4.594050593750050204 ) ) ;
#93839 = ORIENTED_EDGE ( 'NONE', *, *, #26867, .F. ) ;
#93840 = CARTESIAN_POINT ( 'NONE',  ( 74.39841895140679640, 68.21392270468032848, 11.95628786500076934 ) ) ;
#93841 = CARTESIAN_POINT ( 'NONE',  ( 160.3857432900783522, 254.1750887689990179, 15.54860199936536702 ) ) ;
#93842 = CARTESIAN_POINT ( 'NONE',  ( -9.517469918280088592, 23.54023200771947799, 10.00000000000000000 ) ) ;
#93843 = ORIENTED_EDGE ( 'NONE', *, *, #81465, .F. ) ;
#93844 = CARTESIAN_POINT ( 'NONE',  ( 86.78238304187964047, 46.46655037883369488, 9.077226469069437087 ) ) ;
#93845 = CARTESIAN_POINT ( 'NONE',  ( 190.5541309856500050, 300.5975588711562523, -4.167177996129430184 ) ) ;
#93846 = CARTESIAN_POINT ( 'NONE',  ( -30.04356256989558815, 94.88921800892795488, 12.63376007436073323 ) ) ;
#93847 = ORIENTED_EDGE ( 'NONE', *, *, #60933, .T. ) ;
#93848 = CARTESIAN_POINT ( 'NONE',  ( 172.0550459485834267, 258.7583009836712336, -13.85092418383490731 ) ) ;
#93849 = CARTESIAN_POINT ( 'NONE',  ( 170.8756936250306069, 275.5691713738015096, -16.70647311572992066 ) ) ;
#93850 = CARTESIAN_POINT ( 'NONE',  ( 146.5281990801392453, 276.8527097820684730, 0.2636021916935416542 ) ) ;
#93851 = CARTESIAN_POINT ( 'NONE',  ( 192.9633865298379476, 296.4246058602058156, -11.85717392250713864 ) ) ;
#93852 = CARTESIAN_POINT ( 'NONE',  ( 160.7492247939479171, 256.1349200705061548, 15.91803943147225908 ) ) ;
#93853 = CARTESIAN_POINT ( 'NONE',  ( 177.9641021733659727, 269.8628481474571572, 16.10824436788937675 ) ) ;
#93854 = CARTESIAN_POINT ( 'NONE',  ( 206.0691053506789387, 273.7248349927971844, 11.70564474658248422 ) ) ;
#93855 = CARTESIAN_POINT ( 'NONE',  ( 67.37618507725385086, 66.59842348624097497, 8.613459505069345212 ) ) ;
#93856 = CARTESIAN_POINT ( 'NONE',  ( 75.88312381431275355, 64.11863994377948472, -14.52687401886447027 ) ) ;
#93857 = CARTESIAN_POINT ( 'NONE',  ( 207.6590484093196096, 270.9709728340903894, 3.402057849327809524 ) ) ;
#93858 = CARTESIAN_POINT ( 'NONE',  ( 118.4422513298640638, 233.0643266524159856, 9.188101187500095079 ) ) ;
#93859 = ORIENTED_EDGE ( 'NONE', *, *, #38058, .T. ) ;
#93860 = CARTESIAN_POINT ( 'NONE',  ( 190.1052739022278217, 301.3750021449804990, -4.471918118598219749 ) ) ;
#93861 = CARTESIAN_POINT ( 'NONE',  ( 83.54264106503212872, 41.58140769794766811, -1.200180926444211149 ) ) ;
#93862 = CARTESIAN_POINT ( 'NONE',  ( 154.8833801513861772, 262.3811116602312268, -17.49275566389638215 ) ) ;
#93863 = LINE ( 'NONE', #94358, #59613 ) ;
#93864 = CARTESIAN_POINT ( 'NONE',  ( 83.44578961920555571, 51.64149152686551503, -14.89211022975658949 ) ) ;
#93865 = CARTESIAN_POINT ( 'NONE',  ( 174.7971014982606448, 252.6639005122666219, 5.121287243991948124 ) ) ;
#93866 = VERTEX_POINT ( 'NONE', #32943 ) ;
#93867 = DIRECTION ( 'NONE',  ( -3.755686162884237478E-16, -3.302728788975889054E-33, 1.000000000000000000 ) ) ;
#93868 = CARTESIAN_POINT ( 'NONE',  ( -8.762112762712645164, 154.2012482093457777, 0.000000000000000000 ) ) ;
#93869 = CARTESIAN_POINT ( 'NONE',  ( 182.2804195259451774, 259.9783927104286363, 10.74157115564638154 ) ) ;
#93870 = CARTESIAN_POINT ( 'NONE',  ( 74.64154962151783934, 66.95428888261444911, 13.01658699031521849 ) ) ;
#93871 = CARTESIAN_POINT ( 'NONE',  ( 136.7913381204293728, 237.5327760586659736, 1.948934522072302763E-15 ) ) ;
#93872 = CARTESIAN_POINT ( 'NONE',  ( 150.9003228897357189, 269.2799692068659283, -14.30003212299500781 ) ) ;
#93873 = CIRCLE ( 'NONE', #16161, 70.00000000000001421 ) ;
#93874 = CARTESIAN_POINT ( 'NONE',  ( 189.0720805967732758, 299.7343203868808246, 4.955419684386629164 ) ) ;
#93875 = CARTESIAN_POINT ( 'NONE',  ( 196.3021893095863959, 290.6416298092292436, 17.45656988653421138 ) ) ;
#93876 = CARTESIAN_POINT ( 'NONE',  ( 32.29521950065672087, 67.39590844996666874, 59.99999999999999289 ) ) ;
#93877 = CARTESIAN_POINT ( 'NONE',  ( 51.08127902204942927, 209.4869531367911009, 4.594050593750046652 ) ) ;
#93878 = CARTESIAN_POINT ( 'NONE',  ( 76.91089219145437994, 60.33774281596894440, -16.24596170531351902 ) ) ;
#93880 = ORIENTED_EDGE ( 'NONE', *, *, #49491, .T. ) ;
#93879 = B_SPLINE_CURVE_WITH_KNOTS ( 'NONE', 3,
 ( #39973, #86656, #24787, #93743, #48608, #17187, #78515, #71913, #86162, #2515, #55178, #48089 ),
 .UNSPECIFIED., .F., .F.,
 ( 4, 2, 2, 2, 2, 4 ),
 ( 0.001243902885841379705, 0.001690362744074533916, 0.001913592673191032200, 0.002136822602307530700, 0.002583282460540394128, 0.003029742318773257122 ),
 .UNSPECIFIED. ) ;
#93881 = CARTESIAN_POINT ( 'NONE',  ( 173.0837253472800796, 264.8280141993791972, 17.07053884509587860 ) ) ;
#93882 = CARTESIAN_POINT ( 'NONE',  ( 43.83595887736691310, 122.5461495720015677, -10.00000000000000000 ) ) ;
#93883 = CARTESIAN_POINT ( 'NONE',  ( 72.19109158906036328, 71.10838548458626462, -5.953967166465967686 ) ) ;
#93884 = CARTESIAN_POINT ( 'NONE',  ( 175.0973281419315697, 261.2292456205797748, 14.95496001069501091 ) ) ;
#93885 = CARTESIAN_POINT ( 'NONE',  ( 74.14312167556930433, 66.30466486950707861, 1.224646799147354045E-15 ) ) ;
#93886 = DIRECTION ( 'NONE',  ( -0.000000000000000000, -0.000000000000000000, -1.000000000000000000 ) ) ;
#93887 = AXIS2_PLACEMENT_3D ( 'NONE', #54187, #99827, #46596 ) ;
#93888 = CARTESIAN_POINT ( 'NONE',  ( 13.35530768973961457, 178.5177522451418497, -10.00000000000009592 ) ) ;
#93889 = CARTESIAN_POINT ( 'NONE',  ( 126.3716228836089215, 233.7677522451417929, -5.000000000000041744 ) ) ;
#93890 = CARTESIAN_POINT ( 'NONE',  ( 167.5469267500292574, 266.7168544022062520, -17.80679023418265672 ) ) ;
#93891 = ORIENTED_EDGE ( 'NONE', *, *, #11228, .T. ) ;
#93892 = EDGE_CURVE ( 'NONE', #38792, #29884, #1571, .T. ) ;
#93893 = CARTESIAN_POINT ( 'NONE',  ( 163.2835940097493790, 247.8315144631017404, 11.08416305054517359 ) ) ;
#93894 = DIRECTION ( 'NONE',  ( -0.8660254037844387076, -0.4999999999999998890, -0.000000000000000000 ) ) ;
#93895 = CARTESIAN_POINT ( 'NONE',  ( 35.30381256655795852, 185.0643266524160140, 9.188101187500095079 ) ) ;
#93896 = CARTESIAN_POINT ( 'NONE',  ( 13.57497413706089517, 16.03677371833800436, 10.00000000000000533 ) ) ;
#93897 = CARTESIAN_POINT ( 'NONE',  ( 192.2499099399883846, 272.0886754808119008, 15.43621497701505341 ) ) ;
#93898 = CARTESIAN_POINT ( 'NONE',  ( 190.1693911629507738, 301.2639477917662703, -5.112716700269980485 ) ) ;
#93899 = CARTESIAN_POINT ( 'NONE',  ( 72.28819773863641274, 72.03526396437469259, 3.423969264441562466 ) ) ;
#93901 = CARTESIAN_POINT ( 'NONE',  ( 60.19284827774796298, 218.8927522451419350, 2.944929066748280225E-16 ) ) ;
#93900 = CARTESIAN_POINT ( 'NONE',  ( -46.49770490450612215, 29.77544742692501600, -10.00000000000000000 ) ) ;
#93902 = LINE ( 'NONE', #48771, #64425 ) ;
#93903 = CARTESIAN_POINT ( 'NONE',  ( 163.0473843169341706, 256.3777160336861130, -15.36546227846566559 ) ) ;
#93904 = EDGE_CURVE ( 'NONE', #51277, #37680, #48665, .T. ) ;
#93905 = CARTESIAN_POINT ( 'NONE',  ( 157.8696211474012330, 257.2087905314882619, -17.27527248276125604 ) ) ;
#93906 = CARTESIAN_POINT ( 'NONE',  ( 15.30702494462977192, 17.03677371833800791, 10.00000000000000533 ) ) ;
#93907 = EDGE_LOOP ( 'NONE', ( #94092, #51423, #10346, #90598 ) ) ;
#93908 = EDGE_CURVE ( 'NONE', #2785, #11457, #64350, .T. ) ;
#93909 = CARTESIAN_POINT ( 'NONE',  ( 21.31191609055701974, 193.1115022471903160, -5.000000000000047962 ) ) ;
#93910 = CARTESIAN_POINT ( 'NONE',  ( 32.38751264475774860, 201.0530062829863027, -4.648177544792955347E-16 ) ) ;
#93911 = CARTESIAN_POINT ( 'NONE',  ( 181.1477013271936016, 287.8971774238942203, -14.15342935774602218 ) ) ;
#93912 = CARTESIAN_POINT ( 'NONE',  ( -10.75808714510939090, 164.5958772461660544, -9.188101187500095079 ) ) ;
#93913 = CARTESIAN_POINT ( 'NONE',  ( 31.37640799630998956, 30.06628583063843507, -9.188101187500006262 ) ) ;
#93915 = CARTESIAN_POINT ( 'NONE',  ( 200.3843439899536634, 282.5246900502644962, 16.99942400046845492 ) ) ;
#93914 = CARTESIAN_POINT ( 'NONE',  ( 164.1174636406832406, 260.3667033378403630, -16.13808382457397173 ) ) ;
#93916 = CARTESIAN_POINT ( 'NONE',  ( 185.2882774749097052, 260.3413492530625604, 6.861618744156088745 ) ) ;
#93917 = LINE ( 'NONE', #39643, #61059 ) ;
#93918 = CARTESIAN_POINT ( 'NONE',  ( 185.4079346854762207, 258.9246787615279572, -2.323817269112564254 ) ) ;
#93919 = CARTESIAN_POINT ( 'NONE',  ( 66.30824103392255608, 68.65941448300486627, 2.357034909269177358 ) ) ;
#93920 = ORIENTED_EDGE ( 'NONE', *, *, #40480, .T. ) ;
#93921 = CARTESIAN_POINT ( 'NONE',  ( 79.98829826350832661, 44.59498145193617802, 11.76229303994366582 ) ) ;
#93922 = CARTESIAN_POINT ( 'NONE',  ( 4.275827057391709651, 20.65586893147753500, -7.433330006724137462 ) ) ;
#93923 = CARTESIAN_POINT ( 'NONE',  ( 166.8963884910926936, 286.1636476361714472, 0.4999093504684499201 ) ) ;
#93924 = CARTESIAN_POINT ( 'NONE',  ( 11.61057445305848823, 22.10171378149917487, 9.188101187500008038 ) ) ;
#93925 = DIRECTION ( 'NONE',  ( 0.2701803667135113662, 0.9628097264997651505, 0.000000000000000000 ) ) ;
#93926 = CARTESIAN_POINT ( 'NONE',  ( 159.2102594322688844, 254.8867369075254885, -16.13039487917589199 ) ) ;
#93927 = CARTESIAN_POINT ( 'NONE',  ( 152.6615646578087819, 266.2294089801508221, 16.94722993326405813 ) ) ;
#93928 = CARTESIAN_POINT ( 'NONE',  ( 189.9900095322273046, 294.8206031209193725, 12.79687042303630840 ) ) ;
#93929 = LINE ( 'NONE', #86347, #88267 ) ;
#93930 = CARTESIAN_POINT ( 'NONE',  ( 163.4178923001155681, 247.5989030008181260, -10.38047187240561442 ) ) ;
#93931 = DIRECTION ( 'NONE',  ( 0.000000000000000000, 0.000000000000000000, 1.000000000000000000 ) ) ;
#93932 = VERTEX_POINT ( 'NONE', #32454 ) ;
#93933 = VERTEX_POINT ( 'NONE', #77180 ) ;
#93934 = EDGE_CURVE ( 'NONE', #100061, #58518, #98132, .T. ) ;
#93935 = CARTESIAN_POINT ( 'NONE',  ( 129.8617249334801613, 257.3297689869269220, -2.679491924311252493 ) ) ;
#93936 = DIRECTION ( 'NONE',  ( 0.6270036013472576331, 0.3336146661356737542, -0.7039657224870771168 ) ) ;
#93937 = ORIENTED_EDGE ( 'NONE', *, *, #4575, .F. ) ;
#93938 = CARTESIAN_POINT ( 'NONE',  ( 36.10619739613039769, 52.83927550304669296, -10.00000000000000000 ) ) ;
#93939 = CARTESIAN_POINT ( 'NONE',  ( 203.8609927293776707, 267.9499622782657866, -0.9252015903767020211 ) ) ;
#93940 = ORIENTED_EDGE ( 'NONE', *, *, #85891, .F. ) ;
#93941 = AXIS2_PLACEMENT_3D ( 'NONE', #41919, #18639, #72354 ) ;
#93942 = DIRECTION ( 'NONE',  ( -3.755686162884236985E-16, 2.795463207713249976E-32, 1.000000000000000000 ) ) ;
#93943 = CARTESIAN_POINT ( 'NONE',  ( 79.21141449090154651, 59.45940664425069144, -16.53580481313994710 ) ) ;
#93944 = EDGE_CURVE ( 'NONE', #39202, #81343, #53878, .T. ) ;
#93945 = CARTESIAN_POINT ( 'NONE',  ( 80.61419007678392745, 43.44355932592966241, 9.504397039665120062 ) ) ;
#93946 = ORIENTED_EDGE ( 'NONE', *, *, #55161, .F. ) ;
#93947 = CARTESIAN_POINT ( 'NONE',  ( 161.1990332043106946, 251.4420796895884394, 14.26998817770995487 ) ) ;
#93948 = B_SPLINE_CURVE_WITH_KNOTS ( 'NONE', 3,
 ( #90261, #57804, #73043, #3636 ),
 .UNSPECIFIED., .F., .F.,
 ( 4, 4 ),
 ( 0.009422416152678910611, 0.01491714414824748224 ),
 .UNSPECIFIED. ) ;
#93949 = CARTESIAN_POINT ( 'NONE',  ( 151.4159295687746294, 268.3869122420484814, 14.78076517566594106 ) ) ;
#93950 = CARTESIAN_POINT ( 'NONE',  ( 36.68702710410600076, 29.38052372038643867, 10.00000000000000533 ) ) ;
#93951 = ORIENTED_EDGE ( 'NONE', *, *, #27580, .T. ) ;
#93952 = EDGE_CURVE ( 'NONE', #37817, #86137, #91112, .T. ) ;
#93953 = EDGE_LOOP ( 'NONE', ( #8060, #85995, #17678, #51726 ) ) ;
#93954 = ORIENTED_EDGE ( 'NONE', *, *, #35773, .F. ) ;
#93955 = CARTESIAN_POINT ( 'NONE',  ( 74.41922904744917844, 66.10598066252020999, 13.04199649849176978 ) ) ;
#93956 = ORIENTED_EDGE ( 'NONE', *, *, #53934, .T. ) ;
#93957 = CARTESIAN_POINT ( 'NONE',  ( 180.3976227892601685, 269.7841510484220748, 17.25711389196291279 ) ) ;
#93958 = VECTOR ( 'NONE', #86163, 1000.000000000000227 ) ;
#93959 = VERTEX_POINT ( 'NONE', #94786 ) ;
#93960 = CARTESIAN_POINT ( 'NONE',  ( 208.3135187673106543, 269.8373969220020285, 2.829653198597726682 ) ) ;
#93961 = CARTESIAN_POINT ( 'NONE',  ( 81.41038491292694346, 44.34486577817341413, 10.01861531637363001 ) ) ;
#93962 = B_SPLINE_CURVE_WITH_KNOTS ( 'NONE', 3,
 ( #56226, #2052, #79083, #83819 ),
 .UNSPECIFIED., .F., .F.,
 ( 4, 4 ),
 ( 0.01139215366488464942, 0.01983881652011612248 ),
 .UNSPECIFIED. ) ;
#93963 = DIRECTION ( 'NONE',  ( -1.000000000000000000, 0.000000000000000000, 0.000000000000000000 ) ) ;
#93964 = CARTESIAN_POINT ( 'NONE',  ( -13.11024591527734628, 0.000000000000000000, -32.50000000000000000 ) ) ;
#93965 = CYLINDRICAL_SURFACE ( 'NONE', #77428, 70.00000000000002842 ) ;
#93966 = CARTESIAN_POINT ( 'NONE',  ( 198.2505066714982149, 285.2670451491296149, 0.000000000000000000 ) ) ;
#93967 = CARTESIAN_POINT ( 'NONE',  ( 167.1118283438475487, 246.8866125954127426, 1.959209920999884336 ) ) ;
#93968 = CARTESIAN_POINT ( 'NONE',  ( 18.65184876021338312, 28.95586893147755703, 7.433330006724141015 ) ) ;
#93969 = CARTESIAN_POINT ( 'NONE',  ( -30.18034446749236821, 25.12100238203592539, -10.00000000000000000 ) ) ;
#93970 = CARTESIAN_POINT ( 'NONE',  ( 164.2545401858843945, 246.1497863546213978, 2.275217130759496609 ) ) ;
#93972 = ORIENTED_EDGE ( 'NONE', *, *, #90130, .F. ) ;
#93971 = CARTESIAN_POINT ( 'NONE',  ( 159.2303255284352304, 254.8519814094557603, 16.39103317446447150 ) ) ;
#93973 = CARTESIAN_POINT ( 'NONE',  ( -22.42236680055709641, 157.8615022471902591, 0.000000000000000000 ) ) ;
#93974 = FACE_OUTER_BOUND ( 'NONE', #77589, .T. ) ;
#93975 = CARTESIAN_POINT ( 'NONE',  ( 206.2809287719926488, 273.3579460648492159, -10.70911012174624588 ) ) ;
#93976 = CARTESIAN_POINT ( 'NONE',  ( 157.6304115535352537, 270.8650229002738001, -16.00510772102553858 ) ) ;
#93977 = EDGE_CURVE ( 'NONE', #23731, #97425, #48148, .T. ) ;
#93978 = CARTESIAN_POINT ( 'NONE',  ( 200.6449165581618956, 283.1198055712825976, 18.35107460171532523 ) ) ;
#93979 = CARTESIAN_POINT ( 'NONE',  ( 71.48241248555748939, 59.13619044504650901, 15.79769907036114596 ) ) ;
#93980 = ORIENTED_EDGE ( 'NONE', *, *, #63283, .T. ) ;
#93981 = CARTESIAN_POINT ( 'NONE',  ( 155.7698133297891729, 260.8457643577225440, -17.53298471631897826 ) ) ;
#93982 = FACE_OUTER_BOUND ( 'NONE', #83356, .T. ) ;
#93983 = B_SPLINE_CURVE_WITH_KNOTS ( 'NONE', 3,
 ( #10546, #44287, #90950, #18650, #28593, #18144 ),
 .UNSPECIFIED., .F., .F.,
 ( 4, 2, 4 ),
 ( 0.0009160183432510218956, 0.001204151881099926186, 0.001492285418948830584 ),
 .UNSPECIFIED. ) ;
#93985 = EDGE_CURVE ( 'NONE', #43160, #66403, #70087, .T. ) ;
#93984 = LINE ( 'NONE', #10860, #93727 ) ;
#93986 = CARTESIAN_POINT ( 'NONE',  ( 16.02555268474166539, 173.3927522451417929, -10.00000000000009059 ) ) ;
#93987 = CARTESIAN_POINT ( 'NONE',  ( 81.20281187136818346, 223.8149278399160664, 9.188101187500093303 ) ) ;
#93988 = CARTESIAN_POINT ( 'NONE',  ( 82.33681322515650436, 40.36000428313853661, -1.174226880687108565 ) ) ;
#93989 = CARTESIAN_POINT ( 'NONE',  ( 199.5820190223589066, 281.0610403850588455, -17.29246150691365358 ) ) ;
#93990 = CARTESIAN_POINT ( 'NONE',  ( 170.3095142286849750, 280.6389898262832503, -13.87900323416883275 ) ) ;
#93991 = B_SPLINE_CURVE_WITH_KNOTS ( 'NONE', 3,
 ( #53372, #6284, #44274, #14388 ),
 .UNSPECIFIED., .F., .F.,
 ( 4, 4 ),
 ( 0.001625297393536941689, 0.006935763186732861116 ),
 .UNSPECIFIED. ) ;
#93993 = CARTESIAN_POINT ( 'NONE',  ( 75.52860420788245222, 65.41786526994388851, 13.84462426059885232 ) ) ;
#93992 = CARTESIAN_POINT ( 'NONE',  ( 3.802138503898990329, 166.8768266524160140, 9.188101187500098632 ) ) ;
#93994 = CARTESIAN_POINT ( 'NONE',  ( 200.4116241316243645, 283.5238799070667142, 18.37703770054986663 ) ) ;
#93995 = EDGE_LOOP ( 'NONE', ( #26291, #85748, #58730, #80789 ) ) ;
#93997 = ORIENTED_EDGE ( 'NONE', *, *, #90314, .T. ) ;
#93996 = UNCERTAINTY_MEASURE_WITH_UNIT (LENGTH_MEASURE( 1.000000000000000082E-05 ), #678, 'distance_accuracy_value', 'NONE');
#93998 = CARTESIAN_POINT ( 'NONE',  ( 197.8465159808518763, 265.0022582763427863, -3.002757407549030866 ) ) ;
#93999 = CARTESIAN_POINT ( 'NONE',  ( 83.81405641344784385, 46.32409837379321260, -10.73277976188174598 ) ) ;
#94000 = CARTESIAN_POINT ( 'NONE',  ( 83.14518538925494795, 42.42924448188458086, 5.540143244992730587 ) ) ;
#94001 = CARTESIAN_POINT ( 'NONE',  ( 161.4143265314674522, 251.0691807084224365, -12.94469757303959234 ) ) ;
#94002 =( BOUNDED_CURVE ( )  B_SPLINE_CURVE ( 2, ( #76382, #5968, #22164, #6472, #92117, #100181, #30766, #54035, #22669 ),
 .UNSPECIFIED., .F., .T. ) 
 B_SPLINE_CURVE_WITH_KNOTS ( ( 3, 2, 2, 2, 3 ),
 ( 0.6572580645161290036, 0.6586021505376343788, 0.6612903225806451291, 0.6639784946236558794, 0.6653225806451612545 ),
 .UNSPECIFIED. ) 
 CURVE ( )  GEOMETRIC_REPRESENTATION_ITEM ( )  RATIONAL_B_SPLINE_CURVE ( ( 0.9330127018922194093, 0.9330127018922194093, 1.000000000000000000, 0.8660254037844387076, 1.000000000000000000, 0.8660254037844387076, 1.000000000000000000, 0.9330127018922194093, 0.9330127018922194093 ) ) 
 REPRESENTATION_ITEM ( '' )  );
#94003 = CARTESIAN_POINT ( 'NONE',  ( 185.3339445475077696, 286.4653616608484299, 16.08708905285897828 ) ) ;
#94004 = CARTESIAN_POINT ( 'NONE',  ( 107.7317227740038987, 244.5530062829863311, -4.648177544792955347E-16 ) ) ;
#94005 = CARTESIAN_POINT ( 'NONE',  ( 31.13589176296283156, 188.7833772461660544, -9.188101187500095079 ) ) ;
#94006 = CARTESIAN_POINT ( 'NONE',  ( 198.8055222331880145, 277.1762050399552209, 15.17661964589477996 ) ) ;
#94007 = VERTEX_POINT ( 'NONE', #34936 ) ;
#94008 = CARTESIAN_POINT ( 'NONE',  ( 25.93867647934751730, 197.3297689869269220, -2.679491924311252493 ) ) ;
#94009 = CARTESIAN_POINT ( 'NONE',  ( 175.3077253703091003, 281.1061267443325278, -14.92186143449572100 ) ) ;
#94010 = CARTESIAN_POINT ( 'NONE',  ( 38.10324709940346111, 24.12755873383628469, -6.180339887498949025 ) ) ;
#94011 = CARTESIAN_POINT ( 'NONE',  ( 157.2168982216852555, 258.3393398020932636, 18.09635675623264106 ) ) ;
#94012 = CARTESIAN_POINT ( 'NONE',  ( 68.83964938300935898, 63.80711696496913987, -12.26050211274642265 ) ) ;
#94013 = CARTESIAN_POINT ( 'NONE',  ( 169.5007657120409874, 248.2156828994837099, -1.963647642838588503 ) ) ;
#94014 = CARTESIAN_POINT ( 'NONE',  ( 186.5421308631587465, 282.7087754812748130, 16.16777212897319771 ) ) ;
#94015 = CARTESIAN_POINT ( 'NONE',  ( 194.6943296385021824, 293.4265244509877562, -16.10917128197217352 ) ) ;
#94016 = CARTESIAN_POINT ( 'NONE',  ( 189.8346037648321101, 263.3851992863394571, 7.885794067937258234 ) ) ;
#94017 = CARTESIAN_POINT ( 'NONE',  ( 204.3276935076901850, 276.7410487817560920, 13.46217427333259309 ) ) ;
#94018 = CARTESIAN_POINT ( 'NONE',  ( 176.6943099527350682, 256.7931168052207340, -11.17617521364210731 ) ) ;
#94019 = EDGE_CURVE ( 'NONE', #58141, #54753, #66838, .T. ) ;
#94020 = CARTESIAN_POINT ( 'NONE',  ( 146.5913834600193582, 276.7432712258716947, -0.4909717733184599253 ) ) ;
#94021 = CARTESIAN_POINT ( 'NONE',  ( 190.2476911738421848, 301.1283281946692796, -1.360079143321618611 ) ) ;
#94022 = EDGE_LOOP ( 'NONE', ( #98070, #36712, #87003, #58256 ) ) ;
#94023 = CARTESIAN_POINT ( 'NONE',  ( 152.4638493392093608, 266.9524761909081576, -15.49024149966747466 ) ) ;
#94024 = ADVANCED_FACE ( 'NONE', ( #89218 ), #75115, .F. ) ;
#94025 = VECTOR ( 'NONE', #21385, 1000.000000000000000 ) ;
#94026 = CARTESIAN_POINT ( 'NONE',  ( 14.88889434582250537, 172.7365022471902023, -10.00000000000009237 ) ) ;
#94027 = CARTESIAN_POINT ( 'NONE',  ( 112.1907172202364080, 226.3923013555410080, 4.594050593750050204 ) ) ;
#94028 = CARTESIAN_POINT ( 'NONE',  ( 11.93836421708519779, 28.93396525600389069, 2.839279412974139660 ) ) ;
#94029 = CARTESIAN_POINT ( 'NONE',  ( 110.0000000000000000, 15.00000000000003908, 59.99999999999999289 ) ) ;
#94030 = DIRECTION ( 'NONE',  ( 0.08498217737243619896, 0.9963824715083259287, 0.000000000000000000 ) ) ;
#94032 = CARTESIAN_POINT ( 'NONE',  ( 195.6526726375238070, 278.3487319424068573, 16.84146745586420479 ) ) ;
#94031 = CARTESIAN_POINT ( 'NONE',  ( 196.3720681610792553, 290.5205960880691691, 16.18360420724715354 ) ) ;
#94033 = CARTESIAN_POINT ( 'NONE',  ( 151.0468907355330543, 269.0261062511888213, -14.45235335422399814 ) ) ;
#94034 = CARTESIAN_POINT ( 'NONE',  ( 30.06092144891428930, 17.75978393459166682, -1.583844403245396437 ) ) ;
#94035 = CARTESIAN_POINT ( 'NONE',  ( 197.0313051377892748, 289.3787641501790517, -17.15509075150697882 ) ) ;
#94036 = CARTESIAN_POINT ( 'NONE',  ( 2.064617007569734319, 27.83817977871672511, 10.00000000000000000 ) ) ;
#94037 = CARTESIAN_POINT ( 'NONE',  ( -27.42236680055714260, 166.5217562850347406, 1.224646799147364892E-15 ) ) ;
#94038 = CARTESIAN_POINT ( 'NONE',  ( 85.88548993935545184, 47.52640722116844785, 10.83458574080284187 ) ) ;
#94039 = ORIENTED_EDGE ( 'NONE', *, *, #54563, .T. ) ;
#94040 = CARTESIAN_POINT ( 'NONE',  ( 189.4560346390393875, 265.8111423811684517, 10.75552142954006740 ) ) ;
#94041 = CARTESIAN_POINT ( 'NONE',  ( 179.0021197982646584, 280.8427306710001403, 16.33118346667503928 ) ) ;
#94042 = CARTESIAN_POINT ( 'NONE',  ( 200.5907457738537119, 269.0703187529413185, 9.184797546115563094 ) ) ;
#94043 = ORIENTED_EDGE ( 'NONE', *, *, #30650, .F. ) ;
#94044 = B_SPLINE_CURVE_WITH_KNOTS ( 'NONE', 3,
 ( #53021, #23108, #53999, #84960 ),
 .UNSPECIFIED., .F., .F.,
 ( 4, 4 ),
 ( 0.01212979347998805260, 0.02063677174155311225 ),
 .UNSPECIFIED. ) ;
#94045 = CARTESIAN_POINT ( 'NONE',  ( 84.15543808568007478, 42.98865946211766698, 6.707866528308588094 ) ) ;
#94046 = CARTESIAN_POINT ( 'NONE',  ( 186.2588223522137696, 258.3231150775076230, 4.130381131686830187 ) ) ;
#94047 = CARTESIAN_POINT ( 'NONE',  ( 170.9071956757241821, 261.0918318682022914, -16.28277954748680401 ) ) ;
#94048 = CARTESIAN_POINT ( 'NONE',  ( 74.96538493238443834, 53.10769796979874258, -16.50489419803275837 ) ) ;
#94049 = CARTESIAN_POINT ( 'NONE',  ( 192.6470966816805230, 296.9724359471326807, 11.11268290051284424 ) ) ;
#94050 = ORIENTED_EDGE ( 'NONE', *, *, #75362, .T. ) ;
#94051 = EDGE_CURVE ( 'NONE', #45703, #52319, #91673, .T. ) ;
#94052 = CARTESIAN_POINT ( 'NONE',  ( 191.2263287708686050, 280.2574088826832508, 17.09578982601275854 ) ) ;
#94053 = CARTESIAN_POINT ( 'NONE',  ( 36.57375671714491006, 36.51421378149921537, -9.188101187500004485 ) ) ;
#94054 = CARTESIAN_POINT ( 'NONE',  ( 73.06817150023823615, 70.46971108366265923, -8.031831301699734027 ) ) ;
#94055 = ORIENTED_EDGE ( 'NONE', *, *, #75659, .T. ) ;
#94056 = CARTESIAN_POINT ( 'NONE',  ( 177.7342311040593756, 255.2532439957012684, -8.367404576774948310 ) ) ;
#94057 = LINE ( 'NONE', #79369, #1436 ) ;
#94058 = CARTESIAN_POINT ( 'NONE',  ( 201.5189872289815867, 266.7509884862435570, -2.318412474989284267 ) ) ;
#94059 = ORIENTED_EDGE ( 'NONE', *, *, #62646, .T. ) ;
#94060 = CARTESIAN_POINT ( 'NONE',  ( 86.40901846424877419, 47.04753287972406639, -10.02754009819726733 ) ) ;
#94061 = CARTESIAN_POINT ( 'NONE',  ( 188.8213496144733483, 293.6675690155782945, 12.81620811140911265 ) ) ;
#94062 = CARTESIAN_POINT ( 'NONE',  ( 1.210598108517954685, 183.0530062829863596, 2.649461200531984646E-14 ) ) ;
#94063 = CARTESIAN_POINT ( 'NONE',  ( 88.05624235485146301, 44.55787864911079765, -5.145732200269208967 ) ) ;
#94064 = DIRECTION ( 'NONE',  ( -0.000000000000000000, -0.000000000000000000, 1.000000000000000000 ) ) ;
#94065 = CARTESIAN_POINT ( 'NONE',  ( -19.65312891409030271, 93.06504152958497400, 177.5919119679930134 ) ) ;
#94066 = CARTESIAN_POINT ( 'NONE',  ( 80.41490723808537666, 44.37095382489257389, 11.34173964343496621 ) ) ;
#94067 = CARTESIAN_POINT ( 'NONE',  ( 26.18314342202568668, 41.82794442100486521, 10.00000000000000000 ) ) ;
#94068 = ORIENTED_EDGE ( 'NONE', *, *, #35795, .T. ) ;
#94069 = EDGE_LOOP ( 'NONE', ( #26015, #19206, #92688, #30382 ) ) ;
#94070 = CARTESIAN_POINT ( 'NONE',  ( 195.4899348203562965, 291.0385781265877085, 16.10920391193625179 ) ) ;
#94071 = VERTEX_POINT ( 'NONE', #14644 ) ;
#94072 = DIRECTION ( 'NONE',  ( 0.5000000000000014433, -0.8660254037844378194, 0.000000000000000000 ) ) ;
#94073 = ORIENTED_EDGE ( 'NONE', *, *, #46448, .T. ) ;
#94074 = CARTESIAN_POINT ( 'NONE',  ( 74.88642528495033446, 58.21203573159304767, 15.94079607396144560 ) ) ;
#94075 = CARTESIAN_POINT ( 'NONE',  ( 78.71449943708836372, 50.90750488496149018, 15.15446692355688896 ) ) ;
#94076 = ORIENTED_EDGE ( 'NONE', *, *, #49866, .T. ) ;
#94077 = CARTESIAN_POINT ( 'NONE',  ( 184.5471555646610682, 281.3800897130075782, -16.25044877093907658 ) ) ;
#94078 = CARTESIAN_POINT ( 'NONE',  ( 164.3448606421738702, 245.9933467353647814, -1.273739175181084260 ) ) ;
#94079 = CARTESIAN_POINT ( 'NONE',  ( 190.0367258288550829, 301.4937308908229170, 2.142183824395127445 ) ) ;
#94080 = CARTESIAN_POINT ( 'NONE',  ( 196.1272880827983442, 284.4644126364685235, -17.48124770668370331 ) ) ;
#94081 = LINE ( 'NONE', #55514, #61215 ) ;
#94082 = CARTESIAN_POINT ( 'NONE',  ( 168.2785332225647323, 249.6087795265106593, -5.466131228726310631 ) ) ;
#94083 = CARTESIAN_POINT ( 'NONE',  ( 76.97203077703174756, 62.91777711518242455, -15.25263661455074171 ) ) ;
#94084 = CARTESIAN_POINT ( 'NONE',  ( 157.9722338812990472, 280.9990382926234247, 2.257701763675134199 ) ) ;
#94085 = CARTESIAN_POINT ( 'NONE',  ( 134.5719744753492364, 242.3768266524159856, -9.188101187500091527 ) ) ;
#94086 = VERTEX_POINT ( 'NONE', #44018 ) ;
#94087 = CARTESIAN_POINT ( 'NONE',  ( 70.62612002322232740, 60.62352525996839603, -14.61234695924068205 ) ) ;
#94088 = CARTESIAN_POINT ( 'NONE',  ( 37.50955192761952617, 39.84336893147759184, -7.433330006724137462 ) ) ;
#94089 = ADVANCED_FACE ( 'NONE', ( #22235 ), #51633, .T. ) ;
#94090 = ORIENTED_EDGE ( 'NONE', *, *, #94473, .T. ) ;
#94092 = ORIENTED_EDGE ( 'NONE', *, *, #31161, .F. ) ;
#94091 = CARTESIAN_POINT ( 'NONE',  ( 152.6809499003229860, 273.9044486092186048, 12.24870461040242553 ) ) ;
#94093 = CARTESIAN_POINT ( 'NONE',  ( 200.3208879218390450, 274.1164785610297372, 13.54232579234367506 ) ) ;
#94094 = DIRECTION ( 'NONE',  ( -0.8660254037844387076, -0.4999999999999998890, -0.000000000000000000 ) ) ;
#94095 = CARTESIAN_POINT ( 'NONE',  ( -13.11024591527723615, 27.99999999999999645, -32.50000000000017053 ) ) ;
#94096 = CARTESIAN_POINT ( 'NONE',  ( 147.4519858293454320, 275.2526641970844707, 3.572377003827207353 ) ) ;
#94097 = CARTESIAN_POINT ( 'NONE',  ( 73.72578271399891037, 68.22897723188711439, 11.11049049714292991 ) ) ;
#94098 = DIRECTION ( 'NONE',  ( 1.000000000000000000, 0.000000000000000000, 0.000000000000000000 ) ) ;
#94099 = CARTESIAN_POINT ( 'NONE',  ( 173.3818033105709446, 287.4306447483324405, -9.822949107308927452 ) ) ;
#94100 = CARTESIAN_POINT ( 'NONE',  ( 174.7211242335244208, 282.3968719112178292, 14.74411924494472359 ) ) ;
#94101 = AXIS2_PLACEMENT_3D ( 'NONE', #17493, #79344, #2313 ) ;
#94102 = CARTESIAN_POINT ( 'NONE',  ( 176.0127109592394277, 252.6004560315867593, -4.768680066900455650 ) ) ;
#94103 = EDGE_LOOP ( 'NONE', ( #98896, #66148, #33646 ) ) ;
#94104 = CARTESIAN_POINT ( 'NONE',  ( 194.6782745185928434, 293.4543327343926080, -14.56555309295305634 ) ) ;
#94105 = CARTESIAN_POINT ( 'NONE',  ( 152.7208596440031840, 273.9049655622842465, 12.23028915028310415 ) ) ;
#94106 = EDGE_LOOP ( 'NONE', ( #14141, #55859, #67990, #70834 ) ) ;
#94107 = CARTESIAN_POINT ( 'NONE',  ( 190.0162302916581893, 267.2141329825763023, -11.93996759466560853 ) ) ;
#94108 = CARTESIAN_POINT ( 'NONE',  ( 190.9800885167487650, 283.3134609288387651, -16.57359780736571153 ) ) ;
#94109 = CARTESIAN_POINT ( 'NONE',  ( 192.1932326858383249, 297.7585514476576236, -9.982766916270952251 ) ) ;
#94110 = CARTESIAN_POINT ( 'NONE',  ( 86.78549426258132371, 45.83013854792883279, 8.849882187839877901 ) ) ;
#94111 = DIRECTION ( 'NONE',  ( -0.6600842437418951159, 0.7511915808658203852, 0.000000000000000000 ) ) ;
#94113 = CARTESIAN_POINT ( 'NONE',  ( 151.4960827286219001, 274.9315224285210206, -8.792788082167028563 ) ) ;
#94112 = CARTESIAN_POINT ( 'NONE',  ( 161.4469300188632701, 281.4659579066204174, -6.636762326697274617 ) ) ;
#94114 = CARTESIAN_POINT ( 'NONE',  ( 164.9043417134678577, 286.5925546497160212, 0.04530247668140159611 ) ) ;
#94115 = ORIENTED_EDGE ( 'NONE', *, *, #58313, .T. ) ;
#94116 = CARTESIAN_POINT ( 'NONE',  ( 147.5492216329511166, 275.0842468449245644, 4.751613690710122739 ) ) ;
#94117 = CARTESIAN_POINT ( 'NONE',  ( 73.83053071202353124, 66.06161260281930936, 13.30051256284848904 ) ) ;
#94118 = DIRECTION ( 'NONE',  ( 0.8660254037844395958, 0.4999999999999985567, 0.000000000000000000 ) ) ;
#94119 = CARTESIAN_POINT ( 'NONE',  ( 87.88902802526534686, 43.91876200309240375, 0.4180276961671919311 ) ) ;
#94120 = CARTESIAN_POINT ( 'NONE',  ( 3.808674319871268921, 184.5530062829863027, -4.648177544792955347E-16 ) ) ;
#94121 = CARTESIAN_POINT ( 'NONE',  ( 152.6615646578087819, 266.2294089801508221, 16.94722993326405813 ) ) ;
#94122 = CARTESIAN_POINT ( 'NONE',  ( 73.86986929274216607, 68.54753403896816621, 11.39714278534122549 ) ) ;
#94123 = CARTESIAN_POINT ( 'NONE',  ( 74.33743881423829691, 68.50532701121755963, 11.17712573888744920 ) ) ;
#94124 = CARTESIAN_POINT ( 'NONE',  ( 70.52490725396940263, 71.27080261044798704, -1.937046345266181024 ) ) ;
#94125 = CARTESIAN_POINT ( 'NONE',  ( -15.46727382606978374, 168.0024278399161233, -9.188101187500093303 ) ) ;
#94126 = CARTESIAN_POINT ( 'NONE',  ( 84.07169456928664886, 219.3458772461660544, 9.188101187500095079 ) ) ;
#94127 = CARTESIAN_POINT ( 'NONE',  ( 155.6066474290145720, 261.1283759879266881, -18.16552045242181279 ) ) ;
#94128 = CARTESIAN_POINT ( 'NONE',  ( 146.8312060062178830, 276.3278863910550172, -4.807241325481028227 ) ) ;
#94129 = CARTESIAN_POINT ( 'NONE',  ( 182.8446340216047474, 294.1739319776609705, -7.947300712334529393 ) ) ;
#94130 = PLANE ( 'NONE',  #67426 ) ;
#94131 = CARTESIAN_POINT ( 'NONE',  ( 77.84067285015417781, 53.77961970061534203, 15.94779701496784696 ) ) ;
#94132 = LINE ( 'NONE', #54073, #27491 ) ;
#94134 = CARTESIAN_POINT ( 'NONE',  ( 75.87085204095464519, 51.53938293317272468, 15.71483405503507136 ) ) ;
#94133 = CARTESIAN_POINT ( 'NONE',  ( 67.00432206419098691, 66.89247057574091571, 8.809205559600117752 ) ) ;
#94135 = CARTESIAN_POINT ( 'NONE',  ( 178.4123150140798941, 290.7538431597592421, 9.991683058491686253 ) ) ;
#94136 = CARTESIAN_POINT ( 'NONE',  ( -2.160980794731546695, 162.8927522451417929, -10.00000000000009237 ) ) ;
#94137 = SURFACE_STYLE_FILL_AREA ( #72831 ) ;
#94138 = EDGE_CURVE ( 'NONE', #63494, #47254, #40914, .T. ) ;
#94139 = CARTESIAN_POINT ( 'NONE',  ( 157.1338510812060747, 258.4831816688264325, 17.88958125218800888 ) ) ;
#94140 = DIRECTION ( 'NONE',  ( 0.000000000000000000, 0.000000000000000000, 1.000000000000000000 ) ) ;
#94141 = DIRECTION ( 'NONE',  ( -0.3715724127386920705, 0.6435822975543701308, -0.6691306063588670083 ) ) ;
#94142 = ADVANCED_FACE ( 'NONE', ( #87112 ), #86599, .T. ) ;
#94143 = CARTESIAN_POINT ( 'NONE',  ( 46.56214281575564939, 191.5643266524159856, -9.188101187500093303 ) ) ;
#94144 = EDGE_CURVE ( 'NONE', #93491, #51674, #85688, .T. ) ;
#94145 = EDGE_CURVE ( 'NONE', #16902, #95220, #38926, .T. ) ;
#94146 = CARTESIAN_POINT ( 'NONE',  ( 72.70511114461589841, 212.7833772461660544, -9.188101187500095079 ) ) ;
#94147 = CARTESIAN_POINT ( 'NONE',  ( 57.23161641937173982, 215.3967562850347122, -4.648177544792955347E-16 ) ) ;
#94148 = CARTESIAN_POINT ( 'NONE',  ( 88.34978748912247681, 44.19151614600375666, -0.08427336824597120302 ) ) ;
#94149 = CARTESIAN_POINT ( 'NONE',  ( 167.2874460902532689, 259.7876024158500741, 16.17904535958410150 ) ) ;
#94151 = CARTESIAN_POINT ( 'NONE',  ( 77.63584588586775226, 49.30200881430058502, 15.29451607107652222 ) ) ;
#94150 = CARTESIAN_POINT ( 'NONE',  ( 79.36263291408793918, 45.67866562566761957, -12.88899626193393999 ) ) ;
#94152 = CARTESIAN_POINT ( 'NONE',  ( 196.5459883665041332, 268.9076809661281686, -10.53567312597886563 ) ) ;
#94153 = CARTESIAN_POINT ( 'NONE',  ( 22.53213034355507460, 33.98502408145593279, -5.678558825948271327 ) ) ;
#94154 = CARTESIAN_POINT ( 'NONE',  ( 151.0801312611820890, 268.9685319718947198, -15.83903210480701240 ) ) ;
#94155 = CARTESIAN_POINT ( 'NONE',  ( 149.2593905435863348, 272.1221474021800759, -12.98626158366800176 ) ) ;
#94156 = CARTESIAN_POINT ( 'NONE',  ( 6.742211794378569323, 25.93396525600388003, 2.839279412974139660 ) ) ;
#94157 = CARTESIAN_POINT ( 'NONE',  ( 61.47358386746269332, 215.4869531367911009, 4.594050593750046652 ) ) ;
#94158 = CARTESIAN_POINT ( 'NONE',  ( 80.87517248313827167, 58.64441083166272506, 0.000000000000000000 ) ) ;
#94159 = DIRECTION ( 'NONE',  ( 0.4999999999999992784, -0.8660254037844390407, 0.000000000000000000 ) ) ;
#94160 = CARTESIAN_POINT ( 'NONE',  ( 159.4574711498080433, 254.4585536525209477, 16.86100557095418395 ) ) ;
#94161 = CARTESIAN_POINT ( 'NONE',  ( 69.47037063557095848, 62.62442318441491551, -13.85991542342858018 ) ) ;
#94162 = CARTESIAN_POINT ( 'NONE',  ( 154.1156850538427250, 263.7107985738977618, 17.28418349447918700 ) ) ;
#94163 = AXIS2_PLACEMENT_3D ( 'NONE', #87223, #87721, #51007 ) ;
#94164 = CARTESIAN_POINT ( 'NONE',  ( 77.84895608869516082, 55.91079568154652435, -16.15415909428238095 ) ) ;
#94165 = CARTESIAN_POINT ( 'NONE',  ( 87.60351575088976972, 45.13338919493600798, -6.137684345434423427 ) ) ;
#94166 = CARTESIAN_POINT ( 'NONE',  ( 101.8522786425098445, 239.6115022471902876, -5.000000000000047962 ) ) ;
#94167 = CARTESIAN_POINT ( 'NONE',  ( 82.66777534753497036, 40.88273136530058594, 3.288167606880421090 ) ) ;
#94168 = CARTESIAN_POINT ( 'NONE',  ( 164.2578067403839555, 246.1441285162624126, -2.322300236470859591 ) ) ;
#94169 = ORIENTED_EDGE ( 'NONE', *, *, #82570, .F. ) ;
#94170 = CARTESIAN_POINT ( 'NONE',  ( 77.45223888989086447, 49.57236342607031787, 14.91341569047779281 ) ) ;
#94171 = CARTESIAN_POINT ( 'NONE',  ( 188.1310009398110878, 273.3760639908985581, 15.63936761710383827 ) ) ;
#94172 = EDGE_LOOP ( 'NONE', ( #93302, #823, #95337, #81955 ) ) ;
#94173 = CARTESIAN_POINT ( 'NONE',  ( 159.5895502557670795, 254.2297859303815244, -16.92708575547316485 ) ) ;
#94174 = B_SPLINE_CURVE_WITH_KNOTS ( 'NONE', 3,
 ( #53133, #91669, #30335, #61225 ),
 .UNSPECIFIED., .F., .F.,
 ( 4, 4 ),
 ( 0.02770447213199976264, 0.03690780161571044493 ),
 .UNSPECIFIED. ) ;
#94175 = CARTESIAN_POINT ( 'NONE',  ( 190.3874097485314394, 278.8119828322884928, -16.52278601034964112 ) ) ;
#94176 = CARTESIAN_POINT ( 'NONE',  ( 69.72007715475741918, 68.87520295995811637, -7.276862800964089217 ) ) ;
#94177 = VERTEX_POINT ( 'NONE', #62722 ) ;
#94178 = CARTESIAN_POINT ( 'NONE',  ( 177.2494136933412108, 252.9521367768340383, -0.2656116247643500183 ) ) ;
#94179 = VERTEX_POINT ( 'NONE', #39912 ) ;
#94180 = CARTESIAN_POINT ( 'NONE',  ( 79.46801687855551677, 46.39187830138592972, -12.72948678403309053 ) ) ;
#94181 = CARTESIAN_POINT ( 'NONE',  ( 170.0689406639716879, 250.0722447876482875, 3.416113949011092110 ) ) ;
#94182 = DIRECTION ( 'NONE',  ( -0.9923183454821337124, -0.1237105541964824140, 0.000000000000000000 ) ) ;
#94183 = ORIENTED_EDGE ( 'NONE', *, *, #10962, .F. ) ;
#94184 = CARTESIAN_POINT ( 'NONE',  ( 20.10065364775352847, 33.64646525600390703, -2.839279412974133887 ) ) ;
#94185 = CARTESIAN_POINT ( 'NONE',  ( 79.74133107861359804, 44.86189080207443425, 11.44794314671259627 ) ) ;
#94186 = CARTESIAN_POINT ( 'NONE',  ( 82.86586985908988368, 152.2544130683315871, 0.000000000000000000 ) ) ;
#94187 = CARTESIAN_POINT ( 'NONE',  ( 75.32434183498538971, 66.62165581190093633, -13.06803771652694834 ) ) ;
#94188 = CARTESIAN_POINT ( 'NONE',  ( 78.66149435155034553, 49.46989482002797445, -14.61922007752083452 ) ) ;
#94189 = ORIENTED_EDGE ( 'NONE', *, *, #37322, .F. ) ;
#94190 = CARTESIAN_POINT ( 'NONE',  ( -32.10208857249643444, 42.85342256331377087, 59.99999999999999289 ) ) ;
#94191 = CARTESIAN_POINT ( 'NONE',  ( 206.6268150440956504, 272.7588534679261443, -10.76664753678610609 ) ) ;
#94192 = ORIENTED_EDGE ( 'NONE', *, *, #42973, .T. ) ;
#94193 = CARTESIAN_POINT ( 'NONE',  ( 171.8003058497035624, 285.7827424729591712, 11.35508565917934654 ) ) ;
#94195 = CARTESIAN_POINT ( 'NONE',  ( 67.95186835949662907, 65.47617292293909941, -10.34303067525367226 ) ) ;
#94194 = CARTESIAN_POINT ( 'NONE',  ( 67.80686942989439103, 65.67079667550257227, 10.79604664877636289 ) ) ;
#94196 = CARTESIAN_POINT ( 'NONE',  ( 81.76515281898197429, 55.59664093367394599, -15.96652640277710766 ) ) ;
#94197 = CARTESIAN_POINT ( 'NONE',  ( 180.4218656208765310, 293.5880668416769481, 7.617716764297705723 ) ) ;
#94198 = CARTESIAN_POINT ( 'NONE',  ( 41.38738224522862907, 24.86426979415093186, -3.090169943749474069 ) ) ;
#94199 = CARTESIAN_POINT ( 'NONE',  ( 157.8811243250769110, 257.1888664433053009, -17.39256699147873064 ) ) ;
#94200 = CARTESIAN_POINT ( 'NONE',  ( 142.6909626358283560, 247.0643266524159856, -9.188101187500093303 ) ) ;
#94201 = CARTESIAN_POINT ( 'NONE',  ( 205.7955998042208421, 270.2654991239114111, 2.441702357542676616 ) ) ;
#94202 = CARTESIAN_POINT ( 'NONE',  ( 79.04010335995445757, 59.81086823702358402, 16.49488376190979366 ) ) ;
#94203 = CARTESIAN_POINT ( 'NONE',  ( 90.72909131299699936, 229.3149278399160949, -9.188101187500095079 ) ) ;
#94204 = ORIENTED_EDGE ( 'NONE', *, *, #95871, .T. ) ;
#94205 = CARTESIAN_POINT ( 'NONE',  ( 190.7851751463332164, 300.1973786460605425, 8.237717828100052486 ) ) ;
#94206 = CARTESIAN_POINT ( 'NONE',  ( 78.17919853682799669, 61.76234676664309120, -16.10619035535653509 ) ) ;
#94207 = EDGE_CURVE ( 'NONE', #83607, #72764, #70845, .T. ) ;
#94208 = ORIENTED_EDGE ( 'NONE', *, *, #64950, .T. ) ;
#94209 = CARTESIAN_POINT ( 'NONE',  ( 157.4595529495266533, 257.9190494847748027, -17.35536051855973838 ) ) ;
#94210 = ORIENTED_EDGE ( 'NONE', *, *, #22281, .F. ) ;
#94211 = CARTESIAN_POINT ( 'NONE',  ( 80.35890605665858288, 44.73641450380378615, -11.69935222326590640 ) ) ;
#94212 = CARTESIAN_POINT ( 'NONE',  ( 67.16327201103491973, 67.73731889023999031, 6.573435314091262249 ) ) ;
#94214 = B_SPLINE_SURFACE_WITH_KNOTS ( 'NONE', 3, 1, ( 
 ( #25951, #56320 ),
 ( #33539, #79681 ),
 ( #10243, #54821 ),
 ( #41112, #72046 ),
 ( #71345, #24720 ),
 ( #1445, #77943 ),
 ( #38915, #63729 ),
 ( #77446, #55602 ),
 ( #70319, #933 ),
 ( #39901, #15610 ),
 ( #7519, #47026 ),
 ( #78447, #31319 ),
 ( #1936, #38412 ),
 ( #24232, #94168 ),
 ( #46508, #56110 ),
 ( #32822, #70833 ),
 ( #69820, #32325 ),
 ( #8532, #31809 ),
 ( #39404, #94665 ),
 ( #9029, #431 ),
 ( #69327, #93159 ),
 ( #62207, #23709 ),
 ( #63226, #100248 ),
 ( #86587, #87100 ),
 ( #62709, #85062 ),
 ( #17122, #25223 ),
 ( #46002, #61716 ),
 ( #8042, #54603 ),
 ( #48018, #30830 ),
 ( #93668, #54105 ),
 ( #76920, #92663 ),
 ( #78961, #9549 ),
 ( #55110, #85587 ),
 ( #16128, #16623 ) ),
 .UNSPECIFIED., .T., .F., .F.,
 ( 4, 2, 2, 2, 2, 2, 2, 2, 2, 2, 2, 2, 2, 2, 2, 2, 4 ),
 ( 2, 2 ),
 ( 0.000000000000000000, 0.06250000000000000000, 0.1250000000000000000, 0.1875000000000000000, 0.2500000000000000000, 0.3125000000000000000, 0.3750000000000000000, 0.4375000000000000000, 0.5000000000000000000, 0.5625000000000000000, 0.6250000000000000000, 0.6875000000000000000, 0.7500000000000000000, 0.8125000000000000000, 0.8750000000000000000, 0.9375000000000000000, 1.000000000000000000 ),
 ( 0.000000000000000000, 1.000000000000000000 ),
 .UNSPECIFIED. ) ;
#94213 = DIRECTION ( 'NONE',  ( 0.5609510170580086497, 0.8278489937552534483, 0.000000000000000000 ) ) ;
#94215 = CARTESIAN_POINT ( 'NONE',  ( 37.16144446923997435, 23.58380873178789727, 6.180339887498953466 ) ) ;
#94216 = CARTESIAN_POINT ( 'NONE',  ( 84.05270344386845238, 47.46752220604140859, -11.66933861446510079 ) ) ;
#94217 = CARTESIAN_POINT ( 'NONE',  ( 84.12564760914067108, 225.5024278399160664, 9.188101187500095079 ) ) ;
#94218 = ORIENTED_EDGE ( 'NONE', *, *, #14534, .F. ) ;
#94219 = EDGE_CURVE ( 'NONE', #54945, #77851, #33340, .T. ) ;
#94220 = ORIENTED_EDGE ( 'NONE', *, *, #44208, .F. ) ;
#94221 = DIRECTION ( 'NONE',  ( -0.6879669212057208938, -0.7257420446182799578, 0.000000000000000000 ) ) ;
#94222 = AXIS2_PLACEMENT_3D ( 'NONE', #89317, #19872, #81694 ) ;
#94223 = CARTESIAN_POINT ( 'NONE',  ( 200.3254990932456110, 283.6730528493424117, -17.74520030754218780 ) ) ;
#94224 = VERTEX_POINT ( 'NONE', #71862 ) ;
#94225 = EDGE_CURVE ( 'NONE', #96030, #76205, #47381, .T. ) ;
#94226 = CARTESIAN_POINT ( 'NONE',  ( 76.17858836466767514, 64.76715759548049789, -14.35676355172211238 ) ) ;
#94227 = CARTESIAN_POINT ( 'NONE',  ( 163.1501015339556773, 284.1938231124877916, 0.5074629045209336775 ) ) ;
#94228 = CARTESIAN_POINT ( 'NONE',  ( 109.2134945746776538, 223.8615022471902023, 5.000000000000051514 ) ) ;
#94229 = CARTESIAN_POINT ( 'NONE',  ( 45.16679497745494132, 120.1723871950187714, -10.00000000000000000 ) ) ;
#94230 = ORIENTED_EDGE ( 'NONE', *, *, #37322, .T. ) ;
#94231 = CARTESIAN_POINT ( 'NONE',  ( 85.75565660721923678, 43.84343610033825200, -5.420381390687177614 ) ) ;
#94232 = CARTESIAN_POINT ( 'NONE',  ( 185.1813530213977685, 260.2351280040860502, 6.311033929732698944 ) ) ;
#94233 = CARTESIAN_POINT ( 'NONE',  ( 159.9997000813754084, 253.5193855937126841, -16.28798248637880519 ) ) ;
#94234 = CARTESIAN_POINT ( 'NONE',  ( -27.42236680055714260, 166.5217562850347406, 1.224646799147364892E-15 ) ) ;
#94235 = CARTESIAN_POINT ( 'NONE',  ( 153.1983976505312626, 265.2995869615763809, -17.69657798691567763 ) ) ;
#94236 = DIRECTION ( 'NONE',  ( 0.4737039832092607705, 0.8806841296921844586, 0.000000000000000000 ) ) ;
#94237 = DIRECTION ( 'NONE',  ( 0.3782958374750613473, 0.000000000000000000, -0.9256847516023162248 ) ) ;
#94238 = ORIENTED_EDGE ( 'NONE', *, *, #52985, .T. ) ;
#94239 = DIRECTION ( 'NONE',  ( -0.000000000000000000, -0.000000000000000000, -1.000000000000000000 ) ) ;
#94240 = CARTESIAN_POINT ( 'NONE',  ( 200.2316334480823912, 283.8356329158505105, 17.02791935830326508 ) ) ;
#94241 = CARTESIAN_POINT ( 'NONE',  ( 85.92630256486899043, 44.97195868260131846, 7.553312411822113326 ) ) ;
#94242 = CARTESIAN_POINT ( 'NONE',  ( 171.2441523153178480, 251.6414079514013338, 7.096601279279188823 ) ) ;
#94243 = CARTESIAN_POINT ( 'NONE',  ( 83.67285453873573431, 52.00132685099405450, 14.98825055830738329 ) ) ;
#94244 = CARTESIAN_POINT ( 'NONE',  ( 174.9183164536166259, 290.4820404178226454, -6.477921979946556164 ) ) ;
#94245 = CARTESIAN_POINT ( 'NONE',  ( 153.0416928436757189, 270.7721196883188099, 13.91023073786846531 ) ) ;
#94246 = ORIENTED_EDGE ( 'NONE', *, *, #77543, .T. ) ;
#94247 = CARTESIAN_POINT ( 'NONE',  ( 181.0193311394079103, 261.5502185760933003, 13.24438261311760812 ) ) ;
#94248 = CARTESIAN_POINT ( 'NONE',  ( -17.12851661768869604, 103.0207181397640284, 44.62810345821594638 ) ) ;
#94249 = CARTESIAN_POINT ( 'NONE',  ( 74.87853038332181654, 63.73010615337872053, -14.43890213384147003 ) ) ;
#94251 = FACE_BOUND ( 'NONE', #2228, .T. ) ;
#94250 = CARTESIAN_POINT ( 'NONE',  ( 180.5685635681490737, 266.8160690160535182, -14.77224249148190971 ) ) ;
#94252 = CARTESIAN_POINT ( 'NONE',  ( 69.81243019392553606, 62.22010195957141576, -13.63492759933605392 ) ) ;
#94253 = EDGE_CURVE ( 'NONE', #9430, #25628, #442, .T. ) ;
#94254 = CARTESIAN_POINT ( 'NONE',  ( 22.35729902920393997, 37.00034080476290654, -1.878358725466461243E-16 ) ) ;
#94255 = CARTESIAN_POINT ( 'NONE',  ( 183.4832052704994965, 274.8226554140247799, 16.36505719518536495 ) ) ;
#94256 = CARTESIAN_POINT ( 'NONE',  ( 178.2338095707201262, 261.7061032656386601, -14.47991691129509206 ) ) ;
#94257 = CARTESIAN_POINT ( 'NONE',  ( 191.5691986906763873, 262.2710266103114805, 2.934180375091335335 ) ) ;
#94258 = CARTESIAN_POINT ( 'NONE',  ( 161.8926315922002743, 250.2407320417157166, -13.77020595223768495 ) ) ;
#94259 = CARTESIAN_POINT ( 'NONE',  ( 3.071516343397128423, 163.3923013555410080, 4.594050593750050204 ) ) ;
#94260 = CARTESIAN_POINT ( 'NONE',  ( 81.67192807023319290, 46.29478322961348624, 11.76198625675847431 ) ) ;
#94261 = ORIENTED_EDGE ( 'NONE', *, *, #64204, .F. ) ;
#94262 = EDGE_CURVE ( 'NONE', #7411, #26733, #55468, .T. ) ;
#94263 = CARTESIAN_POINT ( 'NONE',  ( 176.1749608394459301, 255.9580892509862906, 8.247052548410042760 ) ) ;
#94264 = LINE ( 'NONE', #55694, #35419 ) ;
#94265 = FACE_OUTER_BOUND ( 'NONE', #82017, .T. ) ;
#94266 = CARTESIAN_POINT ( 'NONE',  ( 21.98867198337220330, 177.3768266524160140, 9.188101187500096856 ) ) ;
#94267 = CIRCLE ( 'NONE', #97520, 16.60714546451156082 ) ;
#94268 = DIRECTION ( 'NONE',  ( 1.000000000000000000, 0.000000000000000000, 0.000000000000000000 ) ) ;
#94269 = CARTESIAN_POINT ( 'NONE',  ( 29.53625146412516500, 35.79103043416551344, 8.090169943749478065 ) ) ;
#94270 = CARTESIAN_POINT ( 'NONE',  ( 178.5328262458293693, 291.6488152232226980, 5.998782872725313631 ) ) ;
#94271 = CARTESIAN_POINT ( 'NONE',  ( 147.3047606266276546, 275.5076657283461827, -0.02269072295920609994 ) ) ;
#94272 = CARTESIAN_POINT ( 'NONE',  ( 72.87667924365860017, 65.01085463311059698, 13.62852699864587969 ) ) ;
#94273 = CARTESIAN_POINT ( 'NONE',  ( 81.42628347097989661, 41.97763379937408956, 7.709395309255075546 ) ) ;
#94274 = CARTESIAN_POINT ( 'NONE',  ( 186.7692638048808362, 295.9158464710309886, -8.508718364155994252 ) ) ;
#94275 = AXIS2_PLACEMENT_3D ( 'NONE', #31772, #69785, #395 ) ;
#94276 = CARTESIAN_POINT ( 'NONE',  ( 91.91334042722833431, 212.3262482093457493, 3.021315404115420679E-15 ) ) ;
#94277 = CARTESIAN_POINT ( 'NONE',  ( 62.37595398666918101, 213.4865022471903160, 10.00000000000009237 ) ) ;
#94278 = CARTESIAN_POINT ( 'NONE',  ( 68.69958519936569985, 66.83058884119587617, -9.320282762443202529 ) ) ;
#94279 = DIRECTION ( 'NONE',  ( 1.000000000000000000, 1.804112415015878984E-15, 0.000000000000000000 ) ) ;
#94280 = DIRECTION ( 'NONE',  ( 1.000000000000000000, 0.000000000000000000, 0.000000000000000000 ) ) ;
#94281 = CARTESIAN_POINT ( 'NONE',  ( 30.29666933122289407, 197.4869531367911293, 4.594050593750046652 ) ) ;
#94282 = DIRECTION ( 'NONE',  ( -0.8660254037844387076, -0.4999999999999998890, -0.000000000000000000 ) ) ;
#94283 = DIRECTION ( 'NONE',  ( 0.9171038997749326738, -0.3986482622784278118, 0.000000000000000000 ) ) ;
#94284 = CARTESIAN_POINT ( 'NONE',  ( 199.1867231605587278, 285.6454706231928071, -17.41989184023605475 ) ) ;
#94285 = CARTESIAN_POINT ( 'NONE',  ( 67.35308227982150697, 66.38192671655097854, -8.894446999883845351 ) ) ;
#94286 = EDGE_LOOP ( 'NONE', ( #68614, #70842, #2449 ) ) ;
#94288 = CARTESIAN_POINT ( 'NONE',  ( 78.01622611019826081, 227.3967562850346837, -4.648177544792955347E-16 ) ) ;
#94287 = VECTOR ( 'NONE', #26921, 1000.000000000000114 ) ;
#94289 = CARTESIAN_POINT ( 'NONE',  ( 51.80235952159636525, 85.00000000000000000, 59.99999999999999289 ) ) ;
#94290 = B_SPLINE_CURVE_WITH_KNOTS ( 'NONE', 3,
 ( #53607, #45011, #76441, #37408, #52115, #6533, #36918, #83566, #30324, #83062, #98752, #91158, #13635, #61212, #84566, #75956, #15104, #35920, #97749, #59196, #28317, #90172, #5529, #20745, #51631, #13146, #98245, #44509, #59714, #29332, #60198, #21724, #52608, #87092, #39894, #54099, #70828, #25216, #86093, #38909, #23702, #9543, #77936, #17629, #93662, #85055 ),
 .UNSPECIFIED., .F., .F.,
 ( 4, 1, 1, 1, 2, 2, 1, 1, 1, 2, 2, 1, 1, 2, 2, 1, 1, 2, 2, 1, 1, 2, 2, 1, 2, 2, 1, 2, 2, 4 ),
 ( 0.000000000000000000, 0.06249999999998047395, 0.09374999999997075950, 0.1093749999999649170, 0.1171874999999624883, 0.1249999999999600597, 0.1874999999999578670, 0.2187499999999581446, 0.2343749999999596989, 0.2421874999999613365, 0.2499999999999629741, 0.3124999999999686362, 0.3437499999999719669, 0.3593749999999722444, 0.3749999999999725220, 0.4374999999999828471, 0.4687499999999875100, 0.4843749999999880096, 0.4999999999999884537, 0.5624999999999913403, 0.5937499999999945599, 0.6093749999999962252, 0.6249999999999978906, 0.6875000000000027756, 0.7187500000000056621, 0.7500000000000085487, 0.8125000000000102141, 0.8437500000000092149, 0.8750000000000082157, 1.000000000000000000 ),
 .UNSPECIFIED. ) ;
#94291 = CARTESIAN_POINT ( 'NONE',  ( -19.15453390681661716, 24.31945705462846163, -10.00000000000000000 ) ) ;
#94292 = DIRECTION ( 'NONE',  ( 0.9954067278227226589, -0.09573633691164461224, 0.000000000000000000 ) ) ;
#94293 = CARTESIAN_POINT ( 'NONE',  ( 27.77157046966360809, 18.96004757982091249, -5.678558825948276656 ) ) ;
#94294 = CARTESIAN_POINT ( 'NONE',  ( 163.3543347837650686, 247.7089878483399730, 10.92686688779373405 ) ) ;
#94295 = CARTESIAN_POINT ( 'NONE',  ( 196.6317700900902139, 290.0707791521982131, -17.91116578096951883 ) ) ;
#94296 = CARTESIAN_POINT ( 'NONE',  ( 185.8360495164496626, 267.6137447244977920, -14.93125900359994063 ) ) ;
#94297 = ORIENTED_EDGE ( 'NONE', *, *, #64706, .F. ) ;
#94298 = CARTESIAN_POINT ( 'NONE',  ( 34.69457829350510281, 43.52903772873360566, -1.583844403245329602 ) ) ;
#94299 = CARTESIAN_POINT ( 'NONE',  ( 4.795442299662375341, 20.95586893147752861, 7.433330006724141015 ) ) ;
#94300 = CARTESIAN_POINT ( 'NONE',  ( 198.0816276881963915, 264.5915495180347534, -1.723934393811154182E-14 ) ) ;
#94301 = CARTESIAN_POINT ( 'NONE',  ( 74.84764555390079011, 59.32158413457844404, -15.77185916182937575 ) ) ;
#94302 = CARTESIAN_POINT ( 'NONE',  ( 71.72790558683757922, 72.47596629505412125, -1.350878852920679662 ) ) ;
#94303 = VERTEX_POINT ( 'NONE', #41936 ) ;
#94305 = FACE_OUTER_BOUND ( 'NONE', #21870, .T. ) ;
#94304 = SHAPE_REPRESENTATION ( 'Screw Retaining Piece Part', ( #68784 ), #54221 ) ;
#94306 = CARTESIAN_POINT ( 'NONE',  ( 178.8278557635266566, 282.3355866844354409, 15.39618937652901742 ) ) ;
#94307 = CARTESIAN_POINT ( 'NONE',  ( 85.47555641224485612, 49.06903847834369969, 12.34201857654865542 ) ) ;
#94308 = CARTESIAN_POINT ( 'NONE',  ( 181.1193550619148311, 257.2754919020080138, -7.706538992632681051 ) ) ;
#94309 = CARTESIAN_POINT ( 'NONE',  ( 190.1751179328237242, 301.2540287353828035, 3.252640783176552475 ) ) ;
#94310 = ORIENTED_EDGE ( 'NONE', *, *, #7043, .F. ) ;
#94311 = VERTEX_POINT ( 'NONE', #12050 ) ;
#94313 = FILL_AREA_STYLE_COLOUR ( '', #92893 ) ;
#94312 = CARTESIAN_POINT ( 'NONE',  ( 207.8718670335145475, 270.6023601641878713, -6.322166851501095586 ) ) ;
#94314 = ORIENTED_EDGE ( 'NONE', *, *, #45141, .T. ) ;
#94315 = CARTESIAN_POINT ( 'NONE',  ( 30.77278128771378007, 63.06390461086555632, 59.99999999999999289 ) ) ;
#94316 = CARTESIAN_POINT ( 'NONE',  ( 72.75640829328646930, 57.27960352001080224, -15.87147226852406234 ) ) ;
#94317 = LINE ( 'NONE', #78596, #40241 ) ;
#94318 = CARTESIAN_POINT ( 'NONE',  ( 205.3465787480556344, 274.9762877783610406, -13.79319041940166279 ) ) ;
#94319 = CARTESIAN_POINT ( 'NONE',  ( 104.8295012880686699, 222.1423013555409796, -4.594050593750043987 ) ) ;
#94320 = CARTESIAN_POINT ( 'NONE',  ( 180.4037401415526460, 287.2066285221069961, -13.85796317411490719 ) ) ;
#94321 = EDGE_CURVE ( 'NONE', #79865, #66165, #96181, .T. ) ;
#94322 = ORIENTED_EDGE ( 'NONE', *, *, #64364, .T. ) ;
#94323 = LINE ( 'NONE', #69970, #44537 ) ;
#94324 = ORIENTED_EDGE ( 'NONE', *, *, #75314, .T. ) ;
#94325 = CARTESIAN_POINT ( 'NONE',  ( 22.55378097864968012, 33.99752408145592852, 5.678558825948277544 ) ) ;
#94326 = CARTESIAN_POINT ( 'NONE',  ( 157.1285250363530679, 258.9546388635270091, 16.90635852484395940 ) ) ;
#94327 = CARTESIAN_POINT ( 'NONE',  ( 78.32185800947360121, 47.85121949867834701, -14.51427106730122141 ) ) ;
#94328 = EDGE_CURVE ( 'NONE', #37845, #23277, #10550, .T. ) ;
#94329 = CARTESIAN_POINT ( 'NONE',  ( 55.81761577081934433, 203.0333772461660544, 9.188101187500095079 ) ) ;
#94330 = CARTESIAN_POINT ( 'NONE',  ( 73.86986929274216607, 68.54753403896816621, 10.89714278534122549 ) ) ;
#94331 = CARTESIAN_POINT ( 'NONE',  ( 190.8443993347725325, 300.0947993426467519, 8.522468760355437212 ) ) ;
#94332 = CARTESIAN_POINT ( 'NONE',  ( 150.2761558193201381, 270.3610582852369930, 14.81920478290713028 ) ) ;
#94333 = CARTESIAN_POINT ( 'NONE',  ( 174.3168710180726464, 271.9212240863662373, 16.46052307220685762 ) ) ;
#94334 = EDGE_LOOP ( 'NONE', ( #15257, #37599, #92432, #54027 ) ) ;
#94335 = CARTESIAN_POINT ( 'NONE',  ( 190.8842374621117699, 299.6106664202726506, 5.533255903905391015 ) ) ;
#94336 = PLANE ( 'NONE',  #12113 ) ;
#94337 = CARTESIAN_POINT ( 'NONE',  ( -52.57320609282758994, 32.70376883311632810, -10.00000000000000000 ) ) ;
#94338 = ORIENTED_EDGE ( 'NONE', *, *, #64505, .T. ) ;
#94339 = CARTESIAN_POINT ( 'NONE',  ( 108.4196379545418978, 226.7365022471902591, -10.00000000000009237 ) ) ;
#94340 = CARTESIAN_POINT ( 'NONE',  ( 68.23957855939767114, 69.39062747421131405, -4.093039667954597505 ) ) ;
#94341 = EDGE_CURVE ( 'NONE', #33367, #40898, #100190, .T. ) ;
#94342 = CARTESIAN_POINT ( 'NONE',  ( 207.6129110656513035, 271.0508850574501025, -5.265106572941297358 ) ) ;
#94343 = CARTESIAN_POINT ( 'NONE',  ( 146.9700173529739970, 276.0874580858064746, -5.099093031535578469 ) ) ;
#94344 = CARTESIAN_POINT ( 'NONE',  ( 21.20245638554209222, 36.22472881207375650, -10.00000000000000000 ) ) ;
#94345 = CIRCLE ( 'NONE', #74882, 10.00000000000001066 ) ;
#94346 = CARTESIAN_POINT ( 'NONE',  ( 82.96854302488638666, 41.23096503478176089, -0.6813192392769399364 ) ) ;
#94347 = CARTESIAN_POINT ( 'NONE',  ( 81.82036482989325066, 42.35048943672428834, -7.944650131338358179 ) ) ;
#94348 = CARTESIAN_POINT ( 'NONE',  ( 67.18318263371854471, 66.87162863476784480, 8.978259895924134426 ) ) ;
#94349 = CARTESIAN_POINT ( 'NONE',  ( 71.00065756275667184, 65.38050944624951910, -12.04497808108590817 ) ) ;
#94350 = DIRECTION ( 'NONE',  ( -0.8660254037844387076, -0.4999999999999998890, -0.000000000000000000 ) ) ;
#94351 = CARTESIAN_POINT ( 'NONE',  ( 114.2743305262689404, 236.7833772461660544, -9.188101187500095079 ) ) ;
#94352 = ORIENTED_EDGE ( 'NONE', *, *, #85582, .T. ) ;
#94353 = CARTESIAN_POINT ( 'NONE',  ( 147.1447476476323004, 275.7848163378367872, 0.6373001129109078233 ) ) ;
#94354 = CARTESIAN_POINT ( 'NONE',  ( 69.42144788871625849, 62.89730317705431872, 13.10748580973936939 ) ) ;
#94355 = AXIS2_PLACEMENT_3D ( 'NONE', #62043, #32163, #33172 ) ;
#94356 = CARTESIAN_POINT ( 'NONE',  ( 203.5629025532486196, 278.0657055720176913, -15.85226727704602823 ) ) ;
#94357 = EDGE_CURVE ( 'NONE', #12913, #75751, #76818, .T. ) ;
#94358 = CARTESIAN_POINT ( 'NONE',  ( 19.39999966495784989, 36.48715600906564305, 10.00000000000000000 ) ) ;
#94359 = CARTESIAN_POINT ( 'NONE',  ( 87.62133583293774564, 45.31115884160843876, -7.293173845241961217 ) ) ;
#94360 = CARTESIAN_POINT ( 'NONE',  ( 178.0841129145181583, 255.3396897122842688, 4.676894877019703856 ) ) ;
#94361 = ORIENTED_EDGE ( 'NONE', *, *, #37923, .F. ) ;
#94362 = CARTESIAN_POINT ( 'NONE',  ( 80.39015929397758953, 57.47250276623566378, -16.58917374605577777 ) ) ;
#94363 = CARTESIAN_POINT ( 'NONE',  ( 156.8878975079533973, 274.1353535065238702, -12.64326179356356938 ) ) ;
#94364 = CARTESIAN_POINT ( 'NONE',  ( 182.1031022951341640, 260.5023910914902103, 9.513370520185286949 ) ) ;
#94365 = CARTESIAN_POINT ( 'NONE',  ( 74.63372323989780455, 66.93453420673688470, 13.02704161780705938 ) ) ;
#94366 = CARTESIAN_POINT ( 'NONE',  ( 130.0789470495699618, 258.1589784336661637, -6.496448406907676862E-16 ) ) ;
#94367 = CARTESIAN_POINT ( 'NONE',  ( 190.2164219629064803, 294.6625793156072177, -12.31662424489765506 ) ) ;
#94368 = DIRECTION ( 'NONE',  ( -0.6123724356957923609, -0.3535533905932727317, 0.7071067811865499042 ) ) ;
#94369 = CARTESIAN_POINT ( 'NONE',  ( 188.9209837766938733, 282.1233005308658903, -16.64026405500985106 ) ) ;
#94370 = DIRECTION ( 'NONE',  ( 0.4999999999999992784, -0.8660254037844390407, 0.000000000000000000 ) ) ;
#94371 = CARTESIAN_POINT ( 'NONE',  ( 38.09089796528284211, 201.9869531367911293, 4.594050593750046652 ) ) ;
#94372 = CARTESIAN_POINT ( 'NONE',  ( 85.37572018521500183, 48.32884972269767587, -12.27680401939018751 ) ) ;
#94373 = CARTESIAN_POINT ( 'NONE',  ( 87.90135287304421752, 44.47855560518080154, -3.950668869199154720 ) ) ;
#94374 = ADVANCED_FACE ( 'NONE', ( #14533 ), #38304, .T. ) ;
#94375 = CARTESIAN_POINT ( 'NONE',  ( 167.0847919564587585, 251.8796711988679533, 11.83011900582259557 ) ) ;
#94376 = CARTESIAN_POINT ( 'NONE',  ( 173.4258591900324689, 261.5801875239348533, 14.40537091172031658 ) ) ;
#94377 = CARTESIAN_POINT ( 'NONE',  ( 151.6587809176374719, 278.2529691159808749, -1.644010740688682581 ) ) ;
#94378 = CARTESIAN_POINT ( 'NONE',  ( 178.8774314082362196, 291.7284028483271072, -6.329699548260768083 ) ) ;
#94379 = CARTESIAN_POINT ( 'NONE',  ( 162.2336410148055279, 251.8862672885301492, -14.09881826716025799 ) ) ;
#94380 = CARTESIAN_POINT ( 'NONE',  ( 178.6939486350811421, 261.2861450363681683, 12.21674390882607852 ) ) ;
#94381 = ADVANCED_FACE ( 'NONE', ( #91071 ), #52517, .F. ) ;
#94382 = CARTESIAN_POINT ( 'NONE',  ( 84.27862564753039010, 50.65054004415126343, -13.76907720482496700 ) ) ;
#94383 = VERTEX_POINT ( 'NONE', #13058 ) ;
#94384 = EDGE_CURVE ( 'NONE', #64537, #80050, #22626, .T. ) ;
#94385 = CARTESIAN_POINT ( 'NONE',  ( 163.1484656051875106, 248.0655637253488806, 9.714247672444804138 ) ) ;
#94386 = CARTESIAN_POINT ( 'NONE',  ( 71.86256228778262312, 72.60615528678948749, -0.5650332253008888417 ) ) ;
#94387 = CARTESIAN_POINT ( 'NONE',  ( 32.08336737017582152, 180.1423013555409796, -4.594050593750043987 ) ) ;
#94388 = CARTESIAN_POINT ( 'NONE',  ( 13.42817895373461390, 26.49103043416548076, -8.090169943749479842 ) ) ;
#94389 = CARTESIAN_POINT ( 'NONE',  ( 188.7278402105932003, 290.4693834276403095, -14.85022589635486590 ) ) ;
#94390 = CARTESIAN_POINT ( 'NONE',  ( 190.2236813008869660, 301.1699145145108218, -5.401374690107298093 ) ) ;
#94391 = CARTESIAN_POINT ( 'NONE',  ( 83.42542119994749328, 51.64995580955419996, -14.90072893730333270 ) ) ;
#94392 = EDGE_CURVE ( 'NONE', #74173, #30217, #83345, .T. ) ;
#94394 = CARTESIAN_POINT ( 'NONE',  ( 54.85235828774393951, 209.1427522451419350, -10.00000000000009415 ) ) ;
#94393 = DIRECTION ( 'NONE',  ( 1.000000000000000000, 0.000000000000000000, 0.000000000000000000 ) ) ;
#94395 = CARTESIAN_POINT ( 'NONE',  ( 3.720166145283430925, 25.08080186712590276, -3.090169943749475845 ) ) ;
#94396 = CARTESIAN_POINT ( 'NONE',  ( 182.4242555483369586, 257.1454310557409144, 1.318756070452638429 ) ) ;
#94397 = DIRECTION ( 'NONE',  ( -0.2270762630343793331, 0.9738769792773321887, 0.000000000000000000 ) ) ;
#94398 = CARTESIAN_POINT ( 'NONE',  ( 162.0972708797375219, 251.7219848490821903, -12.96270428423550491 ) ) ;
#94399 = VERTEX_POINT ( 'NONE', #76344 ) ;
#94400 = CARTESIAN_POINT ( 'NONE',  ( 32.20940242151128530, 182.7365022471902307, 10.00000000000009592 ) ) ;
#94401 = FACE_OUTER_BOUND ( 'NONE', #56804, .T. ) ;
#94402 = CARTESIAN_POINT ( 'NONE',  ( 202.4017613376760494, 280.0768611521521620, 15.73960524502980540 ) ) ;
#94403 = CARTESIAN_POINT ( 'NONE',  ( 151.1618603905361624, 248.8923013555409796, 4.594050593750050204 ) ) ;
#94404 = CARTESIAN_POINT ( 'NONE',  ( 34.45502471548058310, 41.93396525600392977, 2.839279412974139660 ) ) ;
#94406 = CARTESIAN_POINT ( 'NONE',  ( 169.1454910628425807, 262.9544248868517684, 15.90528355961972551 ) ) ;
#94405 = CARTESIAN_POINT ( 'NONE',  ( 21.04740724657494866, 61.13308837878306434, 59.99999999999999289 ) ) ;
#94407 = DIRECTION ( 'NONE',  ( 1.000000000000000000, 0.000000000000000000, 0.000000000000000000 ) ) ;
#94408 = CARTESIAN_POINT ( 'NONE',  ( 35.22599450741489591, 22.19860640527294393, 2.839279412974134775 ) ) ;
#94409 = CARTESIAN_POINT ( 'NONE',  ( 164.8537203408104972, 245.1119758834023230, 2.926011033004258355 ) ) ;
#94410 = CARTESIAN_POINT ( 'NONE',  ( 183.5235222349306525, 257.1254191288140305, -1.613677778301620958 ) ) ;
#94411 = CARTESIAN_POINT ( 'NONE',  ( 65.90510710696692342, 68.96474564273314911, 2.468420138682963394 ) ) ;
#94412 = ORIENTED_EDGE ( 'NONE', *, *, #33031, .F. ) ;
#94413 = LINE ( 'NONE', #71598, #27754 ) ;
#94414 =( NAMED_UNIT ( * ) SI_UNIT ( $, .STERADIAN. ) SOLID_ANGLE_UNIT ( ) );
#94415 = CARTESIAN_POINT ( 'NONE',  ( 178.6224597485341974, 285.5496574381789401, 13.02649328767307502 ) ) ;
#94416 = CARTESIAN_POINT ( 'NONE',  ( 152.9587330967189871, 278.2315804880608425, -6.245711854568786414 ) ) ;
#94417 = CARTESIAN_POINT ( 'NONE',  ( 15.62556418158687244, 11.94754757982088123, 5.678558825948272215 ) ) ;
#94418 = CARTESIAN_POINT ( 'NONE',  ( 207.1057321044409605, 271.9293447867963209, 8.088836166795815075 ) ) ;
#94419 = FACE_OUTER_BOUND ( 'NONE', #99395, .T. ) ;
#94420 = CARTESIAN_POINT ( 'NONE',  ( 206.8313602288537538, 272.4045708154811791, -9.607337080360906612 ) ) ;
#94421 = AXIS2_PLACEMENT_3D ( 'NONE', #93667, #8531, #86586 ) ;
#94422 = LINE ( 'NONE', #62458, #16643 ) ;
#94423 = CARTESIAN_POINT ( 'NONE',  ( 89.43128961965948065, 210.8932355074535678, -2.679491924311248496 ) ) ;
#94424 = CARTESIAN_POINT ( 'NONE',  ( 66.06796213254585837, 68.60782010546279253, 4.332213670276926720 ) ) ;
#94425 = CARTESIAN_POINT ( 'NONE',  ( 162.7007457333762090, 248.8410372908842021, -10.94671474643812914 ) ) ;
#94426 = CARTESIAN_POINT ( 'NONE',  ( 193.7706395672514645, 295.0264025848412075, 15.16938698680137065 ) ) ;
#94427 = EDGE_LOOP ( 'NONE', ( #73108, #62247, #3226 ) ) ;
#94428 = ORIENTED_EDGE ( 'NONE', *, *, #92983, .F. ) ;
#94429 = CARTESIAN_POINT ( 'NONE',  ( 138.2253456014563255, 240.6115022471902023, -5.000000000000041744 ) ) ;
#94430 = VECTOR ( 'NONE', #63593, 1000.000000000000227 ) ;
#94431 = CARTESIAN_POINT ( 'NONE',  ( 86.27668453731669729, 47.22199995466520761, 10.82669603042141304 ) ) ;
#94432 = ORIENTED_EDGE ( 'NONE', *, *, #25032, .T. ) ;
#94433 = DIRECTION ( 'NONE',  ( -1.000000000000000000, 0.000000000000000000, 0.000000000000000000 ) ) ;
#94434 = VERTEX_POINT ( 'NONE', #28228 ) ;
#94435 = CARTESIAN_POINT ( 'NONE',  ( 146.5502055023624735, 276.8145935406849389, 0.3770461397900869427 ) ) ;
#94436 = CARTESIAN_POINT ( 'NONE',  ( 79.48002332306521112, 59.20369081482913742, -16.22437187204984710 ) ) ;
#94437 = VECTOR ( 'NONE', #5808, 1000.000000000000000 ) ;
#94438 = CARTESIAN_POINT ( 'NONE',  ( 80.74974841597983755, 43.27611110042440146, 10.01619596034499260 ) ) ;
#94439 = ORIENTED_EDGE ( 'NONE', *, *, #87652, .F. ) ;
#94440 = CARTESIAN_POINT ( 'NONE',  ( 161.6707029936031574, 250.6251236501384483, 14.45053103226186231 ) ) ;
#94441 = CARTESIAN_POINT ( 'NONE',  ( 69.46659797204442555, 64.04447920839335495, -12.97926778662067093 ) ) ;
#94442 = CARTESIAN_POINT ( 'NONE',  ( 151.4025156491502742, 268.4101458323662541, 14.71049357081981235 ) ) ;
#94443 = CARTESIAN_POINT ( 'NONE',  ( 150.4141202964276260, 274.4678425752150019, -8.669812683062808389 ) ) ;
#94444 = B_SPLINE_SURFACE_WITH_KNOTS ( 'NONE', 3, 1, ( 
 ( #39289, #810 ),
 ( #55492, #17005 ),
 ( #31689, #1829 ),
 ( #32711, #63611 ),
 ( #27631, #65115 ),
 ( #33734, #71740 ),
 ( #95065, #87983 ),
 ( #81361, #96064 ),
 ( #64624, #2333 ),
 ( #96560, #72751 ),
 ( #95579, #26124 ),
 ( #10425, #66111 ),
 ( #41298, #18532 ),
 ( #41804, #3823 ),
 ( #72239, #80361 ),
 ( #19545, #56509 ),
 ( #97059, #50406 ),
 ( #49414, #50901 ),
 ( #81851, #64113 ),
 ( #19043, #25625 ),
 ( #10933, #34706 ),
 ( #3344, #57002 ),
 ( #65606, #87498 ),
 ( #11931, #80872 ),
 ( #58495, #34220 ),
 ( #2844, #18033 ),
 ( #42787, #89469 ),
 ( #26622, #12426 ),
 ( #73722, #20027 ),
 ( #27129, #57503 ),
 ( #4304, #88481 ),
 ( #49916, #33216 ),
 ( #35209, #48925 ),
 ( #79863, #11445 ) ),
 .UNSPECIFIED., .T., .F., .F.,
 ( 4, 2, 2, 2, 2, 2, 2, 2, 2, 2, 2, 2, 2, 2, 2, 2, 4 ),
 ( 2, 2 ),
 ( 0.000000000000000000, 0.06250000000000000000, 0.1250000000000000000, 0.1875000000000000000, 0.2500000000000000000, 0.3125000000000000000, 0.3750000000000000000, 0.4375000000000000000, 0.5000000000000000000, 0.5625000000000000000, 0.6250000000000000000, 0.6875000000000000000, 0.7500000000000000000, 0.8125000000000000000, 0.8750000000000000000, 0.9375000000000000000, 1.000000000000000000 ),
 ( 0.000000000000000000, 1.000000000000000000 ),
 .UNSPECIFIED. ) ;
#94445 = ORIENTED_EDGE ( 'NONE', *, *, #87882, .T. ) ;
#94446 = CARTESIAN_POINT ( 'NONE',  ( 171.2499256315726939, 254.4673999717836352, -11.80878994424205963 ) ) ;
#94447 = CARTESIAN_POINT ( 'NONE',  ( 163.2442700311756596, 247.8996255919473697, 11.14021925110252020 ) ) ;
#94448 = VERTEX_POINT ( 'NONE', #53017 ) ;
#94449 = ORIENTED_EDGE ( 'NONE', *, *, #3737, .F. ) ;
#94450 = CARTESIAN_POINT ( 'NONE',  ( 73.61601042510409343, 62.36123447726389202, 14.66634685749964184 ) ) ;
#94451 = VERTEX_POINT ( 'NONE', #90074 ) ;
#94452 = CARTESIAN_POINT ( 'NONE',  ( 161.0001838071895008, 271.1393494378992273, 16.41176471004197523 ) ) ;
#94453 = VERTEX_POINT ( 'NONE', #67224 ) ;
#94454 = CARTESIAN_POINT ( 'NONE',  ( 83.06160119771897143, 48.50967694913268247, 12.83647970848521425 ) ) ;
#94455 = CARTESIAN_POINT ( 'NONE',  ( 166.5798837419092706, 271.6578438917711082, 16.15769450769992233 ) ) ;
#94456 = CARTESIAN_POINT ( 'NONE',  ( 165.8975677354378035, 271.5909624305264174, 17.28637137770206067 ) ) ;
#94457 = CARTESIAN_POINT ( 'NONE',  ( 194.6782745185928434, 293.4543327343926080, -14.56555309295305634 ) ) ;
#94458 = EDGE_CURVE ( 'NONE', #95964, #3105, #53427, .T. ) ;
#94459 = CARTESIAN_POINT ( 'NONE',  ( 174.5497488978029423, 290.1244087063413417, 6.358272735726022695 ) ) ;
#94460 = LINE ( 'NONE', #17419, #33707 ) ;
#94461 = ORIENTED_EDGE ( 'NONE', *, *, #40719, .T. ) ;
#94462 = CARTESIAN_POINT ( 'NONE',  ( 167.0271109968743417, 287.8086958075197686, 0.5416428030073258126 ) ) ;
#94463 = CARTESIAN_POINT ( 'NONE',  ( 16.80975711337266176, 31.74646525600390135, 2.839279412974139660 ) ) ;
#94464 = CARTESIAN_POINT ( 'NONE',  ( 206.2520115784021471, 273.4080321133600933, 11.69992874350409018 ) ) ;
#94465 = CARTESIAN_POINT ( 'NONE',  ( 205.8918578537579833, 274.0318366629789466, 11.52627491423194250 ) ) ;
#94467 = ORIENTED_EDGE ( 'NONE', *, *, #66263, .F. ) ;
#94466 = CARTESIAN_POINT ( 'NONE',  ( 206.8877919403300041, 271.6698519413213830, 5.894673806612072298 ) ) ;
#94468 = CARTESIAN_POINT ( 'NONE',  ( 190.4261619690305167, 300.8192077097357355, 5.480148282445501451 ) ) ;
#94469 = DIRECTION ( 'NONE',  ( -0.4999999999999987232, 0.8660254037844394848, 0.000000000000000000 ) ) ;
#94470 = CARTESIAN_POINT ( 'NONE',  ( 206.8851632406098702, 272.3113812655195716, -9.957011741946159233 ) ) ;
#94471 = EDGE_CURVE ( 'NONE', #99635, #33095, #72389, .T. ) ;
#94472 = DIRECTION ( 'NONE',  ( -0.000000000000000000, -0.000000000000000000, 1.000000000000000000 ) ) ;
#94473 = EDGE_CURVE ( 'NONE', #21753, #29279, #99185, .T. ) ;
#94474 = CARTESIAN_POINT ( 'NONE',  ( 161.1884843536000744, 251.4603508349806873, 13.21272898143761942 ) ) ;
#94475 = CARTESIAN_POINT ( 'NONE',  ( 191.1851897594308127, 262.2115044052416124, -0.7464089480405260435 ) ) ;
#94476 = ORIENTED_EDGE ( 'NONE', *, *, #10512, .F. ) ;
#94477 = CARTESIAN_POINT ( 'NONE',  ( 194.2703023721977047, 294.1609612200219317, -15.68238946779285037 ) ) ;
#94478 = CARTESIAN_POINT ( 'NONE',  ( -22.42236680055709641, 157.8615022471902591, 0.000000000000000000 ) ) ;
#94479 = CARTESIAN_POINT ( 'NONE',  ( 207.6628070930962906, 270.9644626028195376, 7.378217122120054761 ) ) ;
#94480 = CARTESIAN_POINT ( 'NONE',  ( 12.05626958406292104, 187.7677522451419065, -5.000000000000047962 ) ) ;
#94481 = CARTESIAN_POINT ( 'NONE',  ( 91.86592320334659689, 223.8458772461660544, 9.188101187500095079 ) ) ;
#94482 = CARTESIAN_POINT ( 'NONE',  ( 82.49906311289566929, 40.47457387647443738, -1.406446948987077006 ) ) ;
#94483 = DIRECTION ( 'NONE',  ( 0.3666034970181715202, -0.9303772761487929532, 0.000000000000000000 ) ) ;
#94484 = DIRECTION ( 'NONE',  ( 0.4245406647209822304, 0.9054088711727241723, 0.000000000000000000 ) ) ;
#94486 = CARTESIAN_POINT ( 'NONE',  ( 75.58778754766929353, 65.52267137415682896, 13.80857608998921116 ) ) ;
#94485 = CARTESIAN_POINT ( 'NONE',  ( -2.422939729449181012, 181.6589784336661637, -6.496448406907675876E-16 ) ) ;
#94487 = VECTOR ( 'NONE', #80598, 1000.000000000000114 ) ;
#94488 = CARTESIAN_POINT ( 'NONE',  ( 200.1102648775588193, 284.0458494464393198, 17.54251420653697835 ) ) ;
#94489 = ORIENTED_EDGE ( 'NONE', *, *, #60564, .F. ) ;
#94490 = ORIENTED_EDGE ( 'NONE', *, *, #863, .T. ) ;
#94491 = CARTESIAN_POINT ( 'NONE',  ( 87.86298961015023679, 44.89260222163544256, 6.207647304897665919 ) ) ;
#94492 = CARTESIAN_POINT ( 'NONE',  ( 189.0340129193126018, 261.4605574960352214, -6.057196126885922460 ) ) ;
#94493 = CARTESIAN_POINT ( 'NONE',  ( 79.17490018547003672, 47.23354819373627578, -13.38294009737406043 ) ) ;
#94494 = CARTESIAN_POINT ( 'NONE',  ( 85.14296776498849795, 45.57912900884821283, 9.070685772083578513 ) ) ;
#94495 = VECTOR ( 'NONE', #30746, 1000.000000000000000 ) ;
#94496 = LINE ( 'NONE', #1778, #13975 ) ;
#94497 = CARTESIAN_POINT ( 'NONE',  ( 185.7830797826618721, 286.6111327835436100, 15.87653701371242931 ) ) ;
#94498 = CARTESIAN_POINT ( 'NONE',  ( 74.19835002362358978, 68.51042020854130499, -11.60174470505228150 ) ) ;
#94499 = ADVANCED_FACE ( 'NONE', ( #98655 ), #13546, .T. ) ;
#94500 = CARTESIAN_POINT ( 'NONE',  ( 34.76219959342767396, 197.0024278399161517, 9.188101187500095079 ) ) ;
#94501 = CARTESIAN_POINT ( 'NONE',  ( 84.36939080006362701, 209.5177522451417929, 5.000000000000051514 ) ) ;
#94502 = VECTOR ( 'NONE', #46481, 1000.000000000000000 ) ;
#94503 = FACE_OUTER_BOUND ( 'NONE', #78962, .T. ) ;
#94504 = ORIENTED_EDGE ( 'NONE', *, *, #74967, .F. ) ;
#94505 = CARTESIAN_POINT ( 'NONE',  ( 82.15438889958460322, 43.42002399553825853, 8.329187321006108036 ) ) ;
#94506 = ADVANCED_FACE ( 'NONE', ( #75349 ), #19267, .T. ) ;
#94507 = AXIS2_PLACEMENT_3D ( 'NONE', #18417, #41182, #95465 ) ;
#94508 = EDGE_CURVE ( 'NONE', #12322, #51698, #54491, .T. ) ;
#94509 = DIRECTION ( 'NONE',  ( 0.000000000000000000, -0.000000000000000000, -1.000000000000000000 ) ) ;
#94510 = CARTESIAN_POINT ( 'NONE',  ( 29.49842587079848855, 40.52903772873359856, -1.583844403245363575 ) ) ;
#94511 = CARTESIAN_POINT ( 'NONE',  ( 155.5660013421004919, 261.1987770755905558, 17.28709111629370199 ) ) ;
#94512 = CARTESIAN_POINT ( 'NONE',  ( 161.8750289368003621, 250.2712207352165592, -13.97436367953006098 ) ) ;
#94513 = CARTESIAN_POINT ( 'NONE',  ( 186.1456503528468431, 283.3687638237425404, 16.57478981768027992 ) ) ;
#94514 = CARTESIAN_POINT ( 'NONE',  ( 148.1632261683078013, 274.0207597936089883, -7.853210555358286271 ) ) ;
#94515 = ADVANCED_FACE ( 'NONE', ( #85471 ), #96123, .T. ) ;
#94516 = ADVANCED_FACE ( 'NONE', ( #20030 ), #48928, .T. ) ;
#94517 = CARTESIAN_POINT ( 'NONE',  ( 73.62250635243425734, 69.55784274833358438, 10.23584637956793308 ) ) ;
#94518 = CARTESIAN_POINT ( 'NONE',  ( 204.3574891606595827, 276.6894411969685166, 13.41627538812899978 ) ) ;
#94519 = CARTESIAN_POINT ( 'NONE',  ( 191.8000917695741805, 298.4394914891611847, -9.452573400474340914 ) ) ;
#94520 = CARTESIAN_POINT ( 'NONE',  ( 190.1063449786324213, 301.3731469862293011, 0.2163967485516588019 ) ) ;
#94521 = EDGE_LOOP ( 'NONE', ( #66113, #64242, #89945, #19640 ) ) ;
#94522 = CARTESIAN_POINT ( 'NONE',  ( 181.3121490855964169, 267.9468540978079432, 15.06114782510337236 ) ) ;
#94523 = CARTESIAN_POINT ( 'NONE',  ( 109.2403843188893831, 240.0024278399160949, -9.188101187500093303 ) ) ;
#94524 = CARTESIAN_POINT ( 'NONE',  ( 18.97660828663255117, 29.14336893147755703, 7.433330006724141015 ) ) ;
#94525 = CARTESIAN_POINT ( 'NONE',  ( 74.03931459348295618, 60.54867073305699421, -15.82834853898143912 ) ) ;
#94526 = CARTESIAN_POINT ( 'NONE',  ( -56.06787742410712383, 34.75406423768147590, -10.00000000000000000 ) ) ;
#94528 = CARTESIAN_POINT ( 'NONE',  ( 38.90713653809340400, 79.99999999999998579, 54.99999999999999289 ) ) ;
#94527 = CARTESIAN_POINT ( 'NONE',  ( 178.6627340464712859, 256.9245264283825918, 10.00612643570717708 ) ) ;
#94529 = CARTESIAN_POINT ( 'NONE',  ( 191.3737201945137656, 299.1779887200690951, -7.181879264107196903 ) ) ;
#94530 = FACE_OUTER_BOUND ( 'NONE', #85598, .T. ) ;
#94531 = CARTESIAN_POINT ( 'NONE',  ( 196.7491951525289835, 289.8673929779723721, -16.35352603081977207 ) ) ;
#94532 = CARTESIAN_POINT ( 'NONE',  ( 80.73032772533602497, 228.9637435831425023, 2.679491924311251605 ) ) ;
#94533 = CARTESIAN_POINT ( 'NONE',  ( 203.6458270900087655, 276.5680210061898947, 14.19527340636538959 ) ) ;
#94534 = CARTESIAN_POINT ( 'NONE',  ( 85.86469242221521370, 47.48580584220093925, 10.80557080686977933 ) ) ;
#94535 = CARTESIAN_POINT ( 'NONE',  ( 135.4648896233454991, 249.0177522451418497, -10.00000000000009592 ) ) ;
#94536 = CARTESIAN_POINT ( 'NONE',  ( 175.2191928923303124, 279.1726182442799313, 15.58576654816208062 ) ) ;
#94537 = CARTESIAN_POINT ( 'NONE',  ( 165.6500576547331036, 269.1436911520689250, -17.16406264618244037 ) ) ;
#94538 = VERTEX_POINT ( 'NONE', #57507 ) ;
#94539 = CARTESIAN_POINT ( 'NONE',  ( 71.96852905813886991, 72.61068693531510121, 1.394764389614196354 ) ) ;
#94540 = CARTESIAN_POINT ( 'NONE',  ( 85.86494630647001713, 46.28363073764573699, 10.08731117762910046 ) ) ;
#94541 = CARTESIAN_POINT ( 'NONE',  ( 83.91613728284298190, 51.81858503665881699, -14.46596598907902909 ) ) ;
#94542 = DIRECTION ( 'NONE',  ( 1.000000000000000000, 0.000000000000000000, 0.000000000000000000 ) ) ;
#94543 = CARTESIAN_POINT ( 'NONE',  ( 192.8010417052266234, 296.7057953447782097, 12.10593424093686643 ) ) ;
#94544 = ORIENTED_EDGE ( 'NONE', *, *, #92088, .F. ) ;
#94545 = CARTESIAN_POINT ( 'NONE',  ( 165.3929592122126451, 286.2279243276498732, 4.432946431554212197 ) ) ;
#94546 = CARTESIAN_POINT ( 'NONE',  ( 39.98734656443052415, 28.80170272979929535, 7.433330006724137462 ) ) ;
#94547 = CARTESIAN_POINT ( 'NONE',  ( 193.5255742412444420, 289.0164190174409100, -16.00935465151201598 ) ) ;
#94548 = ORIENTED_EDGE ( 'NONE', *, *, #95672, .T. ) ;
#94549 = CARTESIAN_POINT ( 'NONE',  ( 167.7406742120077752, 280.9361443569400762, 11.73743621418454985 ) ) ;
#94550 = ADVANCED_FACE ( 'NONE', ( #26127 ), #58014, .F. ) ;
#94551 = DIRECTION ( 'NONE',  ( 4.546899780356472071E-16, -9.093799560712944142E-16, 1.000000000000000000 ) ) ;
#94552 = CARTESIAN_POINT ( 'NONE',  ( 16.11576366785043746, 180.1115022471902591, 10.00000000000009592 ) ) ;
#94553 = ORIENTED_EDGE ( 'NONE', *, *, #53326, .T. ) ;
#94554 = CARTESIAN_POINT ( 'NONE',  ( 86.52735458038128513, 47.21746853903349006, -10.13408089075210050 ) ) ;
#94555 = CARTESIAN_POINT ( 'NONE',  ( 77.32817876982272765, 63.13942984521013813, 15.61058464551962111 ) ) ;
#94556 = CARTESIAN_POINT ( 'NONE',  ( 87.02903784321956948, 44.46201794666647800, -6.348227258070155088 ) ) ;
#94557 = DIRECTION ( 'NONE',  ( -0.4924038765061016787, 0.8528685319524424990, -0.1736481776669404342 ) ) ;
#94558 = CARTESIAN_POINT ( 'NONE',  ( 81.82083194927301406, 45.30039977485242275, -11.45098190420846862 ) ) ;
#94559 = CARTESIAN_POINT ( 'NONE',  ( 84.83269492062768791, 49.93259165162010760, -13.18831682406798400 ) ) ;
#94560 = CARTESIAN_POINT ( 'NONE',  ( 155.0619429961492983, 262.0718317407570339, -17.08853361476647592 ) ) ;
#94561 = VERTEX_POINT ( 'NONE', #49418 ) ;
#94562 = ORIENTED_EDGE ( 'NONE', *, *, #37703, .F. ) ;
#94563 = CARTESIAN_POINT ( 'NONE',  ( 178.4219847520450628, 261.0252761168330835, 12.14700762561149538 ) ) ;
#94564 = ORIENTED_EDGE ( 'NONE', *, *, #70776, .T. ) ;
#94565 = CARTESIAN_POINT ( 'NONE',  ( 77.38344707993300631, 49.10671604804453239, -15.27628165703247198 ) ) ;
#94566 = VECTOR ( 'NONE', #79714, 999.9999999999998863 ) ;
#94567 = VERTEX_POINT ( 'NONE', #19549 ) ;
#94568 = CARTESIAN_POINT ( 'NONE',  ( 88.31205481598105678, 44.17345802399140098, -0.1934329303017474633 ) ) ;
#94569 = CARTESIAN_POINT ( 'NONE',  ( 155.6281496932864457, 261.0911329737299980, -18.07904265579665548 ) ) ;
#94570 = ORIENTED_EDGE ( 'NONE', *, *, #5521, .T. ) ;
#94571 = CARTESIAN_POINT ( 'NONE',  ( 182.7167784989862014, 280.1855270853789079, -16.12831863832678536 ) ) ;
#94572 = CARTESIAN_POINT ( 'NONE',  ( 164.6027939175806125, 245.5465931973980105, -2.481135897876769913 ) ) ;
#94573 = CARTESIAN_POINT ( 'NONE',  ( 147.7773877150008559, 274.6890515982507281, -5.974666768616035739 ) ) ;
#94574 = DIRECTION ( 'NONE',  ( -0.3105719460338542404, -0.9505498757754611283, 0.000000000000000000 ) ) ;
#94575 = CARTESIAN_POINT ( 'NONE',  ( 147.5118896528469179, 275.1489077312122049, -3.975523961781759930 ) ) ;
#94576 = CARTESIAN_POINT ( 'NONE',  ( 79.11275361910446691, 46.11146926033848814, 13.27945046499837112 ) ) ;
#94577 = DIRECTION ( 'NONE',  ( 0.000000000000000000, 0.000000000000000000, 1.000000000000000000 ) ) ;
#94579 = EDGE_CURVE ( 'NONE', #41928, #88465, #50409, .T. ) ;
#94578 = CIRCLE ( 'NONE', #3937, 0.1418229129683812317 ) ;
#94580 = CARTESIAN_POINT ( 'NONE',  ( 183.5836227624010917, 284.2690207048559046, -15.88295186417738591 ) ) ;
#94581 = CARTESIAN_POINT ( 'NONE',  ( 124.8827946268633298, 255.1589784336661069, -6.496448406907675876E-16 ) ) ;
#94582 = ORIENTED_EDGE ( 'NONE', *, *, #43684, .T. ) ;
#94583 = CARTESIAN_POINT ( 'NONE',  ( 186.5849876461966801, 262.7207080590939654, -9.049355759300835800 ) ) ;
#94584 = EDGE_LOOP ( 'NONE', ( #59366, #99036, #59999, #25232 ) ) ;
#94586 = ORIENTED_EDGE ( 'NONE', *, *, #98906, .T. ) ;
#94585 = CARTESIAN_POINT ( 'NONE',  ( 20.61848683307935914, 34.83705186507754803, 3.090169943749475401 ) ) ;
#94587 = DIRECTION ( 'NONE',  ( -0.8806841296921844586, 0.4737039832092607705, 0.000000000000000000 ) ) ;
#94588 = LINE ( 'NONE', #24645, #23783 ) ;
#94589 = CARTESIAN_POINT ( 'NONE',  ( 9.242171499132833645, 29.30720582267293040, 177.5919119679930134 ) ) ;
#94590 = CARTESIAN_POINT ( 'NONE',  ( 192.8203422047577078, 296.6723658989791943, 12.07326395438877320 ) ) ;
#94591 = CARTESIAN_POINT ( 'NONE',  ( 71.50240432004942193, 72.40933122983058468, 5.654570818603106787E-06 ) ) ;
#94592 = ADVANCED_FACE ( 'NONE', ( #37685 ), #89950, .F. ) ;
#94593 = CARTESIAN_POINT ( 'NONE',  ( 197.5405456899788419, 268.5419454055666506, 10.87215985704571963 ) ) ;
#94594 = CARTESIAN_POINT ( 'NONE',  ( 176.4132951231468098, 288.3403858341706609, -9.320880473285331647 ) ) ;
#94595 = CARTESIAN_POINT ( 'NONE',  ( 195.2684241838297510, 292.4321635301326978, 16.66903275019414465 ) ) ;
#94596 = EDGE_CURVE ( 'NONE', #46799, #29349, #52400, .T. ) ;
#94597 = CARTESIAN_POINT ( 'NONE',  ( 194.6318672504471863, 291.7125382847361266, 16.11827429453959226 ) ) ;
#94598 =( BOUNDED_CURVE ( )  B_SPLINE_CURVE ( 2, ( #6395, #51487, #21596, #13018, #75310, #73801, #67183, #59569, #52478 ),
 .UNSPECIFIED., .F., .T. ) 
 B_SPLINE_CURVE_WITH_KNOTS ( ( 3, 2, 2, 2, 3 ),
 ( 0.3991935483870967527, 0.4005376344086021279, 0.4032258064516128782, 0.4059139784946236285, 0.4072580645161290591 ),
 .UNSPECIFIED. ) 
 CURVE ( )  GEOMETRIC_REPRESENTATION_ITEM ( )  RATIONAL_B_SPLINE_CURVE ( ( 0.9330127018922194093, 0.9330127018922194093, 1.000000000000000000, 0.8660254037844387076, 1.000000000000000000, 0.8660254037844387076, 1.000000000000000000, 0.9330127018922179660, 0.9330127018922194093 ) ) 
 REPRESENTATION_ITEM ( '' )  );
#94599 = ORIENTED_EDGE ( 'NONE', *, *, #88683, .F. ) ;
#94600 = CARTESIAN_POINT ( 'NONE',  ( 194.1789525331299728, 294.3191837825503967, -15.34533909744314961 ) ) ;
#94601 = CARTESIAN_POINT ( 'NONE',  ( 152.8245645352945417, 273.6623100745259762, 11.98233510762519316 ) ) ;
#94602 = VERTEX_POINT ( 'NONE', #13909 ) ;
#94603 = DIRECTION ( 'NONE',  ( 0.8965230319888196631, -0.4429971254010276471, 0.000000000000000000 ) ) ;
#94604 = CARTESIAN_POINT ( 'NONE',  ( 82.93017357788667709, 175.3855496052738374, 36.50000000000000000 ) ) ;
#94605 = DIRECTION ( 'NONE',  ( 0.000000000000000000, 0.000000000000000000, 1.000000000000000000 ) ) ;
#94606 = CARTESIAN_POINT ( 'NONE',  ( 190.7222376050763444, 300.3063896652212179, 3.365789908110941475 ) ) ;
#94607 = CARTESIAN_POINT ( 'NONE',  ( 202.2773826701151165, 280.2922913237452462, 16.62862787739668846 ) ) ;
#94609 = CARTESIAN_POINT ( 'NONE',  ( 151.5094854109957225, 274.9022664227586006, -9.147610560135673197 ) ) ;
#94608 = CARTESIAN_POINT ( 'NONE',  ( 153.5300831522595502, 269.9241095255698610, 14.65767817066312517 ) ) ;
#94610 = CARTESIAN_POINT ( 'NONE',  ( 153.1983976505312626, 265.2995869615763809, -17.69657798691567763 ) ) ;
#94611 = ORIENTED_EDGE ( 'NONE', *, *, #74365, .F. ) ;
#94612 = CARTESIAN_POINT ( 'NONE',  ( 167.8684523614047635, 281.9072385613080769, -10.90217489050904831 ) ) ;
#94613 = CARTESIAN_POINT ( 'NONE',  ( 186.9162837453443728, 262.3935138041393884, -8.704777280997261002 ) ) ;
#94614 = CARTESIAN_POINT ( 'NONE',  ( 193.5562164153924414, 276.1342835013242620, -16.47396278362798938 ) ) ;
#94615 = CARTESIAN_POINT ( 'NONE',  ( 74.84311135843471163, 224.0177522451419350, 5.000000000000046185 ) ) ;
#94616 = CARTESIAN_POINT ( 'NONE',  ( 188.4553964595242235, 298.4901091694543425, -4.262234365374711231 ) ) ;
#94617 = CARTESIAN_POINT ( 'NONE',  ( 204.2071116102253256, 275.4331146181932013, 13.30069288008150430 ) ) ;
#94618 = DIRECTION ( 'NONE',  ( -0.000000000000000000, 0.000000000000000000, -1.000000000000000000 ) ) ;
#94619 = CARTESIAN_POINT ( 'NONE',  ( -4.215479392844351914, 156.8262482093458061, -4.415768667553307481E-15 ) ) ;
#94620 = CARTESIAN_POINT ( 'NONE',  ( 67.77025216284080500, 69.60538277264423357, 1.930950847018320982 ) ) ;
#94621 = EDGE_CURVE ( 'NONE', #62092, #31573, #4735, .T. ) ;
#94622 = CARTESIAN_POINT ( 'NONE',  ( -9.405095999578705346, 171.5024278399160949, 9.188101187500095079 ) ) ;
#94623 = CARTESIAN_POINT ( 'NONE',  ( 92.62404252742298638, 212.0327760586659451, 1.948934522072303157E-15 ) ) ;
#94624 = CARTESIAN_POINT ( 'NONE',  ( 5.270092192305422252, 185.3967562850347122, -4.648177544792955347E-16 ) ) ;
#94625 = CARTESIAN_POINT ( 'NONE',  ( 88.08080417645612670, 44.69611168586961014, -4.296359715587334094 ) ) ;
#94626 = CARTESIAN_POINT ( 'NONE',  ( 147.7269857344357149, 275.1802626144117312, 4.082897581163150491 ) ) ;
#94627 = CARTESIAN_POINT ( 'NONE',  ( 78.51571825418398021, 47.42707193263058230, 14.24622496894903634 ) ) ;
#94628 = CARTESIAN_POINT ( 'NONE',  ( 77.56166335470948070, 52.46047131205113345, 15.73022103520029980 ) ) ;
#94629 = PRESENTATION_STYLE_ASSIGNMENT (( #9509 ) ) ;
#94630 = CARTESIAN_POINT ( 'NONE',  ( 78.27096424623380244, 61.69037436829221122, 15.77147391507759799 ) ) ;
#94632 = CARTESIAN_POINT ( 'NONE',  ( 208.3764315856425640, 269.7284287242038658, -1.833640725398759441 ) ) ;
#94631 = CARTESIAN_POINT ( 'NONE',  ( -17.69472717286124208, 126.6729902121449811, 2.598076211353400389 ) ) ;
#94633 = CARTESIAN_POINT ( 'NONE',  ( 162.0519062060177475, 249.9648603182279487, 13.45613752710952937 ) ) ;
#94634 = EDGE_CURVE ( 'NONE', #9722, #61780, #12429, .T. ) ;
#94635 = FACE_OUTER_BOUND ( 'NONE', #71359, .T. ) ;
#94636 =( LENGTH_UNIT ( ) NAMED_UNIT ( * ) SI_UNIT ( .MILLI., .METRE. ) );
#94637 = CARTESIAN_POINT ( 'NONE',  ( 72.95830788359974406, 56.77128196665827176, -15.96545419981962333 ) ) ;
#94638 = CARTESIAN_POINT ( 'NONE',  ( -14.37785915960194494, 174.0530062829862743, 6.972266317189433612E-15 ) ) ;
#94639 = CIRCLE ( 'NONE', #47651, 14.99999999999968381 ) ;
#94640 = CARTESIAN_POINT ( 'NONE',  ( 73.63798764345266079, 69.67310094948797428, 10.11710443556177275 ) ) ;
#94641 = CARTESIAN_POINT ( 'NONE',  ( 37.98264478980979675, 201.9244531367911293, -4.594050593750046652 ) ) ;
#94642 = CARTESIAN_POINT ( 'NONE',  ( -36.26652983198114555, 26.35523046909639788, 10.00000000000000000 ) ) ;
#94643 = CARTESIAN_POINT ( 'NONE',  ( 57.65757265809627086, 216.3464784336661353, 1.353441290958777327E-15 ) ) ;
#94644 = CARTESIAN_POINT ( 'NONE',  ( 164.0020300202577346, 247.0572029250454307, -5.999176618229816071 ) ) ;
#94646 = CARTESIAN_POINT ( 'NONE',  ( 88.54283264841694745, 43.89585489789003248, -0.1669414168386815500 ) ) ;
#94645 = AXIS2_PLACEMENT_3D ( 'NONE', #56844, #32558, #54844 ) ;
#94647 = CARTESIAN_POINT ( 'NONE',  ( 167.0980956493596921, 259.5690430767091925, 16.41267671096424863 ) ) ;
#94649 = CARTESIAN_POINT ( 'NONE',  ( 151.9976068546241095, 267.3794176293484952, 15.44464033079018250 ) ) ;
#94648 = CARTESIAN_POINT ( 'NONE',  ( 49.28760614098965931, 105.1966139777580338, 177.5919119679930134 ) ) ;
#94650 = ADVANCED_FACE ( 'NONE', ( #74245 ), #72638, .F. ) ;
#94651 = DIRECTION ( 'NONE',  ( -0.5000000000000019984, 0.8660254037844374864, 0.000000000000000000 ) ) ;
#94652 = CARTESIAN_POINT ( 'NONE',  ( 25.24689923506580769, 37.68290643055188838, 3.479690158560446702E-15 ) ) ;
#94653 = CARTESIAN_POINT ( 'NONE',  ( 81.66039725905243074, 47.34856834791166591, 13.14074354680314372 ) ) ;
#94654 = CARTESIAN_POINT ( 'NONE',  ( 79.06313471345563926, 47.89260127994747762, -13.77394454897267728 ) ) ;
#94655 = ORIENTED_EDGE ( 'NONE', *, *, #58612, .F. ) ;
#94656 = CARTESIAN_POINT ( 'NONE',  ( 21.91745948943428601, 13.44966523072494269, -2.296566073217252530E-15 ) ) ;
#94657 = CARTESIAN_POINT ( 'NONE',  ( 69.78227540684341079, 211.0958772461660544, -9.188101187500095079 ) ) ;
#94658 = CARTESIAN_POINT ( 'NONE',  ( 82.65022647498227570, 54.02725688527395675, -15.50106321898839923 ) ) ;
#94659 = CARTESIAN_POINT ( 'NONE',  ( 179.0685761320505947, 258.5468394390073286, -11.57600102548048149 ) ) ;
#94660 = CARTESIAN_POINT ( 'NONE',  ( 69.73646959995419081, 63.15839211331632441, -13.63664433904350481 ) ) ;
#94661 = CARTESIAN_POINT ( 'NONE',  ( 201.4964414552794949, 281.6449211855650674, 17.70651170561034249 ) ) ;
#94662 = CARTESIAN_POINT ( 'NONE',  ( 189.8554816459523806, 286.6603570597984003, 16.85211268990574851 ) ) ;
#94663 = CARTESIAN_POINT ( 'NONE',  ( 132.5961804768574837, 237.3615022471901739, 5.000000000000051514 ) ) ;
#94664 = DIRECTION ( 'NONE',  ( 0.000000000000000000, 0.000000000000000000, -1.000000000000000000 ) ) ;
#94665 = CARTESIAN_POINT ( 'NONE',  ( 164.3774690880109119, 245.9368672504194819, -2.805681983503304000 ) ) ;
#94666 = EDGE_LOOP ( 'NONE', ( #15036, #15835 ) ) ;
#94667 = CARTESIAN_POINT ( 'NONE',  ( 84.13622801036203214, 43.12737274679144406, 5.841038043053070616 ) ) ;
#94668 = CARTESIAN_POINT ( 'NONE',  ( 188.1508358339878839, 273.3824090696089115, 15.63829542113482418 ) ) ;
#94669 = ORIENTED_EDGE ( 'NONE', *, *, #58430, .F. ) ;
#94670 = CARTESIAN_POINT ( 'NONE',  ( 202.4900219881211854, 279.9239892212719383, 15.63116161057562259 ) ) ;
#94671 = CARTESIAN_POINT ( 'NONE',  ( 207.3553394910502163, 270.5667219550074947, -0.3217649823664716080 ) ) ;
#94672 = CARTESIAN_POINT ( 'NONE',  ( 68.77965372826733415, 68.78927433938119407, -6.398530390328347472 ) ) ;
#94673 = ORIENTED_EDGE ( 'NONE', *, *, #39516, .F. ) ;
#94674 = CARTESIAN_POINT ( 'NONE',  ( 177.2644709662962725, 252.9866977164365096, -0.2652805781673223118 ) ) ;
#94675 = EDGE_LOOP ( 'NONE', ( #10710, #8930, #85358, #68112 ) ) ;
#94676 = CARTESIAN_POINT ( 'NONE',  ( 72.35414581608256412, 71.76618622507949397, 5.628474724962954312 ) ) ;
#94677 = CARTESIAN_POINT ( 'NONE',  ( 170.7247694180109931, 250.3410439623759487, 3.110155547565024214 ) ) ;
#94678 = CARTESIAN_POINT ( 'NONE',  ( 34.05451400132101014, 48.17084265633775431, -10.00000000000000000 ) ) ;
#94679 = VERTEX_POINT ( 'NONE', #697 ) ;
#94680 = VECTOR ( 'NONE', #12304, 1000.000000000000114 ) ;
#94681 = CARTESIAN_POINT ( 'NONE',  ( 23.84800118292001159, 31.95586893147756058, 7.433330006724141015 ) ) ;
#94682 = CARTESIAN_POINT ( 'NONE',  ( 74.67000616351417364, 66.81477949400927230, -13.12245706047551508 ) ) ;
#94683 = CARTESIAN_POINT ( 'NONE',  ( 78.96527083864563679, 49.39199274328564115, -14.51843862548532904 ) ) ;
#94684 = CYLINDRICAL_SURFACE ( 'NONE', #96723, 16.60714546451156792 ) ;
#94685 = CARTESIAN_POINT ( 'NONE',  ( 75.53417530262939295, 225.9637435831425023, 2.679491924311251605 ) ) ;
#94686 = EDGE_LOOP ( 'NONE', ( #47450, #32744, #93712, #29978 ) ) ;
#94687 = ORIENTED_EDGE ( 'NONE', *, *, #98036, .F. ) ;
#94688 = CARTESIAN_POINT ( 'NONE',  ( 185.8761704939435049, 297.8286767897885738, 1.040812290680570795 ) ) ;
#94690 = CARTESIAN_POINT ( 'NONE',  ( 159.0906380018002153, 259.2649656523443582, -17.57712761084927067 ) ) ;
#94689 = CARTESIAN_POINT ( 'NONE',  ( 67.76997328886733385, 65.59689072950045841, 10.11017479253558626 ) ) ;
#94691 = CARTESIAN_POINT ( 'NONE',  ( 81.75866452494919656, 55.62065470240971621, -15.97060719759759628 ) ) ;
#94692 = CARTESIAN_POINT ( 'NONE',  ( 155.4917600441137324, 261.3273667757233056, 17.14261720787171939 ) ) ;
#94693 = CARTESIAN_POINT ( 'NONE',  ( 157.6036818288543486, 257.6694109429415107, -16.73826488331764395 ) ) ;
#94694 = CARTESIAN_POINT ( 'NONE',  ( 164.2953130194600817, 246.0791657352997959, 5.812963931023970687 ) ) ;
#94695 = CARTESIAN_POINT ( 'NONE',  ( 72.96253058994859941, 62.41371533620014134, -14.96910879617931656 ) ) ;
#94696 = CARTESIAN_POINT ( 'NONE',  ( 170.9618134082231506, 249.0169227132842309, -1.633238342494487183 ) ) ;
#94697 = CARTESIAN_POINT ( 'NONE',  ( 89.26784699199328088, 222.3458772461660544, 9.188101187500095079 ) ) ;
#94698 = ORIENTED_EDGE ( 'NONE', *, *, #89791, .F. ) ;
#94699 = CARTESIAN_POINT ( 'NONE',  ( 191.2729698983822288, 299.3524933518466469, 8.871011392605806734 ) ) ;
#94700 = DIRECTION ( 'NONE',  ( -0.3402761906661169178, -0.9403255362191098587, 0.000000000000000000 ) ) ;
#94701 = CARTESIAN_POINT ( 'NONE',  ( -9.693023484072631035, 23.77726266618848072, -10.00000000000000000 ) ) ;
#94702 = ORIENTED_EDGE ( 'NONE', *, *, #98341, .T. ) ;
#94703 = CARTESIAN_POINT ( 'NONE',  ( 196.0995493315176645, 290.9926125468888927, -16.21657796881217806 ) ) ;
#94704 = EDGE_LOOP ( 'NONE', ( #30873, #67903, #27135, #61504 ) ) ;
#94705 = CARTESIAN_POINT ( 'NONE',  ( 80.11135166060731194, 44.61021142565198261, -11.71391964968389132 ) ) ;
#94706 = CARTESIAN_POINT ( 'NONE',  ( 80.87517248313827167, 58.64441083166272506, 0.000000000000000000 ) ) ;
#94707 = CARTESIAN_POINT ( 'NONE',  ( 164.1785392759978492, 249.9733907654231473, 10.19594168643268084 ) ) ;
#94708 = CARTESIAN_POINT ( 'NONE',  ( 79.89582544085288873, 48.49195324432764664, -13.86380691270739440 ) ) ;
#94709 = ADVANCED_FACE ( 'NONE', ( #54370 ), #14890, .T. ) ;
#94710 = CARTESIAN_POINT ( 'NONE',  ( 207.5772549350081988, 271.1126432873252838, 2.658056670308439617 ) ) ;
#94711 = CARTESIAN_POINT ( 'NONE',  ( 97.03527265400872182, 217.6423013555409796, -4.594050593750043987 ) ) ;
#94712 = VECTOR ( 'NONE', #8313, 1000.000000000000000 ) ;
#94713 = EDGE_CURVE ( 'NONE', #99270, #66266, #73631, .T. ) ;
#94714 = ORIENTED_EDGE ( 'NONE', *, *, #90750, .T. ) ;
#94715 = B_SPLINE_SURFACE_WITH_KNOTS ( 'NONE', 3, 1, ( 
 ( #64306, #64813 ),
 ( #95259, #65788 ),
 ( #95761, #26313 ),
 ( #49597, #80552 ),
 ( #48616, #11128 ),
 ( #25825, #79555 ),
 ( #42482, #73416 ),
 ( #96747, #33928 ),
 ( #96245, #41999 ),
 ( #17195, #57689 ),
 ( #26806, #72935 ),
 ( #58196, #71921 ),
 ( #94737, #88667 ),
 ( #19234, #18217 ),
 ( #48098, #79039 ),
 ( #10110, #40975 ),
 ( #2523, #33405 ),
 ( #56701, #87682 ),
 ( #80046, #82045 ),
 ( #37380, #20211 ),
 ( #75411, #52581 ),
 ( #36889, #51599 ),
 ( #12110, #27805 ),
 ( #82553, #13118 ),
 ( #97720, #43485 ),
 ( #58678, #74429 ),
 ( #4499, #35893 ),
 ( #66795, #36384 ),
 ( #28288, #6503 ),
 ( #67288, #98215 ),
 ( #28799, #59679 ) ),
 .UNSPECIFIED., .F., .F., .F.,
 ( 4, 3, 3, 3, 3, 3, 3, 3, 3, 3, 4 ),
 ( 2, 2 ),
 ( 0.000000000000000000, 0.1333490885032345696, 0.3007194338854333737, 0.4699862290245237495, 0.5844252810809289489, 0.6686540514502742338, 0.7354980260655397117, 0.8028463152565420424, 0.8633854507756993923, 0.9437142632667149256, 1.000000000000000000 ),
 ( 0.000000000000000000, 1.000000000000000000 ),
 .UNSPECIFIED. ) ;
#94717 = EDGE_CURVE ( 'NONE', #39405, #28901, #7032, .T. ) ;
#94716 = FACE_OUTER_BOUND ( 'NONE', #67774, .T. ) ;
#94718 = ORIENTED_EDGE ( 'NONE', *, *, #23190, .F. ) ;
#94719 = ADVANCED_FACE ( 'NONE', ( #15376 ), #39667, .F. ) ;
#94720 = AXIS2_PLACEMENT_3D ( 'NONE', #77300, #22096, #37783 ) ;
#94721 = CARTESIAN_POINT ( 'NONE',  ( 22.61461015039527922, 36.55466486950700755, 7.012934429366973338E-14 ) ) ;
#94722 = CARTESIAN_POINT ( 'NONE',  ( 70.00660573506930007, 69.36680803441663556, -6.749214270069086474 ) ) ;
#94723 = CARTESIAN_POINT ( 'NONE',  ( 88.08546139208640113, 44.41188104239807188, 4.690966480777962744 ) ) ;
#94724 = VERTEX_POINT ( 'NONE', #46800 ) ;
#94725 = CARTESIAN_POINT ( 'NONE',  ( 81.23259876005273838, 43.67848304645094970, -9.361027865139382342 ) ) ;
#94726 = CARTESIAN_POINT ( 'NONE',  ( 80.33508072308801218, 44.92307697338561212, 11.19555900290710326 ) ) ;
#94727 = CARTESIAN_POINT ( 'NONE',  ( 206.2313482792274328, 273.4438219973828268, -9.403385562213845361 ) ) ;
#94728 = CARTESIAN_POINT ( 'NONE',  ( 38.08139550823666042, 22.39040679176985904, -6.890680421881970419E-14 ) ) ;
#94729 = CARTESIAN_POINT ( 'NONE',  ( 201.1060504099706350, 282.3210983108598384, -18.18000168485860257 ) ) ;
#94730 = CARTESIAN_POINT ( 'NONE',  ( 102.9889369814289921, 240.2677522451419065, -5.000000000000047962 ) ) ;
#94731 = DIRECTION ( 'NONE',  ( -0.8660254037844359321, -0.5000000000000051070, -0.000000000000000000 ) ) ;
#94732 = ORIENTED_EDGE ( 'NONE', *, *, #86488, .T. ) ;
#94733 = CARTESIAN_POINT ( 'NONE',  ( 203.4917594071969518, 276.5501419217281409, -14.41400602080355675 ) ) ;
#94734 = CARTESIAN_POINT ( 'NONE',  ( 161.2313178023453588, 251.3861611254901618, 13.12937145726518473 ) ) ;
#94735 = CARTESIAN_POINT ( 'NONE',  ( 82.15463706511577868, 40.84277258114416043, 1.595534587534165549 ) ) ;
#94736 = CARTESIAN_POINT ( 'NONE',  ( 171.6188493331028440, 251.5817016751831829, 7.205359137630009236 ) ) ;
#94737 = CARTESIAN_POINT ( 'NONE',  ( 78.08661669030729513, 61.77574478846858597, 16.09152831843414688 ) ) ;
#94738 = CARTESIAN_POINT ( 'NONE',  ( 175.1691724511426571, 290.1382956017840797, -6.308240513192195031 ) ) ;
#94739 = CARTESIAN_POINT ( 'NONE',  ( 153.1064336331667732, 270.6633677442188173, 13.89254713196513258 ) ) ;
#94740 = ORIENTED_EDGE ( 'NONE', *, *, #23137, .F. ) ;
#94741 = AXIS2_PLACEMENT_3D ( 'NONE', #20076, #4360, #42834 ) ;
#94742 = CARTESIAN_POINT ( 'NONE',  ( 206.9059968923335475, 272.2752963222270068, 6.902135944297345560 ) ) ;
#94744 = CARTESIAN_POINT ( 'NONE',  ( 183.6422324172568210, 264.5785696717482551, 14.31652553825990104 ) ) ;
#94743 = CARTESIAN_POINT ( 'NONE',  ( 180.6430269190001354, 266.9122829459220725, -14.79710749879348342 ) ) ;
#94745 = CARTESIAN_POINT ( 'NONE',  ( 199.5820190223589066, 281.0610403850588455, -17.29246150691365358 ) ) ;
#94746 = CARTESIAN_POINT ( 'NONE',  ( 26.99866280452971878, 37.36126292948897287, 6.180339887498949913 ) ) ;
#94747 = CARTESIAN_POINT ( 'NONE',  ( 37.96661208706053969, 52.86061180733513964, 10.00000000000000000 ) ) ;
#94748 = CARTESIAN_POINT ( 'NONE',  ( 172.2641683536514563, 275.0456089790841361, 16.51748826216277877 ) ) ;
#94749 = CARTESIAN_POINT ( 'NONE',  ( -72.48190909937210336, 49.06123820388767598, -10.00000000000000000 ) ) ;
#94750 = CARTESIAN_POINT ( 'NONE',  ( 160.4237162281696953, 273.2376347127639633, -15.66572034412998882 ) ) ;
#94751 = AXIS2_PLACEMENT_3D ( 'NONE', #82768, #29029, #50812 ) ;
#94752 = CARTESIAN_POINT ( 'NONE',  ( 188.6780514684627406, 261.0664558817952638, 2.867164000797742585 ) ) ;
#94753 = CARTESIAN_POINT ( 'NONE',  ( 207.6129110656513035, 271.0508850574501025, -5.265106572941297358 ) ) ;
#94754 = CARTESIAN_POINT ( 'NONE',  ( 8.267668766103758671, 166.3923013555410080, 4.594050593750050204 ) ) ;
#94755 = CARTESIAN_POINT ( 'NONE',  ( 82.13016512221932430, 47.61428595633086758, 12.58464463784943987 ) ) ;
#94756 = VERTEX_POINT ( 'NONE', #53876 ) ;
#94757 = CARTESIAN_POINT ( 'NONE',  ( 174.9036676751700838, 255.2839639389062256, 8.319262650324212416 ) ) ;
#94758 = DIRECTION ( 'NONE',  ( 0.000000000000000000, 0.000000000000000000, 1.000000000000000000 ) ) ;
#94759 = CARTESIAN_POINT ( 'NONE',  ( 82.09831584080588129, 41.83606685967262706, 5.488894909882152895 ) ) ;
#94760 = CARTESIAN_POINT ( 'NONE',  ( 21.36630299834339652, 173.9548013555409796, -4.594050593750042211 ) ) ;
#94761 = EDGE_CURVE ( 'NONE', #28403, #44016, #32600, .T. ) ;
#94762 = CARTESIAN_POINT ( 'NONE',  ( 32.55392312662736032, 19.76426979415091267, 3.090169943749476733 ) ) ;
#94763 = CARTESIAN_POINT ( 'NONE',  ( 38.89349527680885643, 24.58380873178789727, 6.180339887498953466 ) ) ;
#94764 = CARTESIAN_POINT ( 'NONE',  ( 199.9961967999579713, 267.3157181498997375, -6.792282625736725699 ) ) ;
#94765 = CARTESIAN_POINT ( 'NONE',  ( 107.0484310652165476, 222.6115022471901739, -5.000000000000041744 ) ) ;
#94767 = CARTESIAN_POINT ( 'NONE',  ( 149.7656787950428736, 271.2452304273818413, 12.35216892413132328 ) ) ;
#94766 = AXIS2_PLACEMENT_3D ( 'NONE', #14417, #92444, #84841 ) ;
#94768 = CARTESIAN_POINT ( 'NONE',  ( 81.17617732377340189, 56.17678352023477117, 16.10626194070232131 ) ) ;
#94769 = LINE ( 'NONE', #26345, #52515 ) ;
#94770 = CARTESIAN_POINT ( 'NONE',  ( 84.91076779388347973, 49.09221707277423974, 13.05056290568177779 ) ) ;
#94771 = CARTESIAN_POINT ( 'NONE',  ( 83.67285453873573431, 52.00132685099406160, 14.98825055830738151 ) ) ;
#94772 = AXIS2_PLACEMENT_3D ( 'NONE', #61613, #77843, #92567 ) ;
#94773 = CARTESIAN_POINT ( 'NONE',  ( 192.8108164209771473, 295.4770219581381525, -13.03931828728948439 ) ) ;
#94774 = CARTESIAN_POINT ( 'NONE',  ( 73.70645301951556405, 223.3615022471903160, 5.000000000000046185 ) ) ;
#94775 = CARTESIAN_POINT ( 'NONE',  ( 74.65546376004118656, 65.88439924513853896, -13.23886940964006520 ) ) ;
#94776 = CARTESIAN_POINT ( 'NONE',  ( 184.6509992051337861, 277.2187774885003364, -17.79388780315141005 ) ) ;
#94777 = DIRECTION ( 'NONE',  ( 0.5000000000000001110, -0.8660254037844384856, -0.000000000000000000 ) ) ;
#94778 = CARTESIAN_POINT ( 'NONE',  ( 51.43353571204313823, 194.3768266524159856, -9.188101187500091527 ) ) ;
#94779 = CARTESIAN_POINT ( 'NONE',  ( -31.49356256989596758, 94.88921800892812541, 45.19948692389422717 ) ) ;
#94780 = ADVANCED_FACE ( 'NONE', ( #1205 ), #70084, .F. ) ;
#94781 = CARTESIAN_POINT ( 'NONE',  ( 203.0006266442389062, 270.0465963985643612, -6.413920096036100915 ) ) ;
#94782 = CARTESIAN_POINT ( 'NONE',  ( 190.7569505155522904, 300.2462651405980978, -5.670926626284815697 ) ) ;
#94783 = LINE ( 'NONE', #24840, #69306 ) ;
#94784 = ORIENTED_EDGE ( 'NONE', *, *, #78318, .T. ) ;
#94785 = CARTESIAN_POINT ( 'NONE',  ( 66.27113406421898389, 69.38871762109552321, 0.1120879072176016594 ) ) ;
#94786 = CARTESIAN_POINT ( 'NONE',  ( 163.7166294601506991, 282.3380383384618995, 10.03031969300557513 ) ) ;
#94787 = CARTESIAN_POINT ( 'NONE',  ( 147.1567732723861468, 275.7639873447703280, 6.815990338468913556 ) ) ;
#94788 = CARTESIAN_POINT ( 'NONE',  ( -21.88991730065903596, 40.08839396453016235, 59.99999999999999289 ) ) ;
#94789 = CARTESIAN_POINT ( 'NONE',  ( 25.52954022263672940, 23.24335787977764411, -9.188101187500008038 ) ) ;
#94790 = CARTESIAN_POINT ( 'NONE',  ( 202.3421728196210552, 280.1800714929709670, 16.85915999540957344 ) ) ;
#94791 = CARTESIAN_POINT ( 'NONE',  ( 149.2765980486851731, 272.0923431290771646, -11.40617906909507973 ) ) ;
#94792 = CARTESIAN_POINT ( 'NONE',  ( 188.8661607138717216, 269.9864860826438644, -14.08757442533680937 ) ) ;
#94793 = ORIENTED_EDGE ( 'NONE', *, *, #84447, .F. ) ;
#94794 = CARTESIAN_POINT ( 'NONE',  ( 8.860943796042899834, 20.51421378149916919, -9.188101187500004485 ) ) ;
#94795 = DIRECTION ( 'NONE',  ( 0.2500151307524129396, -0.9682419296822740717, 0.000000000000000000 ) ) ;
#94796 = CARTESIAN_POINT ( 'NONE',  ( 18.75993726342624157, 49.68311261143426805, 59.99999999999999289 ) ) ;
#94797 = CARTESIAN_POINT ( 'NONE',  ( 87.80398682648640829, 44.12684940286039392, 2.720675826359043370 ) ) ;
#94798 = VERTEX_POINT ( 'NONE', #70591 ) ;
#94799 = CARTESIAN_POINT ( 'NONE',  ( 72.22232072300009520, 71.11120588350317462, -5.989663598951492141 ) ) ;
#94800 = B_SPLINE_CURVE_WITH_KNOTS ( 'NONE', 3,
 ( #60187, #59703, #15093, #84554, #38395, #44998, #36400 ),
 .UNSPECIFIED., .F., .F.,
 ( 4, 3, 4 ),
 ( 2.060279009607550184E-15, 0.001498044985907314363, 0.002185450007172562263 ),
 .UNSPECIFIED. ) ;
#94801 = CARTESIAN_POINT ( 'NONE',  ( 85.56434759925559774, 49.01624254635854783, 12.26054419347457092 ) ) ;
#94802 = CARTESIAN_POINT ( 'NONE',  ( -67.91103796225580425, 44.10201266000169795, 10.00000000000000000 ) ) ;
#94803 = CARTESIAN_POINT ( 'NONE',  ( 149.4539134692060145, 271.7852238117696402, 12.95627816374690688 ) ) ;
#94804 = ORIENTED_EDGE ( 'NONE', *, *, #21934, .F. ) ;
#94805 = ORIENTED_EDGE ( 'NONE', *, *, #3423, .F. ) ;
#94807 = CARTESIAN_POINT ( 'NONE',  ( 163.2324542190761747, 279.0921727632539842, -13.03962765338508945 ) ) ;
#94806 = CARTESIAN_POINT ( 'NONE',  ( 188.9222622718724836, 273.7787661784663555, -15.66217235147567344 ) ) ;
#94808 = ORIENTED_EDGE ( 'NONE', *, *, #25109, .F. ) ;
#94809 = CARTESIAN_POINT ( 'NONE',  ( 45.60499120716188060, 26.73415679381826138, -6.890680421881970419E-14 ) ) ;
#94810 = DIRECTION ( 'NONE',  ( -0.9659258262890627611, 0.2588190451025410566, 1.149007080238459400E-14 ) ) ;
#94811 = CARTESIAN_POINT ( 'NONE',  ( 72.98918101599892339, 57.62492086428549243, -16.32278002199753075 ) ) ;
#94812 = CARTESIAN_POINT ( 'NONE',  ( -19.65312891409030271, 93.06504152958497400, 10.00000000000000888 ) ) ;
#94813 = CARTESIAN_POINT ( 'NONE',  ( 157.1965120183049578, 258.3746497421212780, -18.06591467563559306 ) ) ;
#94814 = CARTESIAN_POINT ( 'NONE',  ( 99.22679203974934126, 240.3464784336661637, 1.353441290958777525E-15 ) ) ;
#94815 = CARTESIAN_POINT ( 'NONE',  ( 182.9913983929653796, 288.1037905649602635, -13.18133572435033862 ) ) ;
#94816 = VECTOR ( 'NONE', #638, 1000.000000000000000 ) ;
#94817 = ORIENTED_EDGE ( 'NONE', *, *, #17613, .F. ) ;
#94818 = DIRECTION ( 'NONE',  ( -0.5544813661758285495, -0.8321961394790213795, 0.000000000000000000 ) ) ;
#94819 = ORIENTED_EDGE ( 'NONE', *, *, #53344, .T. ) ;
#94820 = CARTESIAN_POINT ( 'NONE',  ( 26.18145187173165311, 30.51421378149920116, -9.188101187500004485 ) ) ;
#94821 = CARTESIAN_POINT ( 'NONE',  ( 157.1924206424350814, 259.3163744206771639, 17.17865936927501380 ) ) ;
#94822 = CARTESIAN_POINT ( 'NONE',  ( 67.73131330550826590, 69.99787020178199271, -2.592847403169493692 ) ) ;
#94823 = CARTESIAN_POINT ( 'NONE',  ( 62.31280629920263436, 206.7833772461660828, -9.188101187500095079 ) ) ;
#94824 = CARTESIAN_POINT ( 'NONE',  ( 74.39896838111268096, 68.39356553035000275, 11.80479640254016083 ) ) ;
#94825 = CARTESIAN_POINT ( 'NONE',  ( 23.99212445955422623, 54.95143152255312913, 59.99999999999999289 ) ) ;
#94826 = CARTESIAN_POINT ( 'NONE',  ( 198.3791677596651368, 287.0441976074670833, 16.95474403075850134 ) ) ;
#94827 = AXIS2_PLACEMENT_3D ( 'NONE', #39980, #55184, #24308 ) ;
#94828 = CARTESIAN_POINT ( 'NONE',  ( -54.25663331465118233, 31.91744790946455979, -10.00000000000000000 ) ) ;
#94829 = ORIENTED_EDGE ( 'NONE', *, *, #1510, .F. ) ;
#94830 = CARTESIAN_POINT ( 'NONE',  ( 76.81910699536521747, 57.83062468730825856, -16.12375912510302101 ) ) ;
#94831 = CARTESIAN_POINT ( 'NONE',  ( 84.65917736194083432, 42.99992238498651886, -4.794713744061861682 ) ) ;
#94832 = CARTESIAN_POINT ( 'NONE',  ( 177.9680647294031246, 288.9635307193505582, 11.07995066775972326 ) ) ;
#94833 = CARTESIAN_POINT ( 'NONE',  ( 189.9457600613112902, 301.6512882219586800, 0.04117870562599101891 ) ) ;
#94834 = ORIENTED_EDGE ( 'NONE', *, *, #25276, .F. ) ;
#94835 = CARTESIAN_POINT ( 'NONE',  ( 174.8478238567398080, 261.1473787441764784, -14.11631832387472762 ) ) ;
#94836 = CARTESIAN_POINT ( 'NONE',  ( 174.1347695310112158, 277.0700907782643299, -15.64018019512398361 ) ) ;
#94837 = CARTESIAN_POINT ( 'NONE',  ( 161.1747502674735415, 251.4841389699472529, -13.25152330924089839 ) ) ;
#94838 = ADVANCED_FACE ( 'NONE', ( #24496 ), #55375, .T. ) ;
#94839 = CARTESIAN_POINT ( 'NONE',  ( 147.5118896528469179, 275.1489077312122049, -3.975523961781759930 ) ) ;
#94840 = DIRECTION ( 'NONE',  ( 0.000000000000000000, 0.000000000000000000, 1.000000000000000000 ) ) ;
#94841 = CARTESIAN_POINT ( 'NONE',  ( 83.33466500116428222, 41.42342953991349219, -0.2387503505471941512 ) ) ;
#94842 = CARTESIAN_POINT ( 'NONE',  ( 85.82824564990275462, 42.91066052166247147, -4.076138561270094662 ) ) ;
#94843 = CARTESIAN_POINT ( 'NONE',  ( 76.17367474885168122, 65.32298633591217651, 14.07450646204639355 ) ) ;
#94844 = CARTESIAN_POINT ( 'NONE',  ( 167.5479283814150051, 256.4993515244221385, 13.68654468072246466 ) ) ;
#94845 = DIRECTION ( 'NONE',  ( -0.8660254037844379305, -0.5000000000000015543, -0.000000000000000000 ) ) ;
#94846 = CARTESIAN_POINT ( 'NONE',  ( 110.3772162092389948, 234.5333772461660828, 9.188101187500095079 ) ) ;
#94847 = EDGE_LOOP ( 'NONE', ( #66175, #8794, #62089, #86627 ) ) ;
#94848 = CARTESIAN_POINT ( 'NONE',  ( 147.1731211915891322, 275.7356719181125868, 0.5879280619134324981 ) ) ;
#94849 = CARTESIAN_POINT ( 'NONE',  ( 83.98760013881610575, 42.11425398099174089, 2.993173605489666933 ) ) ;
#94850 = CARTESIAN_POINT ( 'NONE',  ( 154.9528145190857344, 262.2608478075840708, -17.26679351315302213 ) ) ;
#94851 = AXIS2_PLACEMENT_3D ( 'NONE', #44233, #27071, #65061 ) ;
#94852 = CARTESIAN_POINT ( 'NONE',  ( 204.2129321040862919, 276.9398213635460024, 14.41515352680879758 ) ) ;
#94853 = CARTESIAN_POINT ( 'NONE',  ( 83.73048316204189234, 51.68689211301329323, -14.84080274415373069 ) ) ;
#94854 = CARTESIAN_POINT ( 'NONE',  ( 76.38896655220229093, 51.63588879817334742, -15.66987219493312367 ) ) ;
#94855 = ORIENTED_EDGE ( 'NONE', *, *, #97124, .T. ) ;
#94856 = CARTESIAN_POINT ( 'NONE',  ( 80.46893305712502809, 57.11762031667031891, -16.22953243887947039 ) ) ;
#94857 = CARTESIAN_POINT ( 'NONE',  ( 154.8126376379091482, 273.3510647301234258, -13.05415025889605651 ) ) ;
#94858 = CARTESIAN_POINT ( 'NONE',  ( 185.2040473238361074, 261.9552295311297598, 9.692790394095107231 ) ) ;
#94859 = DIRECTION ( 'NONE',  ( -0.000000000000000000, 0.000000000000000000, -1.000000000000000000 ) ) ;
#94860 = CARTESIAN_POINT ( 'NONE',  ( 135.2750994722765654, 261.1589784336661637, -6.496448406907676862E-16 ) ) ;
#94861 = CARTESIAN_POINT ( 'NONE',  ( 190.6639305750654785, 294.8294108904519248, -12.23618567142708002 ) ) ;
#94862 = CARTESIAN_POINT ( 'NONE',  ( 189.1009243799269939, 299.7219271834727010, 4.948171813933484486 ) ) ;
#94863 = B_SPLINE_CURVE_WITH_KNOTS ( 'NONE', 3,
 ( #37728, #28648, #99558, #98580, #59530, #30141, #61026, #84382, #45819, #76743, #21083, #62016, #7847, #17442, #86906, #8346, #78757, #24534, #62517, #55912, #40218, #46839, #54933, #92968, #48348, #38731, #16932, #71670, #23522, #47332, #24033 ),
 .UNSPECIFIED., .F., .F.,
 ( 4, 3, 3, 3, 3, 3, 3, 3, 3, 3, 4 ),
 ( 0.000000000000000000, 0.1333490885032361239, 0.3007194338854258242, 0.4699862290245113705, 0.5844252810809250631, 0.6686540514502664623, 0.7354980260655568092, 0.8028463152565741279, 0.8633854507757309227, 0.9437142632667492315, 1.000000000000000000 ),
 .UNSPECIFIED. ) ;
#94864 = DIRECTION ( 'NONE',  ( 0.9805290675673896672, 0.1963739994383812415, 0.000000000000000000 ) ) ;
#94865 = B_SPLINE_CURVE_WITH_KNOTS ( 'NONE', 3,
 ( #97850, #93128, #60301, #37509 ),
 .UNSPECIFIED., .F., .F.,
 ( 4, 4 ),
 ( 0.000000000000000000, 0.001113216594625077464 ),
 .UNSPECIFIED. ) ;
#94866 = CARTESIAN_POINT ( 'NONE',  ( 66.15596757637857195, 202.8768266524160140, 9.188101187500098632 ) ) ;
#94867 = CARTESIAN_POINT ( 'NONE',  ( 71.22183910690829123, 62.20025648080263636, -14.61908299792422561 ) ) ;
#94868 = CARTESIAN_POINT ( 'NONE',  ( 157.4211152037729562, 257.9856256133486454, -16.71526195140576831 ) ) ;
#94869 = CARTESIAN_POINT ( 'NONE',  ( 88.01747121012718367, 44.57676444843377794, -4.047986979593448886 ) ) ;
#94870 = CARTESIAN_POINT ( 'NONE',  ( 69.36155480510052485, 70.48406901999045715, -2.430337453229784561 ) ) ;
#94871 = CARTESIAN_POINT ( 'NONE',  ( 174.5041736941544741, 262.1790157217919273, 14.33285218853700549 ) ) ;
#94872 = CARTESIAN_POINT ( 'NONE',  ( 81.56932236973577233, 41.66854487856439704, 5.818248598875920052 ) ) ;
#94873 = CARTESIAN_POINT ( 'NONE',  ( 178.8774038177254226, 291.7538915902231906, -6.223713788846963801 ) ) ;
#94874 = CARTESIAN_POINT ( 'NONE',  ( 203.5477091018662748, 278.0920214017542662, -16.09930363698006062 ) ) ;
#94875 = CARTESIAN_POINT ( 'NONE',  ( 153.6323727466833873, 269.3172676078306154, -15.66543061290010641 ) ) ;
#94876 = CARTESIAN_POINT ( 'NONE',  ( 122.4023397829301700, 248.1427522451419065, -10.00000000000009415 ) ) ;
#94877 = CARTESIAN_POINT ( 'NONE',  ( 25.03708881625784244, 16.58380873178787596, 6.180339887498953466 ) ) ;
#94878 = VERTEX_POINT ( 'NONE', #93438 ) ;
#94879 = CARTESIAN_POINT ( 'NONE',  ( 189.9925954911225290, 301.5701668779311717, 0.1154287172046158938 ) ) ;
#94880 = CARTESIAN_POINT ( 'NONE',  ( 10.22618198766610575, 28.83705186507752671, 3.090169943749475401 ) ) ;
#94882 = EDGE_CURVE ( 'NONE', #9557, #99079, #1137, .T. ) ;
#94881 = CIRCLE ( 'NONE', #65768, 11.91750000000000043 ) ;
#94883 = CARTESIAN_POINT ( 'NONE',  ( 40.22915850269944116, 194.0333772461660544, 9.188101187500095079 ) ) ;
#94884 = CARTESIAN_POINT ( 'NONE',  ( 18.77112655976752009, 19.03677371833801502, 10.00000000000000533 ) ) ;
#94885 = CARTESIAN_POINT ( 'NONE',  ( 68.18482425360609511, 65.67105585894155695, -10.27890673059631510 ) ) ;
#94887 = AXIS2_PLACEMENT_3D ( 'NONE', #69248, #100176, #14064 ) ;
#94886 = CARTESIAN_POINT ( 'NONE',  ( -27.42236680055714260, 166.5217562850347406, 1.224646799147364892E-15 ) ) ;
#94888 = CARTESIAN_POINT ( 'NONE',  ( 147.0670278774466908, 275.9194309285509235, 3.666898409139099257 ) ) ;
#94889 = CARTESIAN_POINT ( 'NONE',  ( 22.66956910419568061, 38.88013629349136835, -10.00000000000000000 ) ) ;
#94891 = CARTESIAN_POINT ( 'NONE',  ( 57.59477206639465408, 217.3927522451419634, 2.944929066748280225E-16 ) ) ;
#94890 = CARTESIAN_POINT ( 'NONE',  ( 198.2531640016911467, 277.4683007453174355, -15.40479037756460912 ) ) ;
#94892 = DIRECTION ( 'NONE',  ( 0.8660254037844385966, 0.5000000000000004441, 0.000000000000000000 ) ) ;
#94893 = CARTESIAN_POINT ( 'NONE',  ( 181.6765490640407847, 256.7658362468879432, 1.316456346048687998 ) ) ;
#94894 = CARTESIAN_POINT ( 'NONE',  ( 158.8270733235451075, 260.0119502166541565, 17.68969926203419618 ) ) ;
#94895 = CARTESIAN_POINT ( 'NONE',  ( 162.2082684172974325, 251.9275946936870980, -13.07642668292197285 ) ) ;
#94896 =( BOUNDED_CURVE ( )  B_SPLINE_CURVE ( 2, ( #10731, #64926, #58304, #3153, #95872, #57309, #49713, #80668, #88279 ),
 .UNSPECIFIED., .F., .T. ) 
 B_SPLINE_CURVE_WITH_KNOTS ( ( 3, 2, 2, 2, 3 ),
 ( 0.05241935483870967943, 0.05376344086021505458, 0.05645161290322580488, 0.05913978494623656212, 0.06048387096774193727 ),
 .UNSPECIFIED. ) 
 CURVE ( )  GEOMETRIC_REPRESENTATION_ITEM ( )  RATIONAL_B_SPLINE_CURVE ( ( 0.9330127018922194093, 0.9330127018922194093, 1.000000000000000000, 0.8660254037844387076, 1.000000000000000000, 0.8660254037844387076, 1.000000000000000000, 0.9330127018922194093, 0.9330127018922194093 ) ) 
 REPRESENTATION_ITEM ( '' )  );
#94897 = ORIENTED_EDGE ( 'NONE', *, *, #62419, .F. ) ;
#94898 = CARTESIAN_POINT ( 'NONE',  ( 26.50806851326374414, 176.1115022471901739, -5.000000000000041744 ) ) ;
#94899 = CARTESIAN_POINT ( 'NONE',  ( 184.5457051153594534, 294.3635293766698169, 10.03055039675435367 ) ) ;
#94900 = CARTESIAN_POINT ( 'NONE',  ( 162.6220573360242270, 248.9773295930640131, 10.49878733418918486 ) ) ;
#94901 = CARTESIAN_POINT ( 'NONE',  ( -8.160010933756074891, 166.0958772461660544, -9.188101187500095079 ) ) ;
#94902 = CARTESIAN_POINT ( 'NONE',  ( 38.86330120330953974, 24.29860640527295246, -2.839279412974138328 ) ) ;
#94905 = EDGE_CURVE ( 'NONE', #74796, #57299, #10811, .T. ) ;
#94904 = CARTESIAN_POINT ( 'NONE',  ( 170.9231213378963616, 262.8267322446009757, 16.60664178200664409 ) ) ;
#94903 = CARTESIAN_POINT ( 'NONE',  ( 163.5210672374943783, 252.3610180297824570, 13.14880157932337390 ) ) ;
#94906 = CARTESIAN_POINT ( 'NONE',  ( 152.9262073036446168, 265.7710344717137900, 16.19159804214501008 ) ) ;
#94907 = CARTESIAN_POINT ( 'NONE',  ( 33.90351810284484202, 25.28920272979928896, -7.433330006724141015 ) ) ;
#94908 = CARTESIAN_POINT ( 'NONE',  ( 55.54027346828191725, 191.3262482093457777, 3.021315404115420679E-15 ) ) ;
#94909 = CARTESIAN_POINT ( 'NONE',  ( 183.3631853222992163, 257.4081984927463509, -1.690945316791027109 ) ) ;
#94910 = CARTESIAN_POINT ( 'NONE',  ( -71.61465314115659453, 63.06504152958490295, 60.00000000000000000 ) ) ;
#94911 = VERTEX_POINT ( 'NONE', #80759 ) ;
#94912 = CARTESIAN_POINT ( 'NONE',  ( 148.9285945872975390, 272.6951028054104427, -12.01265727652413240 ) ) ;
#94913 = DIRECTION ( 'NONE',  ( 1.000000000000000000, 0.000000000000000000, 0.000000000000000000 ) ) ;
#94914 = CARTESIAN_POINT ( 'NONE',  ( 9.991594722369004700, 23.95586893147753926, 7.433330006724141015 ) ) ;
#94915 = CARTESIAN_POINT ( 'NONE',  ( 165.8902591964293549, 285.5389980135179258, 0.4923433930893942878 ) ) ;
#94916 = CARTESIAN_POINT ( 'NONE',  ( 16.72494223679300873, 27.84336893147755987, -7.433330006724137462 ) ) ;
#94917 = FACE_OUTER_BOUND ( 'NONE', #35989, .T. ) ;
#94918 = VECTOR ( 'NONE', #34856, 1000.000000000000000 ) ;
#94919 = CARTESIAN_POINT ( 'NONE',  ( 153.4678846701812915, 275.0478545690473879, 10.56604701146394376 ) ) ;
#94920 = FACE_OUTER_BOUND ( 'NONE', #33400, .T. ) ;
#94921 = CARTESIAN_POINT ( 'NONE',  ( 61.65426615018220957, 199.7365022471902023, -10.00000000000009237 ) ) ;
#94922 = ORIENTED_EDGE ( 'NONE', *, *, #39328, .F. ) ;
#94923 = EDGE_CURVE ( 'NONE', #43843, #72251, #26511, .T. ) ;
#94924 = CARTESIAN_POINT ( 'NONE',  ( 192.0645969571214096, 297.9813550654635605, 11.46542907566974812 ) ) ;
#94925 = CARTESIAN_POINT ( 'NONE',  ( 207.5686001603237116, 271.1276337968068333, 7.659944433763431704 ) ) ;
#94926 = CIRCLE ( 'NONE', #7514, 70.00000000000001421 ) ;
#94927 = CARTESIAN_POINT ( 'NONE',  ( 191.6219713859826186, 298.2580554142066376, 8.895068270853277781 ) ) ;
#94928 = CARTESIAN_POINT ( 'NONE',  ( 87.79538347886169447, 45.10662587206182650, 6.725936807544239393 ) ) ;
#94929 = CARTESIAN_POINT ( 'NONE',  ( 193.8603219414924013, 294.8710681561126989, 15.36476279452078586 ) ) ;
#94930 = EDGE_LOOP ( 'NONE', ( #3880, #85204, #30477, #47843 ) ) ;
#94931 = CARTESIAN_POINT ( 'NONE',  ( 158.7920399039511494, 277.9748776850930767, -9.821990816589480033 ) ) ;
#94932 = CARTESIAN_POINT ( 'NONE',  ( 86.18930939419189485, 47.16029689842823558, 10.81535065263619622 ) ) ;
#94933 = ORIENTED_EDGE ( 'NONE', *, *, #15028, .T. ) ;
#94934 = CARTESIAN_POINT ( 'NONE',  ( 77.97772543808913781, 58.87949468740131209, 16.12526282269577393 ) ) ;
#94935 = CARTESIAN_POINT ( 'NONE',  ( 155.5995420464182644, 262.6346450740109617, -17.48312782858739567 ) ) ;
#94936 = ORIENTED_EDGE ( 'NONE', *, *, #90945, .F. ) ;
#94937 = DIRECTION ( 'NONE',  ( 0.000000000000000000, 0.000000000000000000, 1.000000000000000000 ) ) ;
#94938 = DIRECTION ( 'NONE',  ( -0.5000000000000002220, 0.8660254037844385966, 0.000000000000000000 ) ) ;
#94939 = B_SPLINE_CURVE_WITH_KNOTS ( 'NONE', 3,
 ( #98763, #35439, #91173, #66342 ),
 .UNSPECIFIED., .F., .F.,
 ( 4, 4 ),
 ( 0.006879015221108502644, 0.01190597477310000214 ),
 .UNSPECIFIED. ) ;
#94940 = CARTESIAN_POINT ( 'NONE',  ( 80.51198428680064012, 43.68793065238016737, 9.861687463089005234 ) ) ;
#94941 = ORIENTED_EDGE ( 'NONE', *, *, #76895, .T. ) ;
#94942 = CARTESIAN_POINT ( 'NONE',  ( 200.9111546617170916, 282.6586676490145464, 17.66063511622358106 ) ) ;
#94943 = CARTESIAN_POINT ( 'NONE',  ( 166.1691510717052154, 273.9072633124648632, -15.34805146679062382 ) ) ;
#94944 = DIRECTION ( 'NONE',  ( -0.8660254037844377084, -0.5000000000000014433, -0.000000000000000000 ) ) ;
#94945 = CARTESIAN_POINT ( 'NONE',  ( 151.3795629253287132, 275.1161925579037870, -8.452185327743000798 ) ) ;
#94946 = VERTEX_POINT ( 'NONE', #49795 ) ;
#94947 = EDGE_CURVE ( 'NONE', #30622, #56696, #8169, .T. ) ;
#94948 = EDGE_CURVE ( 'NONE', #14526, #16186, #33609, .T. ) ;
#94949 = CARTESIAN_POINT ( 'NONE',  ( 171.1327466086072207, 254.6685794175523938, -11.52810047878565669 ) ) ;
#94950 = CARTESIAN_POINT ( 'NONE',  ( 39.11189823470242999, 30.78052372038643725, -10.00000000000000355 ) ) ;
#94951 = ORIENTED_EDGE ( 'NONE', *, *, #69760, .F. ) ;
#94952 = ORIENTED_EDGE ( 'NONE', *, *, #19780, .F. ) ;
#94953 = CARTESIAN_POINT ( 'NONE',  ( 160.0395937287001402, 268.6003992623327576, -16.49027686160719952 ) ) ;
#94954 = VERTEX_POINT ( 'NONE', #27006 ) ;
#94955 = CARTESIAN_POINT ( 'NONE',  ( 160.7841707400127405, 270.7800417481713566, 15.89061575048816444 ) ) ;
#94956 = ORIENTED_EDGE ( 'NONE', *, *, #51194, .F. ) ;
#94957 = EDGE_CURVE ( 'NONE', #32826, #96593, #42674, .T. ) ;
#94958 = DIRECTION ( 'NONE',  ( 0.000000000000000000, 0.6788029332000728999, 0.7343204871709473336 ) ) ;
#94959 = CARTESIAN_POINT ( 'NONE',  ( 147.7897704884714472, 274.6676040054608166, 7.256941229896001211 ) ) ;
#94960 = CARTESIAN_POINT ( 'NONE',  ( 190.5526305594705434, 299.9695577504274979, -4.324655322867677398 ) ) ;
#94961 = CARTESIAN_POINT ( 'NONE',  ( 72.11625326144877590, 70.64305112490642102, 6.725456730032719932 ) ) ;
#94962 = LINE ( 'NONE', #57914, #98700 ) ;
#94963 = CARTESIAN_POINT ( 'NONE',  ( 82.77886453090131624, 53.33514393157792455, -15.29216242284640437 ) ) ;
#94964 = EDGE_CURVE ( 'NONE', #88235, #36466, #65007, .T. ) ;
#94965 = DIRECTION ( 'NONE',  ( -0.2942337105004269593, -0.9557335003049495237, 0.000000000000000000 ) ) ;
#94966 = EDGE_LOOP ( 'NONE', ( #23001, #83595, #55124, #5691 ) ) ;
#94967 = CARTESIAN_POINT ( 'NONE',  ( -70.00000000000000000, 15.00000000000000000, -59.99999999999999289 ) ) ;
#94968 = CARTESIAN_POINT ( 'NONE',  ( 22.77687932801360660, 15.01110640527292261, 2.839279412974134775 ) ) ;
#94969 = VECTOR ( 'NONE', #33288, 1000.000000000000114 ) ;
#94970 = CARTESIAN_POINT ( 'NONE',  ( 205.8030308266901898, 274.1856895869457844, 10.55961490432110317 ) ) ;
#94971 = CARTESIAN_POINT ( 'NONE',  ( 164.8537203408104972, 245.1119758834023230, 2.926011033004258355 ) ) ;
#94973 = VERTEX_POINT ( 'NONE', #34594 ) ;
#94972 = CARTESIAN_POINT ( 'NONE',  ( 159.5284711081640125, 254.3355781173132755, 15.34104435652608522 ) ) ;
#94974 = VECTOR ( 'NONE', #42058, 1000.000000000000000 ) ;
#94975 = ORIENTED_EDGE ( 'NONE', *, *, #83937, .T. ) ;
#94976 = EDGE_CURVE ( 'NONE', #6051, #44888, #96442, .T. ) ;
#94977 = CARTESIAN_POINT ( 'NONE',  ( 168.3758771850754670, 256.9182401831289440, -14.77350533378223219 ) ) ;
#94978 = ADVANCED_FACE ( 'NONE', ( #64504 ), #4188, .T. ) ;
#94979 = CARTESIAN_POINT ( 'NONE',  ( 159.5050723400634638, 254.3761059724978679, -15.34938048045353298 ) ) ;
#94980 = DIRECTION ( 'NONE',  ( 0.5000000000000013323, -0.8660254037844378194, 0.000000000000000000 ) ) ;
#94981 = VECTOR ( 'NONE', #28015, 1000.000000000000114 ) ;
#94982 = B_SPLINE_CURVE_WITH_KNOTS ( 'NONE', 3,
 ( #5102, #66886, #43588, #52178 ),
 .UNSPECIFIED., .F., .F.,
 ( 4, 4 ),
 ( 0.0005619842127425911946, 0.0007738637477710976062 ),
 .UNSPECIFIED. ) ;
#94983 = CARTESIAN_POINT ( 'NONE',  ( 200.2316334480823912, 283.8356329158505105, 17.02791935830326508 ) ) ;
#94984 = CARTESIAN_POINT ( 'NONE',  ( 84.47860975560725194, 49.82577972120142817, -13.24615549146050952 ) ) ;
#94985 = ORIENTED_EDGE ( 'NONE', *, *, #41323, .T. ) ;
#94986 = CARTESIAN_POINT ( 'NONE',  ( 176.5337195050044556, 270.3037592414455048, -17.69951539620915071 ) ) ;
#94987 = DIRECTION ( 'NONE',  ( -0.000000000000000000, -0.000000000000000000, -1.000000000000000000 ) ) ;
#94988 = CARTESIAN_POINT ( 'NONE',  ( 36.67532856725514989, 51.07057046370195508, -10.00000000000000000 ) ) ;
#94989 = DIRECTION ( 'NONE',  ( 0.9888308262251265246, -0.1490422661761876266, 0.000000000000000000 ) ) ;
#94990 = CARTESIAN_POINT ( 'NONE',  ( 13.42747647338826589, 191.8927522451419350, 2.944929066748280225E-16 ) ) ;
#94991 = CARTESIAN_POINT ( 'NONE',  ( 97.33288211261837830, 220.8768266524160140, 9.188101187500096856 ) ) ;
#94992 = CARTESIAN_POINT ( 'NONE',  ( 82.16210765379520353, 40.80679471695141558, -1.129513917607761542 ) ) ;
#94993 = CARTESIAN_POINT ( 'NONE',  ( -21.75249381947928740, 146.7012482093458914, -48.95643923738973768 ) ) ;
#94994 = CARTESIAN_POINT ( 'NONE',  ( 162.6684717218148251, 248.8969375186720754, 11.76041465758671833 ) ) ;
#94995 = CARTESIAN_POINT ( 'NONE',  ( 28.72751893051112049, 178.2048013555409796, 4.594050593750051981 ) ) ;
#94996 = CARTESIAN_POINT ( 'NONE',  ( 161.1027382213887336, 251.6088674925233022, 13.55451100897754557 ) ) ;
#94997 = AXIS2_PLACEMENT_3D ( 'NONE', #91496, #23037, #75789 ) ;
#94998 = ORIENTED_EDGE ( 'NONE', *, *, #31635, .T. ) ;
#94999 = VECTOR ( 'NONE', #96853, 1000.000000000000000 ) ;
#95001 = ORIENTED_EDGE ( 'NONE', *, *, #11528, .T. ) ;
#95000 = UNCERTAINTY_MEASURE_WITH_UNIT (LENGTH_MEASURE( 1.000000000000000082E-05 ), #76207, 'distance_accuracy_value', 'NONE');
#95002 = CARTESIAN_POINT ( 'NONE',  ( 199.7522530777181089, 267.1256835885929490, -2.850022460144068237 ) ) ;
#95003 = CARTESIAN_POINT ( 'NONE',  ( 186.0244278979135117, 262.8604796214907537, 11.87503556831948615 ) ) ;
#95005 = B_SPLINE_CURVE_WITH_KNOTS ( 'NONE', 3,
 ( #9116, #48626, #63310, #64820, #47106, #79561, #10118, #64314, #8618, #95767, #26323, #66799, #11628, #97726, #65794, #12625 ),
 .UNSPECIFIED., .F., .F.,
 ( 4, 1, 2, 2, 2, 1, 2, 2, 4 ),
 ( 0.000000000000000000, 0.1250000000000013878, 0.1875000000000020817, 0.2500000000000027756, 0.5000000000000042188, 0.6250000000000046629, 0.6875000000000039968, 0.7500000000000032196, 1.000000000000000000 ),
 .UNSPECIFIED. ) ;
#95004 = VECTOR ( 'NONE', #43664, 1000.000000000000000 ) ;
#95006 = CARTESIAN_POINT ( 'NONE',  ( 82.65244178817603427, 41.86818416018829936, 4.798348907845769062 ) ) ;
#95007 = DIRECTION ( 'NONE',  ( 0.000000000000000000, 0.000000000000000000, 1.000000000000000000 ) ) ;
#95008 = CARTESIAN_POINT ( 'NONE',  ( 58.47569090598246788, 179.7419560658249509, -18.47570218321542868 ) ) ;
#95009 = CARTESIAN_POINT ( 'NONE',  ( 68.89470241882965240, 64.09230978405759060, 12.06256359161597125 ) ) ;
#95010 = CARTESIAN_POINT ( 'NONE',  ( 74.07678436671264421, 68.35284689741969544, -11.67875583378132198 ) ) ;
#95011 = CARTESIAN_POINT ( 'NONE',  ( 26.96797095936772237, 192.5024278399161233, 9.188101187500095079 ) ) ;
#95012 = CARTESIAN_POINT ( 'NONE',  ( 86.96746701141694302, 211.0177522451417929, 5.000000000000051514 ) ) ;
#95013 = CARTESIAN_POINT ( 'NONE',  ( 199.8909283227609990, 276.8366623509729152, 15.27167089021202351 ) ) ;
#95014 = ORIENTED_EDGE ( 'NONE', *, *, #87119, .T. ) ;
#95015 = CARTESIAN_POINT ( 'NONE',  ( 82.69279102287485728, 44.35692915535365444, 9.190022298575403426 ) ) ;
#95016 = DIRECTION ( 'NONE',  ( 0.5000000000000144329, -0.8660254037844303809, -1.474271392894062072E-14 ) ) ;
#95017 = EDGE_CURVE ( 'NONE', #96205, #63867, #96633, .T. ) ;
#95018 = CARTESIAN_POINT ( 'NONE',  ( -6.536213301660246167, 167.0333772461660828, 9.188101187500095079 ) ) ;
#95019 = CARTESIAN_POINT ( 'NONE',  ( 68.49778638537657116, 64.30983983548141225, -12.35708682889201171 ) ) ;
#95020 = CARTESIAN_POINT ( 'NONE',  ( 207.7296438747196134, 270.8486979012336633, -6.692930657757584001 ) ) ;
#95021 = CARTESIAN_POINT ( 'NONE',  ( 186.5316309442283114, 282.7232008768231140, 16.16643943244534398 ) ) ;
#95022 = CARTESIAN_POINT ( 'NONE',  ( 148.4042165687623083, 273.6033521758856750, -8.709765892313745539 ) ) ;
#95023 = ADVANCED_FACE ( 'NONE', ( #58383 ), #66980, .F. ) ;
#95024 = CARTESIAN_POINT ( 'NONE',  ( 67.23469673426404825, 68.21886821911095922, -6.894059962813373410 ) ) ;
#95025 = CARTESIAN_POINT ( 'NONE',  ( 204.8284483594339065, 275.8737159363993214, 14.69997973035875383 ) ) ;
#95026 = CARTESIAN_POINT ( 'NONE',  ( 191.8329718516215223, 298.3825415164982928, -8.871589506312979267 ) ) ;
#95027 = CARTESIAN_POINT ( 'NONE',  ( 207.1122325394003951, 271.9180857031755636, 7.794245785756032774 ) ) ;
#95028 = ORIENTED_EDGE ( 'NONE', *, *, #70725, .T. ) ;
#95029 = CARTESIAN_POINT ( 'NONE',  ( 136.8541387121308617, 256.4865022471902876, -10.00000000000009592 ) ) ;
#95030 = CARTESIAN_POINT ( 'NONE',  ( 118.9295641673753181, 227.2202760586659736, -5.415160957724236172E-17 ) ) ;
#95031 = CARTESIAN_POINT ( 'NONE',  ( 14.85459438965255607, 31.68290643055187061, 3.479690158560446702E-15 ) ) ;
#95033 = EDGE_CURVE ( 'NONE', #2343, #58518, #5197, .T. ) ;
#95032 = CARTESIAN_POINT ( 'NONE',  ( 75.29614551415185986, 66.72342768736930907, 13.41754944753248502 ) ) ;
#95034 = DIRECTION ( 'NONE',  ( 0.000000000000000000, 0.000000000000000000, 1.000000000000000000 ) ) ;
#95036 = PLANE ( 'NONE',  #44097 ) ;
#95035 = PLANE ( 'NONE',  #37125 ) ;
#95037 = CARTESIAN_POINT ( 'NONE',  ( 191.1107143855515176, 299.6335281438774700, -6.486502120340617239 ) ) ;
#95038 = ORIENTED_EDGE ( 'NONE', *, *, #85046, .F. ) ;
#95039 = CARTESIAN_POINT ( 'NONE',  ( 189.6294122595523675, 261.2013800515091475, -4.514607050631846086 ) ) ;
#95040 = CARTESIAN_POINT ( 'NONE',  ( 196.4170778717353585, 290.4426369823788718, -17.78762421190030452 ) ) ;
#95041 = CIRCLE ( 'NONE', #28677, 0.1418229129681557177 ) ;
#95042 = CARTESIAN_POINT ( 'NONE',  ( 33.63888670793727442, 47.67824751478843126, -10.00000000000000000 ) ) ;
#95043 = CARTESIAN_POINT ( 'NONE',  ( 173.5071485195266803, 289.9167268689076877, -1.068890946380929075 ) ) ;
#95044 = CARTESIAN_POINT ( 'NONE',  ( 194.4178591205541409, 270.7991877699529937, -14.20622043910200460 ) ) ;
#95045 = VERTEX_POINT ( 'NONE', #27985 ) ;
#95046 = LINE ( 'NONE', #25609, #60220 ) ;
#95047 = CARTESIAN_POINT ( 'NONE',  ( 175.5424091614122517, 278.6358477417585959, 15.42837206623358348 ) ) ;
#95048 = AXIS2_PLACEMENT_3D ( 'NONE', #96577, #2344, #27142 ) ;
#95049 = CARTESIAN_POINT ( 'NONE',  ( 166.5715075414655360, 270.4169618060113862, -16.29706984472633735 ) ) ;
#95050 = EDGE_CURVE ( 'NONE', #62248, #8715, #45176, .T. ) ;
#95051 = B_SPLINE_SURFACE_WITH_KNOTS ( 'NONE', 3, 1, ( 
 ( #42893, #79971 ),
 ( #34812, #3929 ),
 ( #19652, #18137 ),
 ( #49037, #2963 ),
 ( #95177, #80983 ),
 ( #97168, #34330 ),
 ( #4422, #65713 ),
 ( #49524, #58602 ),
 ( #87609, #56626 ),
 ( #73833, #96668 ),
 ( #27236, #65226 ),
 ( #33857, #66231 ),
 ( #95691, #89102 ),
 ( #96169, #26730 ),
 ( #11549, #26238 ),
 ( #79476, #88593 ),
 ( #42408, #19155 ),
 ( #50514, #81466 ),
 ( #12040, #17639 ),
 ( #48537, #10040 ),
 ( #71851, #2448 ),
 ( #33330, #25747 ),
 ( #64227, #99007 ),
 ( #68085, #29591 ),
 ( #6293, #12538 ),
 ( #89578, #43411 ),
 ( #37185, #74358 ),
 ( #20141, #51012 ),
 ( #81963, #61812 ),
 ( #95153, #34303 ),
 ( #23317, #54204 ) ),
 .UNSPECIFIED., .F., .F., .F.,
 ( 4, 3, 3, 3, 3, 3, 3, 3, 3, 3, 4 ),
 ( 2, 2 ),
 ( 0.000000000000000000, 0.1122669598086755566, 0.2243161639709691235, 0.3396355846219065722, 0.4553962076585197916, 0.5677860799922422874, 0.6749047109689728652, 0.7773884377078309482, 0.8775581155834237812, 0.9782364162377977790, 1.000000000000000000 ),
 ( 0.000000000000000000, 1.000000000000000000 ),
 .UNSPECIFIED. ) ;
#95052 = EDGE_CURVE ( 'NONE', #36208, #40063, #20409, .T. ) ;
#95053 = CARTESIAN_POINT ( 'NONE',  ( 200.2438720683531415, 272.4341333479218861, 12.65294705144797760 ) ) ;
#95054 = CARTESIAN_POINT ( 'NONE',  ( 83.82265501036586386, 51.54306753207543323, -14.37114190926680557 ) ) ;
#95055 = CARTESIAN_POINT ( 'NONE',  ( 72.26191451101281871, 71.91445694603925176, -5.118044210176695863 ) ) ;
#95056 = CARTESIAN_POINT ( 'NONE',  ( 152.7153488183568300, 266.1362520814392951, 17.33540622643059237 ) ) ;
#95057 = VECTOR ( 'NONE', #87541, 1000.000000000000000 ) ;
#95058 = ORIENTED_EDGE ( 'NONE', *, *, #49119, .F. ) ;
#95059 = CARTESIAN_POINT ( 'NONE',  ( 65.48286763772492236, 61.30466486950707150, 0.000000000000000000 ) ) ;
#95060 = AXIS2_PLACEMENT_3D ( 'NONE', #81933, #67689, #36781 ) ;
#95061 = CARTESIAN_POINT ( 'NONE',  ( 35.86231599663030067, 42.74646525600393687, 2.839279412974139660 ) ) ;
#95062 = CARTESIAN_POINT ( 'NONE',  ( 192.2621181266863459, 288.2322237920654402, -15.87800504598256168 ) ) ;
#95063 = ORIENTED_EDGE ( 'NONE', *, *, #42677, .F. ) ;
#95064 = CARTESIAN_POINT ( 'NONE',  ( 167.8294318762166029, 280.8099396157227829, 12.36612508801571231 ) ) ;
#95065 = CARTESIAN_POINT ( 'NONE',  ( 194.6943296385021824, 293.4265244509877562, -16.10917128197217352 ) ) ;
#95066 = CARTESIAN_POINT ( 'NONE',  ( 21.64925731690437516, 171.7592609112379876, 2.679491924311254714 ) ) ;
#95067 = ORIENTED_EDGE ( 'NONE', *, *, #39468, .F. ) ;
#95068 = CARTESIAN_POINT ( 'NONE',  ( 78.72187027071313992, 59.93413112120518349, 16.11827352649737222 ) ) ;
#95069 = CARTESIAN_POINT ( 'NONE',  ( 188.6836721603714864, 293.3912136806342232, 12.63380796591361133 ) ) ;
#95070 = CARTESIAN_POINT ( 'NONE',  ( 88.44601041138486153, 44.07807065378580802, -2.614235559790803798 ) ) ;
#95071 = FACE_OUTER_BOUND ( 'NONE', #47860, .T. ) ;
#95072 = AXIS2_PLACEMENT_3D ( 'NONE', #32354, #9061, #2475 ) ;
#95073 = CARTESIAN_POINT ( 'NONE',  ( 80.19020872641095821, 44.76014306349777883, 11.12255406994323792 ) ) ;
#95074 = CARTESIAN_POINT ( 'NONE',  ( 155.6328838216860220, 261.0829332228125850, -17.51014940606912518 ) ) ;
#95075 = EDGE_LOOP ( 'NONE', ( #33227, #29140, #43343, #51306 ) ) ;
#95076 = EDGE_CURVE ( 'NONE', #36862, #11831, #35594, .T. ) ;
#95077 = ORIENTED_EDGE ( 'NONE', *, *, #306, .T. ) ;
#95078 = CARTESIAN_POINT ( 'NONE',  ( 175.6813301723168479, 259.2852654454819117, 12.45547364025740045 ) ) ;
#95079 = ORIENTED_EDGE ( 'NONE', *, *, #95662, .T. ) ;
#95080 = FACE_OUTER_BOUND ( 'NONE', #53840, .T. ) ;
#95081 = ORIENTED_EDGE ( 'NONE', *, *, #76524, .T. ) ;
#95082 = CARTESIAN_POINT ( 'NONE',  ( 173.2789054804935631, 270.6729449864580488, 16.65581685045554039 ) ) ;
#95083 = CARTESIAN_POINT ( 'NONE',  ( 203.4696564630250464, 278.2272125378923988, -16.38980782817167636 ) ) ;
#95084 = ORIENTED_EDGE ( 'NONE', *, *, #8362, .F. ) ;
#95085 = ADVANCED_FACE ( 'NONE', ( #97907 ), #19911, .T. ) ;
#95086 = CARTESIAN_POINT ( 'NONE',  ( 186.0705390081322435, 282.4759132538421227, -17.12146972818776547 ) ) ;
#95087 = CARTESIAN_POINT ( 'NONE',  ( 164.3883575065421496, 245.9180079563093955, -2.230252308397467687 ) ) ;
#95088 = CARTESIAN_POINT ( 'NONE',  ( 147.8696095030242645, 274.5293187758293811, -6.165255295277477288 ) ) ;
#95089 = CARTESIAN_POINT ( 'NONE',  ( 158.4485968073939546, 275.2084588272041401, -13.86993402366507944 ) ) ;
#95090 = DIRECTION ( 'NONE',  ( 0.3400251696390307887, -0.9404163354663445107, 0.000000000000000000 ) ) ;
#95091 = CARTESIAN_POINT ( 'NONE',  ( 200.8251833487811666, 282.8075743310126882, -16.74393672780000131 ) ) ;
#95092 = DIRECTION ( 'NONE',  ( 0.4552093898365223712, -0.8903844177683372108, 0.000000000000000000 ) ) ;
#95093 = CARTESIAN_POINT ( 'NONE',  ( 153.9280534239306917, 279.9716514717067639, 2.220587593257353554 ) ) ;
#95094 = ADVANCED_FACE ( 'NONE', ( #83727 ), #37564, .T. ) ;
#95095 = CARTESIAN_POINT ( 'NONE',  ( 135.2486435959970947, 239.7048013555409796, 4.594050593750051981 ) ) ;
#95096 = CARTESIAN_POINT ( 'NONE',  ( 70.97972651378927367, 61.11640933415372245, -14.48974805571130098 ) ) ;
#95097 = CARTESIAN_POINT ( 'NONE',  ( 4.275827057391709651, 20.65586893147753500, -7.433330006724137462 ) ) ;
#95098 = ORIENTED_EDGE ( 'NONE', *, *, #41874, .T. ) ;
#95099 = EDGE_CURVE ( 'NONE', #83325, #75846, #27514, .T. ) ;
#95101 = ORIENTED_EDGE ( 'NONE', *, *, #74601, .F. ) ;
#95100 = CARTESIAN_POINT ( 'NONE',  ( 82.92857491607050235, 43.40443588184567147, -8.571747185156002757 ) ) ;
#95102 = CARTESIAN_POINT ( 'NONE',  ( 203.5034052210150719, 276.4946534009981178, 13.91832450903958751 ) ) ;
#95103 = CARTESIAN_POINT ( 'NONE',  ( 177.5631567369229913, 253.5128631816587870, 1.374242336938259701 ) ) ;
#95104 = LINE ( 'NONE', #94589, #67369 ) ;
#95105 = CARTESIAN_POINT ( 'NONE',  ( 147.3869853863401715, 275.3652482668841230, 3.850002650366144419 ) ) ;
#95106 = CARTESIAN_POINT ( 'NONE',  ( 157.4449103128602587, 280.3754508376611057, -7.050241416987695686 ) ) ;
#95107 = CARTESIAN_POINT ( 'NONE',  ( 152.7729059155601021, 266.0365602647466972, -17.50667083025758686 ) ) ;
#95108 = CARTESIAN_POINT ( 'NONE',  ( 176.9886338728968553, 288.6665034793379050, -9.311589415884686360 ) ) ;
#95109 = CARTESIAN_POINT ( 'NONE',  ( 171.4101398265137846, 280.2079561268039924, 13.77150215915619214 ) ) ;
#95110 = CARTESIAN_POINT ( 'NONE',  ( 177.6986938504743136, 255.3162907930642405, -8.390269233711947550 ) ) ;
#95111 = ORIENTED_EDGE ( 'NONE', *, *, #56188, .T. ) ;
#95113 = CARTESIAN_POINT ( 'NONE',  ( 6.430760413625676186, 27.21091486745858390, -1.111400068045478839E-16 ) ) ;
#95112 = B_SPLINE_CURVE_WITH_KNOTS ( 'NONE', 3,
 ( #93057, #99152, #92096, #68730 ),
 .UNSPECIFIED., .F., .F.,
 ( 4, 4 ),
 ( 0.005695445479479283035, 0.01374854309124446533 ),
 .UNSPECIFIED. ) ;
#95114 = CARTESIAN_POINT ( 'NONE',  ( 13.90223112049948639, 33.06302660730329279, -10.00000000000000000 ) ) ;
#95115 = VERTEX_POINT ( 'NONE', #13786 ) ;
#95116 = DIRECTION ( 'NONE',  ( -0.000000000000000000, 0.000000000000000000, -1.000000000000000000 ) ) ;
#95117 = CARTESIAN_POINT ( 'NONE',  ( 201.1778739778297052, 267.9238834610532081, -2.849212060748330888 ) ) ;
#95118 = CARTESIAN_POINT ( 'NONE',  ( 152.5006243422696741, 266.5081657836506679, -15.99602084911275135 ) ) ;
#95119 = CARTESIAN_POINT ( 'NONE',  ( 190.2318383114841254, 301.1557861577188078, 3.177919994438449525 ) ) ;
#95120 = CARTESIAN_POINT ( 'NONE',  ( 162.9148248802443106, 248.4702413316674381, 9.709394404200100581 ) ) ;
#95122 = CARTESIAN_POINT ( 'NONE',  ( 160.9062962349007080, 281.5834788170423622, 5.946759227913918089 ) ) ;
#95121 = CARTESIAN_POINT ( 'NONE',  ( 163.4970835327194436, 283.9977148944103078, -7.100329127627979631 ) ) ;
#95123 = CARTESIAN_POINT ( 'NONE',  ( -22.42236680055709641, 157.8615022471902591, 0.000000000000000000 ) ) ;
#95124 = VERTEX_POINT ( 'NONE', #44663 ) ;
#95125 = CIRCLE ( 'NONE', #15800, 70.00000000000001421 ) ;
#95126 = CARTESIAN_POINT ( 'NONE',  ( 74.38266378283655911, 61.70959607653536239, -15.06044949738370065 ) ) ;
#95127 = CARTESIAN_POINT ( 'NONE',  ( 192.9525843507564957, 275.9342408156254578, -16.09309137864095263 ) ) ;
#95128 = CARTESIAN_POINT ( 'NONE',  ( 72.85736843160729848, 65.69469193138741048, -12.66355394330495976 ) ) ;
#95129 = CARTESIAN_POINT ( 'NONE',  ( 192.0331311261993790, 298.0358554833232461, 11.82583305898340953 ) ) ;
#95130 = LINE ( 'NONE', #78908, #52677 ) ;
#95131 = COLOUR_RGB ( '',0.7921568627450980005, 0.8196078431372548767, 0.9333333333333333481 ) ;
#95132 = DIRECTION ( 'NONE',  ( 0.02225111142182467291, 0.9997524133706773286, 0.000000000000000000 ) ) ;
#95133 = CARTESIAN_POINT ( 'NONE',  ( 70.35209472271311881, 71.19767260777499018, -1.695128100752382849 ) ) ;
#95134 = CARTESIAN_POINT ( 'NONE',  ( -8.782727014549898570, 174.9244531367911293, -4.594050593750046652 ) ) ;
#95135 = CARTESIAN_POINT ( 'NONE',  ( 81.20281187136818346, 223.8149278399160664, 9.188101187500093303 ) ) ;
#95136 = CARTESIAN_POINT ( 'NONE',  ( 87.93887446415499198, 44.76116579897428949, -4.704258403839746805 ) ) ;
#95137 = CARTESIAN_POINT ( 'NONE',  ( 193.8354046899084153, 268.4885937380259406, 12.87375928640720524 ) ) ;
#95138 = CARTESIAN_POINT ( 'NONE',  ( -7.266922234329411978, 166.6115022471902591, 10.00000000000009592 ) ) ;
#95139 = VECTOR ( 'NONE', #91189, 1000.000000000000000 ) ;
#95140 = CARTESIAN_POINT ( 'NONE',  ( -89.11465314115665137, 93.37593066204027537, 30.52142883766497405 ) ) ;
#95141 = AXIS2_PLACEMENT_3D ( 'NONE', #93324, #23877, #85757 ) ;
#95142 = CARTESIAN_POINT ( 'NONE',  ( 160.8951580803594936, 281.6687235497548727, 5.528266179044310391 ) ) ;
#95145 = CARTESIAN_POINT ( 'NONE',  ( 76.48451822609287376, 51.58183040335976699, 15.64690190214837173 ) ) ;
#95144 = B_SPLINE_CURVE_WITH_KNOTS ( 'NONE', 3,
 ( #52687, #98827, #13709, #53681 ),
 .UNSPECIFIED., .F., .F.,
 ( 4, 4 ),
 ( 0.000000000000000000, 0.004151113516842898886 ),
 .UNSPECIFIED. ) ;
#95143 = CARTESIAN_POINT ( 'NONE',  ( 20.27804331926714809, 58.17879771734714467, 59.99999999999999289 ) ) ;
#95146 = CARTESIAN_POINT ( 'NONE',  ( 207.9138579432917879, 270.5296297749978294, 5.245628703246491220 ) ) ;
#95147 = CARTESIAN_POINT ( 'NONE',  ( 175.7622132985686392, 274.0430017844784629, -17.75579533532145504 ) ) ;
#95148 = CARTESIAN_POINT ( 'NONE',  ( 190.0370014622527322, 286.8089957100377205, 16.96978714573610247 ) ) ;
#95149 = CARTESIAN_POINT ( 'NONE',  ( 79.28496812781699532, 45.69181762706666916, -12.92980226288132251 ) ) ;
#95150 = CARTESIAN_POINT ( 'NONE',  ( 73.36774340952439388, 69.90371635966560859, 9.665654898056800448 ) ) ;
#95151 = CARTESIAN_POINT ( 'NONE',  ( 49.16021902710897251, 193.0643266524159856, -9.188101187500093303 ) ) ;
#95152 = COLOUR_RGB ( '',0.7921568627450980005, 0.8196078431372548767, 0.9333333333333333481 ) ;
#95153 = CARTESIAN_POINT ( 'NONE',  ( 75.47830877820287299, 53.32463629016104534, 16.49710431891617901 ) ) ;
#95154 = CARTESIAN_POINT ( 'NONE',  ( 70.10703493326258240, 211.2833772461660544, -9.188101187500095079 ) ) ;
#95155 = CARTESIAN_POINT ( 'NONE',  ( 161.8807657183444064, 250.2612843381103573, -13.52770735624900311 ) ) ;
#95157 = ADVANCED_FACE ( 'NONE', ( #51803 ), #79921, .F. ) ;
#95156 = FACE_OUTER_BOUND ( 'NONE', #55641, .T. ) ;
#95158 = CARTESIAN_POINT ( 'NONE',  ( 13.25914332478948410, 9.783808731787853930, -6.180339887498949025 ) ) ;
#95160 = CARTESIAN_POINT ( 'NONE',  ( 152.2331915504236690, 266.9713729667379880, 15.44938373281010158 ) ) ;
#95159 = CARTESIAN_POINT ( 'NONE',  ( 192.9064638172013417, 270.9369261147751331, 14.92505667092759758 ) ) ;
#95161 = CARTESIAN_POINT ( 'NONE',  ( -59.82327302696293003, 35.73826312759338464, 177.5919119679930134 ) ) ;
#95162 = CARTESIAN_POINT ( 'NONE',  ( 22.33066906249845118, 34.93396525600390845, 2.839279412974139660 ) ) ;
#95163 = DIRECTION ( 'NONE',  ( 1.000000000000000000, 1.135996059125383208E-13, 0.000000000000000000 ) ) ;
#95164 = CARTESIAN_POINT ( 'NONE',  ( 196.2293283710122012, 290.7678286567270902, -17.07152402978540096 ) ) ;
#95165 = ORIENTED_EDGE ( 'NONE', *, *, #21270, .F. ) ;
#95166 = CARTESIAN_POINT ( 'NONE',  ( 15.60392711327956761, 29.98502408145592213, -5.678558825948271327 ) ) ;
#95167 = CARTESIAN_POINT ( 'NONE',  ( 73.95019621043851998, 207.3768266524160140, 9.188101187500096856 ) ) ;
#95168 = CARTESIAN_POINT ( 'NONE',  ( 76.62156306105930526, 63.43458379359962152, 15.37592086074862685 ) ) ;
#95169 = CARTESIAN_POINT ( 'NONE',  ( 169.4535728852475813, 288.8904079931804745, -1.135962625816850480 ) ) ;
#95170 = CARTESIAN_POINT ( 'NONE',  ( 110.0000000000000142, 20.00000000000000000, 1.387778780781445676E-14 ) ) ;
#95171 = CARTESIAN_POINT ( 'NONE',  ( 153.6692166914362474, 264.4841044615581040, 18.11141839824787070 ) ) ;
#95172 = EDGE_CURVE ( 'NONE', #30881, #22269, #24011, .T. ) ;
#95173 = EDGE_CURVE ( 'NONE', #89471, #94179, #53948, .T. ) ;
#95174 = DIRECTION ( 'NONE',  ( -0.5372068985985076761, -0.8434505012732950169, 0.000000000000000000 ) ) ;
#95175 = CARTESIAN_POINT ( 'NONE',  ( 124.7297830591487724, 249.4865022471903160, 10.00000000000009237 ) ) ;
#95176 = CARTESIAN_POINT ( 'NONE',  ( 14.74455677852503932, 185.9865022471903160, -10.00000000000009592 ) ) ;
#95177 = CARTESIAN_POINT ( 'NONE',  ( 74.83378613555646552, 53.36200798387709909, 16.53431728583301208 ) ) ;
#95178 = ORIENTED_EDGE ( 'NONE', *, *, #84316, .F. ) ;
#95179 = CARTESIAN_POINT ( 'NONE',  ( 185.0482011028098270, 271.4938003020888004, 15.97631097496702424 ) ) ;
#95180 = EDGE_LOOP ( 'NONE', ( #57562, #16943 ) ) ;
#95181 = CARTESIAN_POINT ( 'NONE',  ( 163.2835940097493790, 247.8315144631017404, 11.08416305054517359 ) ) ;
#95182 = DIRECTION ( 'NONE',  ( -0.000000000000000000, -0.000000000000000000, 1.000000000000000000 ) ) ;
#95183 = DIRECTION ( 'NONE',  ( -0.8660254037844384856, -0.5000000000000002220, -3.252519625699449945E-16 ) ) ;
#95184 = ORIENTED_EDGE ( 'NONE', *, *, #87124, .F. ) ;
#95185 = CARTESIAN_POINT ( 'NONE',  ( 173.2975034251014392, 251.6701835053000593, -0.1618941120760299945 ) ) ;
#95186 = ORIENTED_EDGE ( 'NONE', *, *, #16900, .F. ) ;
#95187 = CARTESIAN_POINT ( 'NONE',  ( -19.42194755839791753, 24.31068691715150010, -10.00000000000000000 ) ) ;
#95188 = CARTESIAN_POINT ( 'NONE',  ( 45.83126033165607538, 197.2677522451418781, 10.00000000000009592 ) ) ;
#95189 = CARTESIAN_POINT ( 'NONE',  ( 81.29539683296886210, 43.25976067974499273, 9.624898955577574355 ) ) ;
#95190 = AXIS2_PLACEMENT_3D ( 'NONE', #79176, #2648, #9755 ) ;
#95191 = EDGE_LOOP ( 'NONE', ( #96709, #19438, #34187, #13212 ) ) ;
#95192 = CARTESIAN_POINT ( 'NONE',  ( 38.19650550196953986, 40.79103043416552765, 8.090169943749478065 ) ) ;
#95193 = AXIS2_PLACEMENT_3D ( 'NONE', #62882, #32500, #86752 ) ;
#95194 = CARTESIAN_POINT ( 'NONE',  ( 38.91320803870388545, 23.26216523072497466, -2.296566073217252530E-15 ) ) ;
#95195 = CARTESIAN_POINT ( 'NONE',  ( 84.78734842081532008, 50.40784050611168965, -13.89907628984690113 ) ) ;
#95196 = CARTESIAN_POINT ( 'NONE',  ( 85.21227539605295931, 47.84198382932485316, -11.42607603513809877 ) ) ;
#95197 = PLANE ( 'NONE',  #62746 ) ;
#95198 = CARTESIAN_POINT ( 'NONE',  ( 48.59171630976688760, 198.8615022471902591, -10.00000000000009592 ) ) ;
#95199 = ORIENTED_EDGE ( 'NONE', *, *, #90683, .T. ) ;
#95200 = ORIENTED_EDGE ( 'NONE', *, *, #8741, .T. ) ;
#95201 = CARTESIAN_POINT ( 'NONE',  ( -13.90296923609177959, 23.04100004375993649, 10.00000000000000000 ) ) ;
#95202 = AXIS2_PLACEMENT_3D ( 'NONE', #95420, #94892, #62952 ) ;
#95203 =( BOUNDED_CURVE ( )  B_SPLINE_CURVE ( 2, ( #3162, #26933, #34048, #65424, #64937, #50221, #43611, #80680, #11255 ),
 .UNSPECIFIED., .F., .T. ) 
 B_SPLINE_CURVE_WITH_KNOTS ( ( 3, 2, 2, 2, 3 ),
 ( 0.2298387096774193450, 0.2311827956989247201, 0.2338709677419354704, 0.2365591397849462485, 0.2379032258064516236 ),
 .UNSPECIFIED. ) 
 CURVE ( )  GEOMETRIC_REPRESENTATION_ITEM ( )  RATIONAL_B_SPLINE_CURVE ( ( 0.9330127018922194093, 0.9330127018922194093, 1.000000000000000000, 0.8660254037844387076, 1.000000000000000000, 0.8660254037844387076, 1.000000000000000000, 0.9330127018922194093, 0.9330127018922194093 ) ) 
 REPRESENTATION_ITEM ( '' )  );
#95204 = ADVANCED_FACE ( 'NONE', ( #48177 ), #36259, .F. ) ;
#95206 = CARTESIAN_POINT ( 'NONE',  ( 178.8794786194264930, 266.0179056750089899, -16.39995361575137167 ) ) ;
#95205 = CARTESIAN_POINT ( 'NONE',  ( 204.8284483594339065, 275.8737159363993214, 14.69997973035875383 ) ) ;
#95207 = DIRECTION ( 'NONE',  ( -1.000000000000000000, 0.000000000000000000, 0.000000000000000000 ) ) ;
#95208 = CARTESIAN_POINT ( 'NONE',  ( 154.8556227199321427, 262.4291889417971788, 17.77326384500479861 ) ) ;
#95209 = CARTESIAN_POINT ( 'NONE',  ( 71.30420826232683851, 72.17422640967487268, -1.921222099538757666 ) ) ;
#95210 = CARTESIAN_POINT ( 'NONE',  ( -19.51758400505583069, 93.02331244766838836, 59.99999999999999289 ) ) ;
#95211 = CARTESIAN_POINT ( 'NONE',  ( 164.0022889252203129, 246.5866983543648701, 5.359592124775450550 ) ) ;
#95212 = CARTESIAN_POINT ( 'NONE',  ( 38.65784837781280459, 56.65029301956751340, 10.00000000000000000 ) ) ;
#95213 = AXIS2_PLACEMENT_3D ( 'NONE', #6728, #84759, #22421 ) ;
#95214 = CARTESIAN_POINT ( 'NONE',  ( -19.65312891409030271, 93.06504152958497400, -10.00000000000000000 ) ) ;
#95215 = EDGE_CURVE ( 'NONE', #20667, #83357, #40998, .T. ) ;
#95216 = CARTESIAN_POINT ( 'NONE',  ( 79.66011734693590540, 225.9869531367911293, 4.594050593750046652 ) ) ;
#95217 = ORIENTED_EDGE ( 'NONE', *, *, #83049, .F. ) ;
#95218 = CARTESIAN_POINT ( 'NONE',  ( 150.2600589618944582, 271.4479585178293632, 12.50551682633786221 ) ) ;
#95219 = CARTESIAN_POINT ( 'NONE',  ( 48.23560136428437772, 110.1272893647940379, -10.00000000000000000 ) ) ;
#95220 = VERTEX_POINT ( 'NONE', #34962 ) ;
#95221 = B_SPLINE_CURVE_WITH_KNOTS ( 'NONE', 3,
 ( #18486, #49371, #18994, #10884, #41759, #72704, #65070, #49867, #80830, #76181, #21459, #99470, #52845, #36644, #38122, #74690, #68544, #89900, #91387, #84296, #29557, #28550, #75180, #83794, #59433, #14844, #98972, #37150, #60430, #90412, #12889, #90910, #30045, #5752, #97490, #36147, #6756, #67550, #37633, #60934, #98482, #44242, #52346, #82807, #13855, #14358, #51352, #45244 ),
 .UNSPECIFIED., .F., .F.,
 ( 4, 2, 2, 2, 2, 2, 2, 2, 2, 2, 2, 2, 2, 2, 2, 2, 2, 2, 2, 2, 2, 2, 2, 4 ),
 ( 0.002005250820186432748, 0.002448144949604836359, 0.002669592014314038381, 0.002891039079023239970, 0.003001762611377881314, 0.003112486143732522657, 0.003223209676087163134, 0.003333933208441804477, 0.003555380273151086297, 0.003776827337860368984, 0.004662615596697672338, 0.005548403855534974824, 0.006434192114372278178, 0.006877086243790892992, 0.007319980373209508673, 0.007430703905564181241, 0.007486065671741557424, 0.007541427437918933607, 0.007652150970273684238, 0.007762874502628435737, 0.008205768632047496375, 0.008427215696757027127, 0.008648662761466557880, 0.009091556890885619385 ),
 .UNSPECIFIED. ) ;
#95222 = CARTESIAN_POINT ( 'NONE',  ( 168.3457246661429565, 267.1986757268145993, -17.36865887974328615 ) ) ;
#95223 = ORIENTED_EDGE ( 'NONE', *, *, #24576, .F. ) ;
#95224 = CARTESIAN_POINT ( 'NONE',  ( 80.20857768024397672, 44.93227668248793094, -11.26798599081711139 ) ) ;
#95225 = EDGE_CURVE ( 'NONE', #91333, #50922, #52529, .T. ) ;
#95226 = CARTESIAN_POINT ( 'NONE',  ( 156.6812872898450735, 261.2670451491295012, 0.000000000000000000 ) ) ;
#95227 = FACE_OUTER_BOUND ( 'NONE', #89961, .T. ) ;
#95228 = FACE_OUTER_BOUND ( 'NONE', #21163, .T. ) ;
#95229 = CARTESIAN_POINT ( 'NONE',  ( 80.48961952429826283, 48.34260169403606255, -13.60942759726339268 ) ) ;
#95230 = DIRECTION ( 'NONE',  ( -0.001368469433204011270, 0.9999990636452668058, 0.000000000000000000 ) ) ;
#95231 = ORIENTED_EDGE ( 'NONE', *, *, #86416, .T. ) ;
#95232 = VECTOR ( 'NONE', #86232, 1000.000000000000000 ) ;
#95233 = VERTEX_POINT ( 'NONE', #83479 ) ;
#95234 = CARTESIAN_POINT ( 'NONE',  ( 162.8480293090835005, 248.5859346546387769, -9.753154585358942086 ) ) ;
#95235 = ORIENTED_EDGE ( 'NONE', *, *, #64637, .F. ) ;
#95236 = CARTESIAN_POINT ( 'NONE',  ( 27.18159744850307291, 27.64441083166262203, -10.00000000000000533 ) ) ;
#95237 = LINE ( 'NONE', #19705, #20893 ) ;
#95238 = FACE_OUTER_BOUND ( 'NONE', #31497, .T. ) ;
#95239 = CARTESIAN_POINT ( 'NONE',  ( -0.4289299871626708338, 163.8927522451418213, 10.00000000000009592 ) ) ;
#95241 = B_SPLINE_CURVE_WITH_KNOTS ( 'NONE', 3,
 ( #17206, #71932, #64825, #48112, #59056, #2536, #82451, #33418, #26326, #20602, #71433, #90027, #25837, #55686, #79053, #18726, #74816, #36279, #9642, #56712, #87695, #49123, #13014, #32908, #3538, #63815, #43873, #88179, #5395, #94255, #40501, #49610, #2023, #90540, #5886, #52473, #75305, #98102, #14488, #75805, #21590, #45367, #67178, #92031, #14962, #67683, #36775, #22079, #37276, #6873, #83420, #22577 ),
 .UNSPECIFIED., .F., .F.,
 ( 4, 2, 2, 2, 2, 2, 2, 2, 2, 2, 2, 2, 2, 2, 2, 2, 2, 2, 2, 2, 2, 2, 2, 2, 2, 4 ),
 ( 0.0006380557224042569678, 0.001138346313157871745, 0.001638636903911486632, 0.001888782199288259380, 0.002138927494665032129, 0.002264000142353447126, 0.002389072790041862123, 0.002514145437730277120, 0.002639218085418692118, 0.002889363380795566781, 0.003139508676172441011, 0.003639799266926106204, 0.004640380448433350721, 0.005640961629940595239, 0.006141252220694258697, 0.006391397516071126855, 0.006641542811447994146, 0.006704079135292192321, 0.006766615459136391363, 0.006829151782980589537, 0.006891688106824788579, 0.007141833402201395661, 0.007642123992954569928, 0.008142414583707744194, 0.008392559879084330460, 0.008642705174460914991 ),
 .UNSPECIFIED. ) ;
#95240 = CARTESIAN_POINT ( 'NONE',  ( 87.84239280846571774, 44.77947472371889148, 4.964184461739159282 ) ) ;
#95242 = ORIENTED_EDGE ( 'NONE', *, *, #88222, .T. ) ;
#95243 = FACE_OUTER_BOUND ( 'NONE', #64793, .T. ) ;
#95244 = CARTESIAN_POINT ( 'NONE',  ( 81.14562047329557970, 46.93173235953988609, 12.45778470005855354 ) ) ;
#95245 = CARTESIAN_POINT ( 'NONE',  ( -22.42236680055709641, 157.8615022471902591, 0.000000000000000000 ) ) ;
#95246 = CARTESIAN_POINT ( 'NONE',  ( 192.2047958520457200, 271.8935057982316721, 14.16859286990318978 ) ) ;
#95247 = CARTESIAN_POINT ( 'NONE',  ( 71.49943747925016169, 59.40683841810739807, -15.72255559731668129 ) ) ;
#95248 = DIRECTION ( 'NONE',  ( -0.000000000000000000, -0.000000000000000000, -1.000000000000000000 ) ) ;
#95250 = EDGE_CURVE ( 'NONE', #3137, #51575, #60131, .T. ) ;
#95249 = B_SPLINE_CURVE_WITH_KNOTS ( 'NONE', 3,
 ( #70248, #40833, #854, #48464, #7970, #71779, #8957, #2378, #85509, #47940, #94099, #64157, #71277, #31733, #93591, #16552, #47447, #78376, #24650, #78882, #56032, #1867, #9467, #40338, #32751, #63655, #87026, #94594, #25148, #17558, #79406, #95108, #56553, #15536, #46436, #77365, #69749, #360, #31247, #62134, #28021, #36109, #64669, #83249, #88025, #43711, #28513, #98938, #59395, #35625, #58896, #90372 ),
 .UNSPECIFIED., .F., .F.,
 ( 4, 2, 2, 2, 2, 2, 2, 2, 2, 2, 2, 2, 2, 2, 2, 2, 2, 2, 2, 2, 2, 2, 2, 2, 2, 4 ),
 ( 0.0007684721497847792765, 0.001259722117377088746, 0.001750972084969398216, 0.001996597068765640012, 0.002242222052561882242, 0.002365034544460022006, 0.002487847036358162203, 0.002610659528256302833, 0.002733472020154442596, 0.002979097003950728628, 0.003224721987747015094, 0.003715971955339622285, 0.004698471890524970676, 0.005680971825710319500, 0.006172221793303030342, 0.006417846777099385329, 0.006663471760895741183, 0.006724878006844846844, 0.006786284252793953371, 0.006847690498743059032, 0.006909096744692165559, 0.007154721728488628099, 0.007645971696081424809, 0.008137221663674221520, 0.008382846647470635487, 0.008628471631267047720 ),
 .UNSPECIFIED. ) ;
#95251 = DIRECTION ( 'NONE',  ( 0.000000000000000000, 0.000000000000000000, 1.000000000000000000 ) ) ;
#95252 = ORIENTED_EDGE ( 'NONE', *, *, #46324, .T. ) ;
#95253 = CARTESIAN_POINT ( 'NONE',  ( 149.0417755939924405, 274.5147917236959643, 9.103005964151618556 ) ) ;
#95254 = CARTESIAN_POINT ( 'NONE',  ( 161.4025183475459073, 251.0896330829197041, 14.50747140106038735 ) ) ;
#95255 = CARTESIAN_POINT ( 'NONE',  ( 86.12973485563841791, 45.34942800271429775, 7.988429100487741685 ) ) ;
#95256 = AXIS2_PLACEMENT_3D ( 'NONE', #77522, #69892, #99324 ) ;
#95257 = CARTESIAN_POINT ( 'NONE',  ( 22.49950015666239622, 18.15404122711133539, 8.090169943749479842 ) ) ;
#95259 = CARTESIAN_POINT ( 'NONE',  ( 78.44787846840736734, 61.26446607870955319, 16.23792605971963354 ) ) ;
#95258 = B_SPLINE_CURVE_WITH_KNOTS ( 'NONE', 3,
 ( #35666, #90914, #46227, #31044, #21463, #68054, #38646, #21955, #84300, #75673, #52351, #60435, #14848, #99974, #92395, #60941, #45734, #30559 ),
 .UNSPECIFIED., .F., .F.,
 ( 4, 2, 2, 2, 2, 2, 2, 2, 4 ),
 ( 0.001647475917812264148, 0.002184538663664093924, 0.002721601409515923917, 0.003258664155367753910, 0.003795726901219583470, 0.004332789647071413029, 0.004869852392923247793, 0.005406915138775082556, 0.005943977884626917320 ),
 .UNSPECIFIED. ) ;
#95260 = CARTESIAN_POINT ( 'NONE',  ( 174.8794285395499344, 290.4103569552396493, -6.460613355744903252 ) ) ;
#95261 = EDGE_CURVE ( 'NONE', #29839, #99059, #32337, .T. ) ;
#95262 = CYLINDRICAL_SURFACE ( 'NONE', #18751, 17.82106496071139645 ) ;
#95263 = VERTEX_POINT ( 'NONE', #59439 ) ;
#95264 = AXIS2_PLACEMENT_3D ( 'NONE', #93793, #46639, #33451 ) ;
#95265 = B_SPLINE_CURVE_WITH_KNOTS ( 'NONE', 3,
 ( #43706, #13333, #5712, #97931, #12334, #28506, #58890, #66518, #98933, #60389, #44691, #97443, #74648, #73632, #89384, #35113, #96973, #19938, #89859, #67505, #20434, #91344, #51300, #44198, #66024, #75135, #21904, #74143, #82273, #98438, #52793, #82767, #75620, #5224, #29028, #59900, #36103, #27540, #90868, #90364, #58409, #21419, #59387, #52305, #13810, #50810 ),
 .UNSPECIFIED., .F., .F.,
 ( 4, 1, 2, 2, 1, 2, 2, 1, 1, 2, 2, 1, 1, 2, 2, 1, 1, 2, 2, 1, 1, 1, 2, 2, 1, 1, 1, 2, 2, 4 ),
 ( 0.000000000000000000, 0.06250000000000124900, 0.09375000000000187350, 0.1250000000000024980, 0.1875000000000036360, 0.2187500000000061340, 0.2500000000000086042, 0.3125000000000096589, 0.3437500000000101585, 0.3593750000000088263, 0.3750000000000075495, 0.4375000000000063283, 0.4687500000000042188, 0.4843750000000027756, 0.5000000000000013323, 0.5625000000000027756, 0.5937500000000034417, 0.6093750000000038858, 0.6250000000000042188, 0.6875000000000037748, 0.7187500000000018874, 0.7343750000000011102, 0.7421875000000006661, 0.7500000000000001110, 0.8124999999999923395, 0.8437499999999882316, 0.8593749999999862332, 0.8671874999999853451, 0.8749999999999844569, 1.000000000000000000 ),
 .UNSPECIFIED. ) ;
#95266 = AXIS2_PLACEMENT_3D ( 'NONE', #3372, #34734, #80903 ) ;
#95267 = AXIS2_PLACEMENT_3D ( 'NONE', #34338, #87617, #18146 ) ;
#95268 = CARTESIAN_POINT ( 'NONE',  ( 164.2953672501826929, 246.0790718049323687, -2.576662677987826111 ) ) ;
#95270 = CARTESIAN_POINT ( 'NONE',  ( 194.6056312668138162, 268.3159250634341788, -12.34445183914189670 ) ) ;
#95269 = CARTESIAN_POINT ( 'NONE',  ( 178.5610891250362045, 265.5608437732782363, -14.90458899103854051 ) ) ;
#95271 = CARTESIAN_POINT ( 'NONE',  ( 49.10122569834316408, 93.29622288527660601, -10.00000000000000000 ) ) ;
#95272 = CARTESIAN_POINT ( 'NONE',  ( 22.77272502854106762, 36.08080186712593473, -3.090169943749475845 ) ) ;
#95273 = CARTESIAN_POINT ( 'NONE',  ( 77.93060254874920645, 48.03996307830335155, 14.17289077042660139 ) ) ;
#95274 = CARTESIAN_POINT ( 'NONE',  ( 171.6149855087873561, 274.5829882844238341, 16.21406585132328004 ) ) ;
#95275 = DIRECTION ( 'NONE',  ( -0.6141984594095433181, -0.7891516029629184192, 0.000000000000000000 ) ) ;
#95276 = CARTESIAN_POINT ( 'NONE',  ( -19.65312891409030271, 93.06504152958497400, 177.5919119679930134 ) ) ;
#95277 = CARTESIAN_POINT ( 'NONE',  ( 82.89640184790823696, 43.22043319592323485, -7.394312023068621009 ) ) ;
#95278 = CARTESIAN_POINT ( 'NONE',  ( 207.8984236726843164, 270.5563627158673512, -6.084369154771423815 ) ) ;
#95279 = AXIS2_PLACEMENT_3D ( 'NONE', #14508, #39271, #92535 ) ;
#95280 = CARTESIAN_POINT ( 'NONE',  ( 6.454167755106333892, 174.5333772461660828, 9.188101187500095079 ) ) ;
#95281 = CARTESIAN_POINT ( 'NONE',  ( 81.93937120068478919, 47.03835499581510504, 12.23552757480724118 ) ) ;
#95282 = ORIENTED_EDGE ( 'NONE', *, *, #99360, .F. ) ;
#95283 = CARTESIAN_POINT ( 'NONE',  ( 87.32537421964468649, 46.00455475262659633, 8.658505635391252397 ) ) ;
#95284 = DIRECTION ( 'NONE',  ( -1.000000000000000000, 0.000000000000000000, 0.000000000000000000 ) ) ;
#95285 = CARTESIAN_POINT ( 'NONE',  ( 164.4578252119609090, 245.7976863610386999, -6.211333091911165560 ) ) ;
#95286 = CARTESIAN_POINT ( 'NONE',  ( 81.69623217530381964, 41.61371471569898262, 5.513057524364318063 ) ) ;
#95287 = CARTESIAN_POINT ( 'NONE',  ( 29.86365662933068066, 197.2369531367911293, -4.594050593750048428 ) ) ;
#95288 = AXIS2_PLACEMENT_3D ( 'NONE', #44870, #82931, #75309 ) ;
#95289 = CARTESIAN_POINT ( 'NONE',  ( 30.56436172585706146, 22.81029122506296147, 8.090169943749479842 ) ) ;
#95290 = CARTESIAN_POINT ( 'NONE',  ( 43.53485905213462104, 24.94473085651396005, 1.475505719884397138E-15 ) ) ;
#95291 = CARTESIAN_POINT ( 'NONE',  ( 181.7688266870327709, 294.4230621335508999, 6.401746037419756341 ) ) ;
#95292 = B_SPLINE_CURVE_WITH_KNOTS ( 'NONE', 3,
 ( #56134, #95206, #34837, #80502 ),
 .UNSPECIFIED., .F., .F.,
 ( 4, 4 ),
 ( 0.008997718677290020978, 0.01512492955424769338 ),
 .UNSPECIFIED. ) ;
#95293 = CARTESIAN_POINT ( 'NONE',  ( 191.0862225170008628, 299.6759493045793192, -9.402218231374108726 ) ) ;
#95294 = CARTESIAN_POINT ( 'NONE',  ( 149.2197514927185580, 272.1908042522468349, 11.55035869369450197 ) ) ;
#95295 = CARTESIAN_POINT ( 'NONE',  ( 181.7535138776731003, 279.7363418824564860, -16.10976311149228479 ) ) ;
#95296 = CARTESIAN_POINT ( 'NONE',  ( -62.95439910331221256, 68.06504152958493137, -45.00000000000001421 ) ) ;
#95297 = B_SPLINE_SURFACE_WITH_KNOTS ( 'NONE', 3, 1, ( 
 ( #49331, #80270 ),
 ( #19458, #26537 ),
 ( #11839, #6711 ),
 ( #6207, #44195 ),
 ( #67503, #68499 ),
 ( #52302, #36101 ),
 ( #14311, #13808 ),
 ( #45683, #59898 ),
 ( #37589, #84743 ),
 ( #29026, #90865 ),
 ( #99423, #60883 ),
 ( #67004, #90361 ),
 ( #21417, #36599 ),
 ( #30000, #91845 ),
 ( #68007, #13331 ),
 ( #15284, #82765 ),
 ( #38080, #45197 ),
 ( #74646, #22895 ),
 ( #22407, #75133 ),
 ( #76609, #53300 ),
 ( #83241, #53780 ),
 ( #7195, #30504 ),
 ( #84253, #68993 ),
 ( #14801, #99919 ),
 ( #5710, #98435 ),
 ( #61394, #92346 ),
 ( #44689, #75619 ),
 ( #37102, #5222 ),
 ( #97929, #98931 ),
 ( #28504, #59385 ),
 ( #76137, #20942 ),
 ( #51823, #29509 ),
 ( #60387, #91342 ),
 ( #21903, #52791 ) ),
 .UNSPECIFIED., .T., .F., .F.,
 ( 4, 2, 2, 2, 2, 2, 2, 2, 2, 2, 2, 2, 2, 2, 2, 2, 4 ),
 ( 2, 2 ),
 ( 0.000000000000000000, 0.06250000000000000000, 0.1250000000000000000, 0.1875000000000000000, 0.2500000000000000000, 0.3125000000000000000, 0.3750000000000000000, 0.4375000000000000000, 0.5000000000000000000, 0.5625000000000000000, 0.6250000000000000000, 0.6875000000000000000, 0.7500000000000000000, 0.8125000000000000000, 0.8750000000000000000, 0.9375000000000000000, 1.000000000000000000 ),
 ( 0.000000000000000000, 1.000000000000000000 ),
 .UNSPECIFIED. ) ;
#95298 = CARTESIAN_POINT ( 'NONE',  ( 190.1042286455896999, 298.6140004201554348, -8.058983885598134833 ) ) ;
#95299 = CARTESIAN_POINT ( 'NONE',  ( 92.02936583101279666, 212.3932355074535678, -2.679491924311248496 ) ) ;
#95300 = EDGE_CURVE ( 'NONE', #10592, #93322, #14217, .T. ) ;
#95301 = EDGE_CURVE ( 'NONE', #14010, #33732, #45845, .T. ) ;
#95302 = CARTESIAN_POINT ( 'NONE',  ( 84.89261448506465513, 206.4865022471901455, 1.119607411625061291E-15 ) ) ;
#95303 = CARTESIAN_POINT ( 'NONE',  ( 165.5845016731641124, 245.8462254865437160, 0.7221155814038995313 ) ) ;
#95304 = CARTESIAN_POINT ( 'NONE',  ( 161.9385560670746145, 267.8585340882163450, -16.83787897924083055 ) ) ;
#95305 = EDGE_CURVE ( 'NONE', #98479, #93808, #97683, .T. ) ;
#95306 = CARTESIAN_POINT ( 'NONE',  ( 42.77328167419873495, 189.3768266524160140, 9.188101187500098632 ) ) ;
#95307 = CARTESIAN_POINT ( 'NONE',  ( 159.4285914931787431, 254.5085746851079023, 15.41072477910873673 ) ) ;
#95308 = ADVANCED_FACE ( 'NONE', ( #82327 ), #58873, .T. ) ;
#95309 = ORIENTED_EDGE ( 'NONE', *, *, #69508, .F. ) ;
#95310 = CARTESIAN_POINT ( 'NONE',  ( -5.928083997560643859, 82.72996031218040969, 13.41116729756204329 ) ) ;
#95311 = DIRECTION ( 'NONE',  ( -0.5000000000000003331, 0.8660254037844385966, 1.011061903669573814E-15 ) ) ;
#95312 = VERTEX_POINT ( 'NONE', #91393 ) ;
#95313 = CARTESIAN_POINT ( 'NONE',  ( 167.5137480047340830, 285.0270040894174031, 7.743640753283266953 ) ) ;
#95314 = CARTESIAN_POINT ( 'NONE',  ( 168.0608149624495979, 281.9755942893786482, -10.94157658500136598 ) ) ;
#95315 = DIRECTION ( 'NONE',  ( -0.4145187862775162602, 0.7179675985244458047, -0.5591929034707565638 ) ) ;
#95316 = CARTESIAN_POINT ( 'NONE',  ( 87.40047971330908183, 231.2677522451419065, -5.000000000000047962 ) ) ;
#95317 = CARTESIAN_POINT ( 'NONE',  ( 30.25295400085950703, 18.26216523072495690, -2.296566073217252530E-15 ) ) ;
#95318 = CARTESIAN_POINT ( 'NONE',  ( 163.4216610345155800, 247.5923753613567442, 10.58669027323842826 ) ) ;
#95319 = CARTESIAN_POINT ( 'NONE',  ( 110.3501529135968013, 224.5177522451418213, 5.000000000000051514 ) ) ;
#95320 = CARTESIAN_POINT ( 'NONE',  ( 157.0858749576330524, 258.5662787524049122, 18.43576942457294976 ) ) ;
#95321 = VERTEX_POINT ( 'NONE', #69553 ) ;
#95322 = CARTESIAN_POINT ( 'NONE',  ( 7.821713311501573784, 19.91421378149916421, 9.188101187500008038 ) ) ;
#95323 = CARTESIAN_POINT ( 'NONE',  ( 24.36335893204212155, 173.3262482093457777, 3.021315404115420679E-15 ) ) ;
#95324 = DIRECTION ( 'NONE',  ( -0.000000000000000000, -1.000000000000000000, -0.000000000000000000 ) ) ;
#95326 = ORIENTED_EDGE ( 'NONE', *, *, #61740, .T. ) ;
#95325 = B_SPLINE_CURVE_WITH_KNOTS ( 'NONE', 3,
 ( #80347, #40277, #72223, #79351, #65097, #18018, #41281, #79845, #48910, #3326, #65593, #57482, #88466, #96050, #19027, #41790 ),
 .UNSPECIFIED., .F., .F.,
 ( 4, 1, 2, 2, 2, 1, 2, 2, 4 ),
 ( 0.000000000000000000, 0.1250000000000003608, 0.1874999999999987232, 0.2499999999999971134, 0.4999999999999960587, 0.6249999999999973355, 0.6874999999999978906, 0.7499999999999983347, 1.000000000000000000 ),
 .UNSPECIFIED. ) ;
#95327 = CARTESIAN_POINT ( 'NONE',  ( 72.38706308606541029, 71.16596677985461383, -6.083085609279689443 ) ) ;
#95328 = CARTESIAN_POINT ( 'NONE',  ( 85.53100213312241351, 49.04015438577492603, 12.29448614360842207 ) ) ;
#95329 = DIRECTION ( 'NONE',  ( 0.5000000000000013323, -0.8660254037844378194, 0.000000000000000000 ) ) ;
#95330 = DIRECTION ( 'NONE',  ( -0.8660254037844378194, -0.5000000000000014433, -0.000000000000000000 ) ) ;
#95331 = ORIENTED_EDGE ( 'NONE', *, *, #16721, .F. ) ;
#95332 = ORIENTED_EDGE ( 'NONE', *, *, #47887, .T. ) ;
#95333 = EDGE_CURVE ( 'NONE', #41802, #94756, #61395, .T. ) ;
#95335 = DIRECTION ( 'NONE',  ( -0.9997524133706772176, 0.02225111142182466945, 0.000000000000000000 ) ) ;
#95334 = CARTESIAN_POINT ( 'NONE',  ( -19.68616313074564417, 93.20296353353185737, 59.99999999999999289 ) ) ;
#95336 = CARTESIAN_POINT ( 'NONE',  ( 196.9976074755333286, 289.4371302133026802, -16.79549473444794216 ) ) ;
#95337 = ORIENTED_EDGE ( 'NONE', *, *, #93688, .T. ) ;
#95338 = CARTESIAN_POINT ( 'NONE',  ( 152.6740002182599767, 266.2078699576288159, -17.16212636348624088 ) ) ;
#95339 = AXIS2_PLACEMENT_3D ( 'NONE', #26930, #18839, #80675 ) ;
#95340 = CARTESIAN_POINT ( 'NONE',  ( 193.5005633302724277, 262.8551920378705518, -5.236817587991198231 ) ) ;
#95341 = CARTESIAN_POINT ( 'NONE',  ( 72.92456211408232036, 57.41452964202046161, -15.86517170058079529 ) ) ;
#95342 = CARTESIAN_POINT ( 'NONE',  ( 78.06822720212770150, 61.43946511097403373, -16.16087495820213960 ) ) ;
#95343 = CARTESIAN_POINT ( 'NONE',  ( 204.8057697639265768, 275.9129964160624695, -12.68356524114230766 ) ) ;
#95344 = CARTESIAN_POINT ( 'NONE',  ( 113.7598676209481994, 245.6744531367911293, 4.594050593750047540 ) ) ;
#95345 = AXIS2_PLACEMENT_3D ( 'NONE', #5310, #13419, #51909 ) ;
#95346 = AXIS2_PLACEMENT_3D ( 'NONE', #63794, #42963, #33919 ) ;
#95347 = CARTESIAN_POINT ( 'NONE',  ( 180.9150213778623879, 287.7115838886965093, -14.09538787175014996 ) ) ;
#95348 = ORIENTED_EDGE ( 'NONE', *, *, #89022, .F. ) ;
#95349 = AXIS2_PLACEMENT_3D ( 'NONE', #95741, #64796, #26294 ) ;
#95350 = CARTESIAN_POINT ( 'NONE',  ( 201.1403430031335517, 280.2617017971787732, 16.85780947333721613 ) ) ;
#95351 = ORIENTED_EDGE ( 'NONE', *, *, #76521, .F. ) ;
#95352 = CARTESIAN_POINT ( 'NONE',  ( 31.21403501649405854, 38.99752408145594273, 5.678558825948277544 ) ) ;
#95353 = CARTESIAN_POINT ( 'NONE',  ( 157.1202548728886654, 259.0885287614115668, 16.98198004443705500 ) ) ;
#95354 = CARTESIAN_POINT ( 'NONE',  ( 72.16990512472445118, 70.69651720998999167, -7.560285414252116531 ) ) ;
#95355 = CARTESIAN_POINT ( 'NONE',  ( 54.00411475982191689, 211.1744531367911293, 4.594050593750047540 ) ) ;
#95356 = CARTESIAN_POINT ( 'NONE',  ( 74.07459009150333884, 68.62600853808264389, 10.93350474783683701 ) ) ;
#95357 = CARTESIAN_POINT ( 'NONE',  ( 151.3589047706063582, 268.4856820897672378, 14.56544807350869419 ) ) ;
#95358 = CARTESIAN_POINT ( 'NONE',  ( 95.69988983291004558, 219.3927522451418213, 10.00000000000009948 ) ) ;
#95359 = CARTESIAN_POINT ( 'NONE',  ( 173.1256968621561896, 271.2508009423272028, 16.42367957618433039 ) ) ;
#95360 = ORIENTED_EDGE ( 'NONE', *, *, #79346, .F. ) ;
#95361 = VECTOR ( 'NONE', #16394, 1000.000000000000114 ) ;
#95362 = CARTESIAN_POINT ( 'NONE',  ( 76.86653180887425663, 57.81399073350881679, -16.12744706992745947 ) ) ;
#95363 = CARTESIAN_POINT ( 'NONE',  ( 84.36170811391946245, 42.94765869660285063, -5.099173484137480727 ) ) ;
#95364 = CARTESIAN_POINT ( 'NONE',  ( 177.6299345319881411, 288.9505342943081700, 11.21071512699488792 ) ) ;
#95365 = CARTESIAN_POINT ( 'NONE',  ( 189.8171280724701546, 301.8740853621098950, -0.4360232994423257624 ) ) ;
#95366 = ORIENTED_EDGE ( 'NONE', *, *, #45986, .F. ) ;
#95367 = CARTESIAN_POINT ( 'NONE',  ( 172.5074440713383979, 259.9802927986077066, -13.86797602670016438 ) ) ;
#95368 = CARTESIAN_POINT ( 'NONE',  ( 67.37375070832676727, 69.12700154216180692, -3.154838971303389528 ) ) ;
#95369 = CARTESIAN_POINT ( 'NONE',  ( 207.1211793645798878, 271.9025893473983047, -6.294110402770905388 ) ) ;
#95370 = DIRECTION ( 'NONE',  ( -0.8660254037844378194, -0.5000000000000014433, -0.000000000000000000 ) ) ;
#95371 = CARTESIAN_POINT ( 'NONE',  ( 190.0707697440390689, 301.4347651000360884, 4.271360729158901748 ) ) ;
#95372 = ADVANCED_FACE ( 'NONE', ( #44741 ), #23439, .F. ) ;
#95373 = CARTESIAN_POINT ( 'NONE',  ( 177.5204303635850067, 269.6146312835412004, 16.09809966445594753 ) ) ;
#95374 = CARTESIAN_POINT ( 'NONE',  ( 164.3090168944849836, 246.0554299274959931, 2.641760039552302430 ) ) ;
#95375 = PRESENTATION_STYLE_ASSIGNMENT (( #27899 ) ) ;
#95376 = CARTESIAN_POINT ( 'NONE',  ( 167.0666417749207824, 256.2416655149617100, 13.72858796342581833 ) ) ;
#95377 = DIRECTION ( 'NONE',  ( -0.8660254037844387076, -0.4999999999999998890, -0.000000000000000000 ) ) ;
#95378 = CARTESIAN_POINT ( 'NONE',  ( 136.0064158243085046, 240.1423013555409796, -4.594050593750043987 ) ) ;
#95379 = VERTEX_POINT ( 'NONE', #67556 ) ;
#95380 = CARTESIAN_POINT ( 'NONE',  ( 146.6834825911944620, 276.5837508513432681, 0.6716460511724984261 ) ) ;
#95381 = CARTESIAN_POINT ( 'NONE',  ( 48.53010236944518851, 101.9116055364396090, -10.00000000000000000 ) ) ;
#95382 = LINE ( 'NONE', #25934, #37615 ) ;
#95383 = LINE ( 'NONE', #79666, #3041 ) ;
#95384 = CARTESIAN_POINT ( 'NONE',  ( 74.07698310468663294, 57.69947640214264339, 15.94728086577454285 ) ) ;
#95385 = CARTESIAN_POINT ( 'NONE',  ( 177.9758113737784413, 255.3779581033551267, 4.856556020679135166 ) ) ;
#95386 = ORIENTED_EDGE ( 'NONE', *, *, #21352, .T. ) ;
#95387 = CARTESIAN_POINT ( 'NONE',  ( 80.12177396824181130, 57.42895151072963955, -16.59339316893575145 ) ) ;
#95388 = LINE ( 'NONE', #47704, #86754 ) ;
#95390 = CARTESIAN_POINT ( 'NONE',  ( 181.9635258183570841, 260.5293054935651753, 10.24091241681038689 ) ) ;
#95389 = CARTESIAN_POINT ( 'NONE',  ( 147.6272135932435674, 275.4487879174903355, 2.980883776998032531 ) ) ;
#95391 = CARTESIAN_POINT ( 'NONE',  ( 206.2016707383607184, 271.6730508100820316, 8.149847062769225658 ) ) ;
#95392 = DIRECTION ( 'NONE',  ( 0.7499999999999991118, 0.4330127018922202420, -0.5000000000000004441 ) ) ;
#95393 = CARTESIAN_POINT ( 'NONE',  ( 185.9155157935707905, 296.7526516983074316, 4.644333911091743872 ) ) ;
#95394 = LINE ( 'NONE', #27916, #54686 ) ;
#95395 = CARTESIAN_POINT ( 'NONE',  ( 60.41820218054165537, 211.8149278399160664, 9.188101187500093303 ) ) ;
#95396 = CARTESIAN_POINT ( 'NONE',  ( 85.61005001132002690, 48.37664482377094544, -12.20733655019926189 ) ) ;
#95397 = CARTESIAN_POINT ( 'NONE',  ( 157.4068442735347446, 281.9945091197541274, 2.874377194828706905 ) ) ;
#95398 = CARTESIAN_POINT ( 'NONE',  ( 67.82635223848771489, 69.76632902677688719, -0.4661708874699829752 ) ) ;
#95399 = CARTESIAN_POINT ( 'NONE',  ( 171.1029346131852549, 259.8587293126610120, 14.99369131906140140 ) ) ;
#95400 = DIRECTION ( 'NONE',  ( 0.000000000000000000, 0.000000000000000000, 1.000000000000000000 ) ) ;
#95401 = CARTESIAN_POINT ( 'NONE',  ( -44.74834796241764678, 29.05375577536863929, 10.00000000000000000 ) ) ;
#95402 = CARTESIAN_POINT ( 'NONE',  ( 203.0498946958275326, 278.9542612457532869, -15.11479947333269003 ) ) ;
#95403 = DIRECTION ( 'NONE',  ( 0.9403255362191060840, -0.3402761906661271873, 0.000000000000000000 ) ) ;
#95404 = CARTESIAN_POINT ( 'NONE',  ( 132.7946446283434909, 234.1427522451417644, 1.119607411625061291E-15 ) ) ;
#95405 = CARTESIAN_POINT ( 'NONE',  ( 81.35671934171772079, 51.65773188628860169, -14.92242472238318385 ) ) ;
#95406 = ORIENTED_EDGE ( 'NONE', *, *, #56178, .T. ) ;
#95407 = AXIS2_PLACEMENT_3D ( 'NONE', #70039, #652, #55332 ) ;
#95408 = CARTESIAN_POINT ( 'NONE',  ( 159.7633413689523536, 257.8948702361064989, -17.25380331320266336 ) ) ;
#95409 = CARTESIAN_POINT ( 'NONE',  ( -10.59588092978231266, 170.8149278399160949, -9.188101187500095079 ) ) ;
#95410 = CARTESIAN_POINT ( 'NONE',  ( 42.55642822748761489, 201.5024278399160949, 9.188101187500095079 ) ) ;
#95411 = VECTOR ( 'NONE', #25979, 1000.000000000000000 ) ;
#95412 = CARTESIAN_POINT ( 'NONE',  ( 23.30503800868896391, 15.58380873178786885, 6.180339887498953466 ) ) ;
#95413 = CARTESIAN_POINT ( 'NONE',  ( 32.50353804854218964, 201.1199935810940929, 2.679491924311251605 ) ) ;
#95414 = CARTESIAN_POINT ( 'NONE',  ( 181.2581408264541949, 265.9245715698776280, -15.25451850613310434 ) ) ;
#95415 = CARTESIAN_POINT ( 'NONE',  ( 72.09323793696012217, 72.40190342410335234, -3.152634433464706287 ) ) ;
#95416 = CARTESIAN_POINT ( 'NONE',  ( 147.3023124603499809, 275.5119060767245287, 5.196938859334171212 ) ) ;
#95417 = CARTESIAN_POINT ( 'NONE',  ( 72.22324980102312963, 72.08985755953557373, 3.071982638949906086 ) ) ;
#95419 = CARTESIAN_POINT ( 'NONE',  ( 54.05850166760819775, 212.0177522451419065, 5.000000000000046185 ) ) ;
#95418 = CARTESIAN_POINT ( 'NONE',  ( 205.7627300303947209, 272.2554926137148072, 9.584172220806708609 ) ) ;
#95420 = CARTESIAN_POINT ( 'NONE',  ( -13.76211276271278194, 162.8615022471903444, 5.188172501216621122E-14 ) ) ;
#95421 = CARTESIAN_POINT ( 'NONE',  ( 163.0929729200167912, 256.2987166179328256, -15.18292651160261642 ) ) ;
#95422 = CARTESIAN_POINT ( 'NONE',  ( 157.8820657059571033, 257.1872359237914338, -17.60412210594719440 ) ) ;
#95423 = CARTESIAN_POINT ( 'NONE',  ( 165.5298684834693574, 269.3554679133272884, -17.63324793928101997 ) ) ;
#95424 = EDGE_CURVE ( 'NONE', #56685, #27648, #13862, .T. ) ;
#95425 = EDGE_CURVE ( 'NONE', #2862, #47702, #54328, .T. ) ;
#95426 = VECTOR ( 'NONE', #23728, 1000.000000000000114 ) ;
#95427 = CARTESIAN_POINT ( 'NONE',  ( 44.26158929084472504, 186.3615022471902023, 5.000000000000051514 ) ) ;
#95428 = CARTESIAN_POINT ( 'NONE',  ( 151.2701135660092007, 248.9548013555409796, -4.594050593750042211 ) ) ;
#95429 = DIRECTION ( 'NONE',  ( 0.2774202615135334393, -0.9607486656258038549, 0.000000000000000000 ) ) ;
#95430 = CARTESIAN_POINT ( 'NONE',  ( 3.260525530768699998, 178.8149278399161233, 9.188101187500093303 ) ) ;
#95431 = CARTESIAN_POINT ( 'NONE',  ( 34.56506555475243658, 38.14336893147758900, 7.433330006724141015 ) ) ;
#95433 = CARTESIAN_POINT ( 'NONE',  ( 170.7188017663200981, 263.1837195185569271, 15.88278987561155375 ) ) ;
#95432 = DIRECTION ( 'NONE',  ( -1.000000000000000000, -4.892646582054824097E-14, 0.000000000000000000 ) ) ;
#95434 = EDGE_CURVE ( 'NONE', #74497, #69106, #37157, .T. ) ;
#95435 = CARTESIAN_POINT ( 'NONE',  ( 24.54146915528859907, 191.6427522451419350, 10.00000000000009415 ) ) ;
#95436 = CARTESIAN_POINT ( 'NONE',  ( 28.07469292777547309, 37.18502408145594273, 5.678558825948277544 ) ) ;
#95437 = CARTESIAN_POINT ( 'NONE',  ( 206.4695239676918845, 273.0312896038346366, 10.41704154450801667 ) ) ;
#95438 = PLANE ( 'NONE',  #35470 ) ;
#95439 = CARTESIAN_POINT ( 'NONE',  ( 80.82369704674587751, 43.25674710424449643, -9.944928983646200038 ) ) ;
#95440 = CARTESIAN_POINT ( 'NONE',  ( 35.94483945213000453, 39.49103043416551628, -8.090169943749479842 ) ) ;
#95441 = CARTESIAN_POINT ( 'NONE',  ( -19.65312891409030271, 93.06504152958497400, 10.00000000000000888 ) ) ;
#95442 = CARTESIAN_POINT ( 'NONE',  ( 9.471979480098337234, 23.65586893147754566, -7.433330006724137462 ) ) ;
#95443 = CARTESIAN_POINT ( 'NONE',  ( 168.5369495251266017, 288.2168004222731952, 0.5299370344187100956 ) ) ;
#95444 = CARTESIAN_POINT ( 'NONE',  ( 13.34262526062736676, 23.10171378149917487, 9.188101187500008038 ) ) ;
#95445 = AXIS2_PLACEMENT_3D ( 'NONE', #51009, #43407, #35818 ) ;
#95446 = CARTESIAN_POINT ( 'NONE',  ( 160.2868107770284780, 253.0220952814450470, 14.63377360142983896 ) ) ;
#95447 = DIRECTION ( 'NONE',  ( 0.000000000000000000, -0.7457702847286216130, 0.6662031840330625565 ) ) ;
#95448 = CARTESIAN_POINT ( 'NONE',  ( 152.9666954755989821, 274.9684375997553047, 10.70794663735621910 ) ) ;
#95449 = CARTESIAN_POINT ( 'NONE',  ( 206.2041691044954348, 273.4908977089264113, -9.455375957961031474 ) ) ;
#95450 = ORIENTED_EDGE ( 'NONE', *, *, #59890, .T. ) ;
#95451 = CARTESIAN_POINT ( 'NONE',  ( 192.5049767439991513, 297.2185948999652965, 12.57567268027295881 ) ) ;
#95452 = CARTESIAN_POINT ( 'NONE',  ( 164.3706594650489023, 245.9486618633701482, -1.665857659249071698 ) ) ;
#95453 = CARTESIAN_POINT ( 'NONE',  ( 66.26747146336929006, 68.17285859727699915, 4.275621689475024745 ) ) ;
#95454 = CARTESIAN_POINT ( 'NONE',  ( 87.74082335983182190, 45.11567895962653552, 6.804767787324426997 ) ) ;
#95455 = DIRECTION ( 'NONE',  ( -0.8435938723211519052, -0.5369817302126803638, 0.000000000000000000 ) ) ;
#95456 = ORIENTED_EDGE ( 'NONE', *, *, #2059, .T. ) ;
#95457 = ORIENTED_EDGE ( 'NONE', *, *, #12722, .F. ) ;
#95458 = CARTESIAN_POINT ( 'NONE',  ( 155.9203642860871071, 276.9606713036284873, -10.23193020684348653 ) ) ;
#95459 = CARTESIAN_POINT ( 'NONE',  ( 86.61846192408904699, 47.19909516036467068, 10.60101820161781561 ) ) ;
#95460 = ORIENTED_EDGE ( 'NONE', *, *, #32045, .T. ) ;
#95461 = CARTESIAN_POINT ( 'NONE',  ( 77.08070689000365405, 54.07734400991444801, 16.01987238285506976 ) ) ;
#95462 = CARTESIAN_POINT ( 'NONE',  ( 188.6770513902144160, 297.7343742726931168, 7.725911427269801734 ) ) ;
#95463 = ORIENTED_EDGE ( 'NONE', *, *, #79064, .T. ) ;
#95464 = CARTESIAN_POINT ( 'NONE',  ( 27.85515008297419826, 39.58029201028043076, 1.583844403245397769 ) ) ;
#95465 = DIRECTION ( 'NONE',  ( 0.3002896333693371722, 0.9538480676139722281, 0.000000000000000000 ) ) ;
#95466 = B_SPLINE_CURVE_WITH_KNOTS ( 'NONE', 3,
 ( #80648, #49214, #26410, #88262 ),
 .UNSPECIFIED., .F., .F.,
 ( 4, 4 ),
 ( 2.151919402719074343E-15, 0.001406589747191096295 ),
 .UNSPECIFIED. ) ;
#95467 = CARTESIAN_POINT ( 'NONE',  ( 44.08135397534552880, 118.8355609772188188, -10.00000000000000000 ) ) ;
#95468 = ORIENTED_EDGE ( 'NONE', *, *, #28127, .F. ) ;
#95469 = CARTESIAN_POINT ( 'NONE',  ( 173.8153613617645590, 267.2422669803751205, 17.07281103384172383 ) ) ;
#95470 = CARTESIAN_POINT ( 'NONE',  ( 164.8849641302980444, 245.0578600525887794, 2.884140591399200648 ) ) ;
#95471 = CARTESIAN_POINT ( 'NONE',  ( 45.19716250472275476, 70.24742367233086782, -10.00000000000000000 ) ) ;
#95472 = VERTEX_POINT ( 'NONE', #45251 ) ;
#95473 = CARTESIAN_POINT ( 'NONE',  ( 170.9300592470816014, 255.0224789877633214, -11.37166744830014586 ) ) ;
#95474 = CARTESIAN_POINT ( 'NONE',  ( 163.4004183463084416, 247.6291687766210146, 10.19167732382099345 ) ) ;
#95475 = ORIENTED_EDGE ( 'NONE', *, *, #95662, .F. ) ;
#95476 = VERTEX_POINT ( 'NONE', #46229 ) ;
#95477 = CARTESIAN_POINT ( 'NONE',  ( 158.0824493049356363, 267.3773279949191988, -16.20755095283232450 ) ) ;
#95478 = ORIENTED_EDGE ( 'NONE', *, *, #13111, .F. ) ;
#95479 = CARTESIAN_POINT ( 'NONE',  ( 160.6762863198379421, 270.7031352422249597, 15.85774362266417015 ) ) ;
#95480 = VERTEX_POINT ( 'NONE', #30052 ) ;
#95481 = CARTESIAN_POINT ( 'NONE',  ( 84.09736312987760698, 50.03755393994106271, -13.91877743777747511 ) ) ;
#95482 = CARTESIAN_POINT ( 'NONE',  ( 147.4174248404692094, 275.3125255857779052, 7.386196481672387293 ) ) ;
#95483 = CARTESIAN_POINT ( 'NONE',  ( 180.0945261039350953, 290.8209287807282521, -9.536000357058787458 ) ) ;
#95484 = CARTESIAN_POINT ( 'NONE',  ( 194.6820509838467785, 270.8910309865917156, -14.27696746312268239 ) ) ;
#95485 = CARTESIAN_POINT ( 'NONE',  ( 192.1640094933931096, 297.8091675017319062, 12.36911124822534447 ) ) ;
#95487 = CARTESIAN_POINT ( 'NONE',  ( 174.7134278764181659, 289.9860957709516924, 6.278215837728235549 ) ) ;
#95486 = AXIS2_PLACEMENT_3D ( 'NONE', #17539, #8446, #92584 ) ;
#95488 = CARTESIAN_POINT ( 'NONE',  ( 158.3414723807261169, 256.3915202217551723, -16.63524069124627758 ) ) ;
#95489 = ORIENTED_EDGE ( 'NONE', *, *, #83861, .T. ) ;
#95490 = FACE_OUTER_BOUND ( 'NONE', #26516, .T. ) ;
#95491 = CARTESIAN_POINT ( 'NONE',  ( 24.30746885452586525, 16.96004757982090183, -5.678558825948276656 ) ) ;
#95492 = ADVANCED_FACE ( 'NONE', ( #77153 ), #83801, .T. ) ;
#95493 = CARTESIAN_POINT ( 'NONE',  ( 164.2545401858843945, 246.1497863546213978, 2.275217130759496609 ) ) ;
#95494 = CARTESIAN_POINT ( 'NONE',  ( 206.1932826529868805, 273.5097535960530877, 11.72208607728249241 ) ) ;
#95496 = EDGE_LOOP ( 'NONE', ( #13926, #21046, #74750 ) ) ;
#95495 = CARTESIAN_POINT ( 'NONE',  ( 198.3075590527773784, 287.1682275260610027, 16.94807365630277118 ) ) ;
#95497 = ORIENTED_EDGE ( 'NONE', *, *, #84131, .T. ) ;
#95498 = CARTESIAN_POINT ( 'NONE',  ( 190.3379505298266849, 300.9719944042457200, 6.192102975663287268 ) ) ;
#95499 = CARTESIAN_POINT ( 'NONE',  ( -19.65312891409030271, 93.06504152958497400, 203.6502102582797420 ) ) ;
#95500 = CARTESIAN_POINT ( 'NONE',  ( 40.44261144040436307, 35.30066082961425167, -10.00000000000000533 ) ) ;
#95501 = CARTESIAN_POINT ( 'NONE',  ( -19.65312891409030271, 93.06504152958497400, -10.00000000000000888 ) ) ;
#95502 = B_SPLINE_CURVE_WITH_KNOTS ( 'NONE', 3,
 ( #37577, #68485, #99413, #85234, #29990, #60871, #38582, #84242, #14791, #45673 ),
 .UNSPECIFIED., .F., .F.,
 ( 4, 2, 2, 2, 4 ),
 ( 0.000000000000000000, 0.0002622400424272710705, 0.0005244800848545421411, 0.0007867201272818132116, 0.001048960169709084282 ),
 .UNSPECIFIED. ) ;
#95503 = ADVANCED_FACE ( 'NONE', ( #91902 ), #84793, .T. ) ;
#95504 = CARTESIAN_POINT ( 'NONE',  ( 200.2690241097007799, 283.7708703901988656, 16.96680019208369927 ) ) ;
#95505 = CARTESIAN_POINT ( 'NONE',  ( 190.9055496984007902, 261.7574849729193716, -0.1787456162138263693 ) ) ;
#95506 = VECTOR ( 'NONE', #98599, 999.9999999999998863 ) ;
#95507 = ORIENTED_EDGE ( 'NONE', *, *, #10198, .F. ) ;
#95508 = CARTESIAN_POINT ( 'NONE',  ( 161.2535912560966551, 263.0844709175967182, -17.80682751047658030 ) ) ;
#95509 = FACE_OUTER_BOUND ( 'NONE', #60247, .T. ) ;
#95511 = EDGE_CURVE ( 'NONE', #91554, #8241, #84302, .T. ) ;
#95510 = CARTESIAN_POINT ( 'NONE',  ( 207.4826643481121664, 271.2764789897469768, 7.783310782367018454 ) ) ;
#95512 = CARTESIAN_POINT ( 'NONE',  ( 22.44857442947622417, 183.7677522451418497, 10.00000000000009592 ) ) ;
#95513 = CARTESIAN_POINT ( 'NONE',  ( 92.21748570181026139, 233.2369531367911009, -4.594050593750048428 ) ) ;
#95514 = CARTESIAN_POINT ( 'NONE',  ( 82.45152879043666871, 40.98320966393081477, -1.227003583139177234 ) ) ;
#95515 = CARTESIAN_POINT ( 'NONE',  ( 92.09145065047479761, 230.6427522451419065, 10.00000000000009415 ) ) ;
#95516 = CARTESIAN_POINT ( 'NONE',  ( 207.5573902749007971, 271.1470498879065190, 2.528158314636208548 ) ) ;
#95517 = CARTESIAN_POINT ( 'NONE',  ( 20.58103360645747770, 188.8149278399161233, -9.188101187500095079 ) ) ;
#95518 = CIRCLE ( 'NONE', #38811, 0.1418229129680897982 ) ;
#95519 = CARTESIAN_POINT ( 'NONE',  ( 200.6449165581618956, 283.1198055712825976, 18.35107460171532523 ) ) ;
#95520 = ORIENTED_EDGE ( 'NONE', *, *, #76421, .T. ) ;
#95521 = VERTEX_POINT ( 'NONE', #76659 ) ;
#95522 = CARTESIAN_POINT ( 'NONE',  ( 147.7487458879263897, 276.5474634960659728, -0.9591148040551028542 ) ) ;
#95523 =( BOUNDED_CURVE ( )  B_SPLINE_CURVE ( 2, ( #837, #70232, #40321, #87011, #31718, #46423, #77348, #48447, #62622 ),
 .UNSPECIFIED., .F., .T. ) 
 B_SPLINE_CURVE_WITH_KNOTS ( ( 3, 2, 2, 2, 3 ),
 ( 0.3911290322580645018, 0.3924731182795698770, 0.3951612903225806273, 0.3978494623655913776, 0.3991935483870967527 ),
 .UNSPECIFIED. ) 
 CURVE ( )  GEOMETRIC_REPRESENTATION_ITEM ( )  RATIONAL_B_SPLINE_CURVE ( ( 0.9330127018922194093, 0.9330127018922194093, 1.000000000000000000, 0.8660254037844387076, 1.000000000000000000, 0.8660254037844387076, 1.000000000000000000, 0.9330127018922194093, 0.9330127018922194093 ) ) 
 REPRESENTATION_ITEM ( '' )  );
#95524 = CARTESIAN_POINT ( 'NONE',  ( 68.06957118741028978, 69.65128302599352139, 2.634141232969352764 ) ) ;
#95525 = CARTESIAN_POINT ( 'NONE',  ( 84.37164395270971795, 44.14120688093528599, 7.575032260828749919 ) ) ;
#95526 = CARTESIAN_POINT ( 'NONE',  ( 193.6173108488650882, 262.6670938961573825, -4.018541380834022014 ) ) ;
#95527 = CARTESIAN_POINT ( 'NONE',  ( 207.8996209429610360, 270.5542889829179103, -5.987818313449536411 ) ) ;
#95528 = CARTESIAN_POINT ( 'NONE',  ( 185.8808357693771427, 286.5678490806189984, 15.69086117514267897 ) ) ;
#95529 = CARTESIAN_POINT ( 'NONE',  ( 167.7347975179296498, 251.7814102707968118, 10.38933443070461138 ) ) ;
#95530 = CARTESIAN_POINT ( 'NONE',  ( 41.01373370305532973, 203.6744531367911293, 4.594050593750047540 ) ) ;
#95531 = CARTESIAN_POINT ( 'NONE',  ( 78.37938175722116796, 229.3927522451419350, 2.944929066748280225E-16 ) ) ;
#95532 = CARTESIAN_POINT ( 'NONE',  ( 83.57287430471535572, 46.19826479596613922, 10.70837057327410236 ) ) ;
#95533 = CARTESIAN_POINT ( 'NONE',  ( 180.9257151590790897, 260.3651392059021532, -10.38670931792631968 ) ) ;
#95534 = CARTESIAN_POINT ( 'NONE',  ( 7.212287079182728711, 162.7202760586659736, -5.415160957724236172E-17 ) ) ;
#95535 = CARTESIAN_POINT ( 'NONE',  ( 68.63161566428617277, 64.63521157819846508, -12.16067767049918302 ) ) ;
#95536 = CARTESIAN_POINT ( 'NONE',  ( 199.0756812798354645, 285.8378008023734083, -18.45377816087746936 ) ) ;
#95537 = CARTESIAN_POINT ( 'NONE',  ( 186.4273393382061386, 282.8874102186402411, 16.17533557276407308 ) ) ;
#95538 = CARTESIAN_POINT ( 'NONE',  ( 147.2567621633200474, 275.5908015054806128, -3.647191014543873955 ) ) ;
#95539 = B_SPLINE_CURVE_WITH_KNOTS ( 'NONE', 3,
 ( #78370, #24153, #85502, #9461, #86019, #70242, #17043, #39818, #16050, #46951, #63147, #16545, #77868, #94093, #79895, #86512, #64151, #56546, #8951, #56026, #47934, #8453, #70750, #39325, #78875, #40331, #71271, #87533, #9966, #847, #1861, #32745, #63649, #31727, #62629, #25142, #87020, #17551, #48458, #79400, #40827, #2372, #18064, #33250, #95102, #25666, #48961, #10460 ),
 .UNSPECIFIED., .F., .F.,
 ( 4, 2, 2, 2, 2, 2, 2, 2, 2, 2, 2, 2, 2, 2, 2, 2, 2, 2, 2, 2, 2, 2, 2, 4 ),
 ( 0.003452227750546106588, 0.003635194737864935396, 0.003726678231524355872, 0.003818161725183775914, 0.003909645218843195956, 0.004001128712502616432, 0.004184095699821572742, 0.004550029674459376075, 0.004915963649097178541, 0.005647831598372718420, 0.006379699547648259167, 0.007843435446199253924, 0.008026402433518126101, 0.008117885927177600353, 0.008163627674007377377, 0.008209369420837152667, 0.008232240294252041179, 0.008255111167666931427, 0.008300852914496736207, 0.008392336408156418626, 0.008575303395475786933, 0.008758270382795155240, 0.008941237370114523547, 0.009307171344753268835 ),
 .UNSPECIFIED. ) ;
#95540 = CARTESIAN_POINT ( 'NONE',  ( 156.6812872898450735, 261.2670451491295012, 0.000000000000000000 ) ) ;
#95541 = CARTESIAN_POINT ( 'NONE',  ( 204.8523313866422484, 275.8323493198358847, 14.65426965484541100 ) ) ;
#95542 = CARTESIAN_POINT ( 'NONE',  ( 191.4082244002820516, 299.1182256826033949, -8.271837126846561361 ) ) ;
#95543 = CARTESIAN_POINT ( 'NONE',  ( 164.6460902696047128, 245.4716017159096566, -3.036414139157908476 ) ) ;
#95544 = ORIENTED_EDGE ( 'NONE', *, *, #75666, .T. ) ;
#95545 = CARTESIAN_POINT ( 'NONE',  ( 0.09429369783835704621, 160.8615022471902023, 5.000000000000051514 ) ) ;
#95546 = CARTESIAN_POINT ( 'NONE',  ( 161.3754592430677235, 251.5660820581029782, -13.21728889732328582 ) ) ;
#95547 = CARTESIAN_POINT ( 'NONE',  ( 117.9006383567337792, 245.0024278399160949, 9.188101187500095079 ) ) ;
#95548 = EDGE_CURVE ( 'NONE', #31346, #65907, #21586, .T. ) ;
#95549 = CARTESIAN_POINT ( 'NONE',  ( 16.96131155903493593, 31.83396525600390348, -2.839279412974133887 ) ) ;
#95550 = CARTESIAN_POINT ( 'NONE',  ( 75.29548954665729354, 66.77148020061324019, 13.38688763123640868 ) ) ;
#95551 = AXIS2_PLACEMENT_3D ( 'NONE', #35275, #67166, #59549 ) ;
#95552 = EDGE_CURVE ( 'NONE', #67404, #69466, #73437, .T. ) ;
#95553 = CARTESIAN_POINT ( 'NONE',  ( 28.70170512279456076, 111.4490886171364821, 59.99999999999999289 ) ) ;
#95555 = DIRECTION ( 'NONE',  ( -0.9755587037855265597, 0.2197389712097134185, 0.000000000000000000 ) ) ;
#95554 = DIRECTION ( 'NONE',  ( 0.9999580202055560196, 0.009162850352631533510, 0.000000000000000000 ) ) ;
#95556 = CARTESIAN_POINT ( 'NONE',  ( 190.8353200730629737, 300.1105250852234008, -7.980428465987968067 ) ) ;
#95557 = ORIENTED_EDGE ( 'NONE', *, *, #56772, .T. ) ;
#95558 = CARTESIAN_POINT ( 'NONE',  ( 192.7873893855839071, 263.7602658877742670, -4.354176413973807058 ) ) ;
#95559 = CARTESIAN_POINT ( 'NONE',  ( 149.6564118588553924, 271.4344863124460971, -11.76165597393390172 ) ) ;
#95560 = CARTESIAN_POINT ( 'NONE',  ( -63.52717814648517702, 65.65608168532926925, 59.99999999999999289 ) ) ;
#95561 = DIRECTION ( 'NONE',  ( -0.6444573283589029034, 0.7646402761589956576, 0.000000000000000000 ) ) ;
#95562 = CARTESIAN_POINT ( 'NONE',  ( 81.64250830485353561, 55.19057895047647122, -15.91435995628795474 ) ) ;
#95563 = ORIENTED_EDGE ( 'NONE', *, *, #54261, .F. ) ;
#95564 = CARTESIAN_POINT ( 'NONE',  ( 189.1046751719556482, 265.6539275885750158, 10.79115261866721198 ) ) ;
#95565 = CARTESIAN_POINT ( 'NONE',  ( 193.1884577481565373, 273.3595093090821706, -16.04199635000458457 ) ) ;
#95566 = CARTESIAN_POINT ( 'NONE',  ( 168.7265333031080843, 271.8518808229929959, -17.19668397201396814 ) ) ;
#95567 = CARTESIAN_POINT ( 'NONE',  ( 71.94676095904019064, 72.61122666528672198, 1.254485733363779998 ) ) ;
#95568 = CARTESIAN_POINT ( 'NONE',  ( 200.1392393678551684, 272.4654854410964617, 12.57020546295501440 ) ) ;
#95569 = CARTESIAN_POINT ( 'NONE',  ( 74.56414817410225737, 187.8759306620403322, 18.47570218321542868 ) ) ;
#95570 = CARTESIAN_POINT ( 'NONE',  ( 70.94111402853239667, 71.65689097173488165, -0.4145321067673689575 ) ) ;
#95571 = VECTOR ( 'NONE', #89282, 1000.000000000000000 ) ;
#95572 = CARTESIAN_POINT ( 'NONE',  ( 192.5049767439991513, 297.2185948999652965, 12.57567268027295881 ) ) ;
#95573 = ORIENTED_EDGE ( 'NONE', *, *, #80105, .F. ) ;
#95574 = CARTESIAN_POINT ( 'NONE',  ( 159.6023402823087451, 258.6676503891110883, 17.43025742997651761 ) ) ;
#95575 = CARTESIAN_POINT ( 'NONE',  ( 12.62681055351980497, 12.45404122711131656, -8.090169943749478065 ) ) ;
#95576 = CARTESIAN_POINT ( 'NONE',  ( 173.9832671538335660, 272.2600618968111235, -16.61040946315311473 ) ) ;
#95577 = ORIENTED_EDGE ( 'NONE', *, *, #50652, .F. ) ;
#95578 = CARTESIAN_POINT ( 'NONE',  ( 167.2512865494106222, 280.7487606393313513, 11.65990675234894169 ) ) ;
#95579 = CARTESIAN_POINT ( 'NONE',  ( 194.9636675848471441, 292.9600174435121289, -15.57898232594655319 ) ) ;
#95580 = CARTESIAN_POINT ( 'NONE',  ( 164.8961913205752694, 246.0452500519421619, -1.096323744997464322 ) ) ;
#95581 = ORIENTED_EDGE ( 'NONE', *, *, #37258, .T. ) ;
#95582 = DIRECTION ( 'NONE',  ( -0.8660254037844387076, -0.4999999999999998890, -0.000000000000000000 ) ) ;
#95583 = CARTESIAN_POINT ( 'NONE',  ( 186.3725304700115544, 291.5966866658558843, 12.20655306884721369 ) ) ;
#95584 = B_SPLINE_CURVE_WITH_KNOTS ( 'NONE', 3,
 ( #98517, #6292, #51388, #5788, #36676, #74725, #83328, #20010, #58962, #29590 ),
 .UNSPECIFIED., .F., .F.,
 ( 4, 2, 2, 2, 4 ),
 ( 0.3032312338214309122, 0.6516156169107113483, 0.7387117126830333724, 0.8258078084553553966, 1.000000000000000000 ),
 .UNSPECIFIED. ) ;
#95585 = CARTESIAN_POINT ( 'NONE',  ( 191.2056514706806070, 299.4690922889112699, 7.290007621276087590 ) ) ;
#95586 = CARTESIAN_POINT ( 'NONE',  ( 81.62548137452107255, 50.83754634041029163, -14.55613181760977604 ) ) ;
#95587 = CARTESIAN_POINT ( 'NONE',  ( 84.73310270403948152, 49.83751242549850247, -13.16584697690378469 ) ) ;
#95588 = CARTESIAN_POINT ( 'NONE',  ( 203.4357368910538355, 278.2859629599173559, -16.45855118664066197 ) ) ;
#95589 = ORIENTED_EDGE ( 'NONE', *, *, #33178, .T. ) ;
#95590 = ORIENTED_EDGE ( 'NONE', *, *, #80172, .T. ) ;
#95591 = CARTESIAN_POINT ( 'NONE',  ( 178.1614477613976817, 260.9598035071301751, 12.21005518007415702 ) ) ;
#95592 = ORIENTED_EDGE ( 'NONE', *, *, #13893, .F. ) ;
#95593 = CARTESIAN_POINT ( 'NONE',  ( 192.9863438995966760, 294.0432375156728995, 14.14043846130007331 ) ) ;
#95594 = ORIENTED_EDGE ( 'NONE', *, *, #99668, .T. ) ;
#95595 = CARTESIAN_POINT ( 'NONE',  ( -22.42236680055709641, 157.8615022471902591, 0.000000000000000000 ) ) ;
#95596 = CARTESIAN_POINT ( 'NONE',  ( 149.0237174825091415, 274.5263358477994871, 9.114370506038131481 ) ) ;
#95597 = VERTEX_POINT ( 'NONE', #47735 ) ;
#95598 = CARTESIAN_POINT ( 'NONE',  ( 82.55774480658821801, 40.79923812737882116, 3.201402393612977626 ) ) ;
#95599 = CARTESIAN_POINT ( 'NONE',  ( 160.2740869459746023, 254.0686150970925610, -15.36085255641610914 ) ) ;
#95600 = CARTESIAN_POINT ( 'NONE',  ( 159.2487512388012476, 275.3823027008313034, -12.53260474664770463 ) ) ;
#95601 = CARTESIAN_POINT ( 'NONE',  ( 146.8574506849497538, 276.2824292740633041, -4.888313306692038118 ) ) ;
#95602 = FACE_OUTER_BOUND ( 'NONE', #53743, .T. ) ;
#95603 = CARTESIAN_POINT ( 'NONE',  ( 86.64367300647309378, 42.83085291352504242, -0.9951962297809489044 ) ) ;
#95604 = CARTESIAN_POINT ( 'NONE',  ( 157.9689631420808951, 280.9937072662406194, 2.205630096026304887 ) ) ;
#95605 = CARTESIAN_POINT ( 'NONE',  ( 144.0982539169780523, 247.8768266524160140, 9.188101187500098632 ) ) ;
#95606 = CARTESIAN_POINT ( 'NONE',  ( 70.50084764297432116, 61.32838242238358362, -14.81127601099039381 ) ) ;
#95607 = VERTEX_POINT ( 'NONE', #79701 ) ;
#95608 = ADVANCED_FACE ( 'NONE', ( #56843 ), #78671, .F. ) ;
#95610 = ORIENTED_EDGE ( 'NONE', *, *, #37502, .T. ) ;
#95609 = CARTESIAN_POINT ( 'NONE',  ( -14.65312891409034535, 84.40478749174073414, 0.000000000000000000 ) ) ;
#95611 = LINE ( 'NONE', #26160, #17396 ) ;
#95612 = CARTESIAN_POINT ( 'NONE',  ( 163.0683798854284703, 248.2042762609320903, 11.26611642476872710 ) ) ;
#95613 = ADVANCED_FACE ( 'NONE', ( #87339 ), #8263, .F. ) ;
#95614 = CARTESIAN_POINT ( 'NONE',  ( 75.92077897862843372, 64.70916915221214083, -14.31233127451968024 ) ) ;
#95615 = CARTESIAN_POINT ( 'NONE',  ( 79.36263291408793918, 45.67866562566761957, -12.88899626193393999 ) ) ;
#95616 = CARTESIAN_POINT ( 'NONE',  ( 153.3480993750124810, 276.8750838587924363, 7.125264275211442566 ) ) ;
#95617 = CARTESIAN_POINT ( 'NONE',  ( 153.1983976505312626, 265.2995869615763809, -17.69657798691567763 ) ) ;
#95618 = FACE_OUTER_BOUND ( 'NONE', #2896, .T. ) ;
#95619 = CARTESIAN_POINT ( 'NONE',  ( 171.6965468371157897, 280.0430691848860647, 13.87941070326743720 ) ) ;
#95620 = FACE_OUTER_BOUND ( 'NONE', #38817, .T. ) ;
#95621 = FACE_OUTER_BOUND ( 'NONE', #99291, .T. ) ;
#95622 = VERTEX_POINT ( 'NONE', #39626 ) ;
#95623 = CARTESIAN_POINT ( 'NONE',  ( 33.47037235539275457, 49.41749479597460493, 10.00000000000000000 ) ) ;
#95624 = CARTESIAN_POINT ( 'NONE',  ( 77.99518601148065500, 61.05539905302716619, -15.87786080876372274 ) ) ;
#95625 = EDGE_LOOP ( 'NONE', ( #51685, #36078, #94310, #17280 ) ) ;
#95627 = EDGE_CURVE ( 'NONE', #48481, #27644, #24944, .T. ) ;
#95626 = CARTESIAN_POINT ( 'NONE',  ( 164.0769311498514753, 278.1829446335003126, 13.34093408993252439 ) ) ;
#95628 = CARTESIAN_POINT ( 'NONE',  ( 201.0920123907623065, 267.8787980814687444, -2.846255320721498006 ) ) ;
#95629 = CARTESIAN_POINT ( 'NONE',  ( 152.1077061761917832, 267.1887200105145439, -15.41283704233756247 ) ) ;
#95630 = CARTESIAN_POINT ( 'NONE',  ( 190.0550686570564949, 301.4619601804237732, 4.203010638620038542 ) ) ;
#95631 = CARTESIAN_POINT ( 'NONE',  ( 202.2603678735342214, 280.3217618159037556, 16.49712126737133744 ) ) ;
#95633 = CARTESIAN_POINT ( 'NONE',  ( 154.1310696087535632, 276.6461666010558247, -8.687488248752188724 ) ) ;
#95632 = DIRECTION ( 'NONE',  ( 1.000000000000000000, 0.000000000000000000, 0.000000000000000000 ) ) ;
#95634 = CARTESIAN_POINT ( 'NONE',  ( 67.18526205639879834, 198.0494855054051868, -2.679491924311248496 ) ) ;
#95635 = ORIENTED_EDGE ( 'NONE', *, *, #65273, .F. ) ;
#95636 = CARTESIAN_POINT ( 'NONE',  ( 70.85377919256794144, 62.62944324200850588, -13.74144414313397000 ) ) ;
#95637 = CARTESIAN_POINT ( 'NONE',  ( 193.2657730933340474, 276.0652844845805021, -16.22139663033825130 ) ) ;
#95638 = EDGE_CURVE ( 'NONE', #97801, #6804, #23943, .T. ) ;
#95639 = CARTESIAN_POINT ( 'NONE',  ( 69.63879362503037385, 66.25765348761015616, -10.58390212558767374 ) ) ;
#95640 = EDGE_CURVE ( 'NONE', #78334, #54308, #1674, .T. ) ;
#95641 = DIRECTION ( 'NONE',  ( 0.000000000000000000, 0.000000000000000000, -1.000000000000000000 ) ) ;
#95642 = CIRCLE ( 'NONE', #29278, 0.1418229129681557177 ) ;
#95643 = CARTESIAN_POINT ( 'NONE',  ( 80.65610391127596301, 43.47179147593435289, -9.508242589467984729 ) ) ;
#95644 = CARTESIAN_POINT ( 'NONE',  ( 66.53768955469421087, 68.51814803147433963, 3.669749247662600133 ) ) ;
#95645 = CARTESIAN_POINT ( 'NONE',  ( -7.835251407336910390, 166.2833772461660828, -9.188101187500095079 ) ) ;
#95646 = CARTESIAN_POINT ( 'NONE',  ( 82.25819355828922141, 227.4869531367911293, 4.594050593750046652 ) ) ;
#95647 = CARTESIAN_POINT ( 'NONE',  ( 203.2187760522547819, 278.6617501559703101, -15.08675642319914978 ) ) ;
#95648 = CARTESIAN_POINT ( 'NONE',  ( 88.06347939733042551, 44.64227011997218142, -4.166356787718118682 ) ) ;
#95649 = CARTESIAN_POINT ( 'NONE',  ( 184.1217943198085152, 275.8755882355715130, -17.79325935397197256 ) ) ;
#95650 = B_SPLINE_CURVE_WITH_KNOTS ( 'NONE', 3,
 ( #45827, #76750, #61034, #92007, #7344, #22554, #99075, #29658, #61541, #76276 ),
 .UNSPECIFIED., .F., .F.,
 ( 4, 2, 2, 2, 4 ),
 ( 0.000000000000000000, 0.0004052285844863903752, 0.0008104571689727807504, 0.001215685753459171126, 0.001620914337945561501 ),
 .UNSPECIFIED. ) ;
#95651 = CARTESIAN_POINT ( 'NONE',  ( 138.6787122315880367, 239.3262482093457493, 3.021315404115420679E-15 ) ) ;
#95652 = CARTESIAN_POINT ( 'NONE',  ( 75.39279733249207993, 55.13144413046544656, -16.13680074438373069 ) ) ;
#95653 = CARTESIAN_POINT ( 'NONE',  ( 160.6263868137985753, 282.0864858795503096, 5.113129440300967943 ) ) ;
#95655 = CARTESIAN_POINT ( 'NONE',  ( 76.48640248419296483, 51.58918322513654431, 15.64831315713032645 ) ) ;
#95654 = DIRECTION ( 'NONE',  ( 0.6361630342459738685, -0.7715546603183444097, 0.000000000000000000 ) ) ;
#95656 = CARTESIAN_POINT ( 'NONE',  ( 178.0629634300817941, 289.8938732657310879, 9.603314252689274966 ) ) ;
#95657 = ADVANCED_FACE ( 'NONE', ( #25451 ), #27343, .T. ) ;
#95658 = LINE ( 'NONE', #51485, #25592 ) ;
#95659 = CARTESIAN_POINT ( 'NONE',  ( 74.97172962767024273, 56.14972995073008377, -16.13536416545135666 ) ) ;
#95660 = CARTESIAN_POINT ( 'NONE',  ( 82.84414721460336750, 52.67170891611750250, -15.43689080123882640 ) ) ;
#95661 = CARTESIAN_POINT ( 'NONE',  ( 73.33758058659837786, 69.90254644623917102, 9.645949167502998023 ) ) ;
#95662 = EDGE_CURVE ( 'NONE', #25397, #98060, #98932, .T. ) ;
#95663 = CARTESIAN_POINT ( 'NONE',  ( 56.08842225738448661, 197.0643266524160140, 9.188101187500095079 ) ) ;
#95664 = CARTESIAN_POINT ( 'NONE',  ( 77.08113471857714671, 63.57880127914461355, -15.41835532793242791 ) ) ;
#95665 = CARTESIAN_POINT ( 'NONE',  ( 76.87303194821100760, 209.0643266524160424, 9.188101187500095079 ) ) ;
#95666 = CARTESIAN_POINT ( 'NONE',  ( 161.8882824960653579, 250.2482648971885340, -13.83574485983625557 ) ) ;
#95667 = ADVANCED_FACE ( 'NONE', ( #52231 ), #30432, .T. ) ;
#95668 = CARTESIAN_POINT ( 'NONE',  ( 163.4612457243555923, 257.9110273980033980, 15.57507432676986703 ) ) ;
#95670 = FACE_OUTER_BOUND ( 'NONE', #22659, .T. ) ;
#95669 = CARTESIAN_POINT ( 'NONE',  ( 13.67211979723576931, 32.92651376809308772, 10.00000000000000000 ) ) ;
#95671 = CARTESIAN_POINT ( 'NONE',  ( 174.6996461476103661, 269.1010435442095172, -16.34783327481654780 ) ) ;
#95672 = EDGE_CURVE ( 'NONE', #5345, #79622, #5638, .T. ) ;
#95673 = CARTESIAN_POINT ( 'NONE',  ( 38.58005528328081368, 27.98920272979929535, 7.433330006724137462 ) ) ;
#95674 = CARTESIAN_POINT ( 'NONE',  ( 82.20333476588919552, 49.18919034555798930, 14.05466216932103229 ) ) ;
#95675 = CARTESIAN_POINT ( 'NONE',  ( 85.07790208279682531, 46.70498825579053914, -10.39314567700957248 ) ) ;
#95676 = ORIENTED_EDGE ( 'NONE', *, *, #72281, .T. ) ;
#95677 = CARTESIAN_POINT ( 'NONE',  ( 16.72494223679300873, 27.84336893147755987, -7.433330006724137462 ) ) ;
#95678 = CARTESIAN_POINT ( 'NONE',  ( 76.62902843369037953, 224.2369531367911293, -4.594050593750048428 ) ) ;
#95679 = LINE ( 'NONE', #18634, #83758 ) ;
#95680 = CARTESIAN_POINT ( 'NONE',  ( 169.1474947851822321, 288.3004841199922339, -1.112798234388539198 ) ) ;
#95681 = CARTESIAN_POINT ( 'NONE',  ( 192.5551423381268989, 297.1317055421444024, -13.20528585388119858 ) ) ;
#95682 = CARTESIAN_POINT ( 'NONE',  ( 42.55442611339157821, 60.96799964870728417, 10.00000000000000000 ) ) ;
#95683 = EDGE_CURVE ( 'NONE', #59100, #37455, #68923, .T. ) ;
#95684 = EDGE_CURVE ( 'NONE', #3083, #11960, #75975, .T. ) ;
#95685 = ORIENTED_EDGE ( 'NONE', *, *, #93904, .T. ) ;
#95686 = DIRECTION ( 'NONE',  ( -1.000000000000000000, 0.000000000000000000, 0.000000000000000000 ) ) ;
#95687 = CARTESIAN_POINT ( 'NONE',  ( 189.8780818209742733, 286.5329341612866756, 16.47277920618313729 ) ) ;
#95688 = FACE_OUTER_BOUND ( 'NONE', #97699, .T. ) ;
#95689 = CARTESIAN_POINT ( 'NONE',  ( 122.2038756314442054, 231.3615022471901739, 5.000000000000051514 ) ) ;
#95690 = CARTESIAN_POINT ( 'NONE',  ( 205.2414727015710412, 275.1583367910551488, -12.71338796362297963 ) ) ;
#95691 = CARTESIAN_POINT ( 'NONE',  ( 75.02805439306581547, 53.11903014810299339, 16.50248075768144318 ) ) ;
#95692 = ORIENTED_EDGE ( 'NONE', *, *, #44824, .F. ) ;
#95693 = CARTESIAN_POINT ( 'NONE',  ( 165.5692510255798027, 246.8512466342675395, -1.587510859644124750 ) ) ;
#95694 = ORIENTED_EDGE ( 'NONE', *, *, #64382, .F. ) ;
#95695 = CARTESIAN_POINT ( 'NONE',  ( 202.3421728196210552, 280.1800714929709670, 16.85915999540957344 ) ) ;
#95696 = CARTESIAN_POINT ( 'NONE',  ( 207.4143922525829566, 270.9009812163183142, -1.235003168413449703 ) ) ;
#95697 = FACE_OUTER_BOUND ( 'NONE', #31892, .T. ) ;
#95698 = ORIENTED_EDGE ( 'NONE', *, *, #20105, .F. ) ;
#95699 = CARTESIAN_POINT ( 'NONE',  ( 77.29458184488724726, 63.35267271352311269, -15.16560563611173507 ) ) ;
#95700 = ORIENTED_EDGE ( 'NONE', *, *, #15710, .T. ) ;
#95701 = CARTESIAN_POINT ( 'NONE',  ( 42.65610334793076674, 64.00004027534475881, 10.00000000000000000 ) ) ;
#95702 = CARTESIAN_POINT ( 'NONE',  ( 170.6386111665514989, 250.4289151046095299, 3.370994400240735711 ) ) ;
#95703 = B_SPLINE_CURVE_WITH_KNOTS ( 'NONE', 3,
 ( #68995, #30506, #91345, #61397, #77101, #54280, #84256, #8211, #21905, #31491, #83753, #6713, #92348, #22409, #38596, #85250, #45200, #45685, #68503, #15795, #76139, #99425, #30002, #60887, #16304, #115, #85774, #91849, #46700, #53302, #69994, #22898, #30999, #61887, #78120, #8709, #53783, #39577, #14803, #7198, #77627, #39081, #609, #62383, #93340, #41085 ),
 .UNSPECIFIED., .F., .F.,
 ( 4, 1, 2, 2, 1, 2, 2, 1, 1, 2, 2, 1, 1, 2, 2, 1, 1, 2, 2, 1, 1, 1, 2, 2, 1, 1, 1, 2, 2, 4 ),
 ( 0.000000000000000000, 0.06249999999998988309, 0.09374999999998481770, 0.1249999999999797662, 0.1874999999999709677, 0.2187499999999666656, 0.2499999999999623634, 0.3124999999999550915, 0.3437499999999521494, 0.3593749999999485967, 0.3749999999999450440, 0.4374999999999310552, 0.4687499999999235056, 0.4843749999999204525, 0.4999999999999173439, 0.5624999999999097389, 0.5937499999999078515, 0.6093749999999069633, 0.6249999999999059641, 0.6874999999999060751, 0.7187499999999081846, 0.7343749999999101830, 0.7421874999999107381, 0.7499999999999111822, 0.8124999999999258371, 0.8437499999999352740, 0.8593749999999390488, 0.8671874999999417133, 0.8749999999999442668, 1.000000000000000000 ),
 .UNSPECIFIED. ) ;
#95704 = CARTESIAN_POINT ( 'NONE',  ( 83.54554058275616057, 48.97625582294687518, 13.47504863331772107 ) ) ;
#95705 = EDGE_LOOP ( 'NONE', ( #62789, #41926, #90728, #26578 ) ) ;
#95706 = CARTESIAN_POINT ( 'NONE',  ( 31.05164846989082506, 29.87878583063843507, -9.188101187500006262 ) ) ;
#95707 = CARTESIAN_POINT ( 'NONE',  ( 81.59934002536490993, 48.72548848104391084, -13.46818898573163459 ) ) ;
#95708 = CARTESIAN_POINT ( 'NONE',  ( -19.65312891409030271, 93.06504152958497400, 177.5919119679930134 ) ) ;
#95709 = CYLINDRICAL_SURFACE ( 'NONE', #80514, 17.82106496071139645 ) ;
#95710 = ORIENTED_EDGE ( 'NONE', *, *, #28666, .T. ) ;
#95711 = VECTOR ( 'NONE', #22095, 1000.000000000000114 ) ;
#95712 = ORIENTED_EDGE ( 'NONE', *, *, #93204, .F. ) ;
#95713 = CARTESIAN_POINT ( 'NONE',  ( 198.2524512863544430, 286.8805590551967839, 16.95567094640148298 ) ) ;
#95715 = CARTESIAN_POINT ( 'NONE',  ( 194.5252985417586729, 293.7192948986070178, -14.54632727629426370 ) ) ;
#95714 = CARTESIAN_POINT ( 'NONE',  ( 164.2059258710715994, 246.2339888178522926, 7.329631442356459914 ) ) ;
#95716 = CARTESIAN_POINT ( 'NONE',  ( 85.33961507832758286, 48.52663690637297123, 12.44665103731247235 ) ) ;
#95717 = CARTESIAN_POINT ( 'NONE',  ( 155.4812142336614329, 261.3456326552338282, 18.45193178807985745 ) ) ;
#95718 = CARTESIAN_POINT ( 'NONE',  ( 147.7136411429809186, 276.4209930201117231, 0.9264851003149958686 ) ) ;
#95719 = CARTESIAN_POINT ( 'NONE',  ( 205.0994677818405023, 275.4042965269534307, -14.14519517703424789 ) ) ;
#95720 = CARTESIAN_POINT ( 'NONE',  ( 163.9711092878513341, 246.6407030704495185, 4.892543501721282162 ) ) ;
#95721 = CARTESIAN_POINT ( 'NONE',  ( 166.1339902640533523, 265.4989097315049094, 16.56817675206516682 ) ) ;
#95722 = LINE ( 'NONE', #25782, #12724 ) ;
#95723 = CARTESIAN_POINT ( 'NONE',  ( 91.86592320334659689, 223.8458772461660544, 9.188101187500095079 ) ) ;
#95724 = ORIENTED_EDGE ( 'NONE', *, *, #36636, .F. ) ;
#95725 = DIRECTION ( 'NONE',  ( 0.000000000000000000, -0.000000000000000000, -1.000000000000000000 ) ) ;
#95726 = CARTESIAN_POINT ( 'NONE',  ( 119.0307608796806278, 227.9824982072973683, 3.021315404115420679E-15 ) ) ;
#95727 = ORIENTED_EDGE ( 'NONE', *, *, #16674, .T. ) ;
#95728 = ORIENTED_EDGE ( 'NONE', *, *, #95261, .T. ) ;
#95729 = CARTESIAN_POINT ( 'NONE',  ( 80.07107477179017962, 44.27104509910737562, -11.43245809723916828 ) ) ;
#95730 = CARTESIAN_POINT ( 'NONE',  ( 177.2071603091147836, 292.4572209928213624, -2.700943100067172420 ) ) ;
#95731 = DIRECTION ( 'NONE',  ( 0.8660254037844395958, 0.4999999999999985567, 0.000000000000000000 ) ) ;
#95732 = CARTESIAN_POINT ( 'NONE',  ( 206.1615484827472358, 273.5647187912443314, -9.556459874778100883 ) ) ;
#95733 = CARTESIAN_POINT ( 'NONE',  ( 206.8716470161501491, 270.6909265943963874, -4.951756624771148196 ) ) ;
#95734 = CARTESIAN_POINT ( 'NONE',  ( 95.92559083146868204, 220.0643266524159856, -9.188101187500093303 ) ) ;
#95735 = VERTEX_POINT ( 'NONE', #6138 ) ;
#95736 = ORIENTED_EDGE ( 'NONE', *, *, #46394, .T. ) ;
#95737 = CARTESIAN_POINT ( 'NONE',  ( 207.6163508138795635, 271.0449272387537576, -1.385071889578343152 ) ) ;
#95738 = EDGE_LOOP ( 'NONE', ( #42713, #61599, #14191, #59663 ) ) ;
#95739 = EDGE_CURVE ( 'NONE', #4581, #82473, #43269, .T. ) ;
#95740 = CARTESIAN_POINT ( 'NONE',  ( 75.96894176838442547, 64.70234315684297144, -14.32931214104222839 ) ) ;
#95741 = CARTESIAN_POINT ( 'NONE',  ( -22.42236680055709641, 157.8615022471902591, 0.000000000000000000 ) ) ;
#95743 = CARTESIAN_POINT ( 'NONE',  ( 110.0000000000000000, -8.000000000000000000, -9.212605237762131694 ) ) ;
#95742 = CARTESIAN_POINT ( 'NONE',  ( 143.4758849319492526, 244.4548013555409796, -4.594050593750042211 ) ) ;
#95744 = CARTESIAN_POINT ( 'NONE',  ( -3.027006198515987734, 162.3927522451418213, 10.00000000000009592 ) ) ;
#95745 = CARTESIAN_POINT ( 'NONE',  ( 87.76670979354591395, 44.75042847539244661, 5.006797044073166170 ) ) ;
#95746 = ORIENTED_EDGE ( 'NONE', *, *, #91626, .F. ) ;
#95747 = CARTESIAN_POINT ( 'NONE',  ( 87.36419812053318878, 44.11474433763744685, -3.583216742975352087 ) ) ;
#95748 = CARTESIAN_POINT ( 'NONE',  ( 81.16897067834024426, 46.99626341444099609, 12.49506798774365812 ) ) ;
#95749 = CARTESIAN_POINT ( 'NONE',  ( 81.99805462481849361, 40.98459159741175029, -2.988575740387717339 ) ) ;
#95750 = CARTESIAN_POINT ( 'NONE',  ( 80.80672984637854483, 43.46007305841095558, 9.388711751469632105 ) ) ;
#95752 = EDGE_CURVE ( 'NONE', #7444, #66626, #98864, .T. ) ;
#95751 = CARTESIAN_POINT ( 'NONE',  ( 175.8027662909930484, 284.8719843250962072, 14.11304877541382119 ) ) ;
#95753 = B_SPLINE_CURVE_WITH_KNOTS ( 'NONE', 3,
 ( #60896, #58899, #89868, #31500 ),
 .UNSPECIFIED., .F., .F.,
 ( 4, 4 ),
 ( 0.004047834017227748896, 0.01202942932177893109 ),
 .UNSPECIFIED. ) ;
#95754 = CARTESIAN_POINT ( 'NONE',  ( 88.86175791728626905, 45.81123908072883921, 1.850091733736755357E-15 ) ) ;
#95755 = ADVANCED_FACE ( 'NONE', ( #51756 ), #60811, .T. ) ;
#95756 = DIRECTION ( 'NONE',  ( 0.5000000000000048850, -0.8660254037844358210, 0.000000000000000000 ) ) ;
#95757 = CARTESIAN_POINT ( 'NONE',  ( 7.888522331898304429, 165.3615022471902023, 5.000000000000051514 ) ) ;
#95758 = CARTESIAN_POINT ( 'NONE',  ( 161.0952649348064938, 251.6218116045831437, 13.81854265722852482 ) ) ;
#95759 = CARTESIAN_POINT ( 'NONE',  ( 83.29111138074479470, 41.74013809017890964, 3.135737421875423259 ) ) ;
#95760 = CARTESIAN_POINT ( 'NONE',  ( 167.7650414173376134, 249.6746511289063335, 7.938333554227506639 ) ) ;
#95761 = CARTESIAN_POINT ( 'NONE',  ( 78.44279992643997446, 61.32017871564067946, 16.22697472196325208 ) ) ;
#95762 = CARTESIAN_POINT ( 'NONE',  ( 175.8212761817833893, 290.2801695444399002, -6.226935068522726269 ) ) ;
#95763 = DIRECTION ( 'NONE',  ( 1.000000000000000000, 0.000000000000000000, 0.000000000000000000 ) ) ;
#95764 = B_SPLINE_CURVE_WITH_KNOTS ( 'NONE', 3,
 ( #10465, #8956, #33256, #70755 ),
 .UNSPECIFIED., .F., .F.,
 ( 4, 4 ),
 ( 0.000000000000000000, 0.0008757035534864545051 ),
 .UNSPECIFIED. ) ;
#95765 = CARTESIAN_POINT ( 'NONE',  ( 75.15176481940822839, 63.63400548413613933, -14.55503147312456846 ) ) ;
#95766 = CARTESIAN_POINT ( 'NONE',  ( 185.3869297780163095, 266.3934770207134193, 13.10756805561828742 ) ) ;
#95767 = CARTESIAN_POINT ( 'NONE',  ( 79.14863538599044546, 51.66069612159751046, 15.78305943820313573 ) ) ;
#95768 = CARTESIAN_POINT ( 'NONE',  ( 30.11635425815369871, 39.16126292948897003, -6.180339887498951690 ) ) ;
#95769 = LINE ( 'NONE', #94747, #49881 ) ;
#95770 =( LENGTH_UNIT ( ) NAMED_UNIT ( * ) SI_UNIT ( .MILLI., .METRE. ) );
#95771 = CARTESIAN_POINT ( 'NONE',  ( 157.7295765003705696, 271.0796008204293912, -14.71699761758586256 ) ) ;
#95772 = CARTESIAN_POINT ( 'NONE',  ( 86.48029715743111012, 43.63525664527010406, -3.689685108413566450 ) ) ;
#95773 = AXIS2_PLACEMENT_3D ( 'NONE', #79601, #62332, #30947 ) ;
#95774 = EDGE_CURVE ( 'NONE', #24730, #72762, #82698, .T. ) ;
#95775 = CARTESIAN_POINT ( 'NONE',  ( 12.78715206816254302, 172.0643266524160140, -9.188101187500093303 ) ) ;
#95776 = CARTESIAN_POINT ( 'NONE',  ( 81.02962758293600132, 44.75529754875908139, 10.68588457171068029 ) ) ;
#95777 = ORIENTED_EDGE ( 'NONE', *, *, #34860, .T. ) ;
#95778 = ADVANCED_FACE ( 'NONE', ( #38522 ), #15216, .T. ) ;
#95779 = CARTESIAN_POINT ( 'NONE',  ( 87.12517199902879383, 46.36582989257513532, 8.660211133915520776 ) ) ;
#95780 = ADVANCED_FACE ( 'NONE', ( #30932 ), #83684, .T. ) ;
#95781 = CYLINDRICAL_SURFACE ( 'NONE', #69341, 10.00000000000010658 ) ;
#95782 = CARTESIAN_POINT ( 'NONE',  ( 82.10268951128394121, 41.23340284509138343, 5.436379245411558259 ) ) ;
#95783 = CARTESIAN_POINT ( 'NONE',  ( 36.95476026646328194, 182.9548013555409796, -4.594050593750042211 ) ) ;
#95784 = CARTESIAN_POINT ( 'NONE',  ( 87.10076192357585967, 46.06401709681040302, 8.920816893773267253 ) ) ;
#95785 = CARTESIAN_POINT ( 'NONE',  ( 147.5498377207569263, 275.0831797495432056, 4.097967709737811326 ) ) ;
#95786 = CARTESIAN_POINT ( 'NONE',  ( 34.21278864456112956, 38.49103043416551628, -8.090169943749479842 ) ) ;
#95787 = CARTESIAN_POINT ( 'NONE',  ( 11.37297787527554327, 165.8262482093457777, 3.021315404115420679E-15 ) ) ;
#95788 = CARTESIAN_POINT ( 'NONE',  ( 147.1731211915891322, 275.7356719181125868, 0.5879280619134324981 ) ) ;
#95789 = CARTESIAN_POINT ( 'NONE',  ( 182.1788207689431829, 279.9818748238459420, -16.09985332685275594 ) ) ;
#95790 = DIRECTION ( 'NONE',  ( -0.9506327454577400138, -0.3103181967972222788, 0.000000000000000000 ) ) ;
#95791 = EDGE_CURVE ( 'NONE', #80984, #83021, #66453, .T. ) ;
#95792 = CARTESIAN_POINT ( 'NONE',  ( 166.6772716030373260, 257.8718083500641001, -15.18422749061457466 ) ) ;
#95793 = EDGE_CURVE ( 'NONE', #37421, #6372, #58798, .T. ) ;
#95794 = CARTESIAN_POINT ( 'NONE',  ( 83.66574516303663245, 229.1115022471903160, -5.000000000000047962 ) ) ;
#95796 =( BOUNDED_CURVE ( )  B_SPLINE_CURVE ( 2, ( #72505, #55742, #63872, #88236, #64884, #79116, #95830, #18291, #9698, #40558, #49185, #16767, #94809 ),
 .UNSPECIFIED., .F., .T. ) 
 B_SPLINE_CURVE_WITH_KNOTS ( ( 3, 2, 2, 2, 2, 2, 3 ),
 ( 0.9625000000000000222, 0.9649999999999999689, 0.9699999999999999734, 0.9749999999999999778, 0.9799999999999999822, 0.9849999999999999867, 0.9875000000000000444 ),
 .UNSPECIFIED. ) 
 CURVE ( )  GEOMETRIC_REPRESENTATION_ITEM ( )  RATIONAL_B_SPLINE_CURVE ( ( 0.9755282581475767101, 0.9755282581475772652, 1.000000000000000000, 0.9510565162951535312, 1.000000000000000000, 0.9510565162951535312, 1.000000000000000000, 0.9510565162951535312, 1.000000000000000000, 0.9510565162951535312, 1.000000000000000000, 0.9755282581475761550, 0.9755282581475767101 ) ) 
 REPRESENTATION_ITEM ( '' )  );
#95795 = CARTESIAN_POINT ( 'NONE',  ( 92.83118068642198750, 217.7365022471902023, -10.00000000000009059 ) ) ;
#95797 = LINE ( 'NONE', #42034, #37745 ) ;
#95798 = CARTESIAN_POINT ( 'NONE',  ( 29.86737195101775200, 39.01751292744058475, 6.180339887498949913 ) ) ;
#95799 = CARTESIAN_POINT ( 'NONE',  ( 43.63930707798317599, 189.8768266524159856, -9.188101187500091527 ) ) ;
#95800 = CARTESIAN_POINT ( 'NONE',  ( 85.33699565288863198, 48.33901173460943568, -12.30238903177782284 ) ) ;
#95801 = ORIENTED_EDGE ( 'NONE', *, *, #9504, .T. ) ;
#95802 = FACE_OUTER_BOUND ( 'NONE', #99345, .T. ) ;
#95803 = CARTESIAN_POINT ( 'NONE',  ( 198.4427928769277969, 286.9339956717308837, -17.97122743692687763 ) ) ;
#95804 = CARTESIAN_POINT ( 'NONE',  ( 67.14715456163476404, 67.13714923225593623, -8.580159373155410663 ) ) ;
#95805 = ORIENTED_EDGE ( 'NONE', *, *, #31086, .F. ) ;
#95806 = CARTESIAN_POINT ( 'NONE',  ( 171.2443217382905800, 286.5344483683264798, 7.485321208534859494 ) ) ;
#95807 = CARTESIAN_POINT ( 'NONE',  ( 164.2578067403839555, 246.1441285162624126, -2.322300236470859591 ) ) ;
#95808 = CARTESIAN_POINT ( 'NONE',  ( 193.3873874904946035, 295.6902146538902230, 13.58053800763477703 ) ) ;
#95809 = CARTESIAN_POINT ( 'NONE',  ( 82.09429624515669843, 46.55866185173159977, -12.38170325825488405 ) ) ;
#95810 = CARTESIAN_POINT ( 'NONE',  ( 31.32709252658613508, 23.80170272979928114, 7.433330006724137462 ) ) ;
#95811 = CARTESIAN_POINT ( 'NONE',  ( 163.0171530587457767, 248.2930037274571191, 9.677214176418313940 ) ) ;
#95812 = CARTESIAN_POINT ( 'NONE',  ( 197.0313051377892748, 289.3787641501790517, -17.15509075150697882 ) ) ;
#95813 = CARTESIAN_POINT ( 'NONE',  ( 174.9413478015634098, 257.3571669544361384, 11.48782993742858771 ) ) ;
#95814 = ORIENTED_EDGE ( 'NONE', *, *, #39399, .F. ) ;
#95815 = CARTESIAN_POINT ( 'NONE',  ( 17.03285546273658113, 12.76004757982088655, 5.678558825948272215 ) ) ;
#95816 = FACE_OUTER_BOUND ( 'NONE', #89010, .T. ) ;
#95817 = CARTESIAN_POINT ( 'NONE',  ( -55.56624327025929944, 44.99999999999998579, 10.00000000000000000 ) ) ;
#95818 = LINE ( 'NONE', #56249, #1977 ) ;
#95819 = VERTEX_POINT ( 'NONE', #79074 ) ;
#95820 = CARTESIAN_POINT ( 'NONE',  ( 72.16236457449060993, 71.55515601828724925, -5.863900035885150075 ) ) ;
#95821 = CARTESIAN_POINT ( 'NONE',  ( 167.0487131668929806, 261.4106595961994230, 16.87154839675361018 ) ) ;
#95822 = CYLINDRICAL_SURFACE ( 'NONE', #54943, 60.00000000000002132 ) ;
#95823 = DIRECTION ( 'NONE',  ( -0.7226656227773308183, -0.6911977992267138715, 0.000000000000000000 ) ) ;
#95824 = ORIENTED_EDGE ( 'NONE', *, *, #63745, .F. ) ;
#95825 = EDGE_LOOP ( 'NONE', ( #64879, #80299, #66522, #30108 ) ) ;
#95827 = DIRECTION ( 'NONE',  ( -1.000000000000000000, 0.000000000000000000, 0.000000000000000000 ) ) ;
#95826 = CARTESIAN_POINT ( 'NONE',  ( 207.1285138014047504, 271.8898857301724661, -5.752177443817618752 ) ) ;
#95828 = CARTESIAN_POINT ( 'NONE',  ( 149.3253462891332219, 272.0079086998416074, -12.99539319630191336 ) ) ;
#95829 = ORIENTED_EDGE ( 'NONE', *, *, #31753, .F. ) ;
#95830 = CARTESIAN_POINT ( 'NONE',  ( 40.17197850526964942, 35.14441083166263979, 10.00000000000000533 ) ) ;
#95831 = PLANE ( 'NONE',  #80443 ) ;
#95832 = CARTESIAN_POINT ( 'NONE',  ( 72.89289663045832413, 57.39945837237475246, -15.86463492901048511 ) ) ;
#95833 = CARTESIAN_POINT ( 'NONE',  ( 78.38767366332245956, 61.45523861435393798, -15.84040300007290014 ) ) ;
#95834 = EDGE_CURVE ( 'NONE', #74117, #33600, #4320, .T. ) ;
#95835 = CARTESIAN_POINT ( 'NONE',  ( 163.4341025207368716, 282.8476932499685859, 9.116081536633066307 ) ) ;
#95836 = CARTESIAN_POINT ( 'NONE',  ( 109.2403843188893831, 240.0024278399160949, -9.188101187500093303 ) ) ;
#95837 = CARTESIAN_POINT ( 'NONE',  ( 105.0000000000000000, 4.999999999999999112, 59.99999999999999289 ) ) ;
#95838 = VERTEX_POINT ( 'NONE', #63831 ) ;
#95839 = CARTESIAN_POINT ( 'NONE',  ( 207.9622466093905189, 270.4458181468041289, 3.586592550214158681 ) ) ;
#95840 = ORIENTED_EDGE ( 'NONE', *, *, #74715, .F. ) ;
#95841 = CARTESIAN_POINT ( 'NONE',  ( 34.84170590957603508, 35.51421378149921537, -9.188101187500004485 ) ) ;
#95842 = CARTESIAN_POINT ( 'NONE',  ( 159.8655504377736918, 253.7517395922482706, 15.51368179719542262 ) ) ;
#95843 = CARTESIAN_POINT ( 'NONE',  ( 78.19399585541323461, 47.86142559180260037, -14.00782581797713355 ) ) ;
#95844 = CARTESIAN_POINT ( 'NONE',  ( 63.61184440487929947, 207.5333772461660544, 9.188101187500095079 ) ) ;
#95845 = CARTESIAN_POINT ( 'NONE',  ( 73.83553503644242255, 68.51229284434135991, 11.41127707145446379 ) ) ;
#95846 = CARTESIAN_POINT ( 'NONE',  ( 191.5281967176683509, 298.9104275333885994, 7.715154960566919407 ) ) ;
#95847 = DIRECTION ( 'NONE',  ( -0.5000000000000001110, 0.8660254037844384856, 0.000000000000000000 ) ) ;
#95848 = CARTESIAN_POINT ( 'NONE',  ( -19.65312891409030271, 93.06504152958497400, -10.00000000000000888 ) ) ;
#95849 = ORIENTED_EDGE ( 'NONE', *, *, #14071, .F. ) ;
#95850 = FACE_OUTER_BOUND ( 'NONE', #75843, .T. ) ;
#95851 = CARTESIAN_POINT ( 'NONE',  ( 168.3557124657904467, 273.6222795104500278, 17.14480014634877136 ) ) ;
#95852 = ORIENTED_EDGE ( 'NONE', *, *, #12683, .F. ) ;
#95853 = DIRECTION ( 'NONE',  ( 1.000000000000000000, 0.000000000000000000, 0.000000000000000000 ) ) ;
#95854 = CARTESIAN_POINT ( 'NONE',  ( 173.8768829991239500, 278.0004084252144594, -16.03808046269689314 ) ) ;
#95855 = CARTESIAN_POINT ( 'NONE',  ( 161.8153478334749877, 250.3745914384277285, -14.21120979595050215 ) ) ;
#95856 = CARTESIAN_POINT ( 'NONE',  ( 146.8574506849497538, 276.2824292740633041, -4.888313306692038118 ) ) ;
#95857 = EDGE_CURVE ( 'NONE', #71488, #77470, #54714, .T. ) ;
#95858 = CARTESIAN_POINT ( 'NONE',  ( 190.2935937139882299, 301.0488226629397559, 4.649863831023156813 ) ) ;
#95859 = CARTESIAN_POINT ( 'NONE',  ( 36.90037335867696555, 192.1115022471902591, 10.00000000000009592 ) ) ;
#95860 = CARTESIAN_POINT ( 'NONE',  ( 165.0565241268390366, 244.7607094220335568, 2.191926263411719589 ) ) ;
#95861 = CARTESIAN_POINT ( 'NONE',  ( 75.53717334121844829, 65.45021734152629733, 13.83070122522489775 ) ) ;
#95862 = CARTESIAN_POINT ( 'NONE',  ( 164.3199246584869115, 254.2670161280514094, 14.21696250712841270 ) ) ;
#95863 = CARTESIAN_POINT ( 'NONE',  ( 207.9622466093905189, 270.4458181468041289, 3.586592550214158681 ) ) ;
#95864 = CARTESIAN_POINT ( 'NONE',  ( 117.0346129529493311, 244.5024278399160949, -9.188101187500093303 ) ) ;
#95865 = ORIENTED_EDGE ( 'NONE', *, *, #59647, .T. ) ;
#95866 = CARTESIAN_POINT ( 'NONE',  ( 83.88071297790835956, 44.16974053325726146, -8.051342648303378979 ) ) ;
#95867 = CARTESIAN_POINT ( 'NONE',  ( 83.90573916032475665, 42.04407056160079037, 2.878155474715036188 ) ) ;
#95868 = CARTESIAN_POINT ( 'NONE',  ( 155.4810912439522212, 261.3458456796594760, -18.44218279064527266 ) ) ;
#95869 = EDGE_CURVE ( 'NONE', #54902, #6127, #7035, .T. ) ;
#95870 = CARTESIAN_POINT ( 'NONE',  ( 204.9432097630379417, 275.6749433546094679, 13.74700047688257776 ) ) ;
#95871 = EDGE_CURVE ( 'NONE', #68457, #44895, #57278, .T. ) ;
#95872 = CARTESIAN_POINT ( 'NONE',  ( -4.668846022976095966, 168.1115022471902591, 10.00000000000009592 ) ) ;
#95873 = CARTESIAN_POINT ( 'NONE',  ( 175.8939073520130592, 252.7054158260212375, 5.280091837693253964 ) ) ;
#95874 = ORIENTED_EDGE ( 'NONE', *, *, #62989, .T. ) ;
#95875 = CARTESIAN_POINT ( 'NONE',  ( 80.36956643484273854, 57.45342863445996784, -16.58888403658913901 ) ) ;
#95876 = CARTESIAN_POINT ( 'NONE',  ( 155.1825101010379910, 273.4369430123585403, -12.92776615095295156 ) ) ;
#95878 = CARTESIAN_POINT ( 'NONE',  ( 184.9620068429786386, 260.8549389384861570, 10.28307718128925607 ) ) ;
#95877 = CARTESIAN_POINT ( 'NONE',  ( 147.6472966492084140, 275.3178831392595498, 3.373654813989544365 ) ) ;
#95879 = CARTESIAN_POINT ( 'NONE',  ( 206.1142978005191821, 273.6465593735555899, -11.17423994621995753 ) ) ;
#95880 = CARTESIAN_POINT ( 'NONE',  ( 138.9021014942714487, 244.8768266524160140, 9.188101187500096856 ) ) ;
#95881 = LINE ( 'NONE', #20335, #64328 ) ;
#95882 = CARTESIAN_POINT ( 'NONE',  ( 67.41238942065514550, 68.07228407881235910, 6.202831302144204528 ) ) ;
#95883 = CARTESIAN_POINT ( 'NONE',  ( 72.89481452351749624, 203.7048013555409796, 4.594050593750051981 ) ) ;
#95884 = CIRCLE ( 'NONE', #52137, 17.82106496071138224 ) ;
#95885 = CARTESIAN_POINT ( 'NONE',  ( 174.6446264865013802, 251.8031208292603083, 3.583545318800930080 ) ) ;
#95886 = B_SPLINE_SURFACE_WITH_KNOTS ( 'NONE', 3, 1, ( 
 ( #99766, #16155 ),
 ( #37932, #7051 ),
 ( #46030, #47546 ),
 ( #54633, #68845 ),
 ( #77472, #77967 ),
 ( #22763, #30857 ),
 ( #76947, #1472 ),
 ( #15133, #93695 ),
 ( #8066, #38941 ),
 ( #8562, #53640 ),
 ( #45539, #85092 ),
 ( #47053, #69353 ),
 ( #39927, #76471 ),
 ( #31349, #46535 ),
 ( #84595, #94195 ),
 ( #38439, #92691 ),
 ( #23242, #62232 ),
 ( #39429, #93184 ),
 ( #62739, #55135 ),
 ( #85612, #69846 ),
 ( #30357, #61742 ),
 ( #86121, #61242 ),
 ( #70348, #23738 ),
 ( #960, #9060 ),
 ( #24258, #16651 ),
 ( #31836, #78473 ),
 ( #92208, #7547 ),
 ( #70864, #84111 ),
 ( #54129, #32353 ),
 ( #63254, #24749 ),
 ( #14663, #100272 ) ),
 .UNSPECIFIED., .F., .F., .F.,
 ( 4, 3, 3, 3, 3, 3, 3, 3, 3, 3, 4 ),
 ( 2, 2 ),
 ( 0.000000000000000000, 0.1122669598086744880, 0.2243161639709676802, 0.3396355846218965246, 0.4553962076584930907, 0.5677860799922345159, 0.6749047109689415569, 0.7773884377078037478, 0.8775581155834019098, 0.9782364162377737982, 1.000000000000000000 ),
 ( 0.000000000000000000, 1.000000000000000000 ),
 .UNSPECIFIED. ) ;
#95887 = CARTESIAN_POINT ( 'NONE',  ( 15.94411698533127542, 24.90829794293879473, 10.00000000000000355 ) ) ;
#95888 = CARTESIAN_POINT ( 'NONE',  ( 190.6893905452545823, 300.3632824417117604, 3.294993852933539191 ) ) ;
#95889 = CARTESIAN_POINT ( 'NONE',  ( 81.62374368218522136, 41.76230689378201788, 5.959470817902202455 ) ) ;
#95890 = CARTESIAN_POINT ( 'NONE',  ( 172.6334465443935358, 287.8136291912904312, -8.329514407067593496 ) ) ;
#95891 = CARTESIAN_POINT ( 'NONE',  ( -22.42236680055709641, 157.8615022471902591, 0.000000000000000000 ) ) ;
#95892 = CARTESIAN_POINT ( 'NONE',  ( 193.7773542058511680, 288.6392134509156335, 16.07539256311286024 ) ) ;
#95893 = EDGE_CURVE ( 'NONE', #15371, #46807, #52970, .T. ) ;
#95894 = CARTESIAN_POINT ( 'NONE',  ( 110.7831656154889259, 244.7677522451419065, -5.000000000000047962 ) ) ;
#95895 = CARTESIAN_POINT ( 'NONE',  ( 81.59595212483856130, 51.57806399716481138, -14.84616350707865706 ) ) ;
#95896 = ORIENTED_EDGE ( 'NONE', *, *, #28920, .F. ) ;
#95897 = B_SPLINE_CURVE_WITH_KNOTS ( 'NONE', 3,
 ( #58797, #4118, #81662, #43610, #56820, #65913, #89289, #19837, #35520, #49238, #80173, #75527, #83149, #6619, #99822, #91246, #53688, #28409, #29418, #53209, #13717, #84645, #44592, #6112, #37984, #67917, #90267, #21810, #52695, #37493, #14215, #5615, #30406, #67410, #68896, #37007, #36006, #60287, #61298, #83657, #68401, #99328, #51732, #29908, #91744, #84162, #15186, #74548, #5126, #20840 ),
 .UNSPECIFIED., .F., .F.,
 ( 4, 2, 2, 2, 2, 2, 2, 2, 2, 2, 2, 2, 2, 2, 2, 2, 2, 2, 2, 2, 2, 2, 2, 2, 4 ),
 ( 0.001855169425541140348, 0.002306674773933914662, 0.002532427448130358198, 0.002758180122326801299, 0.002871056459425064267, 0.002983932796523326800, 0.003096809133621589334, 0.003209685470719852302, 0.003435438144916219943, 0.003661190819112586717, 0.004112696167505321132, 0.004564201515898056415, 0.005467212212683564276, 0.006370222909469071271, 0.006821728257861788339, 0.007273233606254505407, 0.007386109943352781385, 0.007442548111901956670, 0.007498986280451131956, 0.007611862617549461710, 0.007724738954647791464, 0.008176244303041004663, 0.008627749651434217862, 0.008853502325630750736, 0.009079254999827283609 ),
 .UNSPECIFIED. ) ;
#95899 = CARTESIAN_POINT ( 'NONE',  ( 196.4994169513186364, 290.3000215130921902, 16.82935102260526961 ) ) ;
#95898 = CIRCLE ( 'NONE', #68357, 60.00000000000002132 ) ;
#95900 = CARTESIAN_POINT ( 'NONE',  ( 29.30989995549245464, 44.80713248141895377, -10.00000000000000000 ) ) ;
#95901 = CARTESIAN_POINT ( 'NONE',  ( -3.126064726376516667, 162.8768266524159856, -9.188101187500093303 ) ) ;
#95902 = CARTESIAN_POINT ( 'NONE',  ( 41.36599039304901737, 188.5643266524159571, -9.188101187500093303 ) ) ;
#95903 = FACE_OUTER_BOUND ( 'NONE', #82223, .T. ) ;
#95904 = CARTESIAN_POINT ( 'NONE',  ( 22.23522817490527714, 21.03677371833801857, 10.00000000000000533 ) ) ;
#95905 = CARTESIAN_POINT ( 'NONE',  ( 46.80869107419874098, 110.6443039040113092, -10.00000000000000000 ) ) ;
#95906 = CARTESIAN_POINT ( 'NONE',  ( 204.7764732025852084, 275.9637395487929439, -14.02287343454361412 ) ) ;
#95907 = CARTESIAN_POINT ( 'NONE',  ( 72.27382559518491689, 71.95406617239038383, -3.744659656737702846 ) ) ;
#95908 = CARTESIAN_POINT ( 'NONE',  ( 190.4240181651484818, 300.8229208869809668, -4.214281362166949485 ) ) ;
#95909 = CARTESIAN_POINT ( 'NONE',  ( 73.84282566857962138, 55.27273555838809216, -16.11958282414678933 ) ) ;
#95910 = CARTESIAN_POINT ( 'NONE',  ( 67.84273934451060484, 196.6427522451417644, 1.119607411625061291E-15 ) ) ;
#95911 = CARTESIAN_POINT ( 'NONE',  ( 179.4717503424750191, 254.9888846402135698, -4.048912934998680768 ) ) ;
#95912 = CARTESIAN_POINT ( 'NONE',  ( 205.4103625296683617, 274.8658110279089897, -13.38953657917851814 ) ) ;
#95913 = CARTESIAN_POINT ( 'NONE',  ( -19.65312891409030271, 93.06504152958497400, -10.00000000000000888 ) ) ;
#95914 = CARTESIAN_POINT ( 'NONE',  ( 40.86965645935558911, 207.7365022471903444, 2.944929066748280225E-16 ) ) ;
#95915 = CYLINDRICAL_SURFACE ( 'NONE', #13486, 70.00000000000002842 ) ;
#95916 = CARTESIAN_POINT ( 'NONE',  ( 202.8167949821795446, 279.3580017930215149, 15.61966256214195070 ) ) ;
#95917 = CARTESIAN_POINT ( 'NONE',  ( 7.590652549690899420, 181.3149278399161233, -9.188101187500095079 ) ) ;
#95918 = CARTESIAN_POINT ( 'NONE',  ( 32.72297390791170812, 40.93396525600392977, 2.839279412974139660 ) ) ;
#95919 = CARTESIAN_POINT ( 'NONE',  ( 164.2249907514728591, 247.3163270870697374, 7.119847084444697494 ) ) ;
#95920 = CARTESIAN_POINT ( 'NONE',  ( 153.2712411579340426, 265.1734183057532732, 16.26687330118495467 ) ) ;
#95921 = CARTESIAN_POINT ( 'NONE',  ( 38.48863484149602954, 25.14754757982092670, -5.678558825948276656 ) ) ;
#95922 = CARTESIAN_POINT ( 'NONE',  ( 16.82306525903893046, 33.21091486745860522, -1.111400068045478839E-16 ) ) ;
#95923 = CARTESIAN_POINT ( 'NONE',  ( 207.6477529416552557, 270.9905371579805546, 7.447146952410988341 ) ) ;
#95924 = DIRECTION ( 'NONE',  ( 0.4999999999999998890, -0.8660254037844385966, 0.000000000000000000 ) ) ;
#95925 = CARTESIAN_POINT ( 'NONE',  ( 148.9831146496684084, 272.6006712873522133, -12.63706091291043343 ) ) ;
#95926 = CARTESIAN_POINT ( 'NONE',  ( 179.1373849174831605, 262.4190059985190828, -12.86234133925216661 ) ) ;
#95927 = ADVANCED_FACE ( 'NONE', ( #52133 ), #35936, .T. ) ;
#95928 = CARTESIAN_POINT ( 'NONE',  ( 13.91516400911260298, 10.96004757982088584, -5.678558825948276656 ) ) ;
#95929 = CARTESIAN_POINT ( 'NONE',  ( 168.8002605504911742, 287.8170950039586842, 0.5153475582423447943 ) ) ;
#95930 = CARTESIAN_POINT ( 'NONE',  ( 9.658441966945924051, 28.68290643055185996, 3.479690158560446702E-15 ) ) ;
#95931 = PLANE ( 'NONE',  #83001 ) ;
#95932 = CARTESIAN_POINT ( 'NONE',  ( 193.8603219414924013, 294.8710681561126989, 15.36476279452078586 ) ) ;
#95933 = CARTESIAN_POINT ( 'NONE',  ( 19.12865694409072148, 32.81751292744056769, -6.180339887498951690 ) ) ;
#95934 = CARTESIAN_POINT ( 'NONE',  ( 159.9997000813754084, 253.5193855937126841, -16.28798248637880519 ) ) ;
#95935 = CARTESIAN_POINT ( 'NONE',  ( 37.34220537994157496, 54.61056725541210710, 10.00000000000000000 ) ) ;
#95936 = VERTEX_POINT ( 'NONE', #66839 ) ;
#95937 = CARTESIAN_POINT ( 'NONE',  ( 153.4281311866982946, 266.9016768047333130, 16.59090889036721350 ) ) ;
#95938 = CARTESIAN_POINT ( 'NONE',  ( 206.9258336080761183, 272.2409381227055292, 6.776000910836894597 ) ) ;
#95939 = CARTESIAN_POINT ( 'NONE',  ( 66.28997097015012230, 68.26748065702538781, 4.019969198947881850 ) ) ;
#95940 = FACE_OUTER_BOUND ( 'NONE', #22373, .T. ) ;
#95941 = ORIENTED_EDGE ( 'NONE', *, *, #17580, .F. ) ;
#95942 = ORIENTED_EDGE ( 'NONE', *, *, #92076, .F. ) ;
#95944 = CYLINDRICAL_SURFACE ( 'NONE', #3864, 10.00000000000010658 ) ;
#95943 = CARTESIAN_POINT ( 'NONE',  ( 159.3707800328339772, 279.3010520915150892, -9.512535167852366413 ) ) ;
#95945 = CARTESIAN_POINT ( 'NONE',  ( 86.17334730086119521, 47.14257514812162952, 10.80675504988608715 ) ) ;
#95946 = ORIENTED_EDGE ( 'NONE', *, *, #18900, .F. ) ;
#95947 = CARTESIAN_POINT ( 'NONE',  ( 76.71053421761779134, 52.48524597020742988, 15.80685200372052357 ) ) ;
#95948 = CARTESIAN_POINT ( 'NONE',  ( 174.4609212082891645, 262.3652053495598011, 14.45053099647883421 ) ) ;
#95949 = ORIENTED_EDGE ( 'NONE', *, *, #36937, .F. ) ;
#95950 = CARTESIAN_POINT ( 'NONE',  ( 78.31205730182037428, 61.08770274336716710, -15.90934363462768708 ) ) ;
#95951 = CARTESIAN_POINT ( 'NONE',  ( 88.54283264841694745, 43.89585489789003248, -0.1669414168386812725 ) ) ;
#95952 = B_SPLINE_CURVE_WITH_KNOTS ( 'NONE', 3,
 ( #98945, #68517, #14326, #21920 ),
 .UNSPECIFIED., .F., .F.,
 ( 4, 4 ),
 ( 0.03783155665041418314, 0.04640911067165707365 ),
 .UNSPECIFIED. ) ;
#95953 = CARTESIAN_POINT ( 'NONE',  ( 80.00967963870645860, 48.43740759703016607, -14.32305472254445355 ) ) ;
#95954 = CARTESIAN_POINT ( 'NONE',  ( 80.53863348453982951, 43.47454295502769384, 9.594131698209025672 ) ) ;
#95955 = EDGE_LOOP ( 'NONE', ( #32651, #16395, #77486, #52810 ) ) ;
#95956 = CARTESIAN_POINT ( 'NONE',  ( 161.8948331661419218, 250.2369188037922356, 13.64419044796309777 ) ) ;
#95957 = CARTESIAN_POINT ( 'NONE',  ( 166.2387117564082928, 273.7804834095634305, -15.53909978882808751 ) ) ;
#95958 = CARTESIAN_POINT ( 'NONE',  ( 79.99999999999990052, 93.06504152958508769, -54.99999999999999289 ) ) ;
#95959 = ORIENTED_EDGE ( 'NONE', *, *, #23362, .T. ) ;
#95960 = LINE ( 'NONE', #41190, #82757 ) ;
#95961 = VECTOR ( 'NONE', #91804, 999.9999999999998863 ) ;
#95962 = VERTEX_POINT ( 'NONE', #5056 ) ;
#95963 = CARTESIAN_POINT ( 'NONE',  ( 160.1909080944511174, 268.7107883851168140, -16.56060088188987223 ) ) ;
#95964 = VERTEX_POINT ( 'NONE', #97766 ) ;
#95965 = CARTESIAN_POINT ( 'NONE',  ( 159.6567935606206277, 270.0351555761940290, 15.68078944156235366 ) ) ;
#95966 = ORIENTED_EDGE ( 'NONE', *, *, #10322, .T. ) ;
#95967 = CARTESIAN_POINT ( 'NONE',  ( 158.9454381233514653, 259.8133225073038375, 16.87078617150929460 ) ) ;
#95968 = CARTESIAN_POINT ( 'NONE',  ( 168.1983705843401538, 272.5412240438793674, 15.99188398643980058 ) ) ;
#95969 = CARTESIAN_POINT ( 'NONE',  ( 147.4780248038723869, 275.2075633702266941, 5.829684594924993135 ) ) ;
#95970 = CARTESIAN_POINT ( 'NONE',  ( 177.2459596484374345, 288.9155558376918407, -10.33532049625327787 ) ) ;
#95971 = CARTESIAN_POINT ( 'NONE',  ( 70.39481278435968647, 67.27897370780323172, 9.975814553134231488 ) ) ;
#95972 = DIRECTION ( 'NONE',  ( 0.000000000000000000, -0.000000000000000000, 1.000000000000000000 ) ) ;
#95973 = CARTESIAN_POINT ( 'NONE',  ( 161.0515428782683500, 277.3244187559503189, -13.42420650014866368 ) ) ;
#95974 = CARTESIAN_POINT ( 'NONE',  ( 197.2421906572374439, 289.0134997159141790, -18.24225164680234812 ) ) ;
#95975 = CIRCLE ( 'NONE', #26440, 0.1418229129680897982 ) ;
#95976 = ORIENTED_EDGE ( 'NONE', *, *, #88010, .F. ) ;
#95977 = LINE ( 'NONE', #17422, #64198 ) ;
#95978 = CARTESIAN_POINT ( 'NONE',  ( 26.65055534615017763, 21.10170272979927830, -7.433330006724141015 ) ) ;
#95979 = CARTESIAN_POINT ( 'NONE',  ( 206.0041637419966776, 273.8373171585603814, 11.66586596407113596 ) ) ;
#95980 = CARTESIAN_POINT ( 'NONE',  ( 77.52911305372531103, 49.76152791203366377, -14.96532194459484089 ) ) ;
#95982 = ORIENTED_EDGE ( 'NONE', *, *, #54191, .T. ) ;
#95981 = CARTESIAN_POINT ( 'NONE',  ( 159.5573297132660002, 254.2855935470410031, 16.91607698584599007 ) ) ;
#95983 = VERTEX_POINT ( 'NONE', #67849 ) ;
#95984 = CARTESIAN_POINT ( 'NONE',  ( 146.9058596572515114, 276.1985824744942875, -2.634658857186392922 ) ) ;
#95985 = CARTESIAN_POINT ( 'NONE',  ( 171.5908562547398617, 259.5510650329395617, -15.12831101081834007 ) ) ;
#95986 = CARTESIAN_POINT ( 'NONE',  ( 43.20833262110986084, 30.11029122506297995, -8.090169943749478065 ) ) ;
#95987 = CARTESIAN_POINT ( 'NONE',  ( 182.7190055043868142, 259.1992038300794547, 9.912833159430794794 ) ) ;
#95988 = EDGE_CURVE ( 'NONE', #33601, #40913, #35445, .T. ) ;
#95989 = CARTESIAN_POINT ( 'NONE',  ( 160.2969203227064554, 253.0045850346894269, -16.23213669264525549 ) ) ;
#95990 = EDGE_CURVE ( 'NONE', #48869, #55638, #55282, .T. ) ;
#95991 = CARTESIAN_POINT ( 'NONE',  ( 190.4261963075636288, 300.8191482336517311, 0.009177945319502334165 ) ) ;
#95992 = ORIENTED_EDGE ( 'NONE', *, *, #15181, .F. ) ;
#95993 = CARTESIAN_POINT ( 'NONE',  ( -14.65312891409034535, 84.40478749174073414, 0.000000000000000000 ) ) ;
#95994 = DIRECTION ( 'NONE',  ( 0.5295078238379082869, 0.5024823063052964445, -0.6834712842135746147 ) ) ;
#95995 = EDGE_CURVE ( 'NONE', #70584, #38287, #36938, .T. ) ;
#95996 = CARTESIAN_POINT ( 'NONE',  ( 207.3062152119541679, 271.5820978585240368, 7.879821064966149535 ) ) ;
#95997 = ADVANCED_FACE ( 'NONE', ( #74478 ), #37832, .F. ) ;
#95998 = CARTESIAN_POINT ( 'NONE',  ( 36.73799359191946934, 192.0177522451418781, -10.00000000000009592 ) ) ;
#95999 = CARTESIAN_POINT ( 'NONE',  ( 107.1028179730028285, 223.4548013555409796, -4.594050593750042211 ) ) ;
#96000 = CARTESIAN_POINT ( 'NONE',  ( 72.10617024684209753, 72.18421392457030095, 4.031754617348218162 ) ) ;
#96001 = CARTESIAN_POINT ( 'NONE',  ( 20.76744934909352125, 17.15404122711133184, 8.090169943749479842 ) ) ;
#96002 = CARTESIAN_POINT ( 'NONE',  ( 162.9703553142854560, 248.3740597985417935, 10.27208824138328680 ) ) ;
#96003 = CARTESIAN_POINT ( 'NONE',  ( 15.38488118375084390, 185.8149278399160949, -9.188101187500095079 ) ) ;
#96004 = CARTESIAN_POINT ( 'NONE',  ( 161.6256441450323678, 250.7031678651938762, 14.48526717260977037 ) ) ;
#96005 = ORIENTED_EDGE ( 'NONE', *, *, #9028, .F. ) ;
#96006 = ORIENTED_EDGE ( 'NONE', *, *, #64559, .F. ) ;
#96007 = CARTESIAN_POINT ( 'NONE',  ( 185.6735584039211346, 258.9728196454306612, -5.407965940105455616 ) ) ;
#96008 = FACE_OUTER_BOUND ( 'NONE', #44306, .T. ) ;
#96009 = CARTESIAN_POINT ( 'NONE',  ( 190.1693911629507738, 301.2639477917662703, -5.112716700269980485 ) ) ;
#96010 = CARTESIAN_POINT ( 'NONE',  ( 193.2375489934525774, 264.0021672994329833, -4.337961694823889047 ) ) ;
#96011 = CARTESIAN_POINT ( 'NONE',  ( 49.54000814145099696, 103.6626726051169527, 10.00000000000000000 ) ) ;
#96012 = CARTESIAN_POINT ( 'NONE',  ( 182.2194435411068412, 284.5217316963779126, 14.88384173871227389 ) ) ;
#96013 = CARTESIAN_POINT ( 'NONE',  ( 167.9188900012335353, 251.8113548967955069, 10.43936956030474406 ) ) ;
#96014 = CARTESIAN_POINT ( 'NONE',  ( 45.77687342386973057, 206.4244531367911293, -4.594050593750046652 ) ) ;
#96015 = CARTESIAN_POINT ( 'NONE',  ( 74.84311135843471163, 224.0177522451419350, 5.000000000000046185 ) ) ;
#96016 = ORIENTED_EDGE ( 'NONE', *, *, #42541, .F. ) ;
#96017 = CARTESIAN_POINT ( 'NONE',  ( 82.28690965751638942, 43.63874554170867270, 8.536804570166234285 ) ) ;
#96018 = B_SPLINE_CURVE_WITH_KNOTS ( 'NONE', 3,
 ( #36192, #90461, #27128, #58010 ),
 .UNSPECIFIED., .F., .F.,
 ( 4, 4 ),
 ( 0.04590184937980493207, 0.04887066958154933499 ),
 .UNSPECIFIED. ) ;
#96019 = CARTESIAN_POINT ( 'NONE',  ( 5.181765596169280563, 27.61866642244642733, -10.00000000000000000 ) ) ;
#96020 = CARTESIAN_POINT ( 'NONE',  ( 3.504529045289348055, 163.6423013555410080, -4.594050593750043987 ) ) ;
#96021 = CARTESIAN_POINT ( 'NONE',  ( 68.72674373419405924, 63.90649084318997097, -12.13465469835461086 ) ) ;
#96022 = CARTESIAN_POINT ( 'NONE',  ( 198.7501991201633018, 286.4015524398827779, -18.58948563601804693 ) ) ;
#96023 = CARTESIAN_POINT ( 'NONE',  ( -24.40473831032599961, 23.22649767201583515, -10.00000000000000000 ) ) ;
#96024 = CARTESIAN_POINT ( 'NONE',  ( 192.8011239859581849, 296.7056528303708660, -11.79847971295421694 ) ) ;
#96025 = AXIS2_PLACEMENT_3D ( 'NONE', #90177, #20752, #28325 ) ;
#96026 = CARTESIAN_POINT ( 'NONE',  ( -13.11024591527734628, 6.000000000000000000, 20.00000000000000000 ) ) ;
#96027 = CARTESIAN_POINT ( 'NONE',  ( 204.9103773355753617, 275.7318107871104189, 13.62808820451859937 ) ) ;
#96028 = CARTESIAN_POINT ( 'NONE',  ( 67.73994666856947333, 221.4637435831424739, 2.679491924311251605 ) ) ;
#96029 = CARTESIAN_POINT ( 'NONE',  ( 164.2723164851102808, 246.1189969011916503, -1.993789335506892302 ) ) ;
#96030 = VERTEX_POINT ( 'NONE', #98263 ) ;
#96031 = CARTESIAN_POINT ( 'NONE',  ( 3.630564096624801174, 166.2365022471902307, 10.00000000000009592 ) ) ;
#96032 = FACE_OUTER_BOUND ( 'NONE', #16207, .T. ) ;
#96033 = VECTOR ( 'NONE', #63092, 1000.000000000000000 ) ;
#96034 = CARTESIAN_POINT ( 'NONE',  ( 117.4133255192225391, 250.8464784336661353, 1.353441290958777327E-15 ) ) ;
#96035 = CARTESIAN_POINT ( 'NONE',  ( 26.36427918851389407, 18.14754757982090894, -5.678558825948276656 ) ) ;
#96036 = CARTESIAN_POINT ( 'NONE',  ( 3.578749241215597010, 161.3262482093458061, 3.021315404115420679E-15 ) ) ;
#96037 = DIRECTION ( 'NONE',  ( -1.000000000000000000, 0.000000000000000000, 1.082076799516502204E-16 ) ) ;
#96038 = VECTOR ( 'NONE', #53716, 1000.000000000000000 ) ;
#96040 = CARTESIAN_POINT ( 'NONE',  ( 185.2961235551778714, 291.2460235572835927, 13.48139818756336616 ) ) ;
#96039 = DIRECTION ( 'NONE',  ( 0.8902628732232650277, -0.4554470513245822971, 0.000000000000000000 ) ) ;
#96041 = CARTESIAN_POINT ( 'NONE',  ( 11.84209618866182190, 52.02562058438156356, 59.99999999999999289 ) ) ;
#96042 = ORIENTED_EDGE ( 'NONE', *, *, #33375, .F. ) ;
#96043 = FACE_OUTER_BOUND ( 'NONE', #46813, .T. ) ;
#96044 = CARTESIAN_POINT ( 'NONE',  ( 149.2765980486851731, 272.0923431290771646, -11.40617906909507973 ) ) ;
#96045 = EDGE_CURVE ( 'NONE', #15205, #20145, #12669, .T. ) ;
#96046 = PLANE ( 'NONE',  #23217 ) ;
#96047 = CARTESIAN_POINT ( 'NONE',  ( 175.1157827236675359, 291.0147020075365276, -1.073647810211864728 ) ) ;
#96048 = CARTESIAN_POINT ( 'NONE',  ( 81.61641279696441131, 55.18026415975641186, -15.91513574126469877 ) ) ;
#96049 = ORIENTED_EDGE ( 'NONE', *, *, #46180, .T. ) ;
#96050 = CARTESIAN_POINT ( 'NONE',  ( 75.38995058909416969, 64.62150842440080112, -14.61153521280294143 ) ) ;
#96051 = DIRECTION ( 'NONE',  ( -0.8660254037844387076, -0.4999999999999998890, -0.000000000000000000 ) ) ;
#96052 = CARTESIAN_POINT ( 'NONE',  ( 168.5384773887906817, 271.6194111364977175, -16.60815838436107228 ) ) ;
#96053 = LINE ( 'NONE', #58000, #97340 ) ;
#96054 = CARTESIAN_POINT ( 'NONE',  ( 48.16808589598787904, 104.3116767361652535, -10.00000000000000000 ) ) ;
#96055 = FACE_OUTER_BOUND ( 'NONE', #31590, .T. ) ;
#96056 = CARTESIAN_POINT ( 'NONE',  ( 148.3005007218871754, 275.7829932922234093, 6.053100225771809839 ) ) ;
#96057 = ORIENTED_EDGE ( 'NONE', *, *, #25118, .T. ) ;
#96058 = CARTESIAN_POINT ( 'NONE',  ( 190.9787802623316395, 280.6762851157768637, 16.68083368884855133 ) ) ;
#96059 = CARTESIAN_POINT ( 'NONE',  ( 12.95333698454457760, 7.288480858562293996, 1.475505719884397138E-15 ) ) ;
#96060 = CARTESIAN_POINT ( 'NONE',  ( 191.8304510568365515, 287.8979185100550922, -15.87805886543832301 ) ) ;
#96061 = ORIENTED_EDGE ( 'NONE', *, *, #85468, .F. ) ;
#96062 = CARTESIAN_POINT ( 'NONE',  ( 78.17252251050902601, 61.73722341659915713, 16.11086890919063919 ) ) ;
#96063 = EDGE_CURVE ( 'NONE', #34200, #69466, #52625, .T. ) ;
#96064 = CARTESIAN_POINT ( 'NONE',  ( 148.3253847707240141, 273.7398928553401447, -9.074433450356286457 ) ) ;
#96065 = CARTESIAN_POINT ( 'NONE',  ( -44.49648453423614569, 28.96346851210257967, -10.00000000000000000 ) ) ;
#96066 = ORIENTED_EDGE ( 'NONE', *, *, #91497, .T. ) ;
#96067 = CARTESIAN_POINT ( 'NONE',  ( 79.19031144066791228, 60.01104784500377320, 16.13641150400241386 ) ) ;
#96068 = CARTESIAN_POINT ( 'NONE',  ( 184.7981748744009565, 292.1161861115109559, 12.46270998733229440 ) ) ;
#96069 = ORIENTED_EDGE ( 'NONE', *, *, #27951, .F. ) ;
#96070 = CARTESIAN_POINT ( 'NONE',  ( 80.33501951744612768, 51.27104759306554627, -14.99191532815999928 ) ) ;
#96071 = CARTESIAN_POINT ( 'NONE',  ( 73.48070833180072725, 69.95435187952867295, -9.683457271946362965 ) ) ;
#96072 = FACE_OUTER_BOUND ( 'NONE', #89476, .T. ) ;
#96073 = ORIENTED_EDGE ( 'NONE', *, *, #97037, .F. ) ;
#96074 = VERTEX_POINT ( 'NONE', #83583 ) ;
#96075 = CARTESIAN_POINT ( 'NONE',  ( 177.7821213501779596, 260.7347052373945075, 12.22434273024177642 ) ) ;
#96076 = ORIENTED_EDGE ( 'NONE', *, *, #34637, .F. ) ;
#96077 = PLANE ( 'NONE',  #57899 ) ;
#96078 = VERTEX_POINT ( 'NONE', #14144 ) ;
#96079 = CARTESIAN_POINT ( 'NONE',  ( 173.0521476969070420, 271.0393772927264422, 16.43803289686445623 ) ) ;
#96080 = CARTESIAN_POINT ( 'NONE',  ( 31.78345146745886751, 98.58241053160183753, 59.99999999999999289 ) ) ;
#96082 = ORIENTED_EDGE ( 'NONE', *, *, #43187, .T. ) ;
#96081 =( BOUNDED_CURVE ( )  B_SPLINE_CURVE ( 2, ( #9953, #1849, #71759, #23615, #32731, #48441, #77341, #69731, #77853, #336, #832, #39310, #93060 ),
 .UNSPECIFIED., .F., .T. ) 
 B_SPLINE_CURVE_WITH_KNOTS ( ( 3, 2, 2, 2, 2, 2, 3 ),
 ( 0.6625000000000000888, 0.6650000000000000355, 0.6700000000000000400, 0.6750000000000000444, 0.6800000000000000488, 0.6850000000000000533, 0.6875000000000000000 ),
 .UNSPECIFIED. ) 
 CURVE ( )  GEOMETRIC_REPRESENTATION_ITEM ( )  RATIONAL_B_SPLINE_CURVE ( ( 0.9755282581475767101, 0.9755282581475772652, 1.000000000000000000, 0.9510565162951535312, 1.000000000000000000, 0.9510565162951535312, 1.000000000000000000, 0.9510565162951535312, 1.000000000000000000, 0.9510565162951535312, 1.000000000000000000, 0.9755282581475768211, 0.9755282581475768211 ) ) 
 REPRESENTATION_ITEM ( '' )  );
#96083 = CARTESIAN_POINT ( 'NONE',  ( 186.0347410764376264, 282.3483404750993486, -16.68897569456403929 ) ) ;
#96084 = CARTESIAN_POINT ( 'NONE',  ( 81.96547941067910870, 41.17040324926905726, 3.814626384468423392 ) ) ;
#96085 = CARTESIAN_POINT ( 'NONE',  ( 151.7906504039364677, 268.6165513190795764, 14.84293751212445756 ) ) ;
#96086 = CARTESIAN_POINT ( 'NONE',  ( 158.6890521156693978, 274.7924871683402444, -13.35768562937069248 ) ) ;
#96087 = CARTESIAN_POINT ( 'NONE',  ( 147.4271219180435253, 275.2957297547342819, -3.800519706258907782 ) ) ;
#96088 = DIRECTION ( 'NONE',  ( 1.000000000000000000, 0.000000000000000000, 0.000000000000000000 ) ) ;
#96089 = LINE ( 'NONE', #97086, #22678 ) ;
#96090 = B_SPLINE_CURVE_WITH_KNOTS ( 'NONE', 3,
 ( #46806, #39674, #47297, #39178 ),
 .UNSPECIFIED., .F., .F.,
 ( 4, 4 ),
 ( 0.01347489213781506538, 0.01986238529349775711 ),
 .UNSPECIFIED. ) ;
#96091 = DIRECTION ( 'NONE',  ( -0.9458118053197299702, 0.3247153044096216523, 0.000000000000000000 ) ) ;
#96092 = CARTESIAN_POINT ( 'NONE',  ( 146.0739611433025686, 245.9548013555409796, -4.594050593750042211 ) ) ;
#96093 = CARTESIAN_POINT ( 'NONE',  ( 75.43135263623493358, 53.72653608919682711, 16.05972988992205686 ) ) ;
#96094 = ORIENTED_EDGE ( 'NONE', *, *, #82293, .T. ) ;
#96095 = CLOSED_SHELL ( 'NONE', ( #95997, #13969, #92312, #54742, #8921, #3780, #67974, #92518, #46291, #89425, #86061, #91245, #44052, #74986, #92542, #69015, #47458, #42489, #27470, #26187, #58736, #38966, #55772, #28210, #12592, #80328, #70318, #20088, #88910, #88366, #23517, #29118, #39972, #90127, #68391, #44494, #17819, #3901, #17026, #92092, #99281, #65310, #23883, #86947, #11105, #55452, #12785, #65068, #74911, #41731, #40014, #14112, #23645, #49131, #48581, #51403, #46388, #88946, #25051, #37149, #8072, #12017, #37460, #16864, #98131, #33764, #46628, #35027, #52072, #63407, #23980, #57717, #46171, #75933, #42805, #54342, #97144, #96779, #18467, #42926, #55535, #14287, #71707, #23893, #96877, #85248, #34921, #74152, #94709, #76885, #13296, #65864, #83631, #76530, #22792, #26019, #82048, #18816, #10150, #89145, #43322, #60936, #6516, #84063, #5359, #75388, #37019, #82744, #61630, #79731, #92867, #4550, #64284, #55755, #83556, #42074, #95927, #93828, #69533, #36111, #96162, #38267, #73814, #78932, #70662, #18842, #76251, #19492, #26442, #2705, #63876, #68542, #91460, #82748, #31976, #41116, #82010, #35441, #65376, #89798, #42312, #21474, #84944, #7396, #60294, #83503, #48326, #24171, #78183, #53016, #12559, #67814, #74726, #23733, #89074, #20587, #8235, #67053, #43097, #65795, #16580, #46982, #59178, #56691, #51455, #44125, #54070, #8232, #14943, #85108, #47494, #60351, #21944, #58971, #53614, #83254, #80543, #5497, #80082, #59108, #68761, #89154, #16990, #72200, #82124, #54000, #23133, #70411, #53820, #58558, #89098, #31842, #5476, #27214, #37446, #98224, #34520, #61632, #3042, #16431, #16181, #15586, #29001, #27708, #27123, #69797, #2760, #67557, #24440, #43640, #33930, #86993, #6727, #85729, #60867, #68924, #74908, #75225, #52029, #93243, #86800, #66438, #99037, #21948, #76654, #54750, #15836, #40332, #33136, #2409, #6340, #43506, #74804, #26447, #94719, #94592, #71310, #42861, #16342, #91886, #99392, #7480, #53668, #20651, #877, #82932, #37938, #26389, #99800, #40656, #60473, #33721, #40405, #85000, #65818, #52743, #52804, #57292, #80078, #67507, #67944, #99603, #41555, #796, #84635, #39318, #73029, #33255, #51515, #72854, #37135, #64740, #54625, #20131, #5988, #52574, #95023, #34087, #10115, #33168, #3960, #66411, #58655, #49562, #13364, #31207, #8465, #49014, #73294, #63798, #27055, #24429, #67715, #60184, #3529, #70473, #1754, #65189, #12835, #96929, #60566, #91295, #99266, #8118, #56604, #29786, #62262, #49729, #38138, #16922, #66502, #65173, #96870, #36626, #22665, #73149, #52375, #51381, #62059, #5391, #92747, #9496, #6011, #36007, #59299, #81553, #29710, #67788, #83423, #38213, #19595, #95608, #98109, #36126, #41141, #67632, #72407, #65633, #7405, #24636, #53466, #52481, #78906, #14837, #52648, #59807, #84756, #72003, #14516, #98710, #48236, #20545, #61440, #41284, #56022, #5790, #27740, #25830, #66529, #12597, #89365, #16105, #58544, #4912, #62733, #10191, #99977, #3112, #8733, #34515, #84010, #3612, #92327, #21289, #40213, #78249, #71441, #9568, #81313, #35123, #44319, #84783, #58394, #30074, #20718, #33426, #94381, #22730, #43445, #60361, #45705, #61591, #52878, #15447, #73266, #51062, #39974, #3896, #21218, #68490, #50079, #69720, #79535, #627, #72786, #98717, #19794, #95372, #92390, #19068, #19561, #61376, #60305, #30774, #63234, #3099, #68456, #210, #49630, #64794, #20248, #60567, #87688, #2073, #73583, #26707, #4501, #96301, #63221, #78304, #56980, #81914, #40910, #92214, #87578, #99934, #22036, #20270, #62940, #63518, #18278, #51926, #86924, #61332, #99607, #69756, #89749, #76297, #93209, #94550, #78792, #47347, #83239, #77926, #41685, #52461, #74679, #86523, #40219, #81355, #28250, #5130, #73998, #7080, #24252, #75157, #56132, #18605, #46577, #16799, #15329, #41162, #24107, #71130, #15767, #18032, #51585, #75854, #4329, #13289, #100179, #5826, #71499, #18013, #40097, #32488, #84664, #15726, #13597 ) ) ;
#96097 = VERTEX_POINT ( 'NONE', #36431 ) ;
#96096 = CARTESIAN_POINT ( 'NONE',  ( 200.0667980463371407, 270.2277230917726456, 9.267277343170334802 ) ) ;
#96098 = CARTESIAN_POINT ( 'NONE',  ( 78.47445242937311605, 48.02372130040763665, -14.00813393920220662 ) ) ;
#96099 = CARTESIAN_POINT ( 'NONE',  ( 76.23413744742458675, 64.83205629739494213, -14.34075561390215015 ) ) ;
#96100 = CARTESIAN_POINT ( 'NONE',  ( 157.4904714317286221, 280.4337344728688208, -7.062405996491910365 ) ) ;
#96101 = CARTESIAN_POINT ( 'NONE',  ( 165.4809825843558144, 246.8843404400683426, -1.876936066672490133 ) ) ;
#96102 =( BOUNDED_CURVE ( )  B_SPLINE_CURVE ( 2, ( #62367, #84731, #78103, #93325, #23878, #86248, #16786, #63391, #17286, #15271, #7690, #71012, #9194 ),
 .UNSPECIFIED., .F., .T. ) 
 B_SPLINE_CURVE_WITH_KNOTS ( ( 3, 2, 2, 2, 2, 2, 3 ),
 ( 0.6625000000000000888, 0.6650000000000000355, 0.6700000000000000400, 0.6750000000000000444, 0.6800000000000000488, 0.6850000000000000533, 0.6875000000000000000 ),
 .UNSPECIFIED. ) 
 CURVE ( )  GEOMETRIC_REPRESENTATION_ITEM ( )  RATIONAL_B_SPLINE_CURVE ( ( 0.9755282581475767101, 0.9755282581475772652, 1.000000000000000000, 0.9510565162951535312, 1.000000000000000000, 0.9510565162951535312, 1.000000000000000000, 0.9510565162951535312, 1.000000000000000000, 0.9510565162951535312, 1.000000000000000000, 0.9755282581475768211, 0.9755282581475768211 ) ) 
 REPRESENTATION_ITEM ( '' )  );
#96103 = CARTESIAN_POINT ( 'NONE',  ( 173.1647931292061742, 280.9218488979392987, 13.94953713923030492 ) ) ;
#96104 =( GEOMETRIC_REPRESENTATION_CONTEXT ( 3 ) GLOBAL_UNCERTAINTY_ASSIGNED_CONTEXT ( ( #9879 ) ) GLOBAL_UNIT_ASSIGNED_CONTEXT ( ( #84711, #79620, #10184 ) ) REPRESENTATION_CONTEXT ( 'NONE', 'WORKASPACE' ) );
#96105 = CARTESIAN_POINT ( 'NONE',  ( 83.67416965427615594, 41.61942911856458949, 0.1873010706438003881 ) ) ;
#96106 = CARTESIAN_POINT ( 'NONE',  ( 88.18231713977282027, 44.19070851116610754, -1.765747973715714236 ) ) ;
#96107 = ORIENTED_EDGE ( 'NONE', *, *, #16510, .T. ) ;
#96108 = CARTESIAN_POINT ( 'NONE',  ( 196.9526636073363477, 287.5149752765084941, -17.63101726665603053 ) ) ;
#96109 = B_SPLINE_CURVE_WITH_KNOTS ( 'NONE', 3,
 ( #90138, #75922, #68286, #20712, #99207, #5995 ),
 .UNSPECIFIED., .F., .F.,
 ( 4, 2, 4 ),
 ( 0.002220428187929036467, 0.002625085253351148312, 0.003029742318773260158 ),
 .UNSPECIFIED. ) ;
#96110 = CARTESIAN_POINT ( 'NONE',  ( 66.10352841413255476, 68.74164459769689017, 0.05599916294954376816 ) ) ;
#96111 = VERTEX_POINT ( 'NONE', #20260 ) ;
#96112 = FACE_OUTER_BOUND ( 'NONE', #76004, .T. ) ;
#96113 = EDGE_CURVE ( 'NONE', #70676, #58533, #63740, .T. ) ;
#96114 = VECTOR ( 'NONE', #43682, 1000.000000000000000 ) ;
#96115 = CARTESIAN_POINT ( 'NONE',  ( 156.8165751444726368, 276.6223283072765753, 10.15807613942431864 ) ) ;
#96116 = DIRECTION ( 'NONE',  ( 0.3782958374750531316, 0.000000000000000000, 0.9256847516023195555 ) ) ;
#96117 = CARTESIAN_POINT ( 'NONE',  ( 82.19428834490943814, 44.75703489301101712, -9.991791377543423280 ) ) ;
#96118 = CARTESIAN_POINT ( 'NONE',  ( 163.4216610345155800, 247.5923753613567442, 10.58669027323842826 ) ) ;
#96120 = CARTESIAN_POINT ( 'NONE',  ( 88.40933139567989940, 44.00655032011064094, 2.323659332633148722 ) ) ;
#96119 = CARTESIAN_POINT ( 'NONE',  ( -67.91103796225580425, 44.10201266000169795, 10.00000000000000000 ) ) ;
#96121 = DIRECTION ( 'NONE',  ( -0.000000000000000000, -0.000000000000000000, -1.000000000000000000 ) ) ;
#96122 = ORIENTED_EDGE ( 'NONE', *, *, #76284, .T. ) ;
#96123 = B_SPLINE_SURFACE_WITH_KNOTS ( 'NONE', 3, 1, ( 
 ( #70202, #8916 ),
 ( #39292, #9422 ),
 ( #31692, #46916 ),
 ( #39784, #93554 ),
 ( #40297, #71239 ),
 ( #17517, #48423 ),
 ( #71743, #72755 ),
 ( #4307, #33219 ),
 ( #11934, #42790 ),
 ( #87501, #96067 ),
 ( #26625, #81853 ),
 ( #80877, #50904 ),
 ( #3348, #42301 ),
 ( #19046, #73725 ),
 ( #49919, #56513 ),
 ( #2848, #73234 ),
 ( #41808, #34223 ),
 ( #40798, #79866 ),
 ( #33737, #66114 ),
 ( #64629, #41300 ),
 ( #3826, #2336 ),
 ( #81365, #64117 ),
 ( #97063, #35212 ),
 ( #88484, #27634 ),
 ( #58499, #11448 ),
 ( #34709, #65118 ),
 ( #10428, #95068 ),
 ( #80364, #87986 ),
 ( #89472, #25629 ),
 ( #18036, #65610 ),
 ( #10936, #96563 ) ),
 .UNSPECIFIED., .F., .F., .F.,
 ( 4, 3, 3, 3, 3, 3, 3, 3, 3, 3, 4 ),
 ( 2, 2 ),
 ( 0.000000000000000000, 0.1333490885032346807, 0.3007194338854402571, 0.4699862290245250818, 0.5844252810809306142, 0.6686540514502837818, 0.7354980260655518132, 0.8028463152565542549, 0.8633854507757066088, 0.9437142632667097075, 1.000000000000000000 ),
 ( 0.000000000000000000, 1.000000000000000000 ),
 .UNSPECIFIED. ) ;
#96124 = CARTESIAN_POINT ( 'NONE',  ( 72.86930352181153125, 62.14391970216223626, -14.54723569203636124 ) ) ;
#96125 = CARTESIAN_POINT ( 'NONE',  ( 80.01857661193632509, 58.13192459411606450, 16.26806844874244362 ) ) ;
#96126 = CARTESIAN_POINT ( 'NONE',  ( 73.99930017925848347, 65.38118273369227040, -13.31775726196476661 ) ) ;
#96127 = CARTESIAN_POINT ( 'NONE',  ( 153.1973045377566507, 265.3014802884401320, 17.70608187426261892 ) ) ;
#96128 = CARTESIAN_POINT ( 'NONE',  ( 80.93613592876508278, 42.95327845838396286, -9.503115154746584636 ) ) ;
#96129 = CARTESIAN_POINT ( 'NONE',  ( 18.97183685527354413, 49.87166901558443044, 59.99999999999999289 ) ) ;
#96130 = CARTESIAN_POINT ( 'NONE',  ( 162.6774150396764469, 248.8814472377480911, 10.88033986792731689 ) ) ;
#96131 = CARTESIAN_POINT ( 'NONE',  ( 7.915412076110063033, 181.5024278399160949, -9.188101187500093303 ) ) ;
#96132 = CARTESIAN_POINT ( 'NONE',  ( 101.9874215621947258, 235.8149278399160664, 9.188101187500093303 ) ) ;
#96133 = CARTESIAN_POINT ( 'NONE',  ( 155.6569868912636991, 261.0411854816857158, -17.75433477650897984 ) ) ;
#96134 = CARTESIAN_POINT ( 'NONE',  ( 88.02334914385743048, 44.75692394554157261, -4.561185668002573301 ) ) ;
#96135 = CARTESIAN_POINT ( 'NONE',  ( 183.4063344672451024, 294.1939596807018233, -7.811441401943769236 ) ) ;
#96136 = FACE_OUTER_BOUND ( 'NONE', #50896, .T. ) ;
#96137 = CARTESIAN_POINT ( 'NONE',  ( -70.00000000000000000, 20.00000000000000000, -59.99999999999999289 ) ) ;
#96138 = CARTESIAN_POINT ( 'NONE',  ( 160.2180067946362385, 282.7949301045907760, 5.350916848644969193 ) ) ;
#96139 = CARTESIAN_POINT ( 'NONE',  ( 147.6264044922760377, 274.9505622111005323, -8.841872555777701592 ) ) ;
#96140 = CARTESIAN_POINT ( 'NONE',  ( 181.4983227144077205, 291.4050983097472454, 9.327077225370901559 ) ) ;
#96141 = CARTESIAN_POINT ( 'NONE',  ( 205.2888330531426959, 275.0763062558687579, -13.80886464497609722 ) ) ;
#96142 = CARTESIAN_POINT ( 'NONE',  ( 79.18557317608008361, 54.66583532628084896, -15.99631523082424600 ) ) ;
#96143 = CARTESIAN_POINT ( 'NONE',  ( 166.2198113297622797, 253.6686547745754012, -13.40419981475687727 ) ) ;
#96144 = CYLINDRICAL_SURFACE ( 'NONE', #88682, 17.82106496071139645 ) ;
#96145 = CARTESIAN_POINT ( 'NONE',  ( 88.13136219740870558, 215.5643266524159571, -9.188101187500093303 ) ) ;
#96146 = CARTESIAN_POINT ( 'NONE',  ( 207.7296438747196134, 270.8486979012336633, -6.692930657757584001 ) ) ;
#96147 = CARTESIAN_POINT ( 'NONE',  ( -19.65312891409030271, 93.06504152958497400, 10.00000000000000888 ) ) ;
#96148 = CARTESIAN_POINT ( 'NONE',  ( -16.05822657194880421, 102.9833706691409105, 12.64279042072237580 ) ) ;
#96150 = CARTESIAN_POINT ( 'NONE',  ( 199.6559772518980651, 284.8326986953333630, 17.73582247532196021 ) ) ;
#96149 = CARTESIAN_POINT ( 'NONE',  ( 83.65470120645571228, 42.99590864647574051, -7.250413499812092155 ) ) ;
#96151 = CARTESIAN_POINT ( 'NONE',  ( 12.48928228595513801, 188.0177522451419065, 5.000000000000046185 ) ) ;
#96152 = EDGE_CURVE ( 'NONE', #65825, #17797, #66981, .T. ) ;
#96153 = CARTESIAN_POINT ( 'NONE',  ( 33.82173346387272517, 28.03085787977764909, 9.188101187500006262 ) ) ;
#96154 = CARTESIAN_POINT ( 'NONE',  ( 81.52443553237245055, 48.71771659309563063, -14.02210268134143512 ) ) ;
#96155 = CARTESIAN_POINT ( 'NONE',  ( 85.79712387213245961, 46.58647785539236708, -9.836184165120874567 ) ) ;
#96156 = ORIENTED_EDGE ( 'NONE', *, *, #44947, .F. ) ;
#96157 = CARTESIAN_POINT ( 'NONE',  ( 19.08966579672462061, 13.94754757982089188, 5.678558825948272215 ) ) ;
#96158 = CARTESIAN_POINT ( 'NONE',  ( 73.40858323730822121, 219.3149278399160664, 9.188101187500093303 ) ) ;
#96159 = CARTESIAN_POINT ( 'NONE',  ( 169.3506085783429569, 288.1634877583111916, -1.098730409881071068 ) ) ;
#96160 = CARTESIAN_POINT ( 'NONE',  ( 198.2505066714982149, 285.2670451491296149, 0.000000000000000000 ) ) ;
#96161 = CARTESIAN_POINT ( 'NONE',  ( 191.7268773518517548, 288.0406801274909867, -15.82109936370516401 ) ) ;
#96162 = ADVANCED_FACE ( 'NONE', ( #44020 ), #74963, .T. ) ;
#96163 = ORIENTED_EDGE ( 'NONE', *, *, #42407, .F. ) ;
#96164 = CARTESIAN_POINT ( 'NONE',  ( -19.65312891409030271, 93.06504152958497400, 59.99999999999999289 ) ) ;
#96165 = CARTESIAN_POINT ( 'NONE',  ( 191.5191886079283279, 287.3386404407627879, 16.08985289718287959 ) ) ;
#96166 = CARTESIAN_POINT ( 'NONE',  ( 191.6148588865760871, 296.7603242537468873, -11.89382487812838995 ) ) ;
#96167 = CARTESIAN_POINT ( 'NONE',  ( 127.3278592705020742, 250.9865022471903160, 10.00000000000009237 ) ) ;
#96168 = CARTESIAN_POINT ( 'NONE',  ( 205.4103625296683617, 274.8658110279089897, -13.38953657917851814 ) ) ;
#96169 = CARTESIAN_POINT ( 'NONE',  ( 75.06334566771610639, 53.10221114767903572, 16.49884716248028838 ) ) ;
#96170 = ORIENTED_EDGE ( 'NONE', *, *, #72576, .T. ) ;
#96171 = CARTESIAN_POINT ( 'NONE',  ( 165.9356184270984613, 246.2207987049553424, -1.153993396985025566 ) ) ;
#96172 = ORIENTED_EDGE ( 'NONE', *, *, #87841, .F. ) ;
#96173 = CARTESIAN_POINT ( 'NONE',  ( 162.8037981520209314, 248.6625452659484381, 9.809699077002424161 ) ) ;
#96174 = CARTESIAN_POINT ( 'NONE',  ( 41.49446470602975978, 58.46153712902343358, 10.00000000000000000 ) ) ;
#96175 = EDGE_CURVE ( 'NONE', #75021, #98005, #90188, .T. ) ;
#96176 = CARTESIAN_POINT ( 'NONE',  ( 153.4542976351440302, 264.8563551865710224, -17.11782692037292009 ) ) ;
#96177 = ORIENTED_EDGE ( 'NONE', *, *, #34312, .T. ) ;
#96178 = CARTESIAN_POINT ( 'NONE',  ( 77.00525802853118762, 62.90742007320628204, -15.26276671481578973 ) ) ;
#96180 = VERTEX_POINT ( 'NONE', #75457 ) ;
#96179 = AXIS2_PLACEMENT_3D ( 'NONE', #2723, #78213, #71623 ) ;
#96181 = LINE ( 'NONE', #33867, #45781 ) ;
#96182 = CARTESIAN_POINT ( 'NONE',  ( 171.4181495053564106, 290.1579472564245634, 2.469270419063871902 ) ) ;
#96183 = CARTESIAN_POINT ( 'NONE',  ( 158.5653297872535177, 257.5252213299329469, -17.07718443373846640 ) ) ;
#96184 = CARTESIAN_POINT ( 'NONE',  ( 80.25178558894602077, 57.14685393251872370, -16.23521980932009612 ) ) ;
#96185 = ORIENTED_EDGE ( 'NONE', *, *, #58991, .F. ) ;
#96186 = CARTESIAN_POINT ( 'NONE',  ( 107.0484310652165192, 232.6115022471902307, 10.00000000000009592 ) ) ;
#96187 = CARTESIAN_POINT ( 'NONE',  ( 34.79119414172389213, 25.80170272979928470, 7.433330006724137462 ) ) ;
#96188 = CARTESIAN_POINT ( 'NONE',  ( 83.16021335601298858, 48.33887568228013976, -12.68239118580088132 ) ) ;
#96189 = CARTESIAN_POINT ( 'NONE',  ( 105.0000000000000000, -8.000000000000000000, -14.21260523776213347 ) ) ;
#96190 = EDGE_CURVE ( 'NONE', #21282, #934, #97736, .T. ) ;
#96191 = CARTESIAN_POINT ( 'NONE',  ( 84.17092664857760553, 212.7365022471902023, 10.00000000000009948 ) ) ;
#96192 = VERTEX_POINT ( 'NONE', #43020 ) ;
#96193 = ORIENTED_EDGE ( 'NONE', *, *, #19596, .T. ) ;
#96194 = CARTESIAN_POINT ( 'NONE',  ( 198.3080508722109698, 286.5404284581068168, 17.10115148743064850 ) ) ;
#96196 = CARTESIAN_POINT ( 'NONE',  ( 194.9757425430702824, 292.9391030023704161, -15.21392314336593365 ) ) ;
#96195 = CARTESIAN_POINT ( 'NONE',  ( 204.4325665793906524, 276.5594032932251594, 13.33817701435311598 ) ) ;
#96197 = CARTESIAN_POINT ( 'NONE',  ( 85.63218110832043806, 48.66108713908771932, 12.42024371201311972 ) ) ;
#96198 = CARTESIAN_POINT ( 'NONE',  ( 198.2505066714982149, 285.2670451491296149, 0.000000000000000000 ) ) ;
#96199 = DIRECTION ( 'NONE',  ( 0.9171038997749326738, -0.3986482622784278673, 0.000000000000000000 ) ) ;
#96200 = CARTESIAN_POINT ( 'NONE',  ( 187.6200950315515854, 291.3050749031608007, -13.78314674982586396 ) ) ;
#96201 = CARTESIAN_POINT ( 'NONE',  ( 207.3663924633328577, 271.4778678016768936, -4.575037815448358636 ) ) ;
#96202 = CARTESIAN_POINT ( 'NONE',  ( 169.8438327850726637, 267.4680064843133209, 17.16903572500528696 ) ) ;
#96203 = CARTESIAN_POINT ( 'NONE',  ( -71.61465314115659453, 63.06504152958490295, -20.00000000000001776 ) ) ;
#96204 = CARTESIAN_POINT ( 'NONE',  ( 98.19890751640281223, 221.3768266524159856, -9.188101187500091527 ) ) ;
#96205 = VERTEX_POINT ( 'NONE', #51134 ) ;
#96206 = CARTESIAN_POINT ( 'NONE',  ( 74.15479259499207387, 55.62765001666249276, -16.59030973340311022 ) ) ;
#96207 = CARTESIAN_POINT ( 'NONE',  ( 163.7597937213045611, 277.3359689971894682, -14.45435855620203647 ) ) ;
#96208 = ORIENTED_EDGE ( 'NONE', *, *, #28685, .F. ) ;
#96209 = ORIENTED_EDGE ( 'NONE', *, *, #4754, .T. ) ;
#96210 = EDGE_CURVE ( 'NONE', #39719, #14532, #51734, .T. ) ;
#96211 = CARTESIAN_POINT ( 'NONE',  ( 87.15508732983295204, 45.91009000376428872, -8.663677684674611967 ) ) ;
#96212 = CARTESIAN_POINT ( 'NONE',  ( 176.8004942653151943, 292.7834445522077544, -2.779440414855350650 ) ) ;
#96213 = DIRECTION ( 'NONE',  ( -1.000000000000000000, 0.000000000000000000, 0.000000000000000000 ) ) ;
#96214 = CARTESIAN_POINT ( 'NONE',  ( 206.8313602288537538, 272.4045708154811791, -9.607337080360906612 ) ) ;
#96215 = CARTESIAN_POINT ( 'NONE',  ( -19.66077996331566524, 93.20665791313032855, 59.99999999999999289 ) ) ;
#96216 = CARTESIAN_POINT ( 'NONE',  ( 93.32751462011533761, 218.5643266524159856, -9.188101187500093303 ) ) ;
#96217 = EDGE_LOOP ( 'NONE', ( #39747, #86217, #40659, #79512 ) ) ;
#96218 = ADVANCED_FACE ( 'NONE', ( #67338 ), #48314, .F. ) ;
#96219 = CARTESIAN_POINT ( 'NONE',  ( 207.5920568422024814, 271.0870056320159165, -1.586464549033245186 ) ) ;
#96220 = ORIENTED_EDGE ( 'NONE', *, *, #93357, .T. ) ;
#96221 = EDGE_CURVE ( 'NONE', #39284, #74626, #10637, .T. ) ;
#96222 = CARTESIAN_POINT ( 'NONE',  ( 22.77272502854106762, 36.08080186712593473, -3.090169943749475845 ) ) ;
#96223 = LINE ( 'NONE', #68265, #62369 ) ;
#96224 = CARTESIAN_POINT ( 'NONE',  ( 165.0397143271508753, 286.3398299935479940, 1.252190257168839249 ) ) ;
#96226 = CARTESIAN_POINT ( 'NONE',  ( 69.46471525646846601, 62.64179866298621846, -13.84787601622161901 ) ) ;
#96225 = CARTESIAN_POINT ( 'NONE',  ( 132.6770232609233062, 259.6589784336661637, -6.496448406907675876E-16 ) ) ;
#96227 = CARTESIAN_POINT ( 'NONE',  ( -13.49147982757802389, 173.0177522451419350, 5.000000000000046185 ) ) ;
#96228 = PLANE ( 'NONE',  #9197 ) ;
#96229 = ORIENTED_EDGE ( 'NONE', *, *, #60001, .F. ) ;
#96230 = CARTESIAN_POINT ( 'NONE',  ( 204.4735667670548764, 276.4883888850707763, 14.55282211540290227 ) ) ;
#96231 = EDGE_CURVE ( 'NONE', #83200, #55188, #1070, .T. ) ;
#96232 = CARTESIAN_POINT ( 'NONE',  ( 160.7803790444903314, 275.4413384178728847, 13.47929685474721495 ) ) ;
#96233 = CARTESIAN_POINT ( 'NONE',  ( 82.17119170860053146, 40.62002387180137220, -3.389656615904392378 ) ) ;
#96234 = EDGE_CURVE ( 'NONE', #7170, #35723, #96552, .T. ) ;
#96235 = CARTESIAN_POINT ( 'NONE',  ( 189.1451319728309954, 269.5633631987243461, 15.00206811136211549 ) ) ;
#96236 = CARTESIAN_POINT ( 'NONE',  ( 44.26158929084472504, 186.3615022471902023, 5.000000000000051514 ) ) ;
#96237 = LINE ( 'NONE', #81052, #64557 ) ;
#96238 = B_SPLINE_CURVE_WITH_KNOTS ( 'NONE', 3,
 ( #97682, #10572, #73373, #89132, #72387, #97197, #35854, #20174, #3961, #57646, #96202, #72894, #66747, #49555, #51041, #2997, #81999, #19683, #81501, #28248, #11580, #42927, #73866, #59123, #41958, #34843, #88622, #18169, #42438, #80003, #49070, #41447, #33887, #64773, #95721, #26270, #57145, #80508, #18674, #11082, #3485, #34360, #83995, #22650, #44440, #37337, #30247, #53535, #68738, #59635, #99163, #76369 ),
 .UNSPECIFIED., .F., .F.,
 ( 4, 2, 2, 2, 2, 2, 2, 2, 2, 2, 2, 2, 2, 2, 2, 2, 2, 2, 2, 2, 2, 2, 2, 2, 2, 4 ),
 ( 0.001642988356310917143, 0.002095883426664464384, 0.002548778497018011190, 0.002775226032194823625, 0.002888449799783281667, 0.003001673567371739276, 0.003228121102548607221, 0.003454568637725474733, 0.003907463708079213227, 0.004360358778432952588, 0.005266148919140437382, 0.006171939059847923043, 0.006624834130201743936, 0.007077729200555563961, 0.007190952968144056698, 0.007247564851938301765, 0.007304176735732547700, 0.007360788619526793634, 0.007417400503321038702, 0.007530624270909660675, 0.007757071806087032124, 0.007983519341264403574, 0.008209966876441775890, 0.008436414411619144738, 0.008662861946796517054, 0.008889309481973889371 ),
 .UNSPECIFIED. ) ;
#96239 = CIRCLE ( 'NONE', #26636, 16.82106496071145685 ) ;
#96240 = DIRECTION ( 'NONE',  ( -0.8660254037844387076, -0.4999999999999998890, -0.000000000000000000 ) ) ;
#96241 = CARTESIAN_POINT ( 'NONE',  ( -66.43946475426807297, 58.88062878445797566, 59.99999999999999289 ) ) ;
#96242 = CARTESIAN_POINT ( 'NONE',  ( 80.31687802057754766, 51.50889260389730140, 15.08045506871916608 ) ) ;
#96243 = CARTESIAN_POINT ( 'NONE',  ( 67.93311001602360477, 69.70947576764457665, -1.762602472474833926 ) ) ;
#96244 = CARTESIAN_POINT ( 'NONE',  ( 167.6093229551651689, 249.9473136708200229, 7.507881343133518293 ) ) ;
#96245 = CARTESIAN_POINT ( 'NONE',  ( 78.26458253827964029, 61.66843869688886315, 16.13698506349214412 ) ) ;
#96246 = CARTESIAN_POINT ( 'NONE',  ( 162.6262389125959373, 248.9700868899859074, -10.50380342094597808 ) ) ;
#96247 = CARTESIAN_POINT ( 'NONE',  ( 163.1438579415164156, 248.0735444329312713, -11.47272517958888116 ) ) ;
#96248 = VECTOR ( 'NONE', #15907, 1000.000000000000000 ) ;
#96249 = CARTESIAN_POINT ( 'NONE',  ( 71.79577640164012564, 64.60757656470461541, -12.94397184867940176 ) ) ;
#96250 = CARTESIAN_POINT ( 'NONE',  ( 183.1835119402560963, 265.1834291825128389, 13.30006602047987130 ) ) ;
#96251 = CARTESIAN_POINT ( 'NONE',  ( 68.76057960370418698, 222.0530062829863027, -4.648177544792955347E-16 ) ) ;
#96252 = CARTESIAN_POINT ( 'NONE',  ( 36.35590661721340666, 26.15404122711136026, 8.090169943749479842 ) ) ;
#96253 = DIRECTION ( 'NONE',  ( -2.168404344971022180E-16, 3.755786496842918286E-16, 1.000000000000000000 ) ) ;
#96254 = CARTESIAN_POINT ( 'NONE',  ( 80.00798602660123038, 150.6044130683315814, 4.041334437186263538E-16 ) ) ;
#96255 = CARTESIAN_POINT ( 'NONE',  ( 158.2435942055431326, 271.3764418995982055, -14.70623264937866637 ) ) ;
#96256 = CARTESIAN_POINT ( 'NONE',  ( 85.74962510757818279, 43.49686255595008078, -4.555259895190277852 ) ) ;
#96257 = CARTESIAN_POINT ( 'NONE',  ( 16.08835327644320401, 192.3464784336661637, 1.353441290958777327E-15 ) ) ;
#96258 = CARTESIAN_POINT ( 'NONE',  ( 82.57639827720844039, 49.19050994824535650, 13.45810755646198409 ) ) ;
#96259 = ORIENTED_EDGE ( 'NONE', *, *, #52189, .T. ) ;
#96260 = CARTESIAN_POINT ( 'NONE',  ( 86.84204249716189850, 45.92435628226732547, 8.934002094794735171 ) ) ;
#96261 = CARTESIAN_POINT ( 'NONE',  ( 25.96864935082048831, 154.0458036431183189, 30.52142883766506998 ) ) ;
#96262 = CARTESIAN_POINT ( 'NONE',  ( 82.03687330897646746, 41.20536659497016529, 5.461263348486533609 ) ) ;
#96263 = CARTESIAN_POINT ( 'NONE',  ( 35.49282175392953320, 200.4869531367911293, 4.594050593750046652 ) ) ;
#96265 = ADVANCED_FACE ( 'NONE', ( #41937 ), #72872, .T. ) ;
#96264 = CIRCLE ( 'NONE', #50959, 17.82106496071138935 ) ;
#96266 = CARTESIAN_POINT ( 'NONE',  ( 86.96880057233924788, 46.02321981727299516, 8.968744825131210519 ) ) ;
#96267 = CARTESIAN_POINT ( 'NONE',  ( 147.5693121967435957, 275.0494489676833041, 4.210973343677100189 ) ) ;
#96268 = CARTESIAN_POINT ( 'NONE',  ( 34.71711421221060334, 41.81751292744059612, -6.180339887498951690 ) ) ;
#96269 = CARTESIAN_POINT ( 'NONE',  ( 179.7950818681164833, 292.4219657804791836, 6.105251856334193761 ) ) ;
#96270 = CARTESIAN_POINT ( 'NONE',  ( 147.0276296945837373, 275.9876705829954062, 0.7617065417431535534 ) ) ;
#96271 = LINE ( 'NONE', #81568, #97541 ) ;
#96272 = FACE_OUTER_BOUND ( 'NONE', #21674, .T. ) ;
#96273 = CARTESIAN_POINT ( 'NONE',  ( 166.9910584687719108, 257.7488603398688838, -15.68734378694487752 ) ) ;
#96274 = EDGE_CURVE ( 'NONE', #54157, #55257, #43059, .T. ) ;
#96275 = DIRECTION ( 'NONE',  ( 0.000000000000000000, 0.000000000000000000, 1.000000000000000000 ) ) ;
#96276 = CARTESIAN_POINT ( 'NONE',  ( 82.36670705735998865, 218.3615022471902591, -10.00000000000009592 ) ) ;
#96277 = DIRECTION ( 'NONE',  ( 0.8902628732232650277, -0.4554470513245822971, 0.000000000000000000 ) ) ;
#96278 = CARTESIAN_POINT ( 'NONE',  ( 187.1412927779018673, 261.9835105880691231, -10.20549468610707322 ) ) ;
#96279 = CARTESIAN_POINT ( 'NONE',  ( 49.94514132322986910, 190.4548013555409796, -4.594050593750042211 ) ) ;
#96280 = ORIENTED_EDGE ( 'NONE', *, *, #56808, .T. ) ;
#96281 = CARTESIAN_POINT ( 'NONE',  ( 162.7713784074331329, 263.3385562889519065, 17.72620173005347866 ) ) ;
#96282 = FACE_OUTER_BOUND ( 'NONE', #97557, .T. ) ;
#96283 = ADVANCED_FACE ( 'NONE', ( #66728 ), #20091, .F. ) ;
#96284 = CARTESIAN_POINT ( 'NONE',  ( 67.27543762298243735, 66.59126356583220741, -8.544430691054564875 ) ) ;
#96285 = ORIENTED_EDGE ( 'NONE', *, *, #97417, .F. ) ;
#96286 = CARTESIAN_POINT ( 'NONE',  ( 168.0515290973648632, 286.0491048284131921, 8.058232580181940108 ) ) ;
#96287 = DIRECTION ( 'NONE',  ( -1.000000000000000000, 0.000000000000000000, 0.000000000000000000 ) ) ;
#96288 = DIRECTION ( 'NONE',  ( -0.8660254037844387076, -0.4999999999999998890, -0.000000000000000000 ) ) ;
#96289 = CARTESIAN_POINT ( 'NONE',  ( 28.99364183777449000, 25.24335787977764767, -9.188101187500008038 ) ) ;
#96290 = CARTESIAN_POINT ( 'NONE',  ( 186.1724765274662730, 262.9988875480885895, 11.43256481527857105 ) ) ;
#96291 = CARTESIAN_POINT ( 'NONE',  ( 196.3507576896697344, 290.5575069072837664, -17.68249398312240928 ) ) ;
#96292 = CARTESIAN_POINT ( 'NONE',  ( -71.61465314115659453, 63.06504152958490295, 40.00000000000000000 ) ) ;
#96293 = ORIENTED_EDGE ( 'NONE', *, *, #73411, .T. ) ;
#96294 = CARTESIAN_POINT ( 'NONE',  ( 12.79778405566451482, 30.49540643055186351, 3.479690158560446702E-15 ) ) ;
#96295 = CARTESIAN_POINT ( 'NONE',  ( -19.65312891409030271, 93.06504152958497400, 177.5919119679930134 ) ) ;
#96296 = CARTESIAN_POINT ( 'NONE',  ( 171.6600481915988041, 252.6781227079003997, 8.579917601003849370 ) ) ;
#96297 = EDGE_CURVE ( 'NONE', #9798, #14868, #68716, .T. ) ;
#96298 = ORIENTED_EDGE ( 'NONE', *, *, #5153, .F. ) ;
#96299 = CARTESIAN_POINT ( 'NONE',  ( -19.65312891409030271, 93.06504152958497400, 10.00000000000000888 ) ) ;
#96300 = CARTESIAN_POINT ( 'NONE',  ( 150.6790040019602088, 269.6633047651677089, 15.38315204620803378 ) ) ;
#96301 = ADVANCED_FACE ( 'NONE', ( #99140 ), #52518, .F. ) ;
#96302 = CARTESIAN_POINT ( 'NONE',  ( 177.3188500945199166, 256.0766865477347665, -7.229946009214981650 ) ) ;
#96303 = CARTESIAN_POINT ( 'NONE',  ( 167.9508935690271016, 247.1955620634513480, 0.2374292289661225908 ) ) ;
#96304 = AXIS2_PLACEMENT_3D ( 'NONE', #52915, #83867, #6326 ) ;
#96305 = B_SPLINE_CURVE_WITH_KNOTS ( 'NONE', 3,
 ( #43951, #74890, #37844, #90622 ),
 .UNSPECIFIED., .F., .F.,
 ( 4, 4 ),
 ( 0.006895705269663468875, 0.01263911957245467989 ),
 .UNSPECIFIED. ) ;
#96306 = EDGE_LOOP ( 'NONE', ( #95038, #58212, #56556, #96076 ) ) ;
#96307 = ORIENTED_EDGE ( 'NONE', *, *, #11654, .F. ) ;
#96309 = CARTESIAN_POINT ( 'NONE',  ( 150.9428143250784728, 269.7061216501884928, -13.70542669507604394 ) ) ;
#96308 = CARTESIAN_POINT ( 'NONE',  ( 161.8882824960653579, 250.2482648971885340, -13.83574485983625557 ) ) ;
#96310 = CARTESIAN_POINT ( 'NONE',  ( 196.2293283710122012, 290.7678286567270902, -17.07152402978540096 ) ) ;
#96311 = ORIENTED_EDGE ( 'NONE', *, *, #91965, .F. ) ;
#96312 = CARTESIAN_POINT ( 'NONE',  ( 66.09342489060131243, 68.50075773664546830, -2.578996081064114598 ) ) ;
#96313 = CARTESIAN_POINT ( 'NONE',  ( 169.5727729373952002, 284.0798650663272156, -11.84966624384599676 ) ) ;
#96314 = CARTESIAN_POINT ( 'NONE',  ( 72.65506221629649986, 57.10929429594364137, -16.37270640794472598 ) ) ;
#96315 = CARTESIAN_POINT ( 'NONE',  ( 78.06091359999885526, 61.03177674231440619, -15.89086307328630276 ) ) ;
#96316 = CARTESIAN_POINT ( 'NONE',  ( 205.2941531242069857, 275.0670916224857478, -13.92605142593109058 ) ) ;
#96318 = CARTESIAN_POINT ( 'NONE',  ( 110.6480226958041158, 228.5643266524160708, 9.188101187500095079 ) ) ;
#96317 = VECTOR ( 'NONE', #37051, 1000.000000000000000 ) ;
#96319 = B_SPLINE_CURVE_WITH_KNOTS ( 'NONE', 3,
 ( #82356, #60469, #98519, #14400 ),
 .UNSPECIFIED., .F., .F.,
 ( 4, 4 ),
 ( 7.881068500304280180E-17, 0.001344325176028971728 ),
 .UNSPECIFIED. ) ;
#96320 = DIRECTION ( 'NONE',  ( 0.000000000000000000, 0.000000000000000000, -1.000000000000000000 ) ) ;
#96321 = ORIENTED_EDGE ( 'NONE', *, *, #39740, .F. ) ;
#96322 = CARTESIAN_POINT ( 'NONE',  ( 163.7085541710205234, 247.0954618725873217, -6.713544974106887331 ) ) ;
#96323 = VERTEX_POINT ( 'NONE', #85472 ) ;
#96324 = CARTESIAN_POINT ( 'NONE',  ( 36.96107555259132482, 29.84335787977765619, 9.188101187500006262 ) ) ;
#96325 = FACE_BOUND ( 'NONE', #91463, .T. ) ;
#96326 = CARTESIAN_POINT ( 'NONE',  ( 78.17699230315889736, 47.82979171855502187, -13.99723441571071980 ) ) ;
#96327 = CARTESIAN_POINT ( 'NONE',  ( 62.85372508080288867, 219.3464784336661637, 1.353441290958777525E-15 ) ) ;
#96328 = DIRECTION ( 'NONE',  ( 0.5000000000000014433, -0.8660254037844379305, 0.000000000000000000 ) ) ;
#96329 = CARTESIAN_POINT ( 'NONE',  ( 191.0900422946452011, 299.6693332556258724, 8.872191398975367349 ) ) ;
#96330 = CARTESIAN_POINT ( 'NONE',  ( 151.0438343122359584, 269.0314001316289705, 14.41873139571475626 ) ) ;
#96331 = CARTESIAN_POINT ( 'NONE',  ( 175.8442789310321928, 278.0726236853578257, 16.35466010686542404 ) ) ;
#96332 = ORIENTED_EDGE ( 'NONE', *, *, #27783, .F. ) ;
#96333 = EDGE_CURVE ( 'NONE', #14660, #29175, #99640, .T. ) ;
#96334 = DIRECTION ( 'NONE',  ( -0.4635919272833941562, 0.8029647720336182681, 0.3746065934159032440 ) ) ;
#96335 = CARTESIAN_POINT ( 'NONE',  ( 87.53652538659707716, 43.81626475740009141, -1.345572693404142983 ) ) ;
#96336 = CARTESIAN_POINT ( 'NONE',  ( 87.49661283931372679, 43.54010870773999642, 2.689214756758103508 ) ) ;
#96337 = ORIENTED_EDGE ( 'NONE', *, *, #35737, .T. ) ;
#96338 = CARTESIAN_POINT ( 'NONE',  ( 73.43762515466688967, 73.52662068827324049, 2.033788753608857291E-15 ) ) ;
#96339 = DIRECTION ( 'NONE',  ( 5.984665299743594308E-16, 0.000000000000000000, 1.000000000000000000 ) ) ;
#96340 = DIRECTION ( 'NONE',  ( -0.8660254037844377084, -0.5000000000000014433, -0.000000000000000000 ) ) ;
#96341 = CARTESIAN_POINT ( 'NONE',  ( 74.57247842330004062, 213.8615022471902591, -10.00000000000009592 ) ) ;
#96342 = EDGE_CURVE ( 'NONE', #24856, #5719, #70233, .T. ) ;
#96343 = CARTESIAN_POINT ( 'NONE',  ( 190.7516742497373059, 300.2554039010641418, 4.342609251298632067 ) ) ;
#96344 = CARTESIAN_POINT ( 'NONE',  ( 205.7668501412109663, 274.2483563724483133, 11.09689540819876896 ) ) ;
#96345 = CARTESIAN_POINT ( 'NONE',  ( 206.4943150373521803, 272.9883502116088039, 11.34100825923693101 ) ) ;
#96346 = DIRECTION ( 'NONE',  ( -0.8660254037844387076, -0.4999999999999998890, -0.000000000000000000 ) ) ;
#96347 = CARTESIAN_POINT ( 'NONE',  ( 164.1280364607038393, 254.0203960612020921, 14.38687283228996350 ) ) ;
#96348 = LINE ( 'NONE', #20822, #46408 ) ;
#96349 = B_SPLINE_CURVE_WITH_KNOTS ( 'NONE', 3,
 ( #4852, #13450, #59507, #44315 ),
 .UNSPECIFIED., .F., .F.,
 ( 4, 4 ),
 ( 0.04668517186442352335, 0.04887066958154938356 ),
 .UNSPECIFIED. ) ;
#96350 = EDGE_CURVE ( 'NONE', #44309, #85762, #23105, .T. ) ;
#96351 = CARTESIAN_POINT ( 'NONE',  ( 120.0114017305758551, 252.3464784336661353, 1.353441290958777327E-15 ) ) ;
#96352 = VERTEX_POINT ( 'NONE', #15500 ) ;
#96353 = CARTESIAN_POINT ( 'NONE',  ( 146.5502055023624735, 276.8145935406849389, 0.3770461397900869427 ) ) ;
#96354 = DIRECTION ( 'NONE',  ( 0.5000000000000048850, -0.8660254037844358210, 0.000000000000000000 ) ) ;
#96355 = DIRECTION ( 'NONE',  ( 0.000000000000000000, 0.000000000000000000, 1.000000000000000000 ) ) ;
#96356 = B_SPLINE_CURVE_WITH_KNOTS ( 'NONE', 3,
 ( #48378, #53949, #84905, #268 ),
 .UNSPECIFIED., .F., .F.,
 ( 4, 4 ),
 ( 0.01288686481989116672, 0.01922162384058315882 ),
 .UNSPECIFIED. ) ;
#96357 = CARTESIAN_POINT ( 'NONE',  ( 164.4761815919938215, 245.7658921781788592, 6.833796894895563412 ) ) ;
#96358 = CARTESIAN_POINT ( 'NONE',  ( 75.06845965858576619, 62.64932666483513657, 14.91362258529271756 ) ) ;
#96359 = DIRECTION ( 'NONE',  ( -1.000000000000000000, 0.000000000000000000, 0.000000000000000000 ) ) ;
#96360 = ORIENTED_EDGE ( 'NONE', *, *, #62298, .F. ) ;
#96361 = CARTESIAN_POINT ( 'NONE',  ( 103.4423036115607601, 218.9824982072973967, 3.021315404115420679E-15 ) ) ;
#96362 = CARTESIAN_POINT ( 'NONE',  ( 158.5080245674752177, 275.0720563644080130, -12.47040154529214817 ) ) ;
#96364 = CARTESIAN_POINT ( 'NONE',  ( 206.9960295002423436, 269.8401794964582905, 1.771342953264500197 ) ) ;
#96363 = CARTESIAN_POINT ( 'NONE',  ( 147.8791740781505837, 276.5127524457575987, 2.771564245682613947 ) ) ;
#96365 = CARTESIAN_POINT ( 'NONE',  ( 164.2901811315512077, 246.0880544258967575, -1.801919852217561235 ) ) ;
#96366 = CARTESIAN_POINT ( 'NONE',  ( 147.5623555321158165, 249.8768266524159856, -9.188101187500093303 ) ) ;
#96367 = CARTESIAN_POINT ( 'NONE',  ( 146.9324727656309335, 276.1524872186338371, 3.813717745456558728 ) ) ;
#96368 = CARTESIAN_POINT ( 'NONE',  ( 157.3305006125302441, 282.1378183958786963, 1.589776369934247979 ) ) ;
#96369 = CARTESIAN_POINT ( 'NONE',  ( 191.2649737798357705, 297.3663430354321235, 11.06343876070684296 ) ) ;
#96370 = CARTESIAN_POINT ( 'NONE',  ( 24.48906155743269508, 15.10801979619929014, 3.090169943749476733 ) ) ;
#96371 = CARTESIAN_POINT ( 'NONE',  ( 190.7705347155322499, 300.2227366160529414, 3.504769718465625239 ) ) ;
#96372 = CARTESIAN_POINT ( 'NONE',  ( 155.2699163265236280, 279.6096657672135279, -1.575243086752120325 ) ) ;
#96373 = CARTESIAN_POINT ( 'NONE',  ( 172.4925392983816153, 287.4467975273285560, -8.192266032599757608 ) ) ;
#96374 = VECTOR ( 'NONE', #44054, 1000.000000000000000 ) ;
#96375 = CARTESIAN_POINT ( 'NONE',  ( 203.3041373168503299, 278.5139001086923827, -16.61929732091214973 ) ) ;
#96376 = CARTESIAN_POINT ( 'NONE',  ( 157.0827652098068654, 271.8075571977315121, -14.85186543366582335 ) ) ;
#96377 =( BOUNDED_CURVE ( )  B_SPLINE_CURVE ( 2, ( #66555, #36638, #74685, #67044, #60424, #93248, #15701, #8125, #97968 ),
 .UNSPECIFIED., .F., .T. ) 
 B_SPLINE_CURVE_WITH_KNOTS ( ( 3, 2, 2, 2, 3 ),
 ( 0.4798387096774193727, 0.4811827956989247479, 0.4838709677419354982, 0.4865591397849462485, 0.4879032258064516236 ),
 .UNSPECIFIED. ) 
 CURVE ( )  GEOMETRIC_REPRESENTATION_ITEM ( )  RATIONAL_B_SPLINE_CURVE ( ( 0.9330127018922194093, 0.9330127018922194093, 1.000000000000000000, 0.8660254037844387076, 1.000000000000000000, 0.8660254037844387076, 1.000000000000000000, 0.9330127018922194093, 0.9330127018922194093 ) ) 
 REPRESENTATION_ITEM ( '' )  );
#96378 = CARTESIAN_POINT ( 'NONE',  ( 127.5984922056368163, 251.1427522451419634, -10.00000000000009415 ) ) ;
#96379 = CARTESIAN_POINT ( 'NONE',  ( 79.91325939341504636, 52.13032348250509784, -15.32992361654147828 ) ) ;
#96380 = ORIENTED_EDGE ( 'NONE', *, *, #97480, .F. ) ;
#96381 = EDGE_CURVE ( 'NONE', #92554, #98025, #93044, .T. ) ;
#96382 = VECTOR ( 'NONE', #89561, 1000.000000000000000 ) ;
#96383 = CARTESIAN_POINT ( 'NONE',  ( 196.1573359623355088, 290.8925231663144473, 17.55680092534192482 ) ) ;
#96384 = CARTESIAN_POINT ( 'NONE',  ( 148.0427192501136062, 274.2294838985851015, 9.385226820296049155 ) ) ;
#96385 = CARTESIAN_POINT ( 'NONE',  ( 1.691375130056927301, 159.5327760586659451, 1.948934522072302763E-15 ) ) ;
#96386 = CARTESIAN_POINT ( 'NONE',  ( 34.27488675591641965, 202.8464784336661353, 1.353441290958777327E-15 ) ) ;
#96387 = CARTESIAN_POINT ( 'NONE',  ( 175.4807071158155054, 256.8036674190846043, -10.68012024109663827 ) ) ;
#96388 = CARTESIAN_POINT ( 'NONE',  ( 18.79197634579341525, 22.80066082961421614, 10.00000000000000533 ) ) ;
#96389 = FACE_OUTER_BOUND ( 'NONE', #22263, .T. ) ;
#96390 = CARTESIAN_POINT ( 'NONE',  ( 157.8820657059571033, 257.1872359237914338, -17.60412210594719440 ) ) ;
#96391 = CARTESIAN_POINT ( 'NONE',  ( 188.8632942670357693, 290.4480958481585731, -14.71172498564733644 ) ) ;
#96392 = CARTESIAN_POINT ( 'NONE',  ( 190.1607982559816890, 301.2788311432216233, -4.972636536415983244 ) ) ;
#96393 = B_SPLINE_CURVE_WITH_KNOTS ( 'NONE', 3,
 ( #40937, #71881, #9583, #56658 ),
 .UNSPECIFIED., .F., .F.,
 ( 4, 4 ),
 ( 0.01101634049414615402, 0.01680390332395608269 ),
 .UNSPECIFIED. ) ;
#96394 = CARTESIAN_POINT ( 'NONE',  ( 73.87485074719697309, 55.34240436449581324, -16.11747225289941099 ) ) ;
#96395 = CARTESIAN_POINT ( 'NONE',  ( 171.2371238201655217, 258.3827728951262657, 14.06634987601701425 ) ) ;
#96396 = CARTESIAN_POINT ( 'NONE',  ( 200.4906113350036776, 281.3870700576555919, -17.24871243658977704 ) ) ;
#96397 = CARTESIAN_POINT ( 'NONE',  ( 205.0994677818405023, 275.4042965269534307, -14.14519517703424789 ) ) ;
#96398 = CARTESIAN_POINT ( 'NONE',  ( 162.2030298726479884, 251.9395672944197315, -14.03258911121123553 ) ) ;
#96399 = CARTESIAN_POINT ( 'NONE',  ( 34.30229714732359980, 200.6115022471903160, -5.000000000000047962 ) ) ;
#96400 = LINE ( 'NONE', #34558, #57131 ) ;
#96401 = CARTESIAN_POINT ( 'NONE',  ( -19.65312891409030271, 93.06504152958497400, 10.00000000000000888 ) ) ;
#96402 = CARTESIAN_POINT ( 'NONE',  ( 1.204062292545672097, 165.3768266524159856, 9.188101187500098632 ) ) ;
#96403 = CARTESIAN_POINT ( 'NONE',  ( 31.19238438139944947, 38.98502408145593989, -5.678558825948271327 ) ) ;
#96404 = CARTESIAN_POINT ( 'NONE',  ( -22.42236680055709641, 157.8615022471902591, 0.000000000000000000 ) ) ;
#96405 = CARTESIAN_POINT ( 'NONE',  ( 192.5254593562406171, 297.1831179748913314, 11.00703791256144015 ) ) ;
#96406 = CARTESIAN_POINT ( 'NONE',  ( 40.59535201087842182, 25.29860640527295601, -2.839279412974138328 ) ) ;
#96407 = CARTESIAN_POINT ( 'NONE',  ( 75.30212449506053929, 225.8297689869268652, -2.679491924311252493 ) ) ;
#96408 = EDGE_CURVE ( 'NONE', #48903, #10254, #46402, .T. ) ;
#96409 = CARTESIAN_POINT ( 'NONE',  ( 179.5755015609138354, 277.2059287606015801, 16.35061197133128275 ) ) ;
#96410 = CARTESIAN_POINT ( 'NONE',  ( 81.03765089968891289, 43.40990969291960511, -9.978953348122514555 ) ) ;
#96411 = CARTESIAN_POINT ( 'NONE',  ( 67.57210640937580592, 216.4865022471902876, 10.00000000000009415 ) ) ;
#96412 = CARTESIAN_POINT ( 'NONE',  ( -36.52772323645827868, 26.41323893245352039, -10.00000000000000000 ) ) ;
#96413 = CARTESIAN_POINT ( 'NONE',  ( 0.000000000000000000, 0.000000000000000000, 0.000000000000000000 ) ) ;
#96414 = CARTESIAN_POINT ( 'NONE',  ( 6.417452267959404821, 25.74646525600388003, 2.839279412974139660 ) ) ;
#96415 = DIRECTION ( 'NONE',  ( 0.000000000000000000, -0.000000000000000000, -1.000000000000000000 ) ) ;
#96416 = CARTESIAN_POINT ( 'NONE',  ( 13.12254358208367577, 30.68290643055186706, 3.479690158560446702E-15 ) ) ;
#96417 = CARTESIAN_POINT ( 'NONE',  ( 159.6023402823087451, 258.6676503891110883, 17.43025742997651761 ) ) ;
#96418 = VECTOR ( 'NONE', #93867, 1000.000000000000000 ) ;
#96419 = CARTESIAN_POINT ( 'NONE',  ( 154.8838596469624349, 262.3802811495310152, 18.07457254681616021 ) ) ;
#96420 = ORIENTED_EDGE ( 'NONE', *, *, #60755, .F. ) ;
#96421 = CARTESIAN_POINT ( 'NONE',  ( 156.2426905888906958, 276.2173076510940177, 10.27655790510740985 ) ) ;
#96422 = CARTESIAN_POINT ( 'NONE',  ( 74.95119442303548851, 53.20651566882768435, -16.03659100943698945 ) ) ;
#96423 = CARTESIAN_POINT ( 'NONE',  ( 158.8266160086023149, 257.5512268093053194, -17.29683829744028856 ) ) ;
#96424 = CARTESIAN_POINT ( 'NONE',  ( -17.42236680055705023, 149.2012482093457777, 0.000000000000000000 ) ) ;
#96425 = EDGE_CURVE ( 'NONE', #11558, #100173, #83466, .T. ) ;
#96426 = ORIENTED_EDGE ( 'NONE', *, *, #50619, .T. ) ;
#96427 = CARTESIAN_POINT ( 'NONE',  ( 192.4454213697443095, 297.3217478340386606, 12.58566886711101596 ) ) ;
#96428 = CARTESIAN_POINT ( 'NONE',  ( 207.1059763530604698, 271.9289217357780899, 6.370907250589925575 ) ) ;
#96429 = VECTOR ( 'NONE', #43074, 1000.000000000000000 ) ;
#96430 = CARTESIAN_POINT ( 'NONE',  ( 66.34027612997587653, 68.16670350466722539, 4.419308956821091705 ) ) ;
#96431 = EDGE_CURVE ( 'NONE', #85237, #30618, #4638, .T. ) ;
#96432 = CARTESIAN_POINT ( 'NONE',  ( 125.6883311748214425, 231.8262482093457493, 3.021315404115420679E-15 ) ) ;
#96433 = ORIENTED_EDGE ( 'NONE', *, *, #37924, .T. ) ;
#96434 = VERTEX_POINT ( 'NONE', #80365 ) ;
#96436 = CARTESIAN_POINT ( 'NONE',  ( 204.8284483594339065, 275.8737159363993214, 14.69997973035875383 ) ) ;
#96435 = CARTESIAN_POINT ( 'NONE',  ( 75.28650001057752661, 66.67572118895705557, 13.44401380721711270 ) ) ;
#96437 = CARTESIAN_POINT ( 'NONE',  ( 86.57431924022760938, 47.22157117268152149, 10.65071021778218352 ) ) ;
#96438 = EDGE_LOOP ( 'NONE', ( #49339, #61361, #70364, #81608 ) ) ;
#96439 = CARTESIAN_POINT ( 'NONE',  ( 77.04668223076443212, 53.92430565998370184, 16.00320842628551787 ) ) ;
#96440 = CARTESIAN_POINT ( 'NONE',  ( 178.1946123598630720, 263.8186659389383522, 15.20355339309904963 ) ) ;
#96441 = ORIENTED_EDGE ( 'NONE', *, *, #22653, .T. ) ;
#96442 = LINE ( 'NONE', #55866, #5461 ) ;
#96443 = CARTESIAN_POINT ( 'NONE',  ( 84.80240350195585108, 209.7677522451417929, -5.000000000000041744 ) ) ;
#96444 = CARTESIAN_POINT ( 'NONE',  ( 81.04805182755087856, 43.65517749199150188, 9.457138610966682180 ) ) ;
#96445 = EDGE_LOOP ( 'NONE', ( #12324, #19053, #88600, #32385 ) ) ;
#96446 = CARTESIAN_POINT ( 'NONE',  ( 161.4469036912142599, 251.0127554125742222, 12.93933463576739307 ) ) ;
#96447 = CARTESIAN_POINT ( 'NONE',  ( 166.7606102460582918, 274.5312062198365197, -15.18303354322240395 ) ) ;
#96448 = AXIS2_PLACEMENT_3D ( 'NONE', #97595, #96121, #80424 ) ;
#96449 = AXIS2_PLACEMENT_3D ( 'NONE', #43498, #58688, #45489 ) ;
#96450 = CARTESIAN_POINT ( 'NONE',  ( 10.06845959268932411, 31.07446838803123157, -10.00000000000000000 ) ) ;
#96451 = ORIENTED_EDGE ( 'NONE', *, *, #95638, .F. ) ;
#96452 = CARTESIAN_POINT ( 'NONE',  ( 148.9230895364621574, 272.7046378331555161, 12.20434325797056019 ) ) ;
#96453 = CARTESIAN_POINT ( 'NONE',  ( 202.9216520459657147, 279.1763840310111391, 15.75371595331685803 ) ) ;
#96454 = VERTEX_POINT ( 'NONE', #72756 ) ;
#96455 = FACE_OUTER_BOUND ( 'NONE', #27388, .T. ) ;
#96456 = VECTOR ( 'NONE', #59177, 1000.000000000000114 ) ;
#96457 = VERTEX_POINT ( 'NONE', #32715 ) ;
#96458 = CARTESIAN_POINT ( 'NONE',  ( 157.0284915711613678, 269.7273995439030045, 16.18108137139518732 ) ) ;
#96459 = ORIENTED_EDGE ( 'NONE', *, *, #93892, .F. ) ;
#96460 = EDGE_CURVE ( 'NONE', #62465, #86376, #55496, .T. ) ;
#96461 = CARTESIAN_POINT ( 'NONE',  ( 147.8105987091051645, 274.6315284690918475, 6.028275121586289309 ) ) ;
#96462 = CARTESIAN_POINT ( 'NONE',  ( 180.5415972302508010, 291.3317084335843674, -9.685907878306698748 ) ) ;
#96463 = CARTESIAN_POINT ( 'NONE',  ( 133.4622058806418750, 257.8615022471902876, 5.000000000000046185 ) ) ;
#96464 = CARTESIAN_POINT ( 'NONE',  ( 199.5820190223589066, 281.0610403850588455, -17.29246150691365358 ) ) ;
#96465 = PRODUCT_DEFINITION_FORMATION_WITH_SPECIFIED_SOURCE ( 'ANY', '', #49980, .NOT_KNOWN. ) ;
#96466 = CYLINDRICAL_SURFACE ( 'NONE', #11132, 70.00000000000002842 ) ;
#96467 = CARTESIAN_POINT ( 'NONE',  ( 128.5163324648304410, 256.5530062829863027, -4.648177544792955347E-16 ) ) ;
#96468 = VERTEX_POINT ( 'NONE', #94555 ) ;
#96469 = CARTESIAN_POINT ( 'NONE',  ( 156.9440562780969231, 274.4750137900673508, 13.77464823823377316 ) ) ;
#96470 = CARTESIAN_POINT ( 'NONE',  ( 28.14623683147711830, 18.11110640527293114, -2.839279412974138328 ) ) ;
#96471 = CARTESIAN_POINT ( 'NONE',  ( 165.0087721269838710, 244.8434183119457543, 2.604344609212914108 ) ) ;
#96473 = ORIENTED_EDGE ( 'NONE', *, *, #76491, .F. ) ;
#96472 = CARTESIAN_POINT ( 'NONE',  ( 159.9880386575927957, 253.5395837721924863, 15.85893018594752846 ) ) ;
#96474 = ORIENTED_EDGE ( 'NONE', *, *, #4721, .F. ) ;
#96475 = CARTESIAN_POINT ( 'NONE',  ( 187.6035355654556724, 277.1252990796724589, 17.06676580984018443 ) ) ;
#96476 = CARTESIAN_POINT ( 'NONE',  ( 69.92928646124981640, 62.82442351299641103, 13.89675756931289641 ) ) ;
#96477 = ADVANCED_FACE ( 'NONE', ( #86482 ), #87987, .T. ) ;
#96478 = DIRECTION ( 'NONE',  ( 0.000000000000000000, 0.000000000000000000, -1.000000000000000000 ) ) ;
#96479 = CARTESIAN_POINT ( 'NONE',  ( 11.69612814616573893, 25.49103043416548076, -8.090169943749479842 ) ) ;
#96480 = CARTESIAN_POINT ( 'NONE',  ( 160.6603037333772761, 252.3751865047794070, -15.24058959229929222 ) ) ;
#96481 = CARTESIAN_POINT ( 'NONE',  ( 147.9974455564266691, 274.3079002362971437, -10.09869768668086820 ) ) ;
#96482 = VERTEX_POINT ( 'NONE', #1331 ) ;
#96483 = DIRECTION ( 'NONE',  ( -0.8660254037844387076, -0.4999999999999998890, -0.000000000000000000 ) ) ;
#96484 = DIRECTION ( 'NONE',  ( -6.526680975732919234E-15, 1.065403912962273439E-14, 1.000000000000000000 ) ) ;
#96485 = CARTESIAN_POINT ( 'NONE',  ( 155.5582350408321588, 263.0053103591359900, 17.59663451232534825 ) ) ;
#96486 = CARTESIAN_POINT ( 'NONE',  ( 26.34568874650619463, 186.0177522451418497, -10.00000000000009592 ) ) ;
#96487 = CARTESIAN_POINT ( 'NONE',  ( 97.41363812451689341, 236.2369531367911009, -4.594050593750048428 ) ) ;
#96488 = CARTESIAN_POINT ( 'NONE',  ( 183.9927074563704537, 296.7549153586903685, -2.755382768168008756 ) ) ;
#96489 = CARTESIAN_POINT ( 'NONE',  ( 167.4702904630335070, 282.8281168849647997, -10.76115858899906108 ) ) ;
#96490 = CARTESIAN_POINT ( 'NONE',  ( 15.94411698533127542, 24.90829794293879473, 10.00000000000000355 ) ) ;
#96491 = CARTESIAN_POINT ( 'NONE',  ( 207.7117873102786518, 270.8796263780940308, 1.712754233133884085 ) ) ;
#96492 = CARTESIAN_POINT ( 'NONE',  ( 16.52171307410043255, 180.3458772461660544, 9.188101187500095079 ) ) ;
#96493 = AXIS2_PLACEMENT_3D ( 'NONE', #20207, #50098, #81534 ) ;
#96494 = CARTESIAN_POINT ( 'NONE',  ( 46.30674614090289509, 112.4688969640381231, -10.00000000000000000 ) ) ;
#96495 = ORIENTED_EDGE ( 'NONE', *, *, #34630, .T. ) ;
#96496 = ORIENTED_EDGE ( 'NONE', *, *, #37610, .F. ) ;
#96497 = CARTESIAN_POINT ( 'NONE',  ( 147.6461304576096438, 276.1816894454201474, -0.8296389602296602162 ) ) ;
#96498 = CARTESIAN_POINT ( 'NONE',  ( 80.53589555931883126, 46.94866704237161770, -12.72290194427851517 ) ) ;
#96499 = VECTOR ( 'NONE', #89495, 999.9999999999998863 ) ;
#96500 = FACE_OUTER_BOUND ( 'NONE', #42794, .T. ) ;
#96501 = CARTESIAN_POINT ( 'NONE',  ( 193.4275275796228186, 262.9968912118912954, -3.779748889324304528 ) ) ;
#96502 = EDGE_CURVE ( 'NONE', #59740, #27862, #26128, .T. ) ;
#96503 = CARTESIAN_POINT ( 'NONE',  ( 207.6357208050208101, 271.0113774299547913, -6.790259683043212036 ) ) ;
#96504 = CARTESIAN_POINT ( 'NONE',  ( 185.7809047750413356, 286.4304272575490700, 15.54309313237488155 ) ) ;
#96505 = CARTESIAN_POINT ( 'NONE',  ( 73.97927654802940367, 68.30869415006648637, -11.66811813765111516 ) ) ;
#96506 = CARTESIAN_POINT ( 'NONE',  ( 46.56214281575564939, 191.5643266524159856, -9.188101187500093303 ) ) ;
#96507 = CARTESIAN_POINT ( 'NONE',  ( 89.99855592466239784, 232.7677522451419065, -5.000000000000047962 ) ) ;
#96508 = ORIENTED_EDGE ( 'NONE', *, *, #39180, .F. ) ;
#96509 = ADVANCED_FACE ( 'NONE', ( #78840 ), #56514, .T. ) ;
#96510 = CARTESIAN_POINT ( 'NONE',  ( 79.31084698818212075, 59.85625551150462087, -16.50595436643997260 ) ) ;
#96511 = CARTESIAN_POINT ( 'NONE',  ( 178.7669947432931110, 259.1165679222901304, -10.20806745893763079 ) ) ;
#96512 = CARTESIAN_POINT ( 'NONE',  ( 4.992923434102598534, 167.5643266524160140, -9.188101187500093303 ) ) ;
#96513 = CARTESIAN_POINT ( 'NONE',  ( 72.93270222632345678, 70.75261854202811662, -7.421515863126949775 ) ) ;
#96514 = CARTESIAN_POINT ( 'NONE',  ( 150.6815632051821581, 269.6588720951601772, -14.68790257316217307 ) ) ;
#96515 = VECTOR ( 'NONE', #52968, 1000.000000000000000 ) ;
#96516 = CARTESIAN_POINT ( 'NONE',  ( 32.47331203838563596, 45.95596728736418868, -10.00000000000000000 ) ) ;
#96517 = CARTESIAN_POINT ( 'NONE',  ( 147.4271219180435253, 275.2957297547342819, -3.800519706258907782 ) ) ;
#96518 = CARTESIAN_POINT ( 'NONE',  ( 68.21857645778533197, 68.29686920240547465, -7.752314361411196231 ) ) ;
#96519 = CARTESIAN_POINT ( 'NONE',  ( 204.8523313866422484, 275.8323493198358847, 14.65426965484541100 ) ) ;
#96520 = CARTESIAN_POINT ( 'NONE',  ( 68.32831816981907025, 66.75461077405910260, 9.160816392852566992 ) ) ;
#96521 = CARTESIAN_POINT ( 'NONE',  ( 207.6007741873543750, 271.0719067473055475, 7.587922723682903658 ) ) ;
#96522 = ORIENTED_EDGE ( 'NONE', *, *, #27585, .F. ) ;
#96523 = VECTOR ( 'NONE', #25799, 1000.000000000000227 ) ;
#96524 = CARTESIAN_POINT ( 'NONE',  ( 164.4414259850711915, 245.8260906552167171, -6.983224448873608381 ) ) ;
#96525 = CARTESIAN_POINT ( 'NONE',  ( 7.094665711762558225, 168.2365022471901739, -10.00000000000009059 ) ) ;
#96526 = CARTESIAN_POINT ( 'NONE',  ( 74.39841895140679640, 68.21392270468032848, 11.95628786500076934 ) ) ;
#96527 = CARTESIAN_POINT ( 'NONE',  ( 122.0685591603289026, 241.2833772461660544, -9.188101187500095079 ) ) ;
#96528 = CARTESIAN_POINT ( 'NONE',  ( 22.39019813391814751, 21.43085787977763701, -9.188101187500008038 ) ) ;
#96529 = CARTESIAN_POINT ( 'NONE',  ( 74.76437051368166919, 67.10386306624577912, 12.96231939749656448 ) ) ;
#96530 = FACE_OUTER_BOUND ( 'NONE', #94103, .T. ) ;
#96532 = FACE_OUTER_BOUND ( 'NONE', #31517, .T. ) ;
#96531 = CARTESIAN_POINT ( 'NONE',  ( 157.3363371328520088, 258.1324655395517311, 18.24585617226787093 ) ) ;
#96533 = DIRECTION ( 'NONE',  ( 0.5000000000000014433, -0.8660254037844378194, 0.000000000000000000 ) ) ;
#96534 = ORIENTED_EDGE ( 'NONE', *, *, #60630, .T. ) ;
#96535 = CARTESIAN_POINT ( 'NONE',  ( 151.0778907302193943, 268.9724126853576536, 15.84769371787143832 ) ) ;
#96536 = CARTESIAN_POINT ( 'NONE',  ( 207.6440815245055092, 270.9968962390196339, -0.7124146351304289082 ) ) ;
#96537 = CARTESIAN_POINT ( 'NONE',  ( 34.73896580337741113, 43.55466486950702887, 7.012934429366973338E-14 ) ) ;
#96538 = LINE ( 'NONE', #13885, #70935 ) ;
#96539 = CARTESIAN_POINT ( 'NONE',  ( 81.54227884105102930, 55.16382101384258618, -15.91942278333091920 ) ) ;
#96540 = EDGE_LOOP ( 'NONE', ( #20090, #65369, #5375, #46949 ) ) ;
#96541 = CARTESIAN_POINT ( 'NONE',  ( 138.1351346183475357, 243.8927522451417929, -10.00000000000009237 ) ) ;
#96542 = CARTESIAN_POINT ( 'NONE',  ( 80.28753194487839551, 45.30207178207673735, 12.22351710471137665 ) ) ;
#96543 = CARTESIAN_POINT ( 'NONE',  ( 71.85125637137586807, 72.20757445900991911, 0.5766358698793758730 ) ) ;
#96544 = EDGE_CURVE ( 'NONE', #3105, #13470, #55009, .T. ) ;
#96545 = CARTESIAN_POINT ( 'NONE',  ( 83.06094347246988718, 41.92204296775934580, 4.233641397788413308 ) ) ;
#96546 = CARTESIAN_POINT ( 'NONE',  ( 80.56202954020663753, 57.53823600680942718, 16.23110421993949259 ) ) ;
#96547 = CARTESIAN_POINT ( 'NONE',  ( 156.6812872898450735, 261.2670451491295012, 0.000000000000000000 ) ) ;
#96548 = EDGE_CURVE ( 'NONE', #34660, #85223, #41809, .T. ) ;
#96549 = CARTESIAN_POINT ( 'NONE',  ( 72.06693479607845632, 71.51559350784613400, -5.828149303013867133 ) ) ;
#96550 = CARTESIAN_POINT ( 'NONE',  ( 150.2135478535318782, 277.3480115108075097, -0.0001741048118424651735 ) ) ;
#96551 = ORIENTED_EDGE ( 'NONE', *, *, #4528, .T. ) ;
#96552 = B_SPLINE_CURVE_WITH_KNOTS ( 'NONE', 3,
 ( #57626, #10051, #88604, #80489, #65236, #9043, #41425, #17134, #72370, #70846, #87620, #40424, #25235, #63240, #3464, #34341, #49535, #1949, #88106, #94181, #79488, #48032, #2976, #32833, #49048, #9561, #64754, #63743, #95702, #87114, #56637, #2459, #17650, #10551, #94677, #71863, #56121, #48548, #79984, #33341, #26249, #11060 ),
 .UNSPECIFIED., .F., .F.,
 ( 4, 2, 2, 2, 2, 2, 2, 2, 2, 2, 2, 2, 2, 2, 2, 2, 2, 2, 2, 2, 4 ),
 ( 0.0009056366646472498085, 0.001003186449675941110, 0.001100736234704632411, 0.001198286019733323712, 0.001295835804762014796, 0.001490935374819419949, 0.001686034944876825103, 0.002466433225106563244, 0.004027229785566034323, 0.004807628065795770296, 0.005197827205910719381, 0.005392926775968194357, 0.005490476560996922738, 0.005588026346025650251, 0.005636801238540015309, 0.005685576131054379499, 0.005783125916083084461, 0.005978225486140473569, 0.006368424626255224895, 0.006758623766369976221, 0.007148822906484728415 ),
 .UNSPECIFIED. ) ;
#96553 = FACE_OUTER_BOUND ( 'NONE', #55272, .T. ) ;
#96554 = EDGE_CURVE ( 'NONE', #14044, #38349, #65119, .T. ) ;
#96555 = CARTESIAN_POINT ( 'NONE',  ( 5.363317384539951327, 21.83478043621385822, -8.090169943749479842 ) ) ;
#96556 = CARTESIAN_POINT ( 'NONE',  ( -71.61465314115659453, 63.06504152958490295, -20.00000000000001776 ) ) ;
#96557 = ORIENTED_EDGE ( 'NONE', *, *, #29284, .T. ) ;
#96558 = DIRECTION ( 'NONE',  ( -0.3958915996110536351, -0.9182972510888840478, 0.000000000000000000 ) ) ;
#96559 = ADVANCED_FACE ( 'NONE', ( #18037 ), #63615, .T. ) ;
#96560 = CARTESIAN_POINT ( 'NONE',  ( 194.9385458806846430, 293.0035295114944347, -15.70518692812489192 ) ) ;
#96561 = CARTESIAN_POINT ( 'NONE',  ( 159.6649394982892716, 264.0993667363822510, -17.39019615698379795 ) ) ;
#96562 = VERTEX_POINT ( 'NONE', #40298 ) ;
#96563 = CARTESIAN_POINT ( 'NONE',  ( 78.70150085959762976, 59.83202584994827333, 16.12694553795979502 ) ) ;
#96564 = CARTESIAN_POINT ( 'NONE',  ( 204.7319642249719038, 272.9966618342774041, -9.756553772762273979 ) ) ;
#96565 = CARTESIAN_POINT ( 'NONE',  ( 75.06725799386214248, 52.99710587067458079, -16.48800421929521676 ) ) ;
#96566 = AXIS2_PLACEMENT_3D ( 'NONE', #15934, #70123, #31124 ) ;
#96567 = DIRECTION ( 'NONE',  ( -0.8660254037844387076, -0.4999999999999998890, -0.000000000000000000 ) ) ;
#96568 = ORIENTED_EDGE ( 'NONE', *, *, #81984, .T. ) ;
#96569 = CARTESIAN_POINT ( 'NONE',  ( 89.94416901687610277, 231.9244531367911009, -4.594050593750046652 ) ) ;
#96570 = CARTESIAN_POINT ( 'NONE',  ( 80.48237008273157755, 51.22225194333302767, -14.94672880192676523 ) ) ;
#96571 = AXIS2_PLACEMENT_3D ( 'NONE', #29776, #37363, #60649 ) ;
#96572 = CARTESIAN_POINT ( 'NONE',  ( 73.44884507967250897, 69.80860085198864340, -9.835095417347671898 ) ) ;
#96573 = CARTESIAN_POINT ( 'NONE',  ( 84.44631528110988938, 49.90853024617071299, -13.72425691458318475 ) ) ;
#96574 = CARTESIAN_POINT ( 'NONE',  ( 181.8938501633026874, 257.1921657151197564, -6.106366152575129824 ) ) ;
#96575 = EDGE_LOOP ( 'NONE', ( #83214, #64622, #2209, #81775 ) ) ;
#96576 = ORIENTED_EDGE ( 'NONE', *, *, #28789, .T. ) ;
#96578 = VECTOR ( 'NONE', #97686, 1000.000000000000000 ) ;
#96577 = CARTESIAN_POINT ( 'NONE',  ( -77.42978507651396569, 55.80833764325424085, -10.00000000000000000 ) ) ;
#96579 = ORIENTED_EDGE ( 'NONE', *, *, #11902, .T. ) ;
#96580 = CARTESIAN_POINT ( 'NONE',  ( 144.9863040978925142, 263.1751974929321705, -1.822351119449947324E-15 ) ) ;
#96581 = ORIENTED_EDGE ( 'NONE', *, *, #72896, .T. ) ;
#96582 = CARTESIAN_POINT ( 'NONE',  ( 169.6747932974647028, 272.0074737424269529, -17.60367342859795059 ) ) ;
#96583 = CARTESIAN_POINT ( 'NONE',  ( 154.9528145190857344, 262.2608478075840708, -17.26679351315302213 ) ) ;
#96584 = ORIENTED_EDGE ( 'NONE', *, *, #85999, .F. ) ;
#96585 = CARTESIAN_POINT ( 'NONE',  ( 182.9098479943871212, 279.8073795562751798, -16.44634284297093885 ) ) ;
#96586 = CARTESIAN_POINT ( 'NONE',  ( 105.0000000000000000, 4.999999999999999112, 14.21260523776213347 ) ) ;
#96587 = CARTESIAN_POINT ( 'NONE',  ( 151.3074424083568204, 269.1194857459262266, 14.21895990402933307 ) ) ;
#96588 = FACE_OUTER_BOUND ( 'NONE', #10823, .T. ) ;
#96589 = CARTESIAN_POINT ( 'NONE',  ( 201.1388841337167435, 282.2642286331299601, -18.17233400608081340 ) ) ;
#96590 = DIRECTION ( 'NONE',  ( 0.5000000000000013323, -0.8660254037844378194, 0.000000000000000000 ) ) ;
#96591 = CARTESIAN_POINT ( 'NONE',  ( 157.4068442735347446, 281.9945091197541274, 2.874377194828706905 ) ) ;
#96592 = CARTESIAN_POINT ( 'NONE',  ( 142.6906155400633622, 259.3149278399160380, -9.188101187500095079 ) ) ;
#96593 = VERTEX_POINT ( 'NONE', #17009 ) ;
#96594 = CARTESIAN_POINT ( 'NONE',  ( 70.76287552252175317, 61.08876315251507805, -14.44714046989205691 ) ) ;
#96595 = CARTESIAN_POINT ( 'NONE',  ( 7.821713311501573784, 19.91421378149916421, 9.188101187500008038 ) ) ;
#96596 = ORIENTED_EDGE ( 'NONE', *, *, #78944, .F. ) ;
#96598 = ORIENTED_EDGE ( 'NONE', *, *, #91502, .F. ) ;
#96597 = CARTESIAN_POINT ( 'NONE',  ( 200.0079957071587273, 270.2013779111154577, 9.272782244027494514 ) ) ;
#96599 = VECTOR ( 'NONE', #15784, 1000.000000000000114 ) ;
#96600 = CARTESIAN_POINT ( 'NONE',  ( -13.86269525828469895, 104.2312461070084879, 10.61543114587583148 ) ) ;
#96601 = CARTESIAN_POINT ( 'NONE',  ( -43.70040200909112116, 27.32518560721127088, -10.00000000000000000 ) ) ;
#96602 = CARTESIAN_POINT ( 'NONE',  ( 129.4230657250939203, 233.9824982072973683, 3.021315404115420679E-15 ) ) ;
#96603 = CARTESIAN_POINT ( 'NONE',  ( 153.2255732592549009, 277.0430973404892825, 6.869329404264208350 ) ) ;
#96604 = CARTESIAN_POINT ( 'NONE',  ( 165.5128516766338294, 246.9059456859405373, -1.886539856749224420 ) ) ;
#96605 = VECTOR ( 'NONE', #65445, 1000.000000000000114 ) ;
#96606 = CARTESIAN_POINT ( 'NONE',  ( 192.6480976257870452, 292.3694868334920329, -14.35794368392827636 ) ) ;
#96607 = CARTESIAN_POINT ( 'NONE',  ( 84.64118529441607564, 42.23213341487252848, 1.449458229959814881 ) ) ;
#96608 = CARTESIAN_POINT ( 'NONE',  ( 88.29906409831174585, 44.33258913401337509, -2.209727062603330516 ) ) ;
#96609 = ORIENTED_EDGE ( 'NONE', *, *, #81456, .F. ) ;
#96610 = CARTESIAN_POINT ( 'NONE',  ( 147.6264044922760377, 274.9505622111005323, -8.841872555777701592 ) ) ;
#96611 = CARTESIAN_POINT ( 'NONE',  ( 66.01596945876833900, 69.23916865775863982, 0.2712613576453007935 ) ) ;
#96612 = ORIENTED_EDGE ( 'NONE', *, *, #2461, .F. ) ;
#96613 = CARTESIAN_POINT ( 'NONE',  ( -18.11259370987442452, 171.8967562850347406, 9.296355089585912665E-16 ) ) ;
#96614 = CARTESIAN_POINT ( 'NONE',  ( 201.0067457102312005, 267.8329504270425900, -2.840095696601848907 ) ) ;
#96615 = CARTESIAN_POINT ( 'NONE',  ( 203.8401700684498792, 277.5854641484010585, -14.28809178781177636 ) ) ;
#96616 = DIRECTION ( 'NONE',  ( 0.000000000000000000, 0.000000000000000000, 1.000000000000000000 ) ) ;
#96617 = EDGE_CURVE ( 'NONE', #45450, #1077, #8229, .T. ) ;
#96618 = CARTESIAN_POINT ( 'NONE',  ( 202.4900219881211854, 279.9239892212719383, 15.63116161057562259 ) ) ;
#96619 = CARTESIAN_POINT ( 'NONE',  ( 88.21232870727821762, 44.34776898565001346, 2.631490070295979145 ) ) ;
#96620 = CARTESIAN_POINT ( 'NONE',  ( 42.87900647455834502, 24.75620593066997444, 1.732050807568941364 ) ) ;
#96621 = ORIENTED_EDGE ( 'NONE', *, *, #8219, .T. ) ;
#96622 = CARTESIAN_POINT ( 'NONE',  ( 76.82263189186275554, 60.88017539376242837, -15.71791450812036395 ) ) ;
#96623 = CARTESIAN_POINT ( 'NONE',  ( 80.47309446435835412, 57.88546628059901167, 16.25201728225186315 ) ) ;
#96624 = CARTESIAN_POINT ( 'NONE',  ( 71.79012238242354726, 65.93304147633399737, -12.01195568269040947 ) ) ;
#96625 = CARTESIAN_POINT ( 'NONE',  ( 153.0070714074088016, 265.6309737354857248, 17.74442213480098474 ) ) ;
#96626 = CARTESIAN_POINT ( 'NONE',  ( -27.42236680055714260, 166.5217562850347406, 1.224646799147364892E-15 ) ) ;
#96627 = LINE ( 'NONE', #66185, #93574 ) ;
#96628 = CARTESIAN_POINT ( 'NONE',  ( 6.805730253569997501, 183.9244531367911293, -4.594050593750046652 ) ) ;
#96629 = CARTESIAN_POINT ( 'NONE',  ( 107.1835739849013578, 238.8149278399160664, 9.188101187500093303 ) ) ;
#96630 = CARTESIAN_POINT ( 'NONE',  ( 87.77887691218910504, 44.16646017302762317, -4.484802941535590115 ) ) ;
#96631 = CARTESIAN_POINT ( 'NONE',  ( 179.9070225497684419, 255.1121438720595620, -2.403939176287567037 ) ) ;
#96632 = DIRECTION ( 'NONE',  ( -1.000000000000000000, 0.000000000000000000, 0.000000000000000000 ) ) ;
#96633 = B_SPLINE_CURVE_WITH_KNOTS ( 'NONE', 3,
 ( #50290, #17394, #56887, #41686, #87870, #48306, #25499, #40684, #48814, #33099, #63996, #79747, #56391, #87387, #10309, #18416, #72629, #3230, #95950, #66490, #43170, #89833, #59875, #27512 ),
 .UNSPECIFIED., .F., .F.,
 ( 4, 2, 2, 2, 2, 2, 2, 2, 2, 2, 2, 4 ),
 ( 0.000000000000000000, 0.1250000000000107692, 0.2500000000000215383, 0.3750000000000323075, 0.4375000000000291434, 0.5000000000000259792, 0.5625000000000227596, 0.6250000000000196509, 0.6875000000000164313, 0.7500000000000133227, 0.8750000000000066613, 1.000000000000000000 ),
 .UNSPECIFIED. ) ;
#96634 = VECTOR ( 'NONE', #26691, 1000.000000000000227 ) ;
#96635 = CARTESIAN_POINT ( 'NONE',  ( 76.40735639740501028, 51.42921241913779085, 15.62223202341787598 ) ) ;
#96636 = VECTOR ( 'NONE', #6684, 1000.000000000000000 ) ;
#96637 = CARTESIAN_POINT ( 'NONE',  ( 160.7389373414059435, 281.8969065408946335, 5.212150423231117990 ) ) ;
#96638 = CARTESIAN_POINT ( 'NONE',  ( 194.7576540903134799, 293.3168432830895540, -14.62421624641040196 ) ) ;
#96639 = CARTESIAN_POINT ( 'NONE',  ( -19.65312891409030271, 5.000000000000004441, -54.99999999999999289 ) ) ;
#96640 = CARTESIAN_POINT ( 'NONE',  ( 84.32075484545329402, 50.66451156707553594, 13.78810211404426411 ) ) ;
#96641 = DIRECTION ( 'NONE',  ( 0.8660254037844394848, 0.4999999999999986122, 0.000000000000000000 ) ) ;
#96642 = CARTESIAN_POINT ( 'NONE',  ( 75.82692561157452360, 55.11882190618480593, -16.59949335850286545 ) ) ;
#96643 = AXIS2_PLACEMENT_3D ( 'NONE', #47939, #9466, #94098 ) ;
#96644 = CARTESIAN_POINT ( 'NONE',  ( 173.3240139114783460, 264.2345359633658859, -15.45835341172655930 ) ) ;
#96645 = CARTESIAN_POINT ( 'NONE',  ( 76.33141897508073725, 221.0024278399160949, 9.188101187500095079 ) ) ;
#96646 = CARTESIAN_POINT ( 'NONE',  ( 161.0965315767822972, 251.6196177163260188, -13.76772246540905442 ) ) ;
#96647 = CARTESIAN_POINT ( 'NONE',  ( 84.55537670905214043, 50.62155581810768012, -14.09136642048690291 ) ) ;
#96648 = CARTESIAN_POINT ( 'NONE',  ( 163.4477778843836404, 257.9215091531312396, 15.58283331752105738 ) ) ;
#96650 = CARTESIAN_POINT ( 'NONE',  ( 151.9413948867106683, 267.4767796137679170, 15.48523777917124100 ) ) ;
#96649 = CARTESIAN_POINT ( 'NONE',  ( 196.4677102463732012, 290.3549391369982686, 16.45225250689336249 ) ) ;
#96651 = CARTESIAN_POINT ( 'NONE',  ( 75.58214075417596689, 65.23491603964200181, 14.35294216029142333 ) ) ;
#96652 = CARTESIAN_POINT ( 'NONE',  ( 176.5572900059099197, 270.1083417844832866, -16.76627801634431947 ) ) ;
#96653 = CARTESIAN_POINT ( 'NONE',  ( 32.78250297933140445, 27.43085787977765122, -9.188101187500008038 ) ) ;
#96654 = LINE ( 'NONE', #10026, #98496 ) ;
#96655 = CARTESIAN_POINT ( 'NONE',  ( 75.63520882045094140, 61.37380848085838636, 15.84745159558423744 ) ) ;
#96656 = ORIENTED_EDGE ( 'NONE', *, *, #42251, .F. ) ;
#96657 = CARTESIAN_POINT ( 'NONE',  ( 13.78045586392592092, 26.14336893147754282, 7.433330006724141015 ) ) ;
#96658 = CARTESIAN_POINT ( 'NONE',  ( 171.8195984572240889, 288.9771131316106789, -1.063263625893295483 ) ) ;
#96659 = CARTESIAN_POINT ( 'NONE',  ( -32.94356256989595977, 94.88921800892812541, 10.61543114587583503 ) ) ;
#96660 = CARTESIAN_POINT ( 'NONE',  ( 30.80155721116056355, 46.36891074996812989, -10.00000000000000000 ) ) ;
#96661 = CARTESIAN_POINT ( 'NONE',  ( 86.57431924022760938, 47.22157117268152149, 10.65071021778218352 ) ) ;
#96662 = CARTESIAN_POINT ( 'NONE',  ( 189.7523420421647131, 286.5162620012252432, 16.62308081069983956 ) ) ;
#96663 = CARTESIAN_POINT ( 'NONE',  ( 72.09375247312608792, 71.41439723707200926, 5.090740936595467225 ) ) ;
#96664 = CARTESIAN_POINT ( 'NONE',  ( 87.28672817441044174, 44.98879080050047463, -6.213673670119491454 ) ) ;
#96666 =( BOUNDED_CURVE ( )  B_SPLINE_CURVE ( 2, ( #64124, #86486, #2854, #25637, #24126, #85993, #70723, #33744, #64636 ),
 .UNSPECIFIED., .F., .T. ) 
 B_SPLINE_CURVE_WITH_KNOTS ( ( 3, 2, 2, 2, 3 ),
 ( 0.2620967741935483764, 0.2634408602150537515, 0.2661290322580645018, 0.2688172043010752521, 0.2701612903225806273 ),
 .UNSPECIFIED. ) 
 CURVE ( )  GEOMETRIC_REPRESENTATION_ITEM ( )  RATIONAL_B_SPLINE_CURVE ( ( 0.9330127018922194093, 0.9330127018922194093, 1.000000000000000000, 0.8660254037844387076, 1.000000000000000000, 0.8660254037844387076, 1.000000000000000000, 0.9330127018922194093, 0.9330127018922194093 ) ) 
 REPRESENTATION_ITEM ( '' )  );
#96665 = CARTESIAN_POINT ( 'NONE',  ( 115.2756724011686202, 247.3615022471903160, 5.000000000000046185 ) ) ;
#96667 = CARTESIAN_POINT ( 'NONE',  ( 157.8696211474012330, 257.2087905314882619, -17.27527248276125604 ) ) ;
#96669 = AXIS2_PLACEMENT_3D ( 'NONE', #78535, #93763, #53220 ) ;
#96668 = CARTESIAN_POINT ( 'NONE',  ( 74.82815960207534545, 53.36537385475131856, 16.05773697466056404 ) ) ;
#96670 = ORIENTED_EDGE ( 'NONE', *, *, #15197, .T. ) ;
#96671 = CARTESIAN_POINT ( 'NONE',  ( 169.5637984545885786, 248.3293919737242845, -1.956443885671045102 ) ) ;
#96672 = ORIENTED_EDGE ( 'NONE', *, *, #5435, .F. ) ;
#96673 = CARTESIAN_POINT ( 'NONE',  ( 203.0535368433499457, 278.9479528611958585, 16.46202213522710167 ) ) ;
#96674 = CARTESIAN_POINT ( 'NONE',  ( 182.7674680796695554, 291.1753568628804487, -12.34959082582511058 ) ) ;
#96675 = EDGE_CURVE ( 'NONE', #28264, #50323, #27624, .T. ) ;
#96676 = ORIENTED_EDGE ( 'NONE', *, *, #69523, .T. ) ;
#96677 = CARTESIAN_POINT ( 'NONE',  ( 89.11175791728626905, 45.37822637883662225, 1.911324073694122932E-15 ) ) ;
#96678 = ORIENTED_EDGE ( 'NONE', *, *, #44375, .T. ) ;
#96679 = CARTESIAN_POINT ( 'NONE',  ( 71.94643353573427191, 71.53214566342799685, 5.625104812542565114 ) ) ;
#96680 = CARTESIAN_POINT ( 'NONE',  ( 13.83268420227240014, 8.390406791769812855, -2.889640176918245968E-15 ) ) ;
#96681 = CARTESIAN_POINT ( 'NONE',  ( 141.9056932439424372, 261.9244531367911577, -4.594050593750046652 ) ) ;
#96682 = CARTESIAN_POINT ( 'NONE',  ( 205.4925884257800988, 274.0740247280971857, 10.80283695292349222 ) ) ;
#96683 = DIRECTION ( 'NONE',  ( -0.000000000000000000, -0.000000000000000000, -1.000000000000000000 ) ) ;
#96684 = CARTESIAN_POINT ( 'NONE',  ( 25.67147243227365649, 35.79752408145593989, -5.678558825948271327 ) ) ;
#96685 = CARTESIAN_POINT ( 'NONE',  ( 79.97511216739995632, 58.10444404117469475, -16.24719292606884125 ) ) ;
#96686 = CARTESIAN_POINT ( 'NONE',  ( 164.6915199398825393, 274.4969406795170812, 14.73953457787395749 ) ) ;
#96687 =( BOUNDED_CURVE ( )  B_SPLINE_CURVE ( 2, ( #84741, #61390, #62894, #9206, #38591, #8704, #7193, #39076, #603 ),
 .UNSPECIFIED., .F., .T. ) 
 B_SPLINE_CURVE_WITH_KNOTS ( ( 3, 2, 2, 2, 3 ),
 ( 0.9314516129032257563, 0.9327956989247311315, 0.9354838709677418818, 0.9381720430107527431, 0.9395161290322581182 ),
 .UNSPECIFIED. ) 
 CURVE ( )  GEOMETRIC_REPRESENTATION_ITEM ( )  RATIONAL_B_SPLINE_CURVE ( ( 0.9330127018922194093, 0.9330127018922194093, 1.000000000000000000, 0.8660254037844387076, 1.000000000000000000, 0.8660254037844387076, 1.000000000000000000, 0.9330127018922194093, 0.9330127018922194093 ) ) 
 REPRESENTATION_ITEM ( '' )  );
#96688 = DIRECTION ( 'NONE',  ( -0.8263106059122556912, -0.5632146860273805622, 0.000000000000000000 ) ) ;
#96689 = ORIENTED_EDGE ( 'NONE', *, *, #82701, .T. ) ;
#96690 = VERTEX_POINT ( 'NONE', #74246 ) ;
#96691 = DIRECTION ( 'NONE',  ( 0.000000000000000000, 0.000000000000000000, 1.000000000000000000 ) ) ;
#96693 = CARTESIAN_POINT ( 'NONE',  ( 194.9220242159064185, 293.0321458743159724, -14.92681063007793263 ) ) ;
#96692 = CARTESIAN_POINT ( 'NONE',  ( 68.17866407165988107, 65.83321247030521306, 10.84866537784224327 ) ) ;
#96694 = CARTESIAN_POINT ( 'NONE',  ( 85.88643775857894980, 48.50416193104786799, 12.18167088616390537 ) ) ;
#96695 = CARTESIAN_POINT ( 'NONE',  ( -19.65312891409030271, 93.06504152958497400, 177.5919119679930134 ) ) ;
#96696 = CARTESIAN_POINT ( 'NONE',  ( 123.2683651867145898, 248.6427522451419350, 10.00000000000009415 ) ) ;
#96697 = DIRECTION ( 'NONE',  ( 0.2942337105004269593, 0.9557335003049495237, 0.000000000000000000 ) ) ;
#96698 = B_SPLINE_CURVE_WITH_KNOTS ( 'NONE', 3,
 ( #2909, #56570, #33803, #95636, #88045, #18089, #79923, #18593, #64686, #50962, #66178, #72813, #58560, #64177, #10483, #41361, #96124, #73783, #80936, #65174, #9991, #97122, #26678, #95126, #88539, #19102, #49981, #87557, #11505, #72302, #42359, #3883, #11990, #27690, #26185, #49471, #96622, #89531, #27187, #40852, #58075, #89056, #19606, #50466, #81418, #42847 ),
 .UNSPECIFIED., .F., .F.,
 ( 4, 1, 1, 1, 2, 2, 1, 1, 1, 2, 2, 1, 1, 2, 2, 1, 1, 2, 2, 1, 1, 2, 2, 1, 2, 2, 1, 2, 2, 4 ),
 ( 0.000000000000000000, 0.06250000000003216871, 0.09375000000004683753, 0.1093750000000559830, 0.1171875000000583283, 0.1250000000000606737, 0.1875000000000799083, 0.2187500000000895950, 0.2343750000000944522, 0.2421875000000950351, 0.2500000000000955902, 0.3125000000001050271, 0.3437500000001079137, 0.3593750000001077471, 0.3750000000001075806, 0.4375000000000972000, 0.4687500000000917599, 0.4843750000000913158, 0.5000000000000908162, 0.5625000000000797140, 0.5937500000000740519, 0.6093750000000709433, 0.6250000000000678346, 0.6875000000000563993, 0.7187500000000501821, 0.7500000000000439648, 0.8125000000000323075, 0.8437500000000265343, 0.8750000000000206501, 1.000000000000000000 ),
 .UNSPECIFIED. ) ;
#96699 = CARTESIAN_POINT ( 'NONE',  ( 208.1405733532425018, 270.1369471661045623, -4.189134151581175303 ) ) ;
#96700 = FACE_OUTER_BOUND ( 'NONE', #60138, .T. ) ;
#96701 = DIRECTION ( 'NONE',  ( -1.000000000000000000, 0.000000000000000000, 0.000000000000000000 ) ) ;
#96702 = CARTESIAN_POINT ( 'NONE',  ( 99.93095832397169431, 222.3768266524160140, 9.188101187500098632 ) ) ;
#96703 = EDGE_LOOP ( 'NONE', ( #39299, #59354, #2660, #65126 ) ) ;
#96704 = LINE ( 'NONE', #27273, #36633 ) ;
#96705 = CARTESIAN_POINT ( 'NONE',  ( 163.7315607857516682, 276.6876062851454208, -13.69158268838586245 ) ) ;
#96706 = VECTOR ( 'NONE', #52187, 1000.000000000000000 ) ;
#96707 = ORIENTED_EDGE ( 'NONE', *, *, #79849, .T. ) ;
#96708 = AXIS2_PLACEMENT_3D ( 'NONE', #94158, #24711, #55594 ) ;
#96709 = ORIENTED_EDGE ( 'NONE', *, *, #58865, .F. ) ;
#96710 = CARTESIAN_POINT ( 'NONE',  ( 87.09644473823584576, 45.85687564672072369, -8.636203292310963064 ) ) ;
#96712 = B_SPLINE_SURFACE_WITH_KNOTS ( 'NONE', 3, 1, ( 
 ( #40166, #32588 ),
 ( #10801, #95939 ),
 ( #94424, #40672 ),
 ( #41169, #71610 ),
 ( #18402, #2710 ),
 ( #41674, #87376 ),
 ( #63984, #25487 ),
 ( #72107, #33597 ),
 ( #64492, #95453 ),
 ( #49294, #26005 ),
 ( #80234, #72618 ),
 ( #3220, #34105 ),
 ( #80746, #96430 ),
 ( #58371, #73596 ),
 ( #59351, #82232 ),
 ( #26994, #50771 ),
 ( #66478, #5674 ),
 ( #57879, #88857 ),
 ( #35583, #89347 ),
 ( #4177, #19423 ),
 ( #81722, #35076 ),
 ( #89821, #43158 ),
 ( #12299, #82729 ),
 ( #36067, #66966 ),
 ( #74098, #90327 ),
 ( #18911, #50279 ),
 ( #81231, #58851 ),
 ( #96934, #65981 ),
 ( #27501, #19900 ),
 ( #97404, #74612 ),
 ( #27973, #20397 ) ),
 .UNSPECIFIED., .F., .F., .F.,
 ( 4, 3, 3, 3, 3, 3, 3, 3, 3, 3, 4 ),
 ( 2, 2 ),
 ( 0.000000000000000000, 0.1122669598086711712, 0.2243161639709570498, 0.3396355846219037966, 0.4553962076585047480, 0.5677860799922284096, 0.6749047109689546575, 0.7773884377078235097, 0.8775581155834147884, 0.9782364162377757966, 1.000000000000000000 ),
 ( 0.000000000000000000, 1.000000000000000000 ),
 .UNSPECIFIED. ) ;
#96711 = CARTESIAN_POINT ( 'NONE',  ( 177.1313973275757405, 292.4482777636210926, -2.705817427292956268 ) ) ;
#96713 = CARTESIAN_POINT ( 'NONE',  ( 195.8627871995700502, 291.4026965887302936, 17.41145040657729481 ) ) ;
#96714 = CARTESIAN_POINT ( 'NONE',  ( 159.9894443651313338, 253.5371490153152081, -16.36035038356864391 ) ) ;
#96715 = CARTESIAN_POINT ( 'NONE',  ( 162.9703553142854560, 248.3740597985417935, 10.27208824138328680 ) ) ;
#96716 = CARTESIAN_POINT ( 'NONE',  ( 92.94880205384217220, 212.2202760586659736, -5.415160957724236172E-17 ) ) ;
#96717 = EDGE_LOOP ( 'NONE', ( #96172, #94793, #91551, #78834 ) ) ;
#96718 = VECTOR ( 'NONE', #58727, 1000.000000000000000 ) ;
#96719 = EDGE_LOOP ( 'NONE', ( #82982, #2273 ) ) ;
#96720 = CARTESIAN_POINT ( 'NONE',  ( 6.117390533544194930, 29.33055864014943026, 10.00000000000000000 ) ) ;
#96721 = CARTESIAN_POINT ( 'NONE',  ( 162.6341128535665064, 248.9564488241690299, -10.63508949045170660 ) ) ;
#96722 = ORIENTED_EDGE ( 'NONE', *, *, #75024, .T. ) ;
#96723 = AXIS2_PLACEMENT_3D ( 'NONE', #48041, #86116, #79495 ) ;
#96724 = CARTESIAN_POINT ( 'NONE',  ( 193.2053853833890287, 265.4515565053490604, -7.760948457033734371 ) ) ;
#96725 = CARTESIAN_POINT ( 'NONE',  ( 29.09658290004530556, 18.92755873383627119, 6.180339887498953466 ) ) ;
#96726 = EDGE_CURVE ( 'NONE', #23023, #41212, #77116, .T. ) ;
#96727 = DIRECTION ( 'NONE',  ( 0.000000000000000000, 0.000000000000000000, 1.000000000000000000 ) ) ;
#96729 = CARTESIAN_POINT ( 'NONE',  ( 69.81243019392555027, 62.22010195957142287, -13.63492759933605036 ) ) ;
#96728 = CARTESIAN_POINT ( 'NONE',  ( 134.1932619090760568, 236.0327760586659736, 1.948934522072303157E-15 ) ) ;
#96730 = CARTESIAN_POINT ( 'NONE',  ( 154.8782533782051871, 264.3899914918594050, -17.45241046926759765 ) ) ;
#96731 = ORIENTED_EDGE ( 'NONE', *, *, #97659, .T. ) ;
#96732 = VECTOR ( 'NONE', #75000, 1000.000000000000114 ) ;
#96733 = CARTESIAN_POINT ( 'NONE',  ( 157.3812306876618266, 258.0547076216885785, 17.10114491953027027 ) ) ;
#96734 = CARTESIAN_POINT ( 'NONE',  ( 157.8961455691572837, 274.3508122300142986, 13.06461853355700775 ) ) ;
#96735 = CARTESIAN_POINT ( 'NONE',  ( 82.67311241900212337, 40.57720724764539000, -1.428110901475119432 ) ) ;
#96736 = CARTESIAN_POINT ( 'NONE',  ( 80.47598030042951223, 43.56226889263761848, 9.740817512588815674 ) ) ;
#96737 = CARTESIAN_POINT ( 'NONE',  ( 178.2793323077814591, 285.7144920781913697, 14.42518415939602683 ) ) ;
#96738 = B_SPLINE_CURVE_WITH_KNOTS ( 'NONE', 3,
 ( #51951, #97577, #59523, #28148, #20565, #51444, #67143, #90502, #75263, #21075, #82891, #13465, #44331, #36733, #98572, #29155, #81715, #35573, #42168, #3214, #35066, #88344, #57870, #89339, #56869, #19891, #18394, #57369, #33590, #12796, #49779, #34575, #50763, #64486, #87853, #42655, #27493, #65972 ),
 .UNSPECIFIED., .F., .F.,
 ( 4, 2, 2, 2, 2, 2, 2, 2, 2, 2, 2, 2, 2, 2, 2, 2, 2, 2, 4 ),
 ( 0.0009333477296225796459, 0.001027619387414748084, 0.001121891045206916413, 0.001310434360791252638, 0.001687520991959938314, 0.002441694254297281912, 0.003950040778971889745, 0.004704214041309194745, 0.005081300672477920104, 0.005269843988062358243, 0.005364115645854540017, 0.005458387303646720923, 0.005505523132542770176, 0.005552658961438818562, 0.005646930619230842475, 0.005835473934814966630, 0.006212560565983246165, 0.006589647197151524832, 0.006966733828319804367 ),
 .UNSPECIFIED. ) ;
#96739 = LINE ( 'NONE', #57182, #2897 ) ;
#96740 = EDGE_CURVE ( 'NONE', #32549, #38232, #21037, .T. ) ;
#96741 = CARTESIAN_POINT ( 'NONE',  ( 195.4525600527361746, 279.6603085545519320, -17.06130316034534999 ) ) ;
#96742 = DIRECTION ( 'NONE',  ( -0.8660254037844379305, -0.5000000000000014433, -0.000000000000000000 ) ) ;
#96743 = CARTESIAN_POINT ( 'NONE',  ( 80.50140447660758980, 52.45483312604073234, 15.35925353569622942 ) ) ;
#96744 = AXIS2_PLACEMENT_3D ( 'NONE', #49018, #42874, #33831 ) ;
#96745 = CARTESIAN_POINT ( 'NONE',  ( 206.3512583665959994, 271.5101124371017818, 7.607313674450764118 ) ) ;
#96746 = CARTESIAN_POINT ( 'NONE',  ( 167.7141816491835868, 249.9697211030261883, 6.963387598742469820 ) ) ;
#96747 = CARTESIAN_POINT ( 'NONE',  ( 78.31186438638634684, 61.61641173835174357, 16.15355831358047922 ) ) ;
#96748 = CARTESIAN_POINT ( 'NONE',  ( 188.9122134955663910, 290.7695941481946988, -15.11888497690123678 ) ) ;
#96749 = EDGE_CURVE ( 'NONE', #53524, #88734, #57508, .T. ) ;
#96750 = DIRECTION ( 'NONE',  ( -0.000000000000000000, 0.000000000000000000, -1.000000000000000000 ) ) ;
#96751 = CARTESIAN_POINT ( 'NONE',  ( 36.34934470066777834, 21.39040679176985194, 1.333680081654574804E-15 ) ) ;
#96752 = CARTESIAN_POINT ( 'NONE',  ( 74.26908450914415027, 55.21978062604117099, 16.60372121789527355 ) ) ;
#96753 = CARTESIAN_POINT ( 'NONE',  ( 9.015913755055775525, 20.90829794293878763, 10.00000000000000355 ) ) ;
#96754 = CARTESIAN_POINT ( 'NONE',  ( 36.70787689013189947, 33.14441083166263979, 10.00000000000000533 ) ) ;
#96755 = DIRECTION ( 'NONE',  ( 1.000000000000000000, 0.000000000000000000, 0.000000000000000000 ) ) ;
#96756 = CARTESIAN_POINT ( 'NONE',  ( 160.5496179049985130, 273.2860930542701112, -15.62709310798295803 ) ) ;
#96757 = CARTESIAN_POINT ( 'NONE',  ( 85.64394211879633190, 43.47961218390750560, -4.674786408818643935 ) ) ;
#96758 = CARTESIAN_POINT ( 'NONE',  ( 161.1750406344237661, 251.4836360396366501, -14.21198410781773802 ) ) ;
#96759 = CARTESIAN_POINT ( 'NONE',  ( 10.35128207213630169, 176.7833772461660544, -9.188101187500095079 ) ) ;
#96760 = CARTESIAN_POINT ( 'NONE',  ( 207.1433070480561014, 270.6377863507698294, 3.317773331146615323 ) ) ;
#96761 = ORIENTED_EDGE ( 'NONE', *, *, #92636, .F. ) ;
#96762 = AXIS2_PLACEMENT_3D ( 'NONE', #89690, #42035, #26351 ) ;
#96763 = B_SPLINE_CURVE_WITH_KNOTS ( 'NONE', 3,
 ( #74608, #4687, #27968, #57372 ),
 .UNSPECIFIED., .F., .F.,
 ( 4, 4 ),
 ( 0.005575214141566578116, 0.01056667930948825516 ),
 .UNSPECIFIED. ) ;
#96764 = FACE_OUTER_BOUND ( 'NONE', #28597, .T. ) ;
#96765 = CARTESIAN_POINT ( 'NONE',  ( 33.00325904164698443, 189.8615022471902591, -10.00000000000009592 ) ) ;
#96766 = CARTESIAN_POINT ( 'NONE',  ( 207.6590484093196096, 270.9709728340903894, 3.402057849327809524 ) ) ;
#96767 = CARTESIAN_POINT ( 'NONE',  ( 82.30672826452196489, 41.36268747567339688, 5.465017951912414240 ) ) ;
#96768 = CARTESIAN_POINT ( 'NONE',  ( 36.16949087457737733, 197.8149278399160949, -9.188101187500095079 ) ) ;
#96769 = AXIS2_PLACEMENT_3D ( 'NONE', #100191, #14075, #99187 ) ;
#96770 = CARTESIAN_POINT ( 'NONE',  ( 200.9111546617170916, 282.6586676490145464, 17.66063511622358106 ) ) ;
#96771 = CARTESIAN_POINT ( 'NONE',  ( 147.5813496936708020, 275.0285994114094592, 4.516581957185684004 ) ) ;
#96772 = CARTESIAN_POINT ( 'NONE',  ( 28.69010979082973023, 40.65659080271451842, -1.878358725466461243E-16 ) ) ;
#96773 = CARTESIAN_POINT ( 'NONE',  ( 183.7975612849717777, 256.6346208101135176, -2.981236333899912161 ) ) ;
#96774 = CARTESIAN_POINT ( 'NONE',  ( 191.4082244002820516, 299.1182256826033949, -8.271837126846561361 ) ) ;
#96775 = VECTOR ( 'NONE', #96558, 1000.000000000000227 ) ;
#96776 = CARTESIAN_POINT ( 'NONE',  ( 179.7576857715609435, 278.6407688031329712, -16.34641460967070259 ) ) ;
#96777 = CARTESIAN_POINT ( 'NONE',  ( 72.79498119441143444, 67.60180456977322194, -11.11215744783703308 ) ) ;
#96778 = B_SPLINE_CURVE_WITH_KNOTS ( 'NONE', 3,
 ( #75927, #30295, #82556, #28292, #44483, #76415, #45481, #83038, #90140, #98218, #5998, #29796, #68288, #22703, #99706, #6506 ),
 .UNSPECIFIED., .F., .F.,
 ( 4, 2, 2, 2, 2, 2, 2, 4 ),
 ( 3.469446951953614189E-18, 0.0003787177898466141516, 0.0007574355796932248338, 0.001136153369539835353, 0.001514871159386446198, 0.001893588949233056826, 0.002272306739079667237, 0.003029742318772781808 ),
 .UNSPECIFIED. ) ;
#96779 = ADVANCED_FACE ( 'NONE', ( #11935 ), #75227, .T. ) ;
#96780 = VECTOR ( 'NONE', #29819, 1000.000000000000114 ) ;
#96781 = EDGE_CURVE ( 'NONE', #81326, #83225, #88997, .T. ) ;
#96782 = CARTESIAN_POINT ( 'NONE',  ( 11.76667899187106059, 31.90941714274742580, -10.00000000000000000 ) ) ;
#96783 = LINE ( 'NONE', #50618, #7854 ) ;
#96784 =( GEOMETRIC_REPRESENTATION_CONTEXT ( 3 ) GLOBAL_UNCERTAINTY_ASSIGNED_CONTEXT ( ( #2784 ) ) GLOBAL_UNIT_ASSIGNED_CONTEXT ( ( #94636, #88064, #87068 ) ) REPRESENTATION_CONTEXT ( 'NONE', 'WORKASPACE' ) );
#96785 = CARTESIAN_POINT ( 'NONE',  ( 86.26382137439000530, 210.6115022471902023, -5.000000000000041744 ) ) ;
#96786 = FACE_OUTER_BOUND ( 'NONE', #58109, .T. ) ;
#96787 = CARTESIAN_POINT ( 'NONE',  ( 36.09163463545626627, 29.03677371833803988, 10.00000000000000533 ) ) ;
#96788 = ORIENTED_EDGE ( 'NONE', *, *, #78042, .F. ) ;
#96789 = CARTESIAN_POINT ( 'NONE',  ( 49.51212862133765213, 190.2048013555409796, 4.594050593750051981 ) ) ;
#96790 = ORIENTED_EDGE ( 'NONE', *, *, #36113, .T. ) ;
#96791 = CARTESIAN_POINT ( 'NONE',  ( -9.674045898528673249, 85.30406559775344988, 14.22504367373031364 ) ) ;
#96792 = CARTESIAN_POINT ( 'NONE',  ( 150.7850480413316632, 269.4796311011364764, -14.43114374163211089 ) ) ;
#96793 = CARTESIAN_POINT ( 'NONE',  ( 67.00800788680665221, 66.91027394849365351, -8.787034667612781291 ) ) ;
#96794 = ADVANCED_FACE ( 'NONE', ( #4308 ), #27635, .T. ) ;
#96795 = ORIENTED_EDGE ( 'NONE', *, *, #99560, .T. ) ;
#96796 = CARTESIAN_POINT ( 'NONE',  ( 171.3574066310837054, 286.5369029633047830, 8.062752042993464485 ) ) ;
#96797 = CARTESIAN_POINT ( 'NONE',  ( 206.9377610035629118, 272.2202792677204002, 7.440532334334675646 ) ) ;
#96798 = CARTESIAN_POINT ( 'NONE',  ( 192.7288556637334125, 292.1918731402626577, -15.52061534916644447 ) ) ;
#96799 = CARTESIAN_POINT ( 'NONE',  ( 25.29680607046014984, 36.64646525600391413, -2.839279412974133887 ) ) ;
#96800 = CARTESIAN_POINT ( 'NONE',  ( 185.9360266901250043, 262.9690012174675076, 11.35307557420283686 ) ) ;
#96801 = CARTESIAN_POINT ( 'NONE',  ( 196.3174919959537306, 290.6151247789487684, -17.61248417473235151 ) ) ;
#96802 = CARTESIAN_POINT ( 'NONE',  ( 171.4894766845286540, 255.7030988890395236, 11.23559410916937296 ) ) ;
#96803 = ORIENTED_EDGE ( 'NONE', *, *, #24300, .F. ) ;
#96804 = CARTESIAN_POINT ( 'NONE',  ( 19.64056747690256088, 19.84335787977762777, 9.188101187500006262 ) ) ;
#96805 = CARTESIAN_POINT ( 'NONE',  ( 82.86586985908988368, 152.2544130683315871, 0.000000000000000000 ) ) ;
#96806 = CARTESIAN_POINT ( 'NONE',  ( 174.8283672253976704, 255.1773154208834455, 8.220612995860930639 ) ) ;
#96807 = CARTESIAN_POINT ( 'NONE',  ( 11.58252532646001498, 30.18528772668517135, -1.583844403245363575 ) ) ;
#96808 = EDGE_CURVE ( 'NONE', #47657, #8304, #6961, .T. ) ;
#96809 = ORIENTED_EDGE ( 'NONE', *, *, #2279, .F. ) ;
#96810 = CARTESIAN_POINT ( 'NONE',  ( 182.4154252063833894, 284.1042553539095366, 14.98678786608993185 ) ) ;
#96811 = CARTESIAN_POINT ( 'NONE',  ( 151.4361976351029000, 268.3518069213970421, 15.15218985681980612 ) ) ;
#96812 = CARTESIAN_POINT ( 'NONE',  ( 172.7371573690596449, 271.6299009131761864, 17.79590902495428040 ) ) ;
#96813 = VERTEX_POINT ( 'NONE', #20032 ) ;
#96814 = VECTOR ( 'NONE', #55992, 1000.000000000000000 ) ;
#96816 = CARTESIAN_POINT ( 'NONE',  ( 151.1237910559533475, 270.8929109891034841, -13.93008610078706688 ) ) ;
#96815 = CARTESIAN_POINT ( 'NONE',  ( 161.8150574665248200, 250.3750943687383881, -13.25074899737357903 ) ) ;
#96817 = CARTESIAN_POINT ( 'NONE',  ( 149.0164813726494799, 272.5428784278667536, -11.67305721329070423 ) ) ;
#96818 = ORIENTED_EDGE ( 'NONE', *, *, #35158, .F. ) ;
#96819 = CARTESIAN_POINT ( 'NONE',  ( 197.8822014719394531, 287.9049684674569676, 17.88172308374019792 ) ) ;
#96820 = DIRECTION ( 'NONE',  ( -0.6303371332823576312, -0.7763215174174805666, 0.000000000000000000 ) ) ;
#96821 = CARTESIAN_POINT ( 'NONE',  ( 77.96041703586088545, 62.15569039082562597, -15.98643159653562940 ) ) ;
#96822 = CARTESIAN_POINT ( 'NONE',  ( 198.0036776755666210, 286.8752984553728993, 16.94019974494662861 ) ) ;
#96823 = CARTESIAN_POINT ( 'NONE',  ( 114.8152493078691947, 249.3464784336662206, 1.353441290958777525E-15 ) ) ;
#96824 = CARTESIAN_POINT ( 'NONE',  ( 112.6775961898153184, 245.8615022471903160, 5.000000000000046185 ) ) ;
#96825 = CARTESIAN_POINT ( 'NONE',  ( 27.64472685218281711, 196.7677522451419350, -5.000000000000047962 ) ) ;
#96826 = ORIENTED_EDGE ( 'NONE', *, *, #19477, .T. ) ;
#96827 = CARTESIAN_POINT ( 'NONE',  ( 163.7587049410067266, 247.0085981909329576, -6.137518685179130351 ) ) ;
#96828 = EDGE_LOOP ( 'NONE', ( #80610, #37691, #78319, #1080 ) ) ;
#96829 = CARTESIAN_POINT ( 'NONE',  ( 30.25658917092484756, 35.65586893147758474, -7.433330006724137462 ) ) ;
#96830 = CARTESIAN_POINT ( 'NONE',  ( 159.5204760365350012, 254.3494259875849082, 16.90107507090185379 ) ) ;
#96831 = CARTESIAN_POINT ( 'NONE',  ( 75.16089758350406669, 66.39091360267232744, -13.15879276033818535 ) ) ;
#96832 = CARTESIAN_POINT ( 'NONE',  ( 72.86731735994297310, 219.0024278399160949, -9.188101187500093303 ) ) ;
#96833 = CARTESIAN_POINT ( 'NONE',  ( 172.1774115781176420, 284.2304136030405743, 13.05068545833847438 ) ) ;
#96834 = CARTESIAN_POINT ( 'NONE',  ( 150.8888667059421209, 269.2998118992572927, 15.79021133717968617 ) ) ;
#96835 = CARTESIAN_POINT ( 'NONE',  ( 193.8913555215501390, 294.8173164187117550, 15.40725395879721837 ) ) ;
#96836 = CARTESIAN_POINT ( 'NONE',  ( -13.76211276271269668, 162.8615022471902591, -10.00000000000007816 ) ) ;
#96837 = ORIENTED_EDGE ( 'NONE', *, *, #55293, .T. ) ;
#96838 = CARTESIAN_POINT ( 'NONE',  ( 82.41933087055697627, 40.38430946167127189, -0.8419157719606927825 ) ) ;
#96839 = CARTESIAN_POINT ( 'NONE',  ( 203.4696564630250464, 278.2272125378923988, -16.38980782817167636 ) ) ;
#96840 = CIRCLE ( 'NONE', #95256, 1.449999999999994627 ) ;
#96841 = ORIENTED_EDGE ( 'NONE', *, *, #19363, .F. ) ;
#96842 = CARTESIAN_POINT ( 'NONE',  ( 148.6255488361104540, 273.2199934434842703, 9.123621776406645623 ) ) ;
#96843 = CARTESIAN_POINT ( 'NONE',  ( -79.28667360730980818, 56.40661347651924729, 177.5919119679930134 ) ) ;
#96844 = CARTESIAN_POINT ( 'NONE',  ( 163.9093945587947587, 260.4689496177562091, -16.17298052259348040 ) ) ;
#96845 = CARTESIAN_POINT ( 'NONE',  ( 207.3589495855971450, 271.0586446502292119, 2.456771036675355457 ) ) ;
#96846 = CIRCLE ( 'NONE', #27313, 70.00000000000001421 ) ;
#96847 = CARTESIAN_POINT ( 'NONE',  ( 79.05688537879109390, 48.64051310273040230, 14.69164152319516425 ) ) ;
#96848 = CARTESIAN_POINT ( 'NONE',  ( 206.3907062969896060, 273.1678058140250300, 11.56942460516550675 ) ) ;
#96849 = EDGE_CURVE ( 'NONE', #28117, #100032, #58972, .T. ) ;
#96850 = CARTESIAN_POINT ( 'NONE',  ( 206.5571822944673670, 272.8794609281530938, 10.95833005210827515 ) ) ;
#96851 = LINE ( 'NONE', #3625, #75243 ) ;
#96852 = CARTESIAN_POINT ( 'NONE',  ( -70.00000000000000000, 20.00000000000000000, -59.99999999999999289 ) ) ;
#96853 = DIRECTION ( 'NONE',  ( 1.000000000000000000, 1.804112415015878984E-15, -1.082076799516502204E-16 ) ) ;
#96854 = AXIS2_PLACEMENT_3D ( 'NONE', #13203, #91214, #82138 ) ;
#96855 = CARTESIAN_POINT ( 'NONE',  ( 123.6384037525706958, 236.0643266524160140, 9.188101187500095079 ) ) ;
#96856 = VERTEX_POINT ( 'NONE', #44789 ) ;
#96857 = CARTESIAN_POINT ( 'NONE',  ( 83.38112233772677939, 44.18327968967634689, -8.473636281462212594 ) ) ;
#96858 = DIRECTION ( 'NONE',  ( 0.5270369400482041167, 0.8498423758701525443, 0.000000000000000000 ) ) ;
#96859 = ADVANCED_FACE ( 'NONE', ( #31087 ), #6806, .T. ) ;
#96860 = CARTESIAN_POINT ( 'NONE',  ( 172.2601350562971447, 284.0070134640075139, -13.26565049143300712 ) ) ;
#96861 = PLANE ( 'NONE',  #56445 ) ;
#96862 = CARTESIAN_POINT ( 'NONE',  ( 73.81300068619336230, 56.52063054796119701, 16.05668348448922345 ) ) ;
#96863 = LINE ( 'NONE', #27431, #95571 ) ;
#96864 = EDGE_LOOP ( 'NONE', ( #75592, #20855, #25665, #31833 ) ) ;
#96865 = CARTESIAN_POINT ( 'NONE',  ( 77.05652628499306900, 57.63148023862245850, 16.16682221975541722 ) ) ;
#96866 = AXIS2_PLACEMENT_3D ( 'NONE', #61083, #46372, #77302 ) ;
#96867 = CARTESIAN_POINT ( 'NONE',  ( -50.81821011400020183, 81.52126639084015380, -10.00000000000000000 ) ) ;
#96868 = CARTESIAN_POINT ( 'NONE',  ( 164.3284847670581144, 246.0217105830841433, -2.055838629128057704 ) ) ;
#96869 = CARTESIAN_POINT ( 'NONE',  ( 139.4158702080621879, 260.4869531367911009, 4.594050593750046652 ) ) ;
#96870 = ADVANCED_FACE ( 'NONE', ( #91953 ), #29610, .F. ) ;
#96871 = CARTESIAN_POINT ( 'NONE',  ( 190.5653282632609091, 300.5781646174276602, -5.775635208185608604 ) ) ;
#96872 = DIRECTION ( 'NONE',  ( -1.000000000000000000, 0.000000000000000000, 0.000000000000000000 ) ) ;
#96873 = CARTESIAN_POINT ( 'NONE',  ( 157.0877926458200307, 258.5629572190321710, -17.40668770468195703 ) ) ;
#96874 = CARTESIAN_POINT ( 'NONE',  ( 172.0768229479522518, 251.2702533327793049, 3.412387498982429879 ) ) ;
#96875 = EDGE_CURVE ( 'NONE', #20065, #130, #17935, .T. ) ;
#96876 = CARTESIAN_POINT ( 'NONE',  ( 18.32728854387591610, 18.78052372038640172, -10.00000000000000355 ) ) ;
#96877 = ADVANCED_FACE ( 'NONE', ( #21516 ), #99024, .T. ) ;
#96878 = DIRECTION ( 'NONE',  ( 0.9890802632347824863, -0.1473778574936323582, 0.000000000000000000 ) ) ;
#96879 = CARTESIAN_POINT ( 'NONE',  ( 155.4178462578491917, 279.7076410523796994, -1.474083510808620767 ) ) ;
#96880 = CARTESIAN_POINT ( 'NONE',  ( 169.1881285547887899, 285.4409231072398256, -9.045257849526111116 ) ) ;
#96881 = CARTESIAN_POINT ( 'NONE',  ( 163.7166294601506991, 282.3380383384618995, 10.03031969300557513 ) ) ;
#96882 = CARTESIAN_POINT ( 'NONE',  ( 193.7377806475841737, 288.6157489428582039, 16.07307194723800947 ) ) ;
#96883 = VECTOR ( 'NONE', #44600, 1000.000000000000000 ) ;
#96884 = CARTESIAN_POINT ( 'NONE',  ( 134.1658515176688411, 248.2677522451418497, 10.00000000000009592 ) ) ;
#96885 = CARTESIAN_POINT ( 'NONE',  ( 182.9478530203177797, 278.8618512465640720, 17.45115622927625409 ) ) ;
#96886 = ORIENTED_EDGE ( 'NONE', *, *, #98732, .T. ) ;
#96887 = CARTESIAN_POINT ( 'NONE',  ( 157.7365441389748923, 257.4392866714015895, 18.13124212464487073 ) ) ;
#96888 = CARTESIAN_POINT ( 'NONE',  ( 190.6036479972031259, 300.5117928913073797, -0.6824572005520307405 ) ) ;
#96889 = CARTESIAN_POINT ( 'NONE',  ( -6.509410329615746171, 176.2369531367911293, -4.594050593750048428 ) ) ;
#96890 = AXIS2_PLACEMENT_3D ( 'NONE', #17334, #68165, #61555 ) ;
#96891 = CARTESIAN_POINT ( 'NONE',  ( 42.47567221558909267, 186.1423013555410080, -4.594050593750043987 ) ) ;
#96892 = CARTESIAN_POINT ( 'NONE',  ( 179.0685761320505947, 258.5468394390073286, -11.57600102548048149 ) ) ;
#96893 = CARTESIAN_POINT ( 'NONE',  ( 22.75024936130811426, 12.94473085651391742, 1.475505719884397138E-15 ) ) ;
#96894 = CARTESIAN_POINT ( 'NONE',  ( 67.91028321870373929, 65.38586328950580651, -10.41284464168438006 ) ) ;
#96895 = CARTESIAN_POINT ( 'NONE',  ( 205.2414727015710412, 275.1583367910551488, -12.71338796362297963 ) ) ;
#96896 = CARTESIAN_POINT ( 'NONE',  ( 192.5408418301696827, 292.3122096881645575, -14.34927581417471032 ) ) ;
#96897 = PLANE ( 'NONE',  #14114 ) ;
#96898 = CARTESIAN_POINT ( 'NONE',  ( 73.89677966998817737, 55.37416586069887359, -16.11664339955940761 ) ) ;
#96899 = EDGE_CURVE ( 'NONE', #16029, #44653, #61492, .T. ) ;
#96900 = CARTESIAN_POINT ( 'NONE',  ( 170.2584372531675285, 258.0169095780440216, 13.81827105252718191 ) ) ;
#96901 = CARTESIAN_POINT ( 'NONE',  ( -42.74117156905490589, 79.73515388767964396, 36.50000000000000000 ) ) ;
#96902 = CARTESIAN_POINT ( 'NONE',  ( 166.1251398123678769, 278.2158936690458972, 14.79076461835531831 ) ) ;
#96903 = CARTESIAN_POINT ( 'NONE',  ( 162.1420711923595945, 252.0453937043351971, -13.78871268869485966 ) ) ;
#96904 = ADVANCED_FACE ( 'NONE', ( #60483 ), #64514, .T. ) ;
#96905 = CARTESIAN_POINT ( 'NONE',  ( 40.72531889205820477, 200.9865022471903160, -10.00000000000009415 ) ) ;
#96906 = CARTESIAN_POINT ( 'NONE',  ( 182.3148671385995954, 291.9086626978152594, 9.339946855409639426 ) ) ;
#96907 = CARTESIAN_POINT ( 'NONE',  ( 189.8147415777049218, 301.8782188922952514, -0.5019643756309712934 ) ) ;
#96908 = CARTESIAN_POINT ( 'NONE',  ( -0.2035760843690503918, 176.8149278399160949, -9.188101187500095079 ) ) ;
#96909 = CARTESIAN_POINT ( 'NONE',  ( 168.2775622310419976, 286.2832889018337141, 4.256419143223407531 ) ) ;
#96910 = LINE ( 'NONE', #65464, #27416 ) ;
#96911 = CARTESIAN_POINT ( 'NONE',  ( 32.83301474718356161, 37.14336893147758900, 7.433330006724141015 ) ) ;
#96912 = CARTESIAN_POINT ( 'NONE',  ( 164.9356397357043704, 244.9700873293209042, 2.799217332519396972 ) ) ;
#96914 = CARTESIAN_POINT ( 'NONE',  ( 179.3501926571443335, 277.5838325412013887, 16.80239616393437885 ) ) ;
#96913 = AXIS2_PLACEMENT_3D ( 'NONE', #57968, #42748, #80319 ) ;
#96915 = EDGE_CURVE ( 'NONE', #66013, #91598, #16397, .T. ) ;
#96916 = CARTESIAN_POINT ( 'NONE',  ( 193.7118145980225279, 295.1282904202991517, 14.61271143546694162 ) ) ;
#96917 = CARTESIAN_POINT ( 'NONE',  ( 73.77862180316432728, 206.7365022471902023, 10.00000000000009948 ) ) ;
#96918 = CARTESIAN_POINT ( 'NONE',  ( -19.65312891409030271, 93.06504152958497400, -45.00000000000001421 ) ) ;
#96919 = AXIS2_PLACEMENT_3D ( 'NONE', #57647, #89133, #96701 ) ;
#96920 = CARTESIAN_POINT ( 'NONE',  ( 6.618913549016022912, 24.79752408145590081, -5.678558825948271327 ) ) ;
#96921 = CARTESIAN_POINT ( 'NONE',  ( 165.6714170802892454, 285.4141558977842692, 0.4680648764968557973 ) ) ;
#96922 = CARTESIAN_POINT ( 'NONE',  ( 20.82171660429349558, 14.94754757982089366, 5.678558825948272215 ) ) ;
#96923 = CARTESIAN_POINT ( 'NONE',  ( 2.064617007569734319, 27.83817977871672511, -10.00000000000000000 ) ) ;
#96924 = EDGE_CURVE ( 'NONE', #48903, #70099, #63997, .T. ) ;
#96925 = LINE ( 'NONE', #66471, #12810 ) ;
#96926 = ORIENTED_EDGE ( 'NONE', *, *, #70067, .F. ) ;
#96927 = AXIS2_PLACEMENT_3D ( 'NONE', #9419, #32208, #63114 ) ;
#96928 = CARTESIAN_POINT ( 'NONE',  ( 24.66009930550170282, 22.43677371833801715, -10.00000000000000355 ) ) ;
#96929 = ADVANCED_FACE ( 'NONE', ( #40179 ), #85871, .F. ) ;
#96930 = CARTESIAN_POINT ( 'NONE',  ( 19.98788723728717898, 104.4047874917408336, 22.50000000000002132 ) ) ;
#96931 = ORIENTED_EDGE ( 'NONE', *, *, #76717, .T. ) ;
#96932 = DIRECTION ( 'NONE',  ( -0.8660254037844387076, -0.4999999999999998890, -0.000000000000000000 ) ) ;
#96933 = CARTESIAN_POINT ( 'NONE',  ( 164.3138894970802824, 246.0469903322357368, -2.642126690130961020 ) ) ;
#96934 = CARTESIAN_POINT ( 'NONE',  ( 66.55830361311562626, 68.75215758827378920, 4.754528328751027821 ) ) ;
#96935 = CARTESIAN_POINT ( 'NONE',  ( 87.57478309584621456, 45.08285526713719094, 6.924932389716523140 ) ) ;
#96936 = ORIENTED_EDGE ( 'NONE', *, *, #26318, .T. ) ;
#96937 = AXIS2_PLACEMENT_3D ( 'NONE', #39168, #70082, #695 ) ;
#96938 = ORIENTED_EDGE ( 'NONE', *, *, #75938, .F. ) ;
#96940 = CARTESIAN_POINT ( 'NONE',  ( 80.93613592869992601, 42.95327845849681836, -9.503115154567232992 ) ) ;
#96939 = CARTESIAN_POINT ( 'NONE',  ( 165.2177353524737953, 246.3385600597696623, -4.395826225581572544 ) ) ;
#96941 = CARTESIAN_POINT ( 'NONE',  ( 192.2431834237441706, 297.6720342317289578, 11.07782187406058938 ) ) ;
#96942 = EDGE_LOOP ( 'NONE', ( #22622, #48856, #3611, #6191 ) ) ;
#96943 = CARTESIAN_POINT ( 'NONE',  ( 77.06387632225415985, 54.00152061585258423, 16.01168232074038400 ) ) ;
#96944 = CARTESIAN_POINT ( 'NONE',  ( 176.9918222592760912, 263.5879201535869925, 14.48983262399754324 ) ) ;
#96945 = ORIENTED_EDGE ( 'NONE', *, *, #72996, .F. ) ;
#96946 = CARTESIAN_POINT ( 'NONE',  ( 31.53257425345116260, 33.90829794293883026, 10.00000000000000355 ) ) ;
#96947 = CARTESIAN_POINT ( 'NONE',  ( 88.53016884517781193, 43.88792164385783678, -0.09627500500477675915 ) ) ;
#96948 = B_SPLINE_CURVE_WITH_KNOTS ( 'NONE', 3,
 ( #45459, #85003, #84511, #30777, #83515, #15055, #7981, #21680, #76863, #45946, #23154, #44460, #38352, #61658, #14076, #84022, #75392, #60151 ),
 .UNSPECIFIED., .F., .F.,
 ( 4, 2, 2, 2, 2, 2, 2, 2, 4 ),
 ( 0.003618221803335557821, 0.003736881880739065936, 0.003855541958142574051, 0.003974202035546082167, 0.004092862112949589848, 0.004330182267756606078, 0.004567502422563622308, 0.005516783041791769628, 0.007415344280248136258 ),
 .UNSPECIFIED. ) ;
#96949 = VECTOR ( 'NONE', #75044, 1000.000000000000114 ) ;
#96950 = CARTESIAN_POINT ( 'NONE',  ( 180.4139436811555299, 273.2462330171467215, 17.76112568380599654 ) ) ;
#96951 = ORIENTED_EDGE ( 'NONE', *, *, #24320, .F. ) ;
#96952 = CARTESIAN_POINT ( 'NONE',  ( 203.0008710209992273, 267.9386651392713929, 2.532706327771747645 ) ) ;
#96953 = CARTESIAN_POINT ( 'NONE',  ( 169.4554350835716150, 276.4675945671627915, -15.95358343529382950 ) ) ;
#96954 = CARTESIAN_POINT ( 'NONE',  ( 73.42974959722798189, 58.60376009667394470, 15.71314503368921223 ) ) ;
#96955 = PRODUCT_DEFINITION_SHAPE ( 'NONE', 'NONE',  #100302 ) ;
#96956 = ORIENTED_EDGE ( 'NONE', *, *, #4337, .F. ) ;
#96957 = CARTESIAN_POINT ( 'NONE',  ( 174.4395595858021579, 277.0650199303285035, -15.70439895477656123 ) ) ;
#96958 = CARTESIAN_POINT ( 'NONE',  ( 170.3633989215723545, 262.4553760836484457, -15.63040615342705486 ) ) ;
#96959 = EDGE_LOOP ( 'NONE', ( #15852, #18913, #30603, #73724 ) ) ;
#96960 = FACE_OUTER_BOUND ( 'NONE', #90785, .T. ) ;
#96961 = ORIENTED_EDGE ( 'NONE', *, *, #74590, .T. ) ;
#96962 = FACE_OUTER_BOUND ( 'NONE', #68481, .T. ) ;
#96963 = ORIENTED_EDGE ( 'NONE', *, *, #38847, .F. ) ;
#96964 = DIRECTION ( 'NONE',  ( -0.8660254037844384856, -0.5000000000000002220, -3.252519625699449945E-16 ) ) ;
#96965 = CARTESIAN_POINT ( 'NONE',  ( 147.6079937265279511, 274.9824505927824134, 7.417156936634978770 ) ) ;
#96966 = CARTESIAN_POINT ( 'NONE',  ( 188.9510948051018602, 298.8071002461200578, -4.271560164622560940 ) ) ;
#96967 = DIRECTION ( 'NONE',  ( -0.9439450758449140499, 0.3301025504114431519, 0.000000000000000000 ) ) ;
#96968 = CARTESIAN_POINT ( 'NONE',  ( 152.6656396574222754, 266.2223508737794759, 17.04346597795114349 ) ) ;
#96969 = B_SPLINE_CURVE_WITH_KNOTS ( 'NONE', 3,
 ( #39746, #33559, #18364, #41638, #87825, #49259, #80195, #3187 ),
 .UNSPECIFIED., .F., .F.,
 ( 4, 2, 2, 4 ),
 ( 0.0003401861652890088511, 0.0006945731674992995652, 0.0008717666686044522406, 0.001048960169709604916 ),
 .UNSPECIFIED. ) ;
#96970 = CARTESIAN_POINT ( 'NONE',  ( 28.76880349826970473, 198.9637435831425023, 2.679491924311251605 ) ) ;
#96971 = CARTESIAN_POINT ( 'NONE',  ( 158.3286259501534232, 256.4137708922029333, -16.88280927543103616 ) ) ;
#96972 = ORIENTED_EDGE ( 'NONE', *, *, #15571, .T. ) ;
#96973 = CARTESIAN_POINT ( 'NONE',  ( 78.05978962947867217, 56.61574962749410389, -16.20259432744737538 ) ) ;
#96974 = CARTESIAN_POINT ( 'NONE',  ( 206.5571822944673670, 272.8794609281530938, 10.95833005210827515 ) ) ;
#96975 = CARTESIAN_POINT ( 'NONE',  ( 182.2991478702006134, 275.2734891516705034, -17.80812521087705846 ) ) ;
#96977 = ORIENTED_EDGE ( 'NONE', *, *, #63283, .F. ) ;
#96976 = CARTESIAN_POINT ( 'NONE',  ( 159.9014600375868440, 253.6895423408921886, 15.57825579621527368 ) ) ;
#96978 = ORIENTED_EDGE ( 'NONE', *, *, #73160, .F. ) ;
#96979 = CARTESIAN_POINT ( 'NONE',  ( 147.3872053751516944, 275.3648672350856259, -2.900151178210554015 ) ) ;
#96980 = CARTESIAN_POINT ( 'NONE',  ( 196.2350291401047571, 264.4780031501763347, 5.359379669934941859 ) ) ;
#96981 = CARTESIAN_POINT ( 'NONE',  ( 163.5475621151755661, 247.8473668945463828, 8.020086546505606151 ) ) ;
#96982 = CARTESIAN_POINT ( 'NONE',  ( 9.850474518891140008, 29.18528772668516424, -1.583844403245363575 ) ) ;
#96983 = CARTESIAN_POINT ( 'NONE',  ( 199.0447321067873361, 285.8914063425450536, -17.01815350566629448 ) ) ;
#96984 = LINE ( 'NONE', #50330, #28849 ) ;
#96985 = ORIENTED_EDGE ( 'NONE', *, *, #66377, .F. ) ;
#96986 = CARTESIAN_POINT ( 'NONE',  ( 167.2496274829885294, 252.8828136207999648, -12.23857971285498181 ) ) ;
#96987 = DIRECTION ( 'NONE',  ( 0.000000000000000000, 0.000000000000000000, 1.000000000000000000 ) ) ;
#96988 = CARTESIAN_POINT ( 'NONE',  ( 2.487887237287232711, 134.7156766241960497, 21.50000000000007461 ) ) ;
#96989 = AXIS2_PLACEMENT_3D ( 'NONE', #11189, #42056, #50648 ) ;
#96990 = CARTESIAN_POINT ( 'NONE',  ( 206.8986117509267899, 272.2880877623646825, 6.975890063856878598 ) ) ;
#96991 = CARTESIAN_POINT ( 'NONE',  ( 25.47966334272171807, 195.5177522451419350, 5.000000000000046185 ) ) ;
#96992 = CARTESIAN_POINT ( 'NONE',  ( 111.1892885731693923, 228.8768266524159856, -9.188101187500093303 ) ) ;
#96993 = ADVANCED_FACE ( 'NONE', ( #47289 ), #79252, .F. ) ;
#96994 = CARTESIAN_POINT ( 'NONE',  ( 182.6307980359219982, 295.3544251836937065, -2.669455251163955101 ) ) ;
#96995 = VECTOR ( 'NONE', #93931, 1000.000000000000000 ) ;
#96996 = CARTESIAN_POINT ( 'NONE',  ( 162.7915066255068837, 249.6040781700690161, -11.20594800013087067 ) ) ;
#96997 = LINE ( 'NONE', #80809, #71226 ) ;
#96998 = CARTESIAN_POINT ( 'NONE',  ( -105.0000000000000000, 0.000000000000000000, 59.99999999999999289 ) ) ;
#96999 = CARTESIAN_POINT ( 'NONE',  ( 17.82075117977708700, 181.0958772461660544, -9.188101187500095079 ) ) ;
#97000 = CARTESIAN_POINT ( 'NONE',  ( -62.95439910331221256, 68.06504152958493137, 20.00000000000000355 ) ) ;
#97001 = VERTEX_POINT ( 'NONE', #10310 ) ;
#97002 = VERTEX_POINT ( 'NONE', #56392 ) ;
#97003 = CARTESIAN_POINT ( 'NONE',  ( 14.11247099069668742, 31.08080186712592052, -3.090169943749475845 ) ) ;
#97004 = CARTESIAN_POINT ( 'NONE',  ( 147.4751173256875632, 275.5971820653270470, -0.1352375326296694491 ) ) ;
#97005 = ADVANCED_FACE ( 'NONE', ( #78717 ), #87388, .T. ) ;
#97006 = CARTESIAN_POINT ( 'NONE',  ( 71.28802077240882795, 71.71698159252220250, -1.887932162199749575 ) ) ;
#97007 = EDGE_CURVE ( 'NONE', #36817, #4740, #36019, .T. ) ;
#97008 = CARTESIAN_POINT ( 'NONE',  ( 193.3043481395981189, 264.0380534965367474, -4.339446791620638955 ) ) ;
#97009 = VECTOR ( 'NONE', #46020, 1000.000000000000000 ) ;
#97010 = CARTESIAN_POINT ( 'NONE',  ( 185.1858115004773140, 285.9426224659952140, 15.27411408704069729 ) ) ;
#97011 = CARTESIAN_POINT ( 'NONE',  ( 74.05623475345208817, 67.87786276047000911, -11.59565021290447362 ) ) ;
#97012 = CARTESIAN_POINT ( 'NONE',  ( 46.20988612576196175, 206.6744531367911009, 4.594050593750047540 ) ) ;
#97013 = CARTESIAN_POINT ( 'NONE',  ( 93.82350145804367969, 231.6427522451419065, -10.00000000000009415 ) ) ;
#97014 = EDGE_LOOP ( 'NONE', ( #10185, #41550, #55014, #2029, #88398 ) ) ;
#97015 = CARTESIAN_POINT ( 'NONE',  ( 78.98660877947108361, 59.42842565914680364, -16.52762269555200447 ) ) ;
#97016 = CARTESIAN_POINT ( 'NONE',  ( 181.6949246677837664, 260.6778951557793675, -10.47883949846568541 ) ) ;
#97017 = AXIS2_PLACEMENT_3D ( 'NONE', #79968, #49034, #77036 ) ;
#97018 = CARTESIAN_POINT ( 'NONE',  ( -5.751638101304356709, 176.6744531367911293, 4.594050593750047540 ) ) ;
#97019 = CARTESIAN_POINT ( 'NONE',  ( 72.79894534421404728, 70.83549005279604671, -7.921956013610877534 ) ) ;
#97020 = CARTESIAN_POINT ( 'NONE',  ( 199.1867231605587278, 285.6454706231928071, -17.41989184023605475 ) ) ;
#97021 = LINE ( 'NONE', #66568, #48354 ) ;
#97022 = CARTESIAN_POINT ( 'NONE',  ( 146.8312060062178830, 276.3278863910550172, -4.807241325481028227 ) ) ;
#97023 = DIRECTION ( 'NONE',  ( -0.000000000000000000, -1.000000000000000000, -0.000000000000000000 ) ) ;
#97024 = LINE ( 'NONE', #20490, #20749 ) ;
#97025 = CARTESIAN_POINT ( 'NONE',  ( 69.07701453075964082, 68.10981339309213922, 7.918463574440547603 ) ) ;
#97026 = CARTESIAN_POINT ( 'NONE',  ( 164.5867587387928950, 245.5743669417666126, -3.022048486790635202 ) ) ;
#97027 = ORIENTED_EDGE ( 'NONE', *, *, #28507, .T. ) ;
#97028 = EDGE_CURVE ( 'NONE', #90758, #74996, #32123, .T. ) ;
#97029 = CARTESIAN_POINT ( 'NONE',  ( -0.6995629222973920314, 163.7365022471902023, -10.00000000000009059 ) ) ;
#97030 = DIRECTION ( 'NONE',  ( -0.000000000000000000, -0.000000000000000000, -1.000000000000000000 ) ) ;
#97031 = CARTESIAN_POINT ( 'NONE',  ( 118.9560200436548314, 248.6744531367911293, 4.594050593750047540 ) ) ;
#97032 = CARTESIAN_POINT ( 'NONE',  ( 22.15746398174156440, 34.83396525600390703, -2.839279412974133887 ) ) ;
#97033 = CARTESIAN_POINT ( 'NONE',  ( 186.3061762155872714, 258.1895346003614122, -3.525132546332560235 ) ) ;
#97034 = LINE ( 'NONE', #34680, #59706 ) ;
#97036 = CARTESIAN_POINT ( 'NONE',  ( 74.62796085038830540, 66.91441896689961766, 13.03852793085608219 ) ) ;
#97035 = CARTESIAN_POINT ( 'NONE',  ( 17.55280445478281592, 33.77154675864928635, 10.00000000000000000 ) ) ;
#97037 = EDGE_CURVE ( 'NONE', #91958, #7762, #49323, .T. ) ;
#97038 = CARTESIAN_POINT ( 'NONE',  ( 22.16161828121410338, 13.76426979415089491, 3.090169943749476733 ) ) ;
#97039 = ORIENTED_EDGE ( 'NONE', *, *, #65851, .T. ) ;
#97040 = CARTESIAN_POINT ( 'NONE',  ( 157.3305006125302441, 282.1378183958786963, 1.589776369934247979 ) ) ;
#97041 = CARTESIAN_POINT ( 'NONE',  ( 207.7670811201955701, 270.7838546899739640, -1.661274253000708079 ) ) ;
#97042 = CARTESIAN_POINT ( 'NONE',  ( 82.27644995706197051, 41.26364417930392392, -3.466983432302654045 ) ) ;
#97043 = CARTESIAN_POINT ( 'NONE',  ( 172.8310867690399846, 268.0400968755592430, -16.30299140802141267 ) ) ;
#97044 = CARTESIAN_POINT ( 'NONE',  ( 81.22979812886450190, 55.45288652294036780, -16.34461090620094126 ) ) ;
#97045 = EDGE_LOOP ( 'NONE', ( #94562, #98784, #12873, #35216 ) ) ;
#97046 = CARTESIAN_POINT ( 'NONE',  ( 69.17486568141271164, 67.30733642665069283, 9.082494864214003982 ) ) ;
#97047 = DIRECTION ( 'NONE',  ( -0.000000000000000000, 1.000000000000000000, -0.000000000000000000 ) ) ;
#97048 = EDGE_CURVE ( 'NONE', #23100, #81391, #13094, .T. ) ;
#97049 = CARTESIAN_POINT ( 'NONE',  ( 83.07333702396124409, 41.93452038489549949, 4.251322240599892943 ) ) ;
#97050 = CARTESIAN_POINT ( 'NONE',  ( 79.60424370460739851, 51.75532430349682755, 15.26378781416301500 ) ) ;
#97051 = CYLINDRICAL_SURFACE ( 'NONE', #70406, 10.00000000000010658 ) ;
#97052 = CARTESIAN_POINT ( 'NONE',  ( 70.46850514343660166, 71.36849393383423035, 0.3238707985676339551 ) ) ;
#97053 = CARTESIAN_POINT ( 'NONE',  ( -79.28667360730979397, 56.40661347651924729, 10.00000000000000000 ) ) ;
#97054 = CARTESIAN_POINT ( 'NONE',  ( 156.0045539464697981, 278.3546514767295434, -9.412258334191998088 ) ) ;
#97055 = CARTESIAN_POINT ( 'NONE',  ( 10.70626499057286196, 14.38052372038638893, 10.00000000000000533 ) ) ;
#97056 = CARTESIAN_POINT ( 'NONE',  ( 124.2269133023872882, 230.9824982072973683, 3.021315404115420679E-15 ) ) ;
#97057 = ORIENTED_EDGE ( 'NONE', *, *, #33240, .T. ) ;
#97058 = CARTESIAN_POINT ( 'NONE',  ( 74.30221102045693726, 55.25029599878391195, 16.60364296989904176 ) ) ;
#97059 = CARTESIAN_POINT ( 'NONE',  ( 194.8432095198904221, 293.1686569321988145, -14.74101036184996616 ) ) ;
#97060 = FACE_OUTER_BOUND ( 'NONE', #6821, .T. ) ;
#97061 = VERTEX_POINT ( 'NONE', #46028 ) ;
#97062 = AXIS2_PLACEMENT_3D ( 'NONE', #26100, #40766, #16977 ) ;
#97063 = CARTESIAN_POINT ( 'NONE',  ( 78.94581588320816934, 59.75573664777502358, 16.49495449398541780 ) ) ;
#97064 = CARTESIAN_POINT ( 'NONE',  ( 184.7894305693181138, 292.1317680087225881, 12.52679022050396895 ) ) ;
#97065 = CARTESIAN_POINT ( 'NONE',  ( -22.42236680055709641, 157.8615022471902591, 0.000000000000000000 ) ) ;
#97066 = ORIENTED_EDGE ( 'NONE', *, *, #47844, .F. ) ;
#97067 = CARTESIAN_POINT ( 'NONE',  ( 91.05385083941617097, 229.5024278399160949, -9.188101187500093303 ) ) ;
#97068 = AXIS2_PLACEMENT_3D ( 'NONE', #70420, #24326, #69910 ) ;
#97069 = CARTESIAN_POINT ( 'NONE',  ( 84.06819687104101035, 49.97680779115592031, -13.47026326439832467 ) ) ;
#97070 = CARTESIAN_POINT ( 'NONE',  ( 84.54034743127247964, 49.80906814226769086, -13.21523024495328968 ) ) ;
#97071 = CARTESIAN_POINT ( 'NONE',  ( 81.25722694078321240, 42.23628214981317797, -7.275039830697891396 ) ) ;
#97072 = ORIENTED_EDGE ( 'NONE', *, *, #35055, .T. ) ;
#97073 = ORIENTED_EDGE ( 'NONE', *, *, #29040, .F. ) ;
#97074 = LINE ( 'NONE', #97553, #2830 ) ;
#97075 = ORIENTED_EDGE ( 'NONE', *, *, #9716, .F. ) ;
#97076 = CARTESIAN_POINT ( 'NONE',  ( 76.92873890057782660, 49.89429371730488327, 15.13083596839045519 ) ) ;
#97077 = ORIENTED_EDGE ( 'NONE', *, *, #6397, .F. ) ;
#97078 = CARTESIAN_POINT ( 'NONE',  ( 75.59343510720033521, 61.64003300003175667, 15.32494136272226548 ) ) ;
#97080 = CARTESIAN_POINT ( 'NONE',  ( 203.2732885619977026, 278.5673317194472247, -16.64305493556850024 ) ) ;
#97079 = VECTOR ( 'NONE', #81805, 1000.000000000000000 ) ;
#97081 = EDGE_LOOP ( 'NONE', ( #50275, #59542, #8588, #37910 ) ) ;
#97082 = CARTESIAN_POINT ( 'NONE',  ( 82.23229681800175683, 40.64091623807065901, 3.329097291065063136 ) ) ;
#97083 = CARTESIAN_POINT ( 'NONE',  ( 81.04961468568201610, 43.68546784643918812, -9.492462169003031747 ) ) ;
#97085 = EDGE_CURVE ( 'NONE', #63052, #70901, #33000, .T. ) ;
#97084 = DIRECTION ( 'NONE',  ( -0.5632146860273895550, 0.8263106059122495850, 0.000000000000000000 ) ) ;
#97086 = CARTESIAN_POINT ( 'NONE',  ( 36.67532856725514989, 51.07057046370195508, 10.00000000000000000 ) ) ;
#97087 = CARTESIAN_POINT ( 'NONE',  ( 157.4702324156611155, 281.8845292153815194, 2.929819485995689199 ) ) ;
#97088 = CARTESIAN_POINT ( 'NONE',  ( 133.7867050834633460, 257.2369531367911009, -4.594050593750048428 ) ) ;
#97089 = CARTESIAN_POINT ( 'NONE',  ( 157.1606728774482065, 258.4367249549846974, -18.41782236529479633 ) ) ;
#97090 = EDGE_LOOP ( 'NONE', ( #21865, #17387, #66754, #3857 ) ) ;
#97091 = CARTESIAN_POINT ( 'NONE',  ( 75.93938602863309484, 55.94919493231355290, 16.15023845270562930 ) ) ;
#97092 = CARTESIAN_POINT ( 'NONE',  ( 8.259543914800127951, 22.95586893147753571, 7.433330006724141015 ) ) ;
#97093 = VERTEX_POINT ( 'NONE', #16152 ) ;
#97094 = AXIS2_PLACEMENT_3D ( 'NONE', #62172, #61682, #79441 ) ;
#97095 = CARTESIAN_POINT ( 'NONE',  ( 164.1096337185929315, 281.6968895742988934, 8.720925588203845891 ) ) ;
#97097 = ORIENTED_EDGE ( 'NONE', *, *, #20597, .F. ) ;
#97096 = CARTESIAN_POINT ( 'NONE',  ( 203.7752293336776006, 271.7063540172214857, 9.638331677649306428 ) ) ;
#97098 = CARTESIAN_POINT ( 'NONE',  ( 167.0546803224166297, 282.1702852132879684, 12.27869116404093752 ) ) ;
#97099 = CARTESIAN_POINT ( 'NONE',  ( 181.3784564040530256, 255.2489373100174532, 0.6922490234118574559 ) ) ;
#97100 = VECTOR ( 'NONE', #53700, 1000.000000000000114 ) ;
#97101 = CARTESIAN_POINT ( 'NONE',  ( 76.22863942704391604, 65.23707805566866114, -14.13549428706411781 ) ) ;
#97102 = CARTESIAN_POINT ( 'NONE',  ( 156.5207620954022616, 279.5661031660920912, 7.531452285229264021 ) ) ;
#97103 = CARTESIAN_POINT ( 'NONE',  ( 165.5301935577539609, 246.9158322381169057, -2.041142469049267660 ) ) ;
#97104 = CARTESIAN_POINT ( 'NONE',  ( 194.3452430042056847, 293.4673175397701357, -14.50972866970454866 ) ) ;
#97105 = CARTESIAN_POINT ( 'NONE',  ( 84.90109790862749151, 42.41940689311433488, 1.808878322148949280 ) ) ;
#97106 = CARTESIAN_POINT ( 'NONE',  ( 88.35080703960181836, 43.95228889933407856, -2.194260235337642140 ) ) ;
#97107 = EDGE_LOOP ( 'NONE', ( #63868, #99305, #42091, #63349 ) ) ;
#97108 = CARTESIAN_POINT ( 'NONE',  ( 184.8382098728736480, 273.0595371315191073, -16.47964124523516460 ) ) ;
#97109 = CARTESIAN_POINT ( 'NONE',  ( 66.40060581361414904, 68.91289971205782194, 0.07367910596505218568 ) ) ;
#97110 = ORIENTED_EDGE ( 'NONE', *, *, #89795, .F. ) ;
#97111 = CARTESIAN_POINT ( 'NONE',  ( 160.6282313088876492, 275.7627601117830523, 12.77581587744434088 ) ) ;
#97112 = EDGE_CURVE ( 'NONE', #48299, #24507, #3410, .T. ) ;
#97113 = CARTESIAN_POINT ( 'NONE',  ( 156.2170492467576821, 277.6398520454177969, 10.26798254968793600 ) ) ;
#97114 = CARTESIAN_POINT ( 'NONE',  ( 175.3074307085254020, 254.5436327766159650, 9.407465564047683415 ) ) ;
#97115 = DIRECTION ( 'NONE',  ( -0.000000000000000000, 1.000000000000000000, -0.000000000000000000 ) ) ;
#97116 = CARTESIAN_POINT ( 'NONE',  ( 161.7595754908867605, 272.9535027612637350, 15.05830031582055817 ) ) ;
#97118 = CARTESIAN_POINT ( 'NONE',  ( 88.23123598884963315, 44.35170718015631053, 2.587891364668495342 ) ) ;
#97117 = CARTESIAN_POINT ( 'NONE',  ( 159.1812762191934212, 274.8495840587517023, 14.39428968362149241 ) ) ;
#97119 = CARTESIAN_POINT ( 'NONE',  ( 162.8839417982861448, 263.3994626277539055, 17.77684832337497767 ) ) ;
#97120 = ORIENTED_EDGE ( 'NONE', *, *, #95225, .F. ) ;
#97121 = ORIENTED_EDGE ( 'NONE', *, *, #36803, .T. ) ;
#97122 = CARTESIAN_POINT ( 'NONE',  ( 73.74770275411985665, 61.89915078644302326, -14.85475798109034606 ) ) ;
#97123 = CARTESIAN_POINT ( 'NONE',  ( 80.24843660680971880, 58.09750880718839028, 16.26407653974109024 ) ) ;
#97124 = EDGE_CURVE ( 'NONE', #74676, #91738, #85090, .T. ) ;
#97125 = FACE_OUTER_BOUND ( 'NONE', #90476, .T. ) ;
#97126 = B_SPLINE_CURVE_WITH_KNOTS ( 'NONE', 3,
 ( #61229, #45033, #75977, #17002, #44526, #22237, #21255, #63110, #99755, #53138, #45526, #98264, #78833, #15121, #22747, #76931, #28853, #52134, #83084, #13654, #75458, #6042, #18528, #11442, #3820, #49912, #40791, #80358, #57498, #27126, #50403, #9929, #48416, #42295, #41295, #19040, #10422, #88988, #81358, #95576, #87980, #88478, #79365, #71737, #11928, #73228 ),
 .UNSPECIFIED., .F., .F.,
 ( 4, 2, 2, 2, 2, 2, 2, 2, 2, 2, 2, 2, 2, 2, 2, 2, 2, 2, 2, 2, 2, 2, 4 ),
 ( 0.0002912000113238576810, 0.001310581117245713037, 0.001820271670206675789, 0.002075116946687189257, 0.002202539584927487408, 0.002329962223167785559, 0.002457384861408083276, 0.002584807499648380993, 0.002839652776129052321, 0.003349343329090460463, 0.004368724435013277181, 0.005388105540936094333, 0.005897796093897495970, 0.006152641370378155589, 0.006407486646858814340, 0.006471197965978995291, 0.006534909285099176242, 0.006598620604219358060, 0.006662331923339539011, 0.006917177199820049444, 0.007426867752781065105, 0.007936558305742080766, 0.008446248858703096427 ),
 .UNSPECIFIED. ) ;
#97127 = CARTESIAN_POINT ( 'NONE',  ( 67.16990927169524639, 66.79708245693809943, -9.067759095298582039 ) ) ;
#97128 = CARTESIAN_POINT ( 'NONE',  ( 192.8010417052266234, 296.7057953447782097, 12.10593424093686643 ) ) ;
#97129 = EDGE_CURVE ( 'NONE', #13582, #88229, #61739, .T. ) ;
#97130 = CARTESIAN_POINT ( 'NONE',  ( 80.76990913474571698, 43.05389971685210782, -9.742651082411008190 ) ) ;
#97131 = CARTESIAN_POINT ( 'NONE',  ( 157.9225728654248257, 276.1116997103654285, -12.95724163227552239 ) ) ;
#97132 = CARTESIAN_POINT ( 'NONE',  ( 9.810363290536042058, 164.2202760586659451, -5.415160957724236172E-17 ) ) ;
#97133 = CARTESIAN_POINT ( 'NONE',  ( 100.7969837277561282, 222.8768266524159856, -9.188101187500091527 ) ) ;
#97134 = DIRECTION ( 'NONE',  ( -0.2503889871761760255, -0.9681453171404016400, 0.000000000000000000 ) ) ;
#97135 = CARTESIAN_POINT ( 'NONE',  ( 183.0033326268229246, 294.1337744772658880, -7.888237667023935806 ) ) ;
#97136 = CARTESIAN_POINT ( 'NONE',  ( -17.42236680055705023, 149.2012482093457777, 0.000000000000000000 ) ) ;
#97137 = CARTESIAN_POINT ( 'NONE',  ( 194.4556067646799420, 282.9884635700969397, 17.82090350285937319 ) ) ;
#97138 = CARTESIAN_POINT ( 'NONE',  ( 0.07393976959879319799, 182.3967562850347406, 2.649461200531984646E-14 ) ) ;
#97139 = CARTESIAN_POINT ( 'NONE',  ( 148.4083960970861256, 273.5961130204771052, -8.574185186226726429 ) ) ;
#97140 = CARTESIAN_POINT ( 'NONE',  ( 84.98383346588632037, 50.06751842512129258, 13.63401461718180485 ) ) ;
#97141 = CARTESIAN_POINT ( 'NONE',  ( 86.83321340830613622, 209.3932355074535678, -2.679491924311248496 ) ) ;
#97142 = CARTESIAN_POINT ( 'NONE',  ( -27.42236680055714260, 166.5217562850347406, 1.224646799147364892E-15 ) ) ;
#97143 = CIRCLE ( 'NONE', #89150, 0.1418229129680828593 ) ;
#97144 = ADVANCED_FACE ( 'NONE', ( #92689 ), #46532, .T. ) ;
#97145 = DIRECTION ( 'NONE',  ( -0.000000000000000000, 0.000000000000000000, -1.000000000000000000 ) ) ;
#97146 = EDGE_CURVE ( 'NONE', #7311, #55128, #56648, .T. ) ;
#97147 = CARTESIAN_POINT ( 'NONE',  ( 79.47110815956433783, 210.5643266524160424, 9.188101187500095079 ) ) ;
#97148 = CARTESIAN_POINT ( 'NONE',  ( 161.1492466472929266, 251.5283125358769212, -13.33353587056634915 ) ) ;
#97149 = CARTESIAN_POINT ( 'NONE',  ( 163.4266023455967911, 257.9436588619666963, 15.59867604562648324 ) ) ;
#97151 = CARTESIAN_POINT ( 'NONE',  ( 84.75337437632948934, 42.49783821425369723, -2.788419914845409853 ) ) ;
#97150 = CARTESIAN_POINT ( 'NONE',  ( 157.3988263959001870, 258.0242309610243865, 16.72376558639979294 ) ) ;
#97152 = CARTESIAN_POINT ( 'NONE',  ( 76.11661262897267477, 65.38883171293761620, 14.43021505105784819 ) ) ;
#97153 = CARTESIAN_POINT ( 'NONE',  ( 203.9080669571095257, 275.9035274530119182, -13.79279311472316394 ) ) ;
#97154 = CARTESIAN_POINT ( 'NONE',  ( 38.69009612255265296, 24.19860640527295104, 2.839279412974134775 ) ) ;
#97155 = LINE ( 'NONE', #28707, #41853 ) ;
#97156 = CARTESIAN_POINT ( 'NONE',  ( 79.15288444911743682, 228.0530062829863027, -4.648177544792955347E-16 ) ) ;
#97157 = ORIENTED_EDGE ( 'NONE', *, *, #45604, .T. ) ;
#97158 = CARTESIAN_POINT ( 'NONE',  ( 21.85012855468117721, 24.56628583063841376, 9.188101187500006262 ) ) ;
#97159 = CARTESIAN_POINT ( 'NONE',  ( 49.07419501245632176, 91.40403951869188859, 10.00000000000000000 ) ) ;
#97160 = CARTESIAN_POINT ( 'NONE',  ( -32.93344297370182971, 94.68900127417109047, 10.52354740462235760 ) ) ;
#97161 = CARTESIAN_POINT ( 'NONE',  ( 191.2622316156482043, 288.8574828335728171, -16.55244734589887656 ) ) ;
#97162 = CARTESIAN_POINT ( 'NONE',  ( 70.62351716309591154, 60.91279443485260714, 15.01748476286653933 ) ) ;
#97163 = CARTESIAN_POINT ( 'NONE',  ( 153.6845034812979804, 266.9389077895647802, 16.46468584801201374 ) ) ;
#97164 = DIRECTION ( 'NONE',  ( -0.000000000000000000, 0.000000000000000000, -1.000000000000000000 ) ) ;
#97165 = CARTESIAN_POINT ( 'NONE',  ( 140.3182403272686543, 258.4865022471902876, 10.00000000000009237 ) ) ;
#97166 = CARTESIAN_POINT ( 'NONE',  ( 205.3708847852691406, 274.9341884869767227, -13.70973585089674174 ) ) ;
#97167 = B_SPLINE_CURVE_WITH_KNOTS ( 'NONE', 3,
 ( #87582, #33297, #41892, #79447 ),
 .UNSPECIFIED., .F., .F.,
 ( 4, 4 ),
 ( 0.01508109614910603871, 0.02383471597684285251 ),
 .UNSPECIFIED. ) ;
#97168 = CARTESIAN_POINT ( 'NONE',  ( 74.84467759388789432, 53.32343055176874458, 16.53062654614232230 ) ) ;
#97169 = VERTEX_POINT ( 'NONE', #42430 ) ;
#97170 = CARTESIAN_POINT ( 'NONE',  ( 85.58519120388885426, 46.64559940333228383, 10.07285853436253120 ) ) ;
#97171 = ORIENTED_EDGE ( 'NONE', *, *, #50036, .F. ) ;
#97172 = CARTESIAN_POINT ( 'NONE',  ( 66.15274061880275269, 50.14441083166266822, 0.000000000000000000 ) ) ;
#97173 = CARTESIAN_POINT ( 'NONE',  ( 86.46877025260693017, 44.29843151041793448, 5.647966490367202219 ) ) ;
#97174 = ORIENTED_EDGE ( 'NONE', *, *, #7512, .T. ) ;
#97175 = CARTESIAN_POINT ( 'NONE',  ( -19.65312891409030271, 93.06504152958497400, 10.00000000000000888 ) ) ;
#97176 = ORIENTED_EDGE ( 'NONE', *, *, #27729, .F. ) ;
#97177 = CARTESIAN_POINT ( 'NONE',  ( 72.27003297432077034, 71.75159315020286499, 5.546042747704600373 ) ) ;
#97178 = CARTESIAN_POINT ( 'NONE',  ( 205.9050707304272407, 274.0089512892737389, 12.32231322111777772 ) ) ;
#97179 = CARTESIAN_POINT ( 'NONE',  ( 158.2778382039339533, 257.5751017963053187, -16.89175558457479198 ) ) ;
#97180 = CARTESIAN_POINT ( 'NONE',  ( 204.0490764393590553, 272.8272845076828617, 11.09290516031127005 ) ) ;
#97181 = CARTESIAN_POINT ( 'NONE',  ( 201.1388841337167435, 282.2642286331299601, -18.17233400608081340 ) ) ;
#97182 = EDGE_CURVE ( 'NONE', #40677, #49707, #33878, .T. ) ;
#97183 = CARTESIAN_POINT ( 'NONE',  ( 27.40352323984253857, 36.79752408145593279, -5.678558825948271327 ) ) ;
#97184 = DIRECTION ( 'NONE',  ( -0.8660254037844387076, -0.4999999999999998890, -0.000000000000000000 ) ) ;
#97185 = CARTESIAN_POINT ( 'NONE',  ( 165.0963061027407832, 274.7047549202629284, 14.74588534425331332 ) ) ;
#97186 = CARTESIAN_POINT ( 'NONE',  ( 167.5469267500292574, 266.7168544022062520, -17.80679023418265672 ) ) ;
#97187 = VERTEX_POINT ( 'NONE', #81008 ) ;
#97188 = ORIENTED_EDGE ( 'NONE', *, *, #37215, .F. ) ;
#97189 = DIRECTION ( 'NONE',  ( -0.5778974349098243701, -0.4186690413702435221, 0.7005360722495073134 ) ) ;
#97191 = CARTESIAN_POINT ( 'NONE',  ( 147.7467138384290308, 274.7421803109381813, -9.190172068879620682 ) ) ;
#97190 = CARTESIAN_POINT ( 'NONE',  ( 68.34875839458671010, 65.66236861316339457, 10.38748295948464140 ) ) ;
#97192 = CARTESIAN_POINT ( 'NONE',  ( 85.74188846148156529, 48.75224078981592157, -11.97363005349371079 ) ) ;
#97193 = CARTESIAN_POINT ( 'NONE',  ( 164.7364331287320738, 247.3151232938002693, -7.618980141130590411 ) ) ;
#97194 = CARTESIAN_POINT ( 'NONE',  ( 147.4749560789897771, 275.5966042365595854, 0.1362648926203907929 ) ) ;
#97195 = CARTESIAN_POINT ( 'NONE',  ( 93.96857342517718337, -8.000000000000000000, -9.212605237762131694 ) ) ;
#97196 = CARTESIAN_POINT ( 'NONE',  ( 170.8905786597765086, 288.0411465072718329, -4.155906328687864359 ) ) ;
#97197 = CARTESIAN_POINT ( 'NONE',  ( 169.7144176936253359, 267.3710074754821449, 17.44705272466886115 ) ) ;
#97198 = CARTESIAN_POINT ( 'NONE',  ( 181.6012535417948186, 256.1925639173799709, 5.230076733189143567 ) ) ;
#97199 = CARTESIAN_POINT ( 'NONE',  ( 93.70588009062352342, 237.1589784336661637, -6.496448406907675876E-16 ) ) ;
#97201 = ORIENTED_EDGE ( 'NONE', *, *, #88805, .T. ) ;
#97200 = B_SPLINE_CURVE_WITH_KNOTS ( 'NONE', 3,
 ( #40714, #41717, #72662, #34140, #41210, #25535, #1233, #55402, #55898, #85898, #16423, #9332, #56423, #9854, #71657, #33128, #17947, #71150 ),
 .UNSPECIFIED., .F., .F.,
 ( 4, 2, 2, 2, 2, 2, 2, 2, 4 ),
 ( 2.819365433277861356E-15, 0.0003786859679666404054, 0.0007573719359304614514, 0.001136057903894282552, 0.001514743871858103543, 0.001893429839821924535, 0.002272115807785745744, 0.002650801775749566519, 0.003029487743713387728 ),
 .UNSPECIFIED. ) ;
#97202 = FACE_OUTER_BOUND ( 'NONE', #6826, .T. ) ;
#97203 = CARTESIAN_POINT ( 'NONE',  ( -14.65312891409034535, 84.40478749174073414, 0.000000000000000000 ) ) ;
#97204 = CARTESIAN_POINT ( 'NONE',  ( 112.0100349375168918, 242.1427522451419065, -10.00000000000009592 ) ) ;
#97205 = ORIENTED_EDGE ( 'NONE', *, *, #73528, .F. ) ;
#97206 = ORIENTED_EDGE ( 'NONE', *, *, #98229, .F. ) ;
#97207 = DIRECTION ( 'NONE',  ( 0.4999999999999998890, -0.8660254037844385966, 0.000000000000000000 ) ) ;
#97208 = CARTESIAN_POINT ( 'NONE',  ( 49.63464994930628649, 103.0251469596019120, 10.00000000000000000 ) ) ;
#97209 = CARTESIAN_POINT ( 'NONE',  ( 164.5512980253735122, 249.3551712322193055, 9.899787939062008491 ) ) ;
#97210 = CARTESIAN_POINT ( 'NONE',  ( 159.4491226731523454, 254.4730136382542582, -15.39140229921534520 ) ) ;
#97211 = CARTESIAN_POINT ( 'NONE',  ( 189.3399741911424314, 300.7005401275983445, 2.182451016153226694E-15 ) ) ;
#97212 = ORIENTED_EDGE ( 'NONE', *, *, #40586, .T. ) ;
#97213 = AXIS2_PLACEMENT_3D ( 'NONE', #9350, #45824, #1766 ) ;
#97214 = VERTEX_POINT ( 'NONE', #41950 ) ;
#97215 = CARTESIAN_POINT ( 'NONE',  ( 162.6262389125959373, 248.9700868899859074, -10.50380342094597808 ) ) ;
#97216 = ORIENTED_EDGE ( 'NONE', *, *, #55034, .T. ) ;
#97217 = CARTESIAN_POINT ( 'NONE',  ( 148.7305541605275607, 275.0381188865328568, -8.045727261058747359 ) ) ;
#97218 = CARTESIAN_POINT ( 'NONE',  ( 15.61058218230948036, 186.4865022471903160, 10.00000000000009415 ) ) ;
#97219 = CARTESIAN_POINT ( 'NONE',  ( 82.23427998234210179, 44.55295170538099114, 9.756742293097531160 ) ) ;
#97221 = CARTESIAN_POINT ( 'NONE',  ( 199.3488497299964024, 284.5376415457495796, 17.19460419984376287 ) ) ;
#97220 = CARTESIAN_POINT ( 'NONE',  ( 124.5040820605901217, 248.8149278399161233, -9.188101187500095079 ) ) ;
#97222 = CARTESIAN_POINT ( 'NONE',  ( 182.5686778644665083, 296.6873302901632314, 1.787712280751329708 ) ) ;
#97223 = EDGE_LOOP ( 'NONE', ( #25575, #87117, #25797, #38845 ) ) ;
#97224 = CARTESIAN_POINT ( 'NONE',  ( 204.5482460332032986, 276.3590406018296903, 14.63243279326650814 ) ) ;
#97225 = CARTESIAN_POINT ( 'NONE',  ( 63.21847669855743135, 195.7592609112380160, 2.679491924311254714 ) ) ;
#97226 = CARTESIAN_POINT ( 'NONE',  ( 82.52124186608902789, 40.48930152589419862, -1.425869482907266450 ) ) ;
#97227 = CARTESIAN_POINT ( 'NONE',  ( 192.3159699081281815, 271.9052417175213918, 14.14648652338713397 ) ) ;
#97228 = CARTESIAN_POINT ( 'NONE',  ( 178.5440531547785952, 285.2457182098279986, 13.27232952186126802 ) ) ;
#97229 = EDGE_CURVE ( 'NONE', #47888, #20349, #72308, .T. ) ;
#97230 = DIRECTION ( 'NONE',  ( 0.2033683215378999376, -0.3522442655536480172, -0.9135454576426004225 ) ) ;
#97231 = CYLINDRICAL_SURFACE ( 'NONE', #8144, 10.00000000000010658 ) ;
#97232 = EDGE_CURVE ( 'NONE', #77581, #26850, #84337, .T. ) ;
#97233 = CARTESIAN_POINT ( 'NONE',  ( 80.51961122738369170, 52.55551232112726012, 15.38693572438338464 ) ) ;
#97234 = CARTESIAN_POINT ( 'NONE',  ( -51.91772629337628331, 101.0347834704168122, -10.00000000000000000 ) ) ;
#97235 = EDGE_CURVE ( 'NONE', #51575, #3137, #2136, .T. ) ;
#97236 = CARTESIAN_POINT ( 'NONE',  ( 167.7939926630123182, 249.6251980485383513, 7.973689277210887383 ) ) ;
#97237 = DIRECTION ( 'NONE',  ( -0.000000000000000000, -0.000000000000000000, 1.000000000000000000 ) ) ;
#97238 = CARTESIAN_POINT ( 'NONE',  ( 207.6523394534040392, 270.9825930866021508, -2.115019688068903392 ) ) ;
#97239 = EDGE_CURVE ( 'NONE', #79062, #57005, #80500, .T. ) ;
#97240 = CARTESIAN_POINT ( 'NONE',  ( 31.78235740255998820, 30.30066082961423746, -10.00000000000000533 ) ) ;
#97241 = CARTESIAN_POINT ( 'NONE',  ( 80.06694460085255116, 44.56748078928367818, -11.69919935169422764 ) ) ;
#97242 = CARTESIAN_POINT ( 'NONE',  ( -20.80355385027020176, 95.10302759471045420, 45.19948259297560611 ) ) ;
#97243 = CARTESIAN_POINT ( 'NONE',  ( 7.614983434379491101, 23.13478043621386249, 8.090169943749478065 ) ) ;
#97244 = CARTESIAN_POINT ( 'NONE',  ( 36.68702710410599366, 29.38052372038643867, 10.00000000000000533 ) ) ;
#97245 = FACE_OUTER_BOUND ( 'NONE', #13182, .T. ) ;
#97246 = DIRECTION ( 'NONE',  ( 0.6647600172776847449, -0.7470569720101488675, 0.000000000000000000 ) ) ;
#97247 = CARTESIAN_POINT ( 'NONE',  ( 157.7483529369466737, 270.6632484235471452, -15.17384122213293729 ) ) ;
#97248 = CARTESIAN_POINT ( 'NONE',  ( 84.59746252465258465, 43.34080150004616883, -5.792757565574923717 ) ) ;
#97249 = CARTESIAN_POINT ( 'NONE',  ( 207.2707369601997982, 271.6435479931266173, -5.381413637561199614 ) ) ;
#97250 =( BOUNDED_CURVE ( )  B_SPLINE_CURVE ( 2, ( #27865, #28870, #59746, #75474, #52149, #12689, #37440, #90208, #45050 ),
 .UNSPECIFIED., .F., .F. ) 
 B_SPLINE_CURVE_WITH_KNOTS ( ( 3, 2, 2, 2, 3 ),
 ( 0.4314516129032258118, 0.4327956989247311870, 0.4354838709677419373, 0.4381720430107526876, 0.4395161290322580627 ),
 .UNSPECIFIED. ) 
 CURVE ( )  GEOMETRIC_REPRESENTATION_ITEM ( )  RATIONAL_B_SPLINE_CURVE ( ( 0.9330127018922194093, 0.9330127018922194093, 1.000000000000000000, 0.8660254037844387076, 1.000000000000000000, 0.8660254037844387076, 1.000000000000000000, 0.9330127018922194093, 0.9330127018922194093 ) ) 
 REPRESENTATION_ITEM ( '' )  );
#97251 = CARTESIAN_POINT ( 'NONE',  ( 16.06189740016370848, 170.8923013555409796, 4.594050593750050204 ) ) ;
#97252 = CARTESIAN_POINT ( 'NONE',  ( 207.3589495855971450, 271.0586446502292119, 2.456771036675355457 ) ) ;
#97253 = ORIENTED_EDGE ( 'NONE', *, *, #75168, .F. ) ;
#97254 = CARTESIAN_POINT ( 'NONE',  ( 87.36774593059779193, 45.94567951850589083, 8.539250186115692642 ) ) ;
#97255 = CARTESIAN_POINT ( 'NONE',  ( 23.89366908878298190, 14.76426979415089846, 3.090169943749476733 ) ) ;
#97256 = CARTESIAN_POINT ( 'NONE',  ( 42.50247518763358556, 195.3458772461660544, 9.188101187500095079 ) ) ;
#97257 = CARTESIAN_POINT ( 'NONE',  ( 86.84204249716189850, 45.92435628226732547, 8.934002094794735171 ) ) ;
#97258 = CARTESIAN_POINT ( 'NONE',  ( 199.1216527653377000, 285.7581758537840528, -18.37739894744384728 ) ) ;
#97259 = CARTESIAN_POINT ( 'NONE',  ( 147.0538900202505488, 275.9421863647172017, 5.192507380313251986 ) ) ;
#97260 = CARTESIAN_POINT ( 'NONE',  ( 39.59743582264582784, 38.56454794089045635, 10.00000000000000355 ) ) ;
#97261 = CARTESIAN_POINT ( 'NONE',  ( 173.3264126386846726, 289.1951097772950448, -8.140207440225699642 ) ) ;
#97262 = CARTESIAN_POINT ( 'NONE',  ( 178.5991144655399410, 293.9124374319637809, 2.724545304837039605 ) ) ;
#97263 = CARTESIAN_POINT ( 'NONE',  ( 198.2489255580726422, 287.2697837179150042, 18.53597557040773225 ) ) ;
#97264 = CARTESIAN_POINT ( 'NONE',  ( 180.1848004237850205, 278.8644883139655235, -16.25315175759617148 ) ) ;
#97265 = CARTESIAN_POINT ( 'NONE',  ( 67.85574724824152781, 67.82218689132628242, -7.169315664176491687 ) ) ;
#97266 = CARTESIAN_POINT ( 'NONE',  ( 166.9153220475343460, 257.9520600803688239, -15.27885173810403785 ) ) ;
#97267 = DIRECTION ( 'NONE',  ( -0.3851501363289908109, 0.9228539280329036698, 0.000000000000000000 ) ) ;
#97268 = CARTESIAN_POINT ( 'NONE',  ( 99.25420243115659957, 218.1115022471901739, -5.000000000000041744 ) ) ;
#97269 = CARTESIAN_POINT ( 'NONE',  ( 10.41442975960284834, 183.4865022471903160, 10.00000000000009415 ) ) ;
#97270 = CARTESIAN_POINT ( 'NONE',  ( 161.6733100514768466, 267.8128507344575837, -17.34687799797600860 ) ) ;
#97271 = ORIENTED_EDGE ( 'NONE', *, *, #31318, .T. ) ;
#97272 = CARTESIAN_POINT ( 'NONE',  ( 63.28708487846012076, 207.3458772461660544, 9.188101187500095079 ) ) ;
#97273 = EDGE_LOOP ( 'NONE', ( #63389, #82021, #69707, #79366 ) ) ;
#97274 = CARTESIAN_POINT ( 'NONE',  ( -11.84316977508124857, 85.52578825423026387, 14.70342373635102895 ) ) ;
#97275 = CARTESIAN_POINT ( 'NONE',  ( 161.7836053227420905, 250.9551966261522296, 12.65126904800779606 ) ) ;
#97276 = CARTESIAN_POINT ( 'NONE',  ( 67.29236409614540548, 66.61846781487172109, -8.519670054875607690 ) ) ;
#97277 = ORIENTED_EDGE ( 'NONE', *, *, #14742, .T. ) ;
#97278 = CARTESIAN_POINT ( 'NONE',  ( 170.8453059873319830, 287.4268083147989614, 8.562683323710214012 ) ) ;
#97279 = CARTESIAN_POINT ( 'NONE',  ( 207.0200405408487541, 272.0777669287182334, 6.494273599193515878 ) ) ;
#97280 = DIRECTION ( 'NONE',  ( 0.000000000000000000, 0.000000000000000000, -1.000000000000000000 ) ) ;
#97281 = CARTESIAN_POINT ( 'NONE',  ( 29.13557404741141355, 37.79752408145594700, -5.678558825948271327 ) ) ;
#97282 = CARTESIAN_POINT ( 'NONE',  ( 189.0171803163284494, 265.5415642084109891, 10.72429650996405215 ) ) ;
#97283 = CARTESIAN_POINT ( 'NONE',  ( 86.38615641404119572, 47.55643641724976334, -10.55640884279900327 ) ) ;
#97284 = EDGE_CURVE ( 'NONE', #4619, #79225, #83263, .T. ) ;
#97285 = PLANE ( 'NONE',  #77521 ) ;
#97286 = VERTEX_POINT ( 'NONE', #98168 ) ;
#97287 = CARTESIAN_POINT ( 'NONE',  ( 14.74991654177707900, 23.91421378149918198, 9.188101187500008038 ) ) ;
#97288 = FACE_OUTER_BOUND ( 'NONE', #29833, .T. ) ;
#97289 = CARTESIAN_POINT ( 'NONE',  ( 16.11576366785039127, 190.1115022471903160, -5.000000000000047962 ) ) ;
#97290 = CARTESIAN_POINT ( 'NONE',  ( 5.386117596089862403, 185.4637435831425023, 2.679491924311251605 ) ) ;
#97291 = ORIENTED_EDGE ( 'NONE', *, *, #2200, .F. ) ;
#97292 = CARTESIAN_POINT ( 'NONE',  ( 76.98982937314906394, 56.23836901630515683, 16.60980887848485921 ) ) ;
#97293 = CARTESIAN_POINT ( 'NONE',  ( 150.6571681785161445, 269.7011255207979730, 15.24894850018880454 ) ) ;
#97294 = CYLINDRICAL_SURFACE ( 'NONE', #51231, 17.82106496071139645 ) ;
#97295 = ORIENTED_EDGE ( 'NONE', *, *, #85458, .F. ) ;
#97296 = VERTEX_POINT ( 'NONE', #42917 ) ;
#97298 = DIRECTION ( 'NONE',  ( -0.2633726137851614135, -0.9634420117996742583, -0.04913609882121805494 ) ) ;
#97297 = CARTESIAN_POINT ( 'NONE',  ( 207.2683629543511756, 271.6476598918739001, -6.694388351944108528 ) ) ;
#97299 = ORIENTED_EDGE ( 'NONE', *, *, #11480, .F. ) ;
#97300 = CARTESIAN_POINT ( 'NONE',  ( 66.28447348300909425, 69.23781496131373103, -2.133696438910710480 ) ) ;
#97301 = CARTESIAN_POINT ( 'NONE',  ( 197.9002057575219453, 287.8737841300738296, 18.01270164875645818 ) ) ;
#97302 = LINE ( 'NONE', #66861, #61283 ) ;
#97303 = CARTESIAN_POINT ( 'NONE',  ( 78.18465668123985779, 61.71620641638569538, -16.11691968629958183 ) ) ;
#97304 = ADVANCED_FACE ( 'NONE', ( #81990 ), #43437, .F. ) ;
#97305 = CARTESIAN_POINT ( 'NONE',  ( 116.8724067376222706, 238.2833772461660544, -9.188101187500095079 ) ) ;
#97306 = CARTESIAN_POINT ( 'NONE',  ( 190.9907605556751093, 299.8412942717858414, 8.799173206188184437 ) ) ;
#97307 = CARTESIAN_POINT ( 'NONE',  ( 31.54184116921283376, 189.0177522451418497, -10.00000000000009592 ) ) ;
#97308 = ORIENTED_EDGE ( 'NONE', *, *, #54175, .F. ) ;
#97309 = CARTESIAN_POINT ( 'NONE',  ( 208.2764314485352770, 269.9016340424377063, 2.433736665191914117 ) ) ;
#97310 = ORIENTED_EDGE ( 'NONE', *, *, #3400, .T. ) ;
#97311 = ORIENTED_EDGE ( 'NONE', *, *, #73436, .F. ) ;
#97312 = FACE_BOUND ( 'NONE', #95705, .T. ) ;
#97313 = CARTESIAN_POINT ( 'NONE',  ( 162.7006039569504594, 261.3497057169571463, 17.57720365097131676 ) ) ;
#97314 = CARTESIAN_POINT ( 'NONE',  ( 75.14098114064213974, 208.0643266524159856, -9.188101187500093303 ) ) ;
#97315 = DIRECTION ( 'NONE',  ( -0.3693965786901617365, 0.9292718480896766664, 0.000000000000000000 ) ) ;
#97316 = CARTESIAN_POINT ( 'NONE',  ( 81.59396048808834223, 55.93895065387218324, 16.03242832552846053 ) ) ;
#97317 = CARTESIAN_POINT ( 'NONE',  ( 198.6701036545953230, 286.5402818557027445, 17.25253558010639310 ) ) ;
#97318 = CARTESIAN_POINT ( 'NONE',  ( 175.8184439186038048, 278.1148561126908021, 16.51363926675430349 ) ) ;
#97319 = EDGE_LOOP ( 'NONE', ( #9045, #26902, #48305, #45216 ) ) ;
#97320 = CARTESIAN_POINT ( 'NONE',  ( 113.3812418268422562, 246.2677522451419065, -5.000000000000047962 ) ) ;
#97321 = CARTESIAN_POINT ( 'NONE',  ( -86.81108781737714253, -8.000000000000000000, -9.212605237762131694 ) ) ;
#97322 = ORIENTED_EDGE ( 'NONE', *, *, #57818, .T. ) ;
#97323 = CYLINDRICAL_SURFACE ( 'NONE', #8133, 70.00000000000002842 ) ;
#97324 = LINE ( 'NONE', #66397, #49949 ) ;
#97325 = CARTESIAN_POINT ( 'NONE',  ( 206.4719461165055066, 270.6153493572695083, 2.407488219507921912 ) ) ;
#97326 = CARTESIAN_POINT ( 'NONE',  ( 200.3687477146384310, 283.1577567649229650, -16.79529056473667126 ) ) ;
#97327 = LINE ( 'NONE', #67391, #96429 ) ;
#97329 = CARTESIAN_POINT ( 'NONE',  ( 206.2456893945931142, 273.4189824569319285, 10.13882547285618152 ) ) ;
#97328 = CARTESIAN_POINT ( 'NONE',  ( 196.3174919959537306, 290.6151247789487684, -17.61248417473235151 ) ) ;
#97330 = LINE ( 'NONE', #4608, #10505 ) ;
#97331 = CARTESIAN_POINT ( 'NONE',  ( 164.3053959849042087, 246.0617015268593661, -7.251939739328854273 ) ) ;
#97332 = CARTESIAN_POINT ( 'NONE',  ( 117.4133255192225391, 250.8464784336661353, 1.353441290958777327E-15 ) ) ;
#97333 = VERTEX_POINT ( 'NONE', #74381 ) ;
#97334 = CARTESIAN_POINT ( 'NONE',  ( 191.0481192767711036, 299.7419460525905492, -9.103377665618040737 ) ) ;
#97335 = CARTESIAN_POINT ( 'NONE',  ( 184.4251457649926067, 259.7825290899927495, 6.334789828098508657 ) ) ;
#97336 = ADVANCED_FACE ( 'NONE', ( #28746 ), #83480, .T. ) ;
#97337 = CARTESIAN_POINT ( 'NONE',  ( 199.5442653985851962, 283.0261893010793415, -17.63221794778640117 ) ) ;
#97338 = CARTESIAN_POINT ( 'NONE',  ( 204.2799274532736433, 276.8237820148827950, 13.55359442435934803 ) ) ;
#97339 = CARTESIAN_POINT ( 'NONE',  ( 74.60895917517520104, 60.22888921480863189, 15.54340603921727748 ) ) ;
#97340 = VECTOR ( 'NONE', #26612, 1000.000000000000114 ) ;
#97341 = DIRECTION ( 'NONE',  ( -0.8660254037844387076, -0.4999999999999998890, -0.000000000000000000 ) ) ;
#97342 = ORIENTED_EDGE ( 'NONE', *, *, #34570, .T. ) ;
#97343 = CARTESIAN_POINT ( 'NONE',  ( 76.76894470656165481, 55.99379639269752573, 16.17573251806829404 ) ) ;
#97344 = DIRECTION ( 'NONE',  ( 0.000000000000000000, 0.000000000000000000, 1.000000000000000000 ) ) ;
#97345 = B_SPLINE_CURVE_WITH_KNOTS ( 'NONE', 3,
 ( #91244, #60286, #60779, #58796, #98836, #76040, #97839, #67409, #27914, #74546, #90266, #90771, #21321, #13239, #52199, #28408, #67916, #5125, #59288, #20839, #89765, #83148, #29417, #21809, #91743, #52694, #83656, #22307, #53208, #84161, #74037, #4626, #35518, #20334, #51205, #85666, #86169, #7603, #69895, #9108, #54179, #16205, #99821, #507, #38990, #47097, #45592, #7102, #1524, #22809, #19, #16703 ),
 .UNSPECIFIED., .F., .F.,
 ( 4, 2, 2, 2, 2, 2, 2, 2, 2, 2, 2, 2, 2, 2, 2, 2, 2, 2, 2, 2, 2, 2, 2, 2, 2, 4 ),
 ( 0.0007713298675087345126, 0.0009758712993485446586, 0.001078142015268449732, 0.001180412731188354696, 0.001282683447108259878, 0.001384954163028164842, 0.001589495594868055653, 0.001998578458547837274, 0.002407661322227618896, 0.003225827049587262369, 0.004043992776946906710, 0.004862158504306550617, 0.005271241367986409000, 0.005475782799826377223, 0.005578053515746398197, 0.005629188873706406950, 0.005680324231666414835, 0.005731459589626423587, 0.005782594947586431472, 0.005884865663506446375, 0.006089407095346483986, 0.006293948527186521598, 0.006498489959026559210, 0.006703031390866596821, 0.006907572822706634433, 0.007316655686386753024 ),
 .UNSPECIFIED. ) ;
#97346 = LINE ( 'NONE', #90264, #72179 ) ;
#97347 = CARTESIAN_POINT ( 'NONE',  ( 164.3448606421738702, 245.9933467353647814, -1.273739175181084260 ) ) ;
#97348 = EDGE_CURVE ( 'NONE', #26159, #27875, #1047, .T. ) ;
#97349 = CARTESIAN_POINT ( 'NONE',  ( 73.38874485642215006, 69.17140463384058080, -9.961793831881072592 ) ) ;
#97350 = EDGE_CURVE ( 'NONE', #61085, #68592, #14047, .T. ) ;
#97351 = CARTESIAN_POINT ( 'NONE',  ( 146.8358616138309571, 276.3198226421291679, 4.054088818585255716 ) ) ;
#97352 = CARTESIAN_POINT ( 'NONE',  ( 70.15174361226061706, 71.00165729854369090, 2.050894468748571509 ) ) ;
#97353 = CARTESIAN_POINT ( 'NONE',  ( 157.1458804504438831, 258.4623461901232417, -17.08829597948888335 ) ) ;
#97354 = CARTESIAN_POINT ( 'NONE',  ( 171.0793476467304970, 250.7099474803164298, 3.411557086744808398 ) ) ;
#97355 = CARTESIAN_POINT ( 'NONE',  ( 25.07769263752670597, 14.28848085856231798, 1.475505719884397138E-15 ) ) ;
#97356 = CARTESIAN_POINT ( 'NONE',  ( 190.0274641710971082, 301.5097725526222803, 3.738976720635653450 ) ) ;
#97357 = DIRECTION ( 'NONE',  ( 0.4999999999999992784, -0.8660254037844390407, 0.000000000000000000 ) ) ;
#97358 = CARTESIAN_POINT ( 'NONE',  ( 93.96857342517718337, 0.000000000000000000, 9.212605237762133470 ) ) ;
#97359 = CARTESIAN_POINT ( 'NONE',  ( 197.8822014719394531, 287.9049684674569676, 17.88172308374019792 ) ) ;
#97360 = CARTESIAN_POINT ( 'NONE',  ( 157.5034794998415180, 271.0532920065124358, -14.68140584649887614 ) ) ;
#97361 = CARTESIAN_POINT ( 'NONE',  ( 134.1658515176688411, 238.2677522451417929, -5.000000000000041744 ) ) ;
#97362 = CARTESIAN_POINT ( 'NONE',  ( 175.7752474544214465, 285.2040480104212179, -12.03434417915003607 ) ) ;
#97363 = ORIENTED_EDGE ( 'NONE', *, *, #35562, .T. ) ;
#97364 = CARTESIAN_POINT ( 'NONE',  ( 157.3363371328520088, 258.1324655395517311, 18.24585617226787093 ) ) ;
#97365 = CARTESIAN_POINT ( 'NONE',  ( 198.9369963555428740, 286.0780101374919013, -18.58432392708837710 ) ) ;
#97367 = CARTESIAN_POINT ( 'NONE',  ( -3.478321416370212305, 177.9869531367911293, 4.594050593750046652 ) ) ;
#97366 = B_SPLINE_CURVE_WITH_KNOTS ( 'NONE', 3,
 ( #88703, #50139, #41529, #81092 ),
 .UNSPECIFIED., .F., .F.,
 ( 4, 4 ),
 ( 0.01180967855186642636, 0.01789565966245129647 ),
 .UNSPECIFIED. ) ;
#97368 = B_SPLINE_CURVE_WITH_KNOTS ( 'NONE', 3,
 ( #6444, #100151, #17400, #83474 ),
 .UNSPECIFIED., .F., .F.,
 ( 4, 4 ),
 ( 0.005778719348092632713, 0.01383577470342770011 ),
 .UNSPECIFIED. ) ;
#97369 = CARTESIAN_POINT ( 'NONE',  ( 61.01376819352597636, 206.0333772461660544, 9.188101187500095079 ) ) ;
#97370 = CARTESIAN_POINT ( 'NONE',  ( 83.86224871339140918, 42.07689945840732548, 4.987215453410938970 ) ) ;
#97371 = CARTESIAN_POINT ( 'NONE',  ( 28.83231091828818649, 21.81029122506295792, 8.090169943749479842 ) ) ;
#97372 = CARTESIAN_POINT ( 'NONE',  ( 85.30407614177579489, 48.45294084599412088, 12.40582119231524949 ) ) ;
#97373 = CARTESIAN_POINT ( 'NONE',  ( 157.8811243250769110, 257.1888664433053009, -17.39256699147873064 ) ) ;
#97374 = CARTESIAN_POINT ( 'NONE',  ( 189.4518811391805855, 290.6466329671102926, -14.51581993625191025 ) ) ;
#97375 = CARTESIAN_POINT ( 'NONE',  ( 73.83769579401584338, 55.54879188763737830, -16.58599655330451128 ) ) ;
#97376 = CARTESIAN_POINT ( 'NONE',  ( 168.2274955120613811, 256.9427370946946780, 13.69819450224870572 ) ) ;
#97377 = CARTESIAN_POINT ( 'NONE',  ( 179.3779096336606642, 254.7328586665793466, -4.090843683719358026 ) ) ;
#97378 = CARTESIAN_POINT ( 'NONE',  ( 150.5355989389948093, 269.9116896202863245, 15.28294032643914768 ) ) ;
#97379 = CARTESIAN_POINT ( 'NONE',  ( 36.90037335867692292, 202.1115022471903160, -5.000000000000047962 ) ) ;
#97380 = CARTESIAN_POINT ( 'NONE',  ( 181.1156277128715431, 292.7914473640799997, 9.490545386343454126 ) ) ;
#97381 = CARTESIAN_POINT ( 'NONE',  ( 147.6300909839706321, 274.9441770201837585, 8.328755691084779755 ) ) ;
#97382 = CARTESIAN_POINT ( 'NONE',  ( 10.97399815293012892, 167.9548013555409796, -4.594050593750042211 ) ) ;
#97383 = CARTESIAN_POINT ( 'NONE',  ( 72.76446422349046372, 71.15534465558161514, -7.354170587574377471 ) ) ;
#97384 = CARTESIAN_POINT ( 'NONE',  ( 79.11589578886889740, 60.05912704548522640, 16.12809997863940836 ) ) ;
#97385 = CARTESIAN_POINT ( 'NONE',  ( 27.72828276626169952, 36.98502408145593989, -5.678558825948271327 ) ) ;
#97386 = DIRECTION ( 'NONE',  ( -0.03004293549037833494, -0.9995486091367047354, 0.000000000000000000 ) ) ;
#97387 = CARTESIAN_POINT ( 'NONE',  ( 206.9676408587583296, 272.1685258403992975, 7.544050792475608169 ) ) ;
#97388 = CARTESIAN_POINT ( 'NONE',  ( 193.9204722154232741, 294.7668848255750049, 15.43855698596013859 ) ) ;
#97389 = DIRECTION ( 'NONE',  ( 1.000000000000000000, 0.000000000000000000, 0.000000000000000000 ) ) ;
#97390 = CARTESIAN_POINT ( 'NONE',  ( 176.7575342647435832, 260.2821926596799926, -13.68860621714789083 ) ) ;
#97391 = CARTESIAN_POINT ( 'NONE',  ( 9.708348802340269756, 27.64646525600388571, -2.839279412974133887 ) ) ;
#97392 = LINE ( 'NONE', #27960, #43438 ) ;
#97393 = CARTESIAN_POINT ( 'NONE',  ( 82.92115063973837152, 53.64018987990929332, 15.71948723892795741 ) ) ;
#97394 = LINE ( 'NONE', #66957, #65170 ) ;
#97395 = EDGE_CURVE ( 'NONE', #20462, #56406, #81642, .T. ) ;
#97396 = DIRECTION ( 'NONE',  ( -0.8660254037844378194, -0.5000000000000014433, -0.000000000000000000 ) ) ;
#97397 = ORIENTED_EDGE ( 'NONE', *, *, #25039, .F. ) ;
#97398 = CARTESIAN_POINT ( 'NONE',  ( 154.4564265542881287, 275.3778590288120540, 10.40416966185339653 ) ) ;
#97399 = CARTESIAN_POINT ( 'NONE',  ( 81.10384738341275579, 42.53340397202252632, 7.902204148537900430 ) ) ;
#97400 = EDGE_CURVE ( 'NONE', #64662, #84833, #28239, .T. ) ;
#97401 = VERTEX_POINT ( 'NONE', #37328 ) ;
#97402 = CARTESIAN_POINT ( 'NONE',  ( 153.4289928607825573, 264.9001843414388873, 17.27358709529985958 ) ) ;
#97403 = CARTESIAN_POINT ( 'NONE',  ( -19.65312891409030271, 93.06504152958497400, 59.99999999999999289 ) ) ;
#97404 = CARTESIAN_POINT ( 'NONE',  ( 66.56647152974866799, 68.76039119326856053, 4.744323796004452198 ) ) ;
#97405 = CARTESIAN_POINT ( 'NONE',  ( 155.1601726304954809, 261.9016930232608615, -18.56587418422714464 ) ) ;
#97406 = ORIENTED_EDGE ( 'NONE', *, *, #1496, .T. ) ;
#97407 = ORIENTED_EDGE ( 'NONE', *, *, #46259, .T. ) ;
#97408 = B_SPLINE_CURVE_WITH_KNOTS ( 'NONE', 3,
 ( #11041, #57105, #41918, #86094, #16618, #47514, #39895 ),
 .UNSPECIFIED., .F., .F.,
 ( 4, 3, 4 ),
 ( 0.000000000000000000, 0.001498044977021790319, 0.001501190957620832577 ),
 .UNSPECIFIED. ) ;
#97410 = CARTESIAN_POINT ( 'NONE',  ( 163.8040269124969939, 246.9300982336122559, 6.025552750865228013 ) ) ;
#97409 = CARTESIAN_POINT ( 'NONE',  ( 159.1615944546315689, 279.6649321670822133, -9.874806447338704274 ) ) ;
#97411 = CARTESIAN_POINT ( 'NONE',  ( 192.7507137768506880, 296.7929658737652971, 11.30364540927242345 ) ) ;
#97412 = ORIENTED_EDGE ( 'NONE', *, *, #28697, .T. ) ;
#97413 = CARTESIAN_POINT ( 'NONE',  ( 124.7815979145579632, 254.3967562850346553, -4.648177544792955347E-16 ) ) ;
#97414 = CARTESIAN_POINT ( 'NONE',  ( 80.41065583177754661, 57.49148768039361812, -16.58946210043120217 ) ) ;
#97415 = CARTESIAN_POINT ( 'NONE',  ( 178.3247016823351601, 264.0066948325919043, 15.02962100587847871 ) ) ;
#97417 = EDGE_CURVE ( 'NONE', #81475, #21873, #50564, .T. ) ;
#97416 = ORIENTED_EDGE ( 'NONE', *, *, #28447, .T. ) ;
#97418 = CARTESIAN_POINT ( 'NONE',  ( -22.42236680055709641, 157.8615022471902591, 0.000000000000000000 ) ) ;
#97419 = CARTESIAN_POINT ( 'NONE',  ( 83.57553417992789946, 212.3927522451417929, -10.00000000000009237 ) ) ;
#97420 = CARTESIAN_POINT ( 'NONE',  ( 81.05146334655599105, 43.66063824279576266, 9.461398633974173578 ) ) ;
#97421 = VERTEX_POINT ( 'NONE', #27259 ) ;
#97422 = PLANE ( 'NONE',  #48422 ) ;
#97423 = CARTESIAN_POINT ( 'NONE',  ( 164.8537203408104972, 245.1119758834023230, 2.926011033004258355 ) ) ;
#97424 = DIRECTION ( 'NONE',  ( -0.000000000000000000, -0.000000000000000000, 1.000000000000000000 ) ) ;
#97425 = VERTEX_POINT ( 'NONE', #19675 ) ;
#97426 = CARTESIAN_POINT ( 'NONE',  ( 190.0226014859668453, 301.5181949703289774, 3.835066345245774500 ) ) ;
#97427 = CARTESIAN_POINT ( 'NONE',  ( 172.0812938429579617, 263.5228582765859642, -15.46802600247669801 ) ) ;
#97428 = ORIENTED_EDGE ( 'NONE', *, *, #90756, .T. ) ;
#97429 = EDGE_CURVE ( 'NONE', #33116, #84611, #46793, .T. ) ;
#97430 = CARTESIAN_POINT ( 'NONE',  ( 94.51141663858166453, 213.8262482093457493, 3.021315404115420679E-15 ) ) ;
#97431 = EDGE_LOOP ( 'NONE', ( #28771, #45655, #3855, #87250 ) ) ;
#97432 = DIRECTION ( 'NONE',  ( -0.9213551052231903071, 0.3887219701524006754, 0.000000000000000000 ) ) ;
#97433 = VERTEX_POINT ( 'NONE', #15020 ) ;
#97434 = CARTESIAN_POINT ( 'NONE',  ( 154.1866580352537142, 265.2320175785073388, -16.52215184523099012 ) ) ;
#97435 = CARTESIAN_POINT ( 'NONE',  ( 87.88857223635071136, 44.01828834560762971, 1.459818322210690189 ) ) ;
#97436 = DIRECTION ( 'NONE',  ( 0.9439450758449176027, -0.3301025504114332709, 0.000000000000000000 ) ) ;
#97437 = DIRECTION ( 'NONE',  ( 0.5000000000000014433, -0.8660254037844379305, 0.000000000000000000 ) ) ;
#97438 = CARTESIAN_POINT ( 'NONE',  ( 19.46611421548295695, 12.20801979619928090, -3.090169943749474069 ) ) ;
#97439 = CARTESIAN_POINT ( 'NONE',  ( 157.0986688504555957, 258.9827579613123589, -16.89964245493843009 ) ) ;
#97440 = CARTESIAN_POINT ( 'NONE',  ( 178.5510943472214080, 291.5559069241597285, 6.267371293791870634 ) ) ;
#97441 = CARTESIAN_POINT ( 'NONE',  ( 197.5889545809544927, 288.4128869818045473, -18.07878478781679732 ) ) ;
#97442 = EDGE_LOOP ( 'NONE', ( #90086, #67473, #72059, #47158 ) ) ;
#97443 = CARTESIAN_POINT ( 'NONE',  ( 78.98411721334434787, 56.24657107981478532, -16.18231381929481572 ) ) ;
#97444 = CARTESIAN_POINT ( 'NONE',  ( 206.5318754762992910, 272.9232936229979032, 10.63244694018452741 ) ) ;
#97445 = AXIS2_PLACEMENT_3D ( 'NONE', #44047, #74503, #5081 ) ;
#97446 = EDGE_CURVE ( 'NONE', #89517, #98021, #95112, .T. ) ;
#97447 = CARTESIAN_POINT ( 'NONE',  ( 164.5348324038273518, 245.6643059921780718, 1.473102934610569958 ) ) ;
#97449 = ORIENTED_EDGE ( 'NONE', *, *, #11405, .F. ) ;
#97448 = DIRECTION ( 'NONE',  ( 1.000000000000000000, 0.000000000000000000, 0.000000000000000000 ) ) ;
#97450 = CARTESIAN_POINT ( 'NONE',  ( 190.3920422363981118, 300.2250452325370134, 3.000504360528113423 ) ) ;
#97451 = CARTESIAN_POINT ( 'NONE',  ( 13.83268420227240014, 8.390406791769812855, -2.889640176918245968E-15 ) ) ;
#97452 = ORIENTED_EDGE ( 'NONE', *, *, #20682, .F. ) ;
#97453 = CARTESIAN_POINT ( 'NONE',  ( 190.9657205613840176, 299.8846648141192190, 6.643422157963062347 ) ) ;
#97454 = EDGE_CURVE ( 'NONE', #60835, #47928, #19006, .T. ) ;
#97455 = CARTESIAN_POINT ( 'NONE',  ( 82.02356888928309786, 52.10171163115919057, -14.99001706985075622 ) ) ;
#97456 = CARTESIAN_POINT ( 'NONE',  ( 196.0051728737935832, 265.8263463907475170, 8.406970388261065352 ) ) ;
#97457 = CARTESIAN_POINT ( 'NONE',  ( 18.45529574749610902, 12.78380873178786281, -6.180339887498949025 ) ) ;
#97458 = CARTESIAN_POINT ( 'NONE',  ( 199.1664853598643958, 285.6805235222289525, -17.06967930939392986 ) ) ;
#97459 = CARTESIAN_POINT ( 'NONE',  ( 148.7148527636650783, 273.0653145036440606, -9.755595106506282477 ) ) ;
#97460 = EDGE_LOOP ( 'NONE', ( #92576, #86773, #57381, #75466 ) ) ;
#97462 = EDGE_CURVE ( 'NONE', #91470, #59759, #35846, .T. ) ;
#97461 = FACE_OUTER_BOUND ( 'NONE', #26997, .T. ) ;
#97463 = CARTESIAN_POINT ( 'NONE',  ( 205.6722311478874019, 272.8858671130868743, 10.04445090448162325 ) ) ;
#97464 = CARTESIAN_POINT ( 'NONE',  ( -22.42236680055709641, 157.8615022471902591, 0.000000000000000000 ) ) ;
#97465 = CARTESIAN_POINT ( 'NONE',  ( 165.0156970625405108, 244.8314239717225007, -1.890480716182876719 ) ) ;
#97466 = CARTESIAN_POINT ( 'NONE',  ( 28.94376495785951775, 187.5177522451418497, -10.00000000000009592 ) ) ;
#97467 = CARTESIAN_POINT ( 'NONE',  ( 104.5854977735480560, 237.3149278399160949, 9.188101187500093303 ) ) ;
#97468 = CARTESIAN_POINT ( 'NONE',  ( 183.9376067633702405, 297.0345910832352843, -2.798678428840943866 ) ) ;
#97469 = EDGE_CURVE ( 'NONE', #45532, #94007, #64645, .T. ) ;
#97470 = CARTESIAN_POINT ( 'NONE',  ( 162.6526018557966324, 249.3110776357280542, -10.56149055985843077 ) ) ;
#97471 = CARTESIAN_POINT ( 'NONE',  ( 84.40414035640600332, 50.68119616098906022, 13.77015003724606146 ) ) ;
#97472 = CARTESIAN_POINT ( 'NONE',  ( 162.5705829494080490, 249.0664858459717550, 10.39261705965051341 ) ) ;
#97473 = CARTESIAN_POINT ( 'NONE',  ( 42.15091268916992817, 185.9548013555409796, -4.594050593750042211 ) ) ;
#97474 = CARTESIAN_POINT ( 'NONE',  ( 200.8828793852583203, 282.7076418644388696, 17.90302398138411633 ) ) ;
#97475 = ORIENTED_EDGE ( 'NONE', *, *, #44629, .T. ) ;
#97476 = ORIENTED_EDGE ( 'NONE', *, *, #11542, .T. ) ;
#97478 = ADVANCED_FACE ( 'NONE', ( #1845 ), #9948, .T. ) ;
#97477 = CARTESIAN_POINT ( 'NONE',  ( 191.2475944631368918, 298.9070266337688508, 7.531767195273644688 ) ) ;
#97479 = CARTESIAN_POINT ( 'NONE',  ( 74.46953068837864009, 68.18058761729560047, -11.53831106377694127 ) ) ;
#97480 = EDGE_CURVE ( 'NONE', #37072, #43568, #94578, .T. ) ;
#97481 = DIRECTION ( 'NONE',  ( -0.8660254037844387076, -0.4999999999999998890, -0.000000000000000000 ) ) ;
#97482 = DIRECTION ( 'NONE',  ( -0.8660254037844379305, -0.5000000000000014433, -0.000000000000000000 ) ) ;
#97483 = CARTESIAN_POINT ( 'NONE',  ( 207.3874697692679945, 271.4413608369101780, -6.809237722377445401 ) ) ;
#97484 = CARTESIAN_POINT ( 'NONE',  ( 179.1577515201028348, 287.5192237336674452, -12.38474070812784156 ) ) ;
#97485 = CARTESIAN_POINT ( 'NONE',  ( 73.80638704669730998, 68.31061168272385942, -11.57820046455322505 ) ) ;
#97486 = CARTESIAN_POINT ( 'NONE',  ( 56.57573509489573382, 191.2202760586659451, -5.415160957724236172E-17 ) ) ;
#97487 = CARTESIAN_POINT ( 'NONE',  ( 91.36976281398784749, 216.8927522451417929, -10.00000000000009059 ) ) ;
#97488 = ORIENTED_EDGE ( 'NONE', *, *, #48028, .T. ) ;
#97489 = CARTESIAN_POINT ( 'NONE',  ( 79.28302063466354355, 59.54490948036851705, -16.53220260971268374 ) ) ;
#97490 = CARTESIAN_POINT ( 'NONE',  ( 155.4606602694522337, 279.7057978631885931, -1.662051915602662966 ) ) ;
#97491 = CARTESIAN_POINT ( 'NONE',  ( 162.6262389125959373, 248.9700868899859074, -10.50380342094597808 ) ) ;
#97492 = CARTESIAN_POINT ( 'NONE',  ( 17.11727908708474288, 174.5643266524160424, 9.188101187500095079 ) ) ;
#97493 = CARTESIAN_POINT ( 'NONE',  ( 150.6916211261701619, 269.6414512649903941, -15.44346024757110847 ) ) ;
#97494 = DIRECTION ( 'NONE',  ( -0.8660254037844378194, -0.5000000000000014433, -0.000000000000000000 ) ) ;
#97495 = CARTESIAN_POINT ( 'NONE',  ( 66.30989429470714924, 68.09514072150794561, -4.585047217807751707 ) ) ;
#97496 = CARTESIAN_POINT ( 'NONE',  ( 45.77687342386973057, 206.4244531367911293, -4.594050593750046652 ) ) ;
#97497 = CARTESIAN_POINT ( 'NONE',  ( 163.7587049410067266, 247.0085981909329576, -6.137518685179130351 ) ) ;
#97498 = CARTESIAN_POINT ( 'NONE',  ( 72.50080294041131879, 57.38314053816311855, 15.83417486949919351 ) ) ;
#97499 = CARTESIAN_POINT ( 'NONE',  ( 69.20114864676770594, 68.32048725079164342, 7.706386681980674780 ) ) ;
#97500 = CARTESIAN_POINT ( 'NONE',  ( 165.0437781805843258, 244.7827860485373606, -2.050141714668513693 ) ) ;
#97501 = ORIENTED_EDGE ( 'NONE', *, *, #91868, .T. ) ;
#97502 = CARTESIAN_POINT ( 'NONE',  ( 10.48659854325162222, 166.8615022471902023, 5.000000000000051514 ) ) ;
#97503 = DIRECTION ( 'NONE',  ( 0.000000000000000000, 0.000000000000000000, 1.000000000000000000 ) ) ;
#97504 = CARTESIAN_POINT ( 'NONE',  ( 130.8102634016018442, 237.1423013555409796, -4.594050593750043987 ) ) ;
#97505 = CARTESIAN_POINT ( 'NONE',  ( 20.05074681235918277, 34.68290643055188127, 3.479690158560446702E-15 ) ) ;
#97506 = CARTESIAN_POINT ( 'NONE',  ( 182.4308498937394347, 262.1046043556927430, 13.04123466523721753 ) ) ;
#97507 = CARTESIAN_POINT ( 'NONE',  ( 188.1018771210319471, 260.4230313274653099, 6.875771660441075461 ) ) ;
#97508 = CARTESIAN_POINT ( 'NONE',  ( 98.82118972926437550, 217.8615022471902023, 5.000000000000051514 ) ) ;
#97510 = CARTESIAN_POINT ( 'NONE',  ( 75.25521838011508180, 66.92519264401985879, 13.27308740013157085 ) ) ;
#97509 = DIRECTION ( 'NONE',  ( 0.03487823687205911238, -0.06041087834082882468, 0.9975640502598247528 ) ) ;
#97511 = LINE ( 'NONE', #19524, #17359 ) ;
#97512 = ORIENTED_EDGE ( 'NONE', *, *, #68581, .T. ) ;
#97513 = CARTESIAN_POINT ( 'NONE',  ( 190.7779368023172708, 300.2099158256590385, 8.142228434510803581 ) ) ;
#97514 = CARTESIAN_POINT ( 'NONE',  ( 163.9771286558119527, 246.6302772193120916, 8.800578722892527850 ) ) ;
#97515 = DIRECTION ( 'NONE',  ( -0.8074371744834166753, -0.5899535653441180250, 0.000000000000000000 ) ) ;
#97516 = DIRECTION ( 'NONE',  ( -0.9689885751534038638, -0.2471055264905585858, 0.000000000000000000 ) ) ;
#97517 = CARTESIAN_POINT ( 'NONE',  ( 193.9623890821095245, 270.7088843966109266, -14.00671964082007293 ) ) ;
#97518 = ORIENTED_EDGE ( 'NONE', *, *, #62081, .T. ) ;
#97519 = DIRECTION ( 'NONE',  ( -0.2877784213863818774, 0.9576970189910596343, 0.000000000000000000 ) ) ;
#97520 = AXIS2_PLACEMENT_3D ( 'NONE', #53717, #60317, #92285 ) ;
#97521 = CARTESIAN_POINT ( 'NONE',  ( 171.1428126037558286, 284.1639577662504621, -11.21521392563669828 ) ) ;
#97522 = VECTOR ( 'NONE', #97893, 1000.000000000000000 ) ;
#97523 = CARTESIAN_POINT ( 'NONE',  ( 72.06430047377128290, 72.31697432814085857, 0.7629622467667349639 ) ) ;
#97524 = B_SPLINE_SURFACE_WITH_KNOTS ( 'NONE', 3, 1, ( 
 ( #39531, #14267 ),
 ( #1066, #91301 ),
 ( #994, #47580 ),
 ( #2507, #87165 ),
 ( #55662, #88153 ),
 ( #40474, #1996 ),
 ( #40961, #33389 ),
 ( #10097, #55171 ),
 ( #18201, #16689 ),
 ( #47084, #63286 ),
 ( #71906, #26298 ),
 ( #64291, #49095 ),
 ( #70386, #71406 ),
 ( #94723, #24295 ),
 ( #24780, #95240 ),
 ( #17697, #9093 ),
 ( #9611, #25809 ),
 ( #33911, #95745 ),
 ( #48600, #32882 ),
 ( #57173, #79539 ),
 ( #17179, #56684 ),
 ( #64800, #78004 ),
 ( #87667, #31874 ),
 ( #86649, #80030 ),
 ( #1507, #8596 ),
 ( #78508, #39964 ),
 ( #10598, #48081 ),
 ( #41471, #72419 ),
 ( #70900, #3023 ),
 ( #39461, #62777 ),
 ( #93735, #86156 ) ),
 .UNSPECIFIED., .F., .F., .F.,
 ( 4, 3, 3, 3, 3, 3, 3, 3, 3, 3, 4 ),
 ( 2, 2 ),
 ( 0.000000000000000000, 0.1333490885032314888, 0.3007194338854323190, 0.4699862290245113150, 0.5844252810809227316, 0.6686540514502676835, 0.7354980260655422653, 0.8028463152565505911, 0.8633854507757149355, 0.9437142632667404607, 1.000000000000000000 ),
 ( 0.000000000000000000, 1.000000000000000000 ),
 .UNSPECIFIED. ) ;
#97525 = CARTESIAN_POINT ( 'NONE',  ( 85.39968305126339487, 44.98980877744030948, 7.996374091334619294 ) ) ;
#97526 = LINE ( 'NONE', #12924, #68226 ) ;
#97527 = CARTESIAN_POINT ( 'NONE',  ( 185.4705698274941597, 296.4713422579150119, 4.661272572182228124 ) ) ;
#97528 = CARTESIAN_POINT ( 'NONE',  ( -71.61465314115659453, 63.06504152958490295, -25.00000000000000000 ) ) ;
#97529 = CARTESIAN_POINT ( 'NONE',  ( 148.5539059455934137, 274.4840833604166619, -7.867015923118076515 ) ) ;
#97530 = CARTESIAN_POINT ( 'NONE',  ( 35.43817338645655468, 49.87999306568065805, -10.00000000000000000 ) ) ;
#97531 = CARTESIAN_POINT ( 'NONE',  ( 11.77607482435655051, 8.927558733836240989, 6.180339887498953466 ) ) ;
#97532 = CARTESIAN_POINT ( 'NONE',  ( 84.46506227560851698, 231.1199935810940929, 2.679491924311251605 ) ) ;
#97533 = VERTEX_POINT ( 'NONE', #88497 ) ;
#97534 = CARTESIAN_POINT ( 'NONE',  ( 74.32283972735670829, 55.33658384534070507, 16.60204640374922036 ) ) ;
#97535 = CARTESIAN_POINT ( 'NONE',  ( 71.94643353573427191, 71.53214566342799685, 5.625104812542565114 ) ) ;
#97536 = CARTESIAN_POINT ( 'NONE',  ( 156.2331364254156085, 261.5399799853009313, -17.15694452653591640 ) ) ;
#97538 = EDGE_CURVE ( 'NONE', #49399, #73618, #51640, .T. ) ;
#97537 = ORIENTED_EDGE ( 'NONE', *, *, #48115, .F. ) ;
#97539 = CARTESIAN_POINT ( 'NONE',  ( 146.9456733906991417, 276.1296230653242105, -0.7988785540157754550 ) ) ;
#97540 = DIRECTION ( 'NONE',  ( -0.6911977992267216431, 0.7226656227773233798, 0.000000000000000000 ) ) ;
#97541 = VECTOR ( 'NONE', #18248, 1000.000000000000227 ) ;
#97542 = CARTESIAN_POINT ( 'NONE',  ( 164.0777181605478745, 246.4560510864015441, 5.763760713451748785 ) ) ;
#97543 = CARTESIAN_POINT ( 'NONE',  ( 88.42017002704760387, 43.92753743058676719, 1.721442031696316377 ) ) ;
#97544 = CARTESIAN_POINT ( 'NONE',  ( 75.14833501749109246, 53.26070039134698675, 16.02921398246552087 ) ) ;
#97545 = EDGE_LOOP ( 'NONE', ( #57385, #37948, #13853, #89452 ) ) ;
#97546 = CARTESIAN_POINT ( 'NONE',  ( 77.38680066200176100, 224.6744531367911293, 4.594050593750047540 ) ) ;
#97547 = CARTESIAN_POINT ( 'NONE',  ( 198.6706607409806793, 282.8345047477174035, 17.53097579465153899 ) ) ;
#97548 = CARTESIAN_POINT ( 'NONE',  ( 84.47860975560725194, 49.82577972120141396, -13.24615549146050597 ) ) ;
#97549 = CARTESIAN_POINT ( 'NONE',  ( 181.9149013745693821, 257.5326720783834844, -5.998799190420378125 ) ) ;
#97550 = ORIENTED_EDGE ( 'NONE', *, *, #41974, .F. ) ;
#97551 = EDGE_CURVE ( 'NONE', #95379, #24879, #88001, .T. ) ;
#97552 = ORIENTED_EDGE ( 'NONE', *, *, #60522, .F. ) ;
#97553 = CARTESIAN_POINT ( 'NONE',  ( -9.093968788749004162, 61.55273967620898645, -10.00000000000000000 ) ) ;
#97554 = EDGE_CURVE ( 'NONE', #3234, #34021, #71755, .T. ) ;
#97555 = ORIENTED_EDGE ( 'NONE', *, *, #41492, .F. ) ;
#97556 = FACE_OUTER_BOUND ( 'NONE', #81099, .T. ) ;
#97557 = EDGE_LOOP ( 'NONE', ( #37241, #25641, #56744, #69611 ) ) ;
#97558 = CARTESIAN_POINT ( 'NONE',  ( 75.15495416781809013, 59.46171984578271719, 15.76924538335189396 ) ) ;
#97559 = CARTESIAN_POINT ( 'NONE',  ( 203.2369479875374623, 278.6302754407888074, -16.66242713208754367 ) ) ;
#97560 = ORIENTED_EDGE ( 'NONE', *, *, #8996, .T. ) ;
#97561 = CARTESIAN_POINT ( 'NONE',  ( 158.4485968073939546, 275.2084588272041401, -13.86993402366507944 ) ) ;
#97562 = CARTESIAN_POINT ( 'NONE',  ( 81.91642347199164931, 41.06807863313601104, 3.527822212322262896 ) ) ;
#97563 = CARTESIAN_POINT ( 'NONE',  ( 176.2806738015978567, 292.0729657887243889, -5.728603416521778513 ) ) ;
#97564 = CARTESIAN_POINT ( 'NONE',  ( 148.0346525705264469, 274.2434557974783615, -9.381294579651672905 ) ) ;
#97565 = LINE ( 'NONE', #26650, #51536 ) ;
#97566 = CARTESIAN_POINT ( 'NONE',  ( 168.3608126884537342, 267.2090580166349696, -17.33422820738878301 ) ) ;
#97567 = CARTESIAN_POINT ( 'NONE',  ( 76.73007396570457672, 60.00601218884718691, 15.86901231296716119 ) ) ;
#97568 = B_SPLINE_CURVE_WITH_KNOTS ( 'NONE', 3,
 ( #23839, #70448, #1573, #31936, #78571, #9677, #93796, #24357, #86211, #55228, #71472, #17767, #32456, #54732 ),
 .UNSPECIFIED., .F., .F.,
 ( 4, 2, 2, 2, 2, 2, 4 ),
 ( 0.002656117551711010150, 0.002819458382855290820, 0.002982799213999571923, 0.003146140045143852593, 0.003309480876288133262, 0.003962844200865130173, 0.005269570850019082361 ),
 .UNSPECIFIED. ) ;
#97569 = CARTESIAN_POINT ( 'NONE',  ( 9.941082954516854642, 14.24335787977761036, -9.188101187500008038 ) ) ;
#97570 = ORIENTED_EDGE ( 'NONE', *, *, #21934, .T. ) ;
#97571 = CARTESIAN_POINT ( 'NONE',  ( 167.3679022544422423, 283.9162485395274302, 9.094197141742041524 ) ) ;
#97573 = ORIENTED_EDGE ( 'NONE', *, *, #29360, .F. ) ;
#97572 = CARTESIAN_POINT ( 'NONE',  ( 200.5676506042510141, 270.4838747193165887, 9.277400309797105393 ) ) ;
#97574 = CARTESIAN_POINT ( 'NONE',  ( 1.898513289055925979, 165.2365022471902023, -10.00000000000009237 ) ) ;
#97575 = DIRECTION ( 'NONE',  ( -0.4999999999999987788, 0.8660254037844392627, 0.000000000000000000 ) ) ;
#97576 = CARTESIAN_POINT ( 'NONE',  ( 76.06972881656521679, 64.70592176699422282, -14.35599997814377282 ) ) ;
#97577 = CARTESIAN_POINT ( 'NONE',  ( 149.0751598600045611, 276.4070164360279591, -5.531358103402955528 ) ) ;
#97578 = CARTESIAN_POINT ( 'NONE',  ( -22.42236680055709641, 157.8615022471902591, 0.000000000000000000 ) ) ;
#97579 = DIRECTION ( 'NONE',  ( -0.000000000000000000, 0.000000000000000000, -1.000000000000000000 ) ) ;
#97580 = CARTESIAN_POINT ( 'NONE',  ( 168.3515070634022948, 252.8892669010618306, 12.01402775453702709 ) ) ;
#97581 = CARTESIAN_POINT ( 'NONE',  ( 194.9222774061866232, 292.5393265380751586, 15.09658607083830439 ) ) ;
#97582 = ORIENTED_EDGE ( 'NONE', *, *, #97348, .F. ) ;
#97583 = EDGE_CURVE ( 'NONE', #47298, #18338, #49429, .T. ) ;
#97584 = CARTESIAN_POINT ( 'NONE',  ( 77.55708701662783255, 61.25438087302521240, -15.77812108083495524 ) ) ;
#97585 = EDGE_LOOP ( 'NONE', ( #21287, #52404, #9307, #3697 ) ) ;
#97586 = CARTESIAN_POINT ( 'NONE',  ( 10.91961124514384274, 167.1115022471901739, -5.000000000000041744 ) ) ;
#97587 = EDGE_CURVE ( 'NONE', #9722, #8604, #33230, .T. ) ;
#97588 = EDGE_CURVE ( 'NONE', #89224, #57901, #44260, .T. ) ;
#97589 = CARTESIAN_POINT ( 'NONE',  ( 175.0183846948854125, 281.5670661755301580, -14.11114436949414674 ) ) ;
#97590 = CARTESIAN_POINT ( 'NONE',  ( 196.1252721995043942, 284.4712197134549001, -17.81715240067734030 ) ) ;
#97591 = CARTESIAN_POINT ( 'NONE',  ( 149.0802055316563326, 272.4325049467973940, 12.84384348890831085 ) ) ;
#97592 = DIRECTION ( 'NONE',  ( -0.9820299053580078263, -0.1887253692075926415, 0.000000000000000000 ) ) ;
#97594 = CARTESIAN_POINT ( 'NONE',  ( 88.22316733864592209, 44.26875609612614682, 2.029272769359140582 ) ) ;
#97593 = DIRECTION ( 'NONE',  ( -0.5544813661758285495, -0.8321961394790213795, 0.000000000000000000 ) ) ;
#97595 = CARTESIAN_POINT ( 'NONE',  ( -19.65312891409030271, 93.06504152958497400, 177.5919119679930134 ) ) ;
#97596 = ORIENTED_EDGE ( 'NONE', *, *, #27995, .T. ) ;
#97597 = B_SPLINE_CURVE_WITH_KNOTS ( 'NONE', 3,
 ( #12806, #5186, #42176, #20902 ),
 .UNSPECIFIED., .F., .F.,
 ( 4, 4 ),
 ( 0.04303599427739471933, 0.04887120950165264183 ),
 .UNSPECIFIED. ) ;
#97598 = EDGE_CURVE ( 'NONE', #65714, #49571, #29138, .T. ) ;
#97599 = VERTEX_POINT ( 'NONE', #90482 ) ;
#97600 = DIRECTION ( 'NONE',  ( -0.4999999999999987788, 0.8660254037844392627, 0.000000000000000000 ) ) ;
#97601 = EDGE_CURVE ( 'NONE', #41192, #87863, #43315, .T. ) ;
#97602 = CARTESIAN_POINT ( 'NONE',  ( -19.65312891409030271, 93.06504152958497400, 10.00000000000000888 ) ) ;
#97603 = AXIS2_PLACEMENT_3D ( 'NONE', #48137, #48655, #62318 ) ;
#97604 = EDGE_CURVE ( 'NONE', #59369, #93038, #65625, .T. ) ;
#97605 = LINE ( 'NONE', #38109, #15787 ) ;
#97606 = CARTESIAN_POINT ( 'NONE',  ( 175.6309865724497001, 290.9702953720650385, 2.692108822669778245 ) ) ;
#97607 = CARTESIAN_POINT ( 'NONE',  ( 192.3401793061076717, 297.5040324353506094, 12.56432540404525611 ) ) ;
#97608 = DIRECTION ( 'NONE',  ( -0.3696446237802352708, -0.9291732088853876803, 0.000000000000000000 ) ) ;
#97609 = CARTESIAN_POINT ( 'NONE',  ( 6.454167755106333892, 174.5333772461660828, 9.188101187500095079 ) ) ;
#97610 = CARTESIAN_POINT ( 'NONE',  ( 101.4736528484039724, 220.2048013555409796, 4.594050593750051981 ) ) ;
#97611 = CARTESIAN_POINT ( 'NONE',  ( 87.79988801543919408, 44.42003386087115757, -3.950855289944771975 ) ) ;
#97612 = CARTESIAN_POINT ( 'NONE',  ( 186.3706575779193599, 296.6012036956348652, -7.271390144495396335 ) ) ;
#97613 = CARTESIAN_POINT ( 'NONE',  ( 77.87934091665805170, 50.93078553898673988, 15.28564964083246558 ) ) ;
#97614 = VECTOR ( 'NONE', #37669, 999.9999999999998863 ) ;
#97615 = CARTESIAN_POINT ( 'NONE',  ( 77.04391226188317887, 50.32083652003289842, 15.24994158219132068 ) ) ;
#97616 = CARTESIAN_POINT ( 'NONE',  ( 163.3740049908953438, 249.6749180501957710, -11.76522313559978627 ) ) ;
#97617 = CARTESIAN_POINT ( 'NONE',  ( 110.0000000000000000, 0.000000000000000000, 59.99999999999999289 ) ) ;
#97618 = CARTESIAN_POINT ( 'NONE',  ( 147.7467138384290308, 274.7421803109381813, -9.190172068879620682 ) ) ;
#97619 = CARTESIAN_POINT ( 'NONE',  ( 84.20844839706383311, 50.59124878818558813, 13.78330635088765455 ) ) ;
#97620 = CARTESIAN_POINT ( 'NONE',  ( 196.3986213162682759, 266.7212399403405243, 8.097488202709509864 ) ) ;
#97621 = CARTESIAN_POINT ( 'NONE',  ( 77.90020070641381267, 227.3297689869269504, -2.679491924311252493 ) ) ;
#97622 = CARTESIAN_POINT ( 'NONE',  ( 56.65657787896151376, 213.5177522451419065, 5.000000000000046185 ) ) ;
#97623 = CARTESIAN_POINT ( 'NONE',  ( 54.07885559584777013, 190.4824982072973967, 3.021315404115420679E-15 ) ) ;
#97624 = CARTESIAN_POINT ( 'NONE',  ( 152.8894687064977234, 278.3516875449029158, -6.243347624783317507 ) ) ;
#97626 = EDGE_CURVE ( 'NONE', #32206, #1197, #28124, .T. ) ;
#97625 = B_SPLINE_CURVE_WITH_KNOTS ( 'NONE', 3,
 ( #89528, #20089, #49978, #97119 ),
 .UNSPECIFIED., .F., .F.,
 ( 4, 4 ),
 ( 0.001250264319432415911, 0.006536272345052643665 ),
 .UNSPECIFIED. ) ;
#97627 = CARTESIAN_POINT ( 'NONE',  ( 90.72943840876202160, 217.0643266524159571, -9.188101187500093303 ) ) ;
#97628 = CARTESIAN_POINT ( 'NONE',  ( 8.064688198948626763, 22.84336893147754211, -7.433330006724137462 ) ) ;
#97629 = CARTESIAN_POINT ( 'NONE',  ( 163.2245414155497087, 258.2687556262928297, 16.54154467503536452 ) ) ;
#97631 = CARTESIAN_POINT ( 'NONE',  ( 199.9055245033136714, 284.4004701769926555, 18.46055504797378077 ) ) ;
#97630 = FACE_OUTER_BOUND ( 'NONE', #2738, .T. ) ;
#97632 = FACE_OUTER_BOUND ( 'NONE', #36941, .T. ) ;
#97633 = CARTESIAN_POINT ( 'NONE',  ( 75.76889645089327985, 65.47676480558789081, 14.28475327549652185 ) ) ;
#97634 = CARTESIAN_POINT ( 'NONE',  ( 80.22522614674704755, 44.29332910989383265, 11.37138867391942476 ) ) ;
#97635 = CARTESIAN_POINT ( 'NONE',  ( 37.36761971798259196, 27.28920272979929607, -7.433330006724141015 ) ) ;
#97636 = CARTESIAN_POINT ( 'NONE',  ( 193.0761489135300906, 296.2292956824684893, -11.99675185248219655 ) ) ;
#97637 = CARTESIAN_POINT ( 'NONE',  ( 127.8330407560429904, 254.6115022471903160, -5.000000000000047962 ) ) ;
#97638 = ORIENTED_EDGE ( 'NONE', *, *, #97843, .T. ) ;
#97639 = CARTESIAN_POINT ( 'NONE',  ( 20.70865909420142259, 30.14336893147755703, 7.433330006724141015 ) ) ;
#97640 = DIRECTION ( 'NONE',  ( -1.000000000000000000, 0.000000000000000000, 5.984665299743594308E-16 ) ) ;
#97641 = CARTESIAN_POINT ( 'NONE',  ( 193.2140586456748679, 295.9904290195353269, -12.67640480829088823 ) ) ;
#97642 = CARTESIAN_POINT ( 'NONE',  ( 190.4205601722502479, 287.1571841927307673, -15.84311712791906857 ) ) ;
#97643 = B_SPLINE_CURVE_WITH_KNOTS ( 'NONE', 3,
 ( #93018, #54464, #14982, #30701, #786, #1302, #33193, #64094, #10908, #56490, #55470, #86456, #56978, #95039, #87477, #33711, #80341, #48398, #64603, #41784, #87964, #40769, #25603, #18011, #93532, #16489, #10405, #32186, #31672, #8890, #86957, #95558, #71721, #85963, #62568, #49394, #48904, #79839, #39759, #41275, #72217, #47385, #18508, #24088, #2821, #9397 ),
 .UNSPECIFIED., .F., .F.,
 ( 4, 2, 2, 2, 2, 2, 2, 2, 2, 2, 2, 2, 2, 2, 2, 2, 2, 2, 2, 2, 2, 2, 4 ),
 ( 0.0009098864418214376668, 0.001395788648591240848, 0.001881690855361043812, 0.002124641958745928597, 0.002367593062130813383, 0.002489068613823246234, 0.002610544165515678652, 0.002732019717208111504, 0.002853495268900544356, 0.003096446372285409192, 0.003339397475670274895, 0.003825299682440005435, 0.004797104095979466513, 0.005768908509518927592, 0.006254810716288658132, 0.006740712923058388671, 0.006862188474750856651, 0.006922926250597124034, 0.006983664026443391418, 0.007226615129828508656, 0.007712517336598743133, 0.008198419543368978477, 0.008684321750139212953 ),
 .UNSPECIFIED. ) ;
#97644 = ORIENTED_EDGE ( 'NONE', *, *, #89156, .T. ) ;
#97645 = CARTESIAN_POINT ( 'NONE',  ( 70.37335645893944047, 61.05447394354146695, 14.89803406748600523 ) ) ;
#97646 = CARTESIAN_POINT ( 'NONE',  ( 198.6587626159274294, 286.5599251108861267, 17.99840276545888784 ) ) ;
#97647 = CARTESIAN_POINT ( 'NONE',  ( 178.3542226995226940, 255.3138203415698513, 7.881446944319069559 ) ) ;
#97648 = CARTESIAN_POINT ( 'NONE',  ( 201.5189872289815867, 266.7509884862435570, -2.318412474989284267 ) ) ;
#97649 = CARTESIAN_POINT ( 'NONE',  ( 130.4311169673963207, 256.1115022471902876, -5.000000000000047962 ) ) ;
#97650 = CARTESIAN_POINT ( 'NONE',  ( 88.24427088181241174, 44.33808775276298775, -2.403621623811780683 ) ) ;
#97651 = ORIENTED_EDGE ( 'NONE', *, *, #3349, .T. ) ;
#97652 = CARTESIAN_POINT ( 'NONE',  ( 81.53430506435155678, 46.66854249687567346, -12.70094556911029038 ) ) ;
#97653 = ORIENTED_EDGE ( 'NONE', *, *, #27395, .F. ) ;
#97654 = CARTESIAN_POINT ( 'NONE',  ( 196.6801871783479498, 265.3273392373002366, -4.500484501757973099 ) ) ;
#97655 = CARTESIAN_POINT ( 'NONE',  ( 85.39747940901729351, 43.05929300263707660, 3.749131589292365341 ) ) ;
#97656 = ORIENTED_EDGE ( 'NONE', *, *, #62450, .F. ) ;
#97657 = CARTESIAN_POINT ( 'NONE',  ( 77.09671571037877413, 63.64621968971055566, -15.01522762802964905 ) ) ;
#97659 = EDGE_CURVE ( 'NONE', #71349, #64147, #53940, .T. ) ;
#97658 = ORIENTED_EDGE ( 'NONE', *, *, #87771, .T. ) ;
#97660 = CARTESIAN_POINT ( 'NONE',  ( 46.89542285554266954, 70.53237680267110932, -10.00000000000000000 ) ) ;
#97661 = CARTESIAN_POINT ( 'NONE',  ( 205.9877610862153858, 273.8657273917527846, 10.74600286489862988 ) ) ;
#97662 = CARTESIAN_POINT ( 'NONE',  ( 150.4851912698882757, 251.5643266524160424, -9.188101187500093303 ) ) ;
#97663 = CARTESIAN_POINT ( 'NONE',  ( 193.0139627561028988, 296.3370052666596735, -13.53354153023428275 ) ) ;
#97664 = CARTESIAN_POINT ( 'NONE',  ( 196.3249884498792994, 275.2518087180711177, 16.06659936265807431 ) ) ;
#97665 = CARTESIAN_POINT ( 'NONE',  ( 39.54951596113196644, 25.76004757982092741, 5.678558825948272215 ) ) ;
#97666 = CARTESIAN_POINT ( 'NONE',  ( 76.63781029191453342, 59.43798239135757910, -15.94570803233245293 ) ) ;
#97668 = EDGE_CURVE ( 'NONE', #17163, #27033, #10564, .T. ) ;
#97667 = CARTESIAN_POINT ( 'NONE',  ( 167.4994950215155427, 276.2173684559796243, 14.96917790999040321 ) ) ;
#97669 = CARTESIAN_POINT ( 'NONE',  ( 87.57113761115280681, 45.50653608346983248, 6.901679451313498248 ) ) ;
#97670 = EDGE_CURVE ( 'NONE', #25798, #1197, #27649, .T. ) ;
#97671 = ORIENTED_EDGE ( 'NONE', *, *, #45339, .F. ) ;
#97672 = ORIENTED_EDGE ( 'NONE', *, *, #79077, .T. ) ;
#97673 = CARTESIAN_POINT ( 'NONE',  ( 81.31286011338397657, 42.41139741970113164, 7.506920912044924954 ) ) ;
#97675 = CARTESIAN_POINT ( 'NONE',  ( 162.3916291218297943, 272.3095098889435235, -15.78716446736534351 ) ) ;
#97674 = CARTESIAN_POINT ( 'NONE',  ( 173.9599451638853509, 256.5427416416744677, -12.41841015343009680 ) ) ;
#97676 = CARTESIAN_POINT ( 'NONE',  ( 85.72569040894076409, 48.78770323298218869, -12.00764425159951898 ) ) ;
#97677 = CARTESIAN_POINT ( 'NONE',  ( 168.2235428883953432, 249.7409626584020543, -8.343714295448053875 ) ) ;
#97678 = VECTOR ( 'NONE', #8633, 1000.000000000000114 ) ;
#97679 = CARTESIAN_POINT ( 'NONE',  ( 147.6130046165826570, 276.0663062336524263, 0.7645130601501862744 ) ) ;
#97680 = CARTESIAN_POINT ( 'NONE',  ( 189.8147415777049218, 301.8782188922952514, -0.5019643756309712934 ) ) ;
#97681 = CARTESIAN_POINT ( 'NONE',  ( 84.14312167556933275, 48.98415679381830756, 0.000000000000000000 ) ) ;
#97682 = CARTESIAN_POINT ( 'NONE',  ( 168.9285091408607684, 266.8905904589466900, 17.77692745299157195 ) ) ;
#97683 = CIRCLE ( 'NONE', #37758, 70.00000000000001421 ) ;
#97684 = CARTESIAN_POINT ( 'NONE',  ( 178.7706546344515743, 255.8485219706211353, 4.885452066709516039 ) ) ;
#97685 = CARTESIAN_POINT ( 'NONE',  ( 97.84665082640911749, 236.4869531367911293, 4.594050593750046652 ) ) ;
#97686 = DIRECTION ( 'NONE',  ( -0.9909246428798921258, -0.1344185706417024839, 0.000000000000000000 ) ) ;
#97687 = CARTESIAN_POINT ( 'NONE',  ( 192.0122679602540643, 293.3270677385487488, -14.68313672456705810 ) ) ;
#97688 = ORIENTED_EDGE ( 'NONE', *, *, #49730, .F. ) ;
#97689 = ORIENTED_EDGE ( 'NONE', *, *, #38257, .T. ) ;
#97690 = CARTESIAN_POINT ( 'NONE',  ( 87.20542010897281671, 46.22683608894070062, -9.058801420718495478 ) ) ;
#97691 = CARTESIAN_POINT ( 'NONE',  ( 195.0951974243075142, 285.7261168938122751, -17.71149292247018181 ) ) ;
#97692 = CARTESIAN_POINT ( 'NONE',  ( 195.8248271798537417, 291.4684452715354155, 17.35175160929494709 ) ) ;
#97693 = CARTESIAN_POINT ( 'NONE',  ( 159.7132918459648181, 254.0154592091499239, -16.90058287995827158 ) ) ;
#97694 = CARTESIAN_POINT ( 'NONE',  ( 208.3210024379012282, 269.8244348243121635, 2.045688540111487264 ) ) ;
#97695 = VERTEX_POINT ( 'NONE', #58516 ) ;
#97696 = ORIENTED_EDGE ( 'NONE', *, *, #26131, .T. ) ;
#97697 = EDGE_CURVE ( 'NONE', #58893, #87878, #20048, .T. ) ;
#97698 = CARTESIAN_POINT ( 'NONE',  ( 163.2000388741132895, 247.9762362032568035, -11.19676374274550312 ) ) ;
#97699 = EDGE_LOOP ( 'NONE', ( #96621, #57249, #54039, #70183 ) ) ;
#97700 = CARTESIAN_POINT ( 'NONE',  ( 81.30975366074838462, 56.24313983998633404, -16.44754541364717326 ) ) ;
#97701 = CARTESIAN_POINT ( 'NONE',  ( 99.09182266439904652, 228.0177522451418781, -10.00000000000009592 ) ) ;
#97702 = CARTESIAN_POINT ( 'NONE',  ( 81.96835758032909780, 44.03121486362022807, 9.310397246505914381 ) ) ;
#97704 = CARTESIAN_POINT ( 'NONE',  ( 199.9134407114337364, 283.6250491837689651, 17.05367660732407842 ) ) ;
#97703 = CARTESIAN_POINT ( 'NONE',  ( 141.9874905431360332, 240.5327760586659451, 1.948934522072303157E-15 ) ) ;
#97705 = CARTESIAN_POINT ( 'NONE',  ( -55.34571675428254878, 55.61878071410718150, 59.99999999999999289 ) ) ;
#97706 = ORIENTED_EDGE ( 'NONE', *, *, #95215, .F. ) ;
#97707 = CARTESIAN_POINT ( 'NONE',  ( 190.8545714895799392, 300.0771806536980648, -5.516553996882049837 ) ) ;
#97708 = CARTESIAN_POINT ( 'NONE',  ( 82.00328269441645546, 49.67669804047655902, 13.87900603238908026 ) ) ;
#97709 = CARTESIAN_POINT ( 'NONE',  ( 190.0760587457662325, 263.4785607165754868, -9.739317369409583591 ) ) ;
#97710 = EDGE_CURVE ( 'NONE', #15038, #21882, #49126, .T. ) ;
#97711 = CARTESIAN_POINT ( 'NONE',  ( 173.2675837151294900, 251.6514125879787969, -0.3741643316691787846 ) ) ;
#97712 = CARTESIAN_POINT ( 'NONE',  ( 178.3763904113375247, 285.3699055491184140, 13.04576391269180746 ) ) ;
#97713 = CARTESIAN_POINT ( 'NONE',  ( 72.08446838866018425, 72.31872904169155447, 3.483634709754478642 ) ) ;
#97714 = CARTESIAN_POINT ( 'NONE',  ( 197.9956738476683711, 281.2438040225179634, -16.56933298855467740 ) ) ;
#97715 = DIRECTION ( 'NONE',  ( 0.5000000000000014433, -0.8660254037844378194, 0.000000000000000000 ) ) ;
#97716 = CARTESIAN_POINT ( 'NONE',  ( 79.65053214023340900, 48.80355187758674873, 14.09044789434124922 ) ) ;
#97717 = CARTESIAN_POINT ( 'NONE',  ( 67.98237831623328020, 69.73113656707158725, -1.821194602964219866 ) ) ;
#97718 = CARTESIAN_POINT ( 'NONE',  ( 61.82584055745639517, 200.3768266524159856, -9.188101187500091527 ) ) ;
#97719 = CARTESIAN_POINT ( 'NONE',  ( 159.3586121662929713, 254.6297824347537642, -15.50090345830412630 ) ) ;
#97720 = CARTESIAN_POINT ( 'NONE',  ( 77.77576245277342082, 61.68761876588025217, 16.07113493600748200 ) ) ;
#97721 = CARTESIAN_POINT ( 'NONE',  ( 162.7070706717508699, 248.8300821762643693, -9.986337079333621247 ) ) ;
#97722 = EDGE_CURVE ( 'NONE', #79294, #9648, #60053, .T. ) ;
#97723 = PLANE ( 'NONE',  #27121 ) ;
#97725 = DIRECTION ( 'NONE',  ( 0.5000000000000014433, -0.8660254037844378194, 0.000000000000000000 ) ) ;
#97724 = CARTESIAN_POINT ( 'NONE',  ( 73.34867049892106650, 70.14346970443526175, -9.354907352444854496 ) ) ;
#97726 = CARTESIAN_POINT ( 'NONE',  ( 78.60844116473590759, 49.40628642118211644, 15.13497465346012660 ) ) ;
#97727 = CARTESIAN_POINT ( 'NONE',  ( 40.15112871924373650, 31.38052372038644933, 10.00000000000000533 ) ) ;
#97728 = CARTESIAN_POINT ( 'NONE',  ( 74.42293240810788291, 58.11393764944256191, -16.37586900588139116 ) ) ;
#97729 = FACE_OUTER_BOUND ( 'NONE', #69147, .T. ) ;
#97730 = CARTESIAN_POINT ( 'NONE',  ( 72.29113772080887657, 72.04443532774766368, 3.396961777288337814 ) ) ;
#97731 = AXIS2_PLACEMENT_3D ( 'NONE', #12176, #5561, #6567 ) ;
#97732 = CARTESIAN_POINT ( 'NONE',  ( 17.98330449086917682, 175.0643266524160140, -9.188101187500093303 ) ) ;
#97733 = CARTESIAN_POINT ( 'NONE',  ( 69.98676787869841576, 71.07097491031876757, 3.687581967789058446 ) ) ;
#97734 = VERTEX_POINT ( 'NONE', #61507 ) ;
#97735 = CARTESIAN_POINT ( 'NONE',  ( 49.03918259513505973, 79.59780946358317522, 177.5919119679930134 ) ) ;
#97737 = CARTESIAN_POINT ( 'NONE',  ( 201.7504478526379899, 278.7391314730009526, 15.42661883977095805 ) ) ;
#97736 = CIRCLE ( 'NONE', #52372, 70.00000000000001421 ) ;
#97738 = CARTESIAN_POINT ( 'NONE',  ( 178.3142739445455618, 279.4967965441328488, 17.12304257816909825 ) ) ;
#97739 = CARTESIAN_POINT ( 'NONE',  ( 208.0287371622045782, 270.3306531311065442, 3.558879245883286746 ) ) ;
#97740 = CARTESIAN_POINT ( 'NONE',  ( 71.61159621314317292, 72.40963678617121957, -1.342178375522450562 ) ) ;
#97741 = CARTESIAN_POINT ( 'NONE',  ( 61.44712799118319424, 194.0327760586659451, 1.948934522072302763E-15 ) ) ;
#97742 = CARTESIAN_POINT ( 'NONE',  ( 87.37978634506822573, 45.87160741090568905, 8.420816086386249566 ) ) ;
#97743 = CARTESIAN_POINT ( 'NONE',  ( 171.1378123370926971, 286.9384401993552842, 7.092917925564754533 ) ) ;
#97744 = CARTESIAN_POINT ( 'NONE',  ( 146.8000281410530192, 276.3818880375922049, 4.652863924796177386 ) ) ;
#97745 = CARTESIAN_POINT ( 'NONE',  ( 44.43605786102924782, 27.78380873178790722, -6.180339887498949025 ) ) ;
#97746 = CARTESIAN_POINT ( 'NONE',  ( 197.8517725239618699, 287.3315203694608044, 17.01882341879843707 ) ) ;
#97747 = CARTESIAN_POINT ( 'NONE',  ( 178.4307736886035229, 293.0376200449680368, 2.618413240329335867 ) ) ;
#97748 = CARTESIAN_POINT ( 'NONE',  ( 178.4481950008050433, 276.1063989467955935, 16.34093626456154524 ) ) ;
#97749 = CARTESIAN_POINT ( 'NONE',  ( 72.94799627050929303, 62.71678750348689846, 14.32205132279771220 ) ) ;
#97750 = CARTESIAN_POINT ( 'NONE',  ( 74.02122080984301533, 67.34355054658300332, -11.96938251222216998 ) ) ;
#97751 = B_SPLINE_SURFACE_WITH_KNOTS ( 'NONE', 3, 1, ( 
 ( #67147, #34262 ),
 ( #81898, #59023 ),
 ( #43342, #20570 ),
 ( #4358, #89516 ),
 ( #5361, #21079 ),
 ( #34749, #96608 ),
 ( #36241, #27170 ),
 ( #49964, #27675 ),
 ( #43842, #89994 ),
 ( #82895, #3866 ),
 ( #58541, #98069 ),
 ( #73272, #28645 ),
 ( #51448, #65157 ),
 ( #97106, #82416 ),
 ( #59527, #96106 ),
 ( #26663, #57547 ),
 ( #88525, #19085 ),
 ( #73767, #11490 ),
 ( #42343, #58058 ),
 ( #89042, #20074 ),
 ( #19588, #81402 ),
 ( #11972, #42832 ),
 ( #35253, #66159 ),
 ( #50947, #7092 ),
 ( #21800, #37974 ),
 ( #61287, #52685 ),
 ( #45097, #6101 ),
 ( #13228, #66900 ),
 ( #13708, #21312 ),
 ( #99810, #84633 ),
 ( #97829, #83646 ) ),
 .UNSPECIFIED., .F., .F., .F.,
 ( 4, 3, 3, 3, 3, 3, 3, 3, 3, 3, 4 ),
 ( 2, 2 ),
 ( 0.000000000000000000, 0.1333490885032329043, 0.3007194338854308202, 0.4699862290245099827, 0.5844252810809248411, 0.6686540514502534727, 0.7354980260655189506, 0.8028463152565233907, 0.8633854507756654195, 0.9437142632666670750, 1.000000000000000000 ),
 ( 0.000000000000000000, 1.000000000000000000 ),
 .UNSPECIFIED. ) ;
#97752 = CARTESIAN_POINT ( 'NONE',  ( 118.1443815476567352, 229.0177522451417929, 5.000000000000051514 ) ) ;
#97753 = CARTESIAN_POINT ( 'NONE',  ( 82.41914487369291464, 41.31337197830497132, 3.340431838514237750 ) ) ;
#97754 = CARTESIAN_POINT ( 'NONE',  ( 96.65612621980318409, 236.6115022471902876, -5.000000000000047962 ) ) ;
#97755 = DIRECTION ( 'NONE',  ( 0.5000000000000014433, -0.8660254037844378194, 0.000000000000000000 ) ) ;
#97756 = CARTESIAN_POINT ( 'NONE',  ( 194.7041213697769422, 285.5929353680269855, -17.62016002267809256 ) ) ;
#97757 = ORIENTED_EDGE ( 'NONE', *, *, #9635, .T. ) ;
#97758 = CARTESIAN_POINT ( 'NONE',  ( 56.27743144475606130, 212.4869531367911009, 4.594050593750046652 ) ) ;
#97759 = ORIENTED_EDGE ( 'NONE', *, *, #27411, .F. ) ;
#97760 = CARTESIAN_POINT ( 'NONE',  ( 165.8605944207784262, 265.2106218463247274, 16.56633027260685864 ) ) ;
#97761 = CARTESIAN_POINT ( 'NONE',  ( 161.5266078408477597, 251.3399204103630211, 13.01505764280997468 ) ) ;
#97762 = CARTESIAN_POINT ( 'NONE',  ( 67.33503286408792121, 66.66970121028828089, -8.481744889717480973 ) ) ;
#97763 = ORIENTED_EDGE ( 'NONE', *, *, #35519, .T. ) ;
#97764 = CARTESIAN_POINT ( 'NONE',  ( -110.0000000000000000, 15.00000000000000000, 59.99999999999999289 ) ) ;
#97765 = CARTESIAN_POINT ( 'NONE',  ( 207.3062152119541679, 271.5820978585240368, 7.879821064966149535 ) ) ;
#97766 = CARTESIAN_POINT ( 'NONE',  ( 39.04508293989853485, 204.8967562850347122, -4.648177544792955347E-16 ) ) ;
#97767 = CARTESIAN_POINT ( 'NONE',  ( 32.78369927745970358, 30.87878583063843863, -9.188101187500006262 ) ) ;
#97768 = CARTESIAN_POINT ( 'NONE',  ( 189.5731351232621762, 264.7541819150383162, 10.55408932226666785 ) ) ;
#97769 = LINE ( 'NONE', #61728, #6869 ) ;
#97770 = CARTESIAN_POINT ( 'NONE',  ( 156.8993174718108605, 258.8894057963813680, 16.93179113901802069 ) ) ;
#97771 = ORIENTED_EDGE ( 'NONE', *, *, #40293, .F. ) ;
#97772 = B_SPLINE_CURVE_WITH_KNOTS ( 'NONE', 3,
 ( #19383, #33558, #49749, #35036, #96894, #33047, #27464, #94885, #10260, #56839 ),
 .UNSPECIFIED., .F., .F.,
 ( 4, 2, 2, 2, 4 ),
 ( 0.000000000000000000, 0.2500000000000000000, 0.5000000000000000000, 0.7500000000000000000, 1.000000000000000000 ),
 .UNSPECIFIED. ) ;
#97773 = CARTESIAN_POINT ( 'NONE',  ( 15.13723537722347956, 17.24335787977762280, -9.188101187500008038 ) ) ;
#97774 = FACE_OUTER_BOUND ( 'NONE', #43435, .T. ) ;
#97775 = CARTESIAN_POINT ( 'NONE',  ( 175.1307738592725798, 254.8361248832076740, 7.862726238744712326 ) ) ;
#97776 = CARTESIAN_POINT ( 'NONE',  ( 20.18734655506498754, 13.78380873178786459, -6.180339887498949025 ) ) ;
#97777 = ORIENTED_EDGE ( 'NONE', *, *, #69711, .F. ) ;
#97779 = EDGE_CURVE ( 'NONE', #19199, #82529, #99537, .T. ) ;
#97778 = CARTESIAN_POINT ( 'NONE',  ( 76.19322934838378103, 52.39361190095211640, 16.33354292047609491 ) ) ;
#97780 = CARTESIAN_POINT ( 'NONE',  ( 150.8359915840788688, 269.3913942967808453, 15.73449616766854575 ) ) ;
#97781 = CARTESIAN_POINT ( 'NONE',  ( 206.8659638600981623, 272.3446355680395641, -10.26115277030573125 ) ) ;
#97782 = EDGE_CURVE ( 'NONE', #81073, #75787, #22517, .T. ) ;
#97783 = ORIENTED_EDGE ( 'NONE', *, *, #1363, .T. ) ;
#97785 = CARTESIAN_POINT ( 'NONE',  ( 196.1245817477023650, 288.9492551302209336, 17.30641872853625074 ) ) ;
#97784 = CARTESIAN_POINT ( 'NONE',  ( 207.7666684749232786, 270.7845694125510931, -6.630926507062123498 ) ) ;
#97786 = CARTESIAN_POINT ( 'NONE',  ( 196.3174919959537306, 290.6151247789487684, -17.61248417473235151 ) ) ;
#97787 = ORIENTED_EDGE ( 'NONE', *, *, #12101, .F. ) ;
#97788 = EDGE_CURVE ( 'NONE', #7026, #85624, #80566, .T. ) ;
#97789 = CARTESIAN_POINT ( 'NONE',  ( 198.2040940955416488, 287.3474340887963763, 16.95806375232200480 ) ) ;
#97790 = DIRECTION ( 'NONE',  ( 0.4999999999999992784, -0.8660254037844390407, 0.000000000000000000 ) ) ;
#97791 = CARTESIAN_POINT ( 'NONE',  ( 77.77867966053455007, 61.43039905302717330, -16.12786080876373873 ) ) ;
#97792 = EDGE_CURVE ( 'NONE', #45532, #1725, #91456, .T. ) ;
#97793 = CARTESIAN_POINT ( 'NONE',  ( 124.1521724663614492, 251.6744531367911577, 4.594050593750047540 ) ) ;
#97794 = DIRECTION ( 'NONE',  ( -0.8660254037844387076, -0.4999999999999998890, -0.000000000000000000 ) ) ;
#97795 = ORIENTED_EDGE ( 'NONE', *, *, #42615, .T. ) ;
#97796 = CARTESIAN_POINT ( 'NONE',  ( 81.70640461168267166, 59.20467455214015473, -0.4951340343707861247 ) ) ;
#97797 = LINE ( 'NONE', #82633, #12239 ) ;
#97798 = CARTESIAN_POINT ( 'NONE',  ( 106.5950644350847369, 243.8967562850346837, -4.648177544792955347E-16 ) ) ;
#97799 = ORIENTED_EDGE ( 'NONE', *, *, #86527, .F. ) ;
#97800 = CARTESIAN_POINT ( 'NONE',  ( 166.2800977938260019, 260.3313707980180993, -16.91817955569885257 ) ) ;
#97801 = VERTEX_POINT ( 'NONE', #93454 ) ;
#97802 = ORIENTED_EDGE ( 'NONE', *, *, #22702, .F. ) ;
#97803 = CARTESIAN_POINT ( 'NONE',  ( 198.4706398937704819, 286.8857632237200619, 17.04020736381253798 ) ) ;
#97804 = DIRECTION ( 'NONE',  ( 0.000000000000000000, 0.000000000000000000, 1.000000000000000000 ) ) ;
#97805 = CARTESIAN_POINT ( 'NONE',  ( 83.61187889534991768, 209.8923013555409796, 4.594050593750050204 ) ) ;
#97806 = ORIENTED_EDGE ( 'NONE', *, *, #23137, .T. ) ;
#97807 = CARTESIAN_POINT ( 'NONE',  ( 24.61363793893735874, 175.0177522451417929, 5.000000000000051514 ) ) ;
#97808 = CARTESIAN_POINT ( 'NONE',  ( 179.7389585068036979, 283.2694176073634935, 16.15404047216739514 ) ) ;
#97809 = CARTESIAN_POINT ( 'NONE',  ( 150.3996455637841621, 270.1471677736116703, 15.13740740754872327 ) ) ;
#97810 = CARTESIAN_POINT ( 'NONE',  ( -16.43235775771475105, 167.9865022471903160, -10.00000000000009592 ) ) ;
#97811 = ORIENTED_EDGE ( 'NONE', *, *, #13609, .F. ) ;
#97812 = AXIS2_PLACEMENT_3D ( 'NONE', #23795, #71920, #61791 ) ;
#97813 = CARTESIAN_POINT ( 'NONE',  ( 70.74807497663788070, 64.07295471535329057, -12.85902237599238163 ) ) ;
#97814 = CARTESIAN_POINT ( 'NONE',  ( 153.3939648708017387, 264.9608545997728015, -16.49556533540763681 ) ) ;
#97815 = B_SPLINE_SURFACE_WITH_KNOTS ( 'NONE', 3, 1, ( 
 ( #8180, #60851 ),
 ( #38052, #7675 ),
 ( #53754, #78086 ),
 ( #38560, #30967 ),
 ( #61856, #23358 ),
 ( #29974, #85216 ),
 ( #15761, #91815 ),
 ( #93306, #62351 ),
 ( #23863, #54754 ),
 ( #53273, #85741 ),
 ( #39545, #47162 ),
 ( #21874, #83722 ),
 ( #70467, #91314 ),
 ( #14279, #84227 ),
 ( #14774, #76581 ),
 ( #45171, #49667 ),
 ( #26383, #80623 ),
 ( #24868, #25370 ),
 ( #70992, #17270 ),
 ( #62862, #79623 ),
 ( #86733, #64376 ),
 ( #56768, #80121 ),
 ( #40052, #87254 ),
 ( #71988, #48173 ),
 ( #2593, #95338 ),
 ( #1596, #2087 ),
 ( #33479, #32965 ),
 ( #93819, #10186 ),
 ( #10683, #3111 ),
 ( #55250, #33999 ),
 ( #17788, #32479 ),
 ( #71494, #41561 ),
 ( #63375, #48688 ),
 ( #41052, #25896 ) ),
 .UNSPECIFIED., .T., .F., .F.,
 ( 4, 2, 2, 2, 2, 2, 2, 2, 2, 2, 2, 2, 2, 2, 2, 2, 4 ),
 ( 2, 2 ),
 ( 0.000000000000000000, 0.06250000000000000000, 0.1250000000000000000, 0.1875000000000000000, 0.2500000000000000000, 0.3125000000000000000, 0.3750000000000000000, 0.4375000000000000000, 0.5000000000000000000, 0.5625000000000000000, 0.6250000000000000000, 0.6875000000000000000, 0.7500000000000000000, 0.8125000000000000000, 0.8750000000000000000, 0.9375000000000000000, 1.000000000000000000 ),
 ( 0.000000000000000000, 1.000000000000000000 ),
 .UNSPECIFIED. ) ;
#97816 = CARTESIAN_POINT ( 'NONE',  ( -72.92390943388483038, 47.25396573843040926, -10.00000000000000000 ) ) ;
#97817 = ORIENTED_EDGE ( 'NONE', *, *, #85842, .F. ) ;
#97818 = DIRECTION ( 'NONE',  ( -0.9172102815913020235, -0.3984034379158949979, 0.000000000000000000 ) ) ;
#97819 = CARTESIAN_POINT ( 'NONE',  ( 76.06543009505163866, 51.20229643674512232, -16.10824878130317117 ) ) ;
#97820 = DIRECTION ( 'NONE',  ( -0.4831861483251571054, -0.8755176446347036068, 0.000000000000000000 ) ) ;
#97821 = CARTESIAN_POINT ( 'NONE',  ( 50.00170217996129907, 86.12209509027381671, -10.00000000000000000 ) ) ;
#97822 = CARTESIAN_POINT ( 'NONE',  ( 49.19475937879462890, 79.05079877653317055, -10.00000000000000000 ) ) ;
#97823 = CARTESIAN_POINT ( 'NONE',  ( 196.1197415632541379, 279.6791495332669797, 16.37442619035736158 ) ) ;
#97824 = LINE ( 'NONE', #34995, #94999 ) ;
#97825 = CARTESIAN_POINT ( 'NONE',  ( 130.8910194135003735, 252.5024278399160949, 9.188101187500095079 ) ) ;
#97826 = ORIENTED_EDGE ( 'NONE', *, *, #91500, .F. ) ;
#97827 = CARTESIAN_POINT ( 'NONE',  ( 148.6500818154487433, 275.1775010768142238, 7.719411301773694944 ) ) ;
#97828 = CARTESIAN_POINT ( 'NONE',  ( 69.30885647817778761, 67.84364059337893593, -9.314741131470263724 ) ) ;
#97829 = CARTESIAN_POINT ( 'NONE',  ( 87.98594423550160570, 43.75089820288620501, -2.253463800273097561 ) ) ;
#97830 = CARTESIAN_POINT ( 'NONE',  ( 203.5517807763935991, 276.4131063546051337, 14.32831804246049678 ) ) ;
#97831 = CARTESIAN_POINT ( 'NONE',  ( 153.2819058590468160, 274.2512448977743134, -12.24885634829186287 ) ) ;
#97832 = FACE_OUTER_BOUND ( 'NONE', #43454, .T. ) ;
#97833 = ORIENTED_EDGE ( 'NONE', *, *, #53336, .F. ) ;
#97834 = CARTESIAN_POINT ( 'NONE',  ( 76.32480335349765710, 53.80613752448550713, 16.04086341519817793 ) ) ;
#97835 =( BOUNDED_CURVE ( )  B_SPLINE_CURVE ( 2, ( #50807, #96970, #81265, #36100, #81757, #89856, #12842, #97928, #28503 ),
 .UNSPECIFIED., .F., .T. ) 
 B_SPLINE_CURVE_WITH_KNOTS ( ( 3, 2, 2, 2, 3 ),
 ( 0.2943548387096774355, 0.2956989247311828106, 0.2983870967741935609, 0.3010752688172043112, 0.3024193548387096864 ),
 .UNSPECIFIED. ) 
 CURVE ( )  GEOMETRIC_REPRESENTATION_ITEM ( )  RATIONAL_B_SPLINE_CURVE ( ( 0.9330127018922194093, 0.9330127018922194093, 1.000000000000000000, 0.8660254037844387076, 1.000000000000000000, 0.8660254037844387076, 1.000000000000000000, 0.9330127018922194093, 0.9330127018922194093 ) ) 
 REPRESENTATION_ITEM ( '' )  );
#97836 = CARTESIAN_POINT ( 'NONE',  ( 185.5156133380430390, 277.7268379766968565, -17.03516142629836594 ) ) ;
#97837 = CARTESIAN_POINT ( 'NONE',  ( 72.54662768515015614, 71.52720332855409424, -5.424102431521803602 ) ) ;
#97838 = CARTESIAN_POINT ( 'NONE',  ( 205.9281787291064347, 273.9689270615001533, -10.62323193457751458 ) ) ;
#97839 = CARTESIAN_POINT ( 'NONE',  ( 202.6577094508454024, 267.5156926251955838, 0.8710555158424478917 ) ) ;
#97840 = EDGE_CURVE ( 'NONE', #312, #8895, #8321, .T. ) ;
#97841 = FACE_OUTER_BOUND ( 'NONE', #98166, .T. ) ;
#97842 = CARTESIAN_POINT ( 'NONE',  ( 70.17655873119920784, 71.02233810139671277, 2.012687245299938255 ) ) ;
#97843 = EDGE_CURVE ( 'NONE', #5537, #32075, #28670, .T. ) ;
#97844 = CARTESIAN_POINT ( 'NONE',  ( 80.01979875032591849, 57.54866692369599690, 16.59896302490740538 ) ) ;
#97845 = CARTESIAN_POINT ( 'NONE',  ( 19.38736881444313198, 23.14441083166260782, 10.00000000000000533 ) ) ;
#97846 = CARTESIAN_POINT ( 'NONE',  ( 148.9266665119372703, 272.6984423298952152, 12.06339424062075061 ) ) ;
#97847 = DIRECTION ( 'NONE',  ( -0.8660254037844387076, -0.4999999999999998890, -0.000000000000000000 ) ) ;
#97848 = CARTESIAN_POINT ( 'NONE',  ( 19.18375657693640335, 36.32959363016014720, -10.00000000000000000 ) ) ;
#97849 = CARTESIAN_POINT ( 'NONE',  ( 159.3169041484411537, 254.7020228407560580, 16.67170756419672628 ) ) ;
#97850 = CARTESIAN_POINT ( 'NONE',  ( 193.6523268064705974, 293.2313262976975352, 15.26490498002906193 ) ) ;
#97851 = CARTESIAN_POINT ( 'NONE',  ( 137.2691092145631160, 243.3927522451418213, 10.00000000000009592 ) ) ;
#97852 = DIRECTION ( 'NONE',  ( -0.9805290675673918876, -0.1963739994383708332, 0.000000000000000000 ) ) ;
#97853 = VERTEX_POINT ( 'NONE', #26529 ) ;
#97854 = EDGE_CURVE ( 'NONE', #88861, #94383, #68640, .T. ) ;
#97855 = CARTESIAN_POINT ( 'NONE',  ( 178.0315741628076012, 287.5935043698759728, -13.06113257055532451 ) ) ;
#97856 = CARTESIAN_POINT ( 'NONE',  ( 198.4522155198218059, 286.9176751754968109, -17.57438352224490075 ) ) ;
#97857 = CARTESIAN_POINT ( 'NONE',  ( 4.992576338337582520, 179.8149278399160949, -9.188101187500095079 ) ) ;
#97858 = CARTESIAN_POINT ( 'NONE',  ( 175.6766631755835419, 257.0359803582177847, -10.59688122334902793 ) ) ;
#97859 = CARTESIAN_POINT ( 'NONE',  ( 18.71323094475359738, 33.73705186507753950, -3.090169943749475845 ) ) ;
#97860 = CARTESIAN_POINT ( 'NONE',  ( 85.41398746878978443, 48.60267188261818916, 12.47190137721841019 ) ) ;
#97861 = CARTESIAN_POINT ( 'NONE',  ( -22.42236680055709641, 157.8615022471902591, 0.000000000000000000 ) ) ;
#97862 = DIRECTION ( 'NONE',  ( -1.000000000000000000, 0.000000000000000000, 0.000000000000000000 ) ) ;
#97863 = CARTESIAN_POINT ( 'NONE',  ( 150.1195797453556793, 276.5050416553082755, 3.721351720276065755 ) ) ;
#97865 = CARTESIAN_POINT ( 'NONE',  ( 70.58515312316129098, 204.8927522451418213, -10.00000000000009059 ) ) ;
#97864 = CARTESIAN_POINT ( 'NONE',  ( 171.3734714223081426, 258.1936803860005512, 14.40034214095746989 ) ) ;
#97866 = CARTESIAN_POINT ( 'NONE',  ( 173.2798715285074991, 281.8114527337138497, 15.08241540710736750 ) ) ;
#97867 = CARTESIAN_POINT ( 'NONE',  ( 198.0827002274358222, 287.5576944360828975, 17.17879237213074006 ) ) ;
#97868 = VECTOR ( 'NONE', #49221, 1000.000000000000000 ) ;
#97869 = CARTESIAN_POINT ( 'NONE',  ( 53.71569994882479193, 208.4865022471902876, -10.00000000000009415 ) ) ;
#97870 = CARTESIAN_POINT ( 'NONE',  ( 181.8674585300132378, 291.6431133160953664, 9.312409377393402465 ) ) ;
#97871 = CARTESIAN_POINT ( 'NONE',  ( 189.9052851100924215, 301.7213928939034986, -1.077181946533001256 ) ) ;
#97872 = CARTESIAN_POINT ( 'NONE',  ( 13.92363686274711299, 178.8458772461660544, 9.188101187500095079 ) ) ;
#97873 = CARTESIAN_POINT ( 'NONE',  ( 168.2127584262427149, 286.2670693736010890, 4.111954200343466148 ) ) ;
#97874 = CARTESIAN_POINT ( 'NONE',  ( 5.218277336896219865, 180.4865022471903160, 10.00000000000009415 ) ) ;
#97875 = CARTESIAN_POINT ( 'NONE',  ( 40.03666203415436797, 35.06628583063844928, -9.188101187500006262 ) ) ;
#97876 = CARTESIAN_POINT ( 'NONE',  ( 201.6018788519649831, 280.5407822744489863, -16.29061894498408947 ) ) ;
#97877 = VECTOR ( 'NONE', #38028, 1000.000000000000000 ) ;
#97878 = CARTESIAN_POINT ( 'NONE',  ( 180.9785907350442926, 277.5730618892402504, 16.35545640519342925 ) ) ;
#97879 = CARTESIAN_POINT ( 'NONE',  ( 16.77867774916664345, 33.18528772668517490, -1.583844403245363575 ) ) ;
#97880 = CARTESIAN_POINT ( 'NONE',  ( 153.4409967745565666, 266.3578157004054106, -16.49295564300695460 ) ) ;
#97881 = CARTESIAN_POINT ( 'NONE',  ( 176.4956094263426110, 260.4465060475594100, -13.34520323348970194 ) ) ;
#97882 = DIRECTION ( 'NONE',  ( 1.000000000000000000, 0.000000000000000000, 0.000000000000000000 ) ) ;
#97883 = CARTESIAN_POINT ( 'NONE',  ( 10.08301516415377641, 26.79752408145591147, -5.678558825948271327 ) ) ;
#97884 = CARTESIAN_POINT ( 'NONE',  ( 165.6285009359904734, 285.3942701294749327, 0.4263846489270779472 ) ) ;
#97885 = CARTESIAN_POINT ( 'NONE',  ( -22.42236680055709641, 157.8615022471902591, 0.000000000000000000 ) ) ;
#97886 = CARTESIAN_POINT ( 'NONE',  ( 159.1005818787057819, 259.4300168470162475, 16.69242165874631567 ) ) ;
#97887 = CARTESIAN_POINT ( 'NONE',  ( 193.9401685343300699, 294.7327698005063326, 14.01047396938887069 ) ) ;
#97888 = ORIENTED_EDGE ( 'NONE', *, *, #33579, .F. ) ;
#97889 = CARTESIAN_POINT ( 'NONE',  ( 87.27161142932803273, 45.46653660222711579, -7.106486493650752578 ) ) ;
#97890 = CARTESIAN_POINT ( 'NONE',  ( 156.5356202806696615, 276.3685272183531083, 10.26723329993582112 ) ) ;
#97891 = CARTESIAN_POINT ( 'NONE',  ( 206.6703863510205679, 272.6833857505801006, -10.72500664779635393 ) ) ;
#97892 = VERTEX_POINT ( 'NONE', #33115 ) ;
#97893 = DIRECTION ( 'NONE',  ( -0.000000000000000000, 1.000000000000000000, -0.000000000000000000 ) ) ;
#97894 = CARTESIAN_POINT ( 'NONE',  ( 67.05462070971094590, 69.20977875835498594, 1.581595143886974197 ) ) ;
#97895 = LINE ( 'NONE', #51267, #21813 ) ;
#97896 = CARTESIAN_POINT ( 'NONE',  ( 155.6535436963908694, 261.0471492701456668, -17.87366571046205976 ) ) ;
#97897 = ORIENTED_EDGE ( 'NONE', *, *, #10351, .T. ) ;
#97898 = ORIENTED_EDGE ( 'NONE', *, *, #64448, .F. ) ;
#97900 = CARTESIAN_POINT ( 'NONE',  ( 164.3853877993040840, 245.9231516401292197, 5.995325337583643943 ) ) ;
#97899 = DIRECTION ( 'NONE',  ( 4.546899780356472071E-16, -9.093799560712944142E-16, 1.000000000000000000 ) ) ;
#97901 = CARTESIAN_POINT ( 'NONE',  ( 192.8325075361489382, 296.6512949269187516, 11.74553025762331515 ) ) ;
#97902 = ORIENTED_EDGE ( 'NONE', *, *, #58991, .T. ) ;
#97903 = CARTESIAN_POINT ( 'NONE',  ( 150.6453220160077251, 269.7216436761371483, 14.94145576020818034 ) ) ;
#97904 = CARTESIAN_POINT ( 'NONE',  ( 80.16500549515171770, 58.13051307499745235, 16.26618726186349306 ) ) ;
#97905 = FACE_OUTER_BOUND ( 'NONE', #57388, .T. ) ;
#97906 = VERTEX_POINT ( 'NONE', #16906 ) ;
#97908 = EDGE_CURVE ( 'NONE', #13677, #99877, #2739, .T. ) ;
#97907 = FACE_OUTER_BOUND ( 'NONE', #49880, .T. ) ;
#97909 = AXIS2_PLACEMENT_3D ( 'NONE', #96547, #66103, #5795 ) ;
#97910 = ORIENTED_EDGE ( 'NONE', *, *, #92628, .T. ) ;
#97911 = CARTESIAN_POINT ( 'NONE',  ( 165.0087721269838710, 244.8434183119457543, 2.604344609212914108 ) ) ;
#97912 = CARTESIAN_POINT ( 'NONE',  ( 73.78990874245801024, 60.11125809112680685, 15.42103814799846795 ) ) ;
#97913 = ORIENTED_EDGE ( 'NONE', *, *, #7315, .T. ) ;
#97914 = CARTESIAN_POINT ( 'NONE',  ( 174.8404000400799703, 277.4648157049296628, -15.64849645087200791 ) ) ;
#97915 = CYLINDRICAL_SURFACE ( 'NONE', #2978, 10.00000000000010658 ) ;
#97916 = ORIENTED_EDGE ( 'NONE', *, *, #66147, .T. ) ;
#97917 = CARTESIAN_POINT ( 'NONE',  ( 75.41814989884494480, 225.8967562850346837, -4.648177544792955347E-16 ) ) ;
#97918 = CARTESIAN_POINT ( 'NONE',  ( 147.5381343315788172, 275.1034506142203782, -4.056595942992749393 ) ) ;
#97919 = ORIENTED_EDGE ( 'NONE', *, *, #80206, .T. ) ;
#97920 = CARTESIAN_POINT ( 'NONE',  ( 157.0239713899953244, 269.7369771206523978, 16.31777668093047851 ) ) ;
#97921 = ORIENTED_EDGE ( 'NONE', *, *, #59683, .F. ) ;
#97922 = CARTESIAN_POINT ( 'NONE',  ( 156.2277803658613777, 266.3225699999913445, -16.24938540415413613 ) ) ;
#97923 = CARTESIAN_POINT ( 'NONE',  ( 168.8785100482814698, 272.6966330010931756, 17.41127854651366391 ) ) ;
#97924 = CARTESIAN_POINT ( 'NONE',  ( 147.4811722709131914, 275.2021117973970377, 3.890385073228495916 ) ) ;
#97925 = CARTESIAN_POINT ( 'NONE',  ( 82.95708619573620979, 53.58516627418448053, 15.69712586674409671 ) ) ;
#97926 = CARTESIAN_POINT ( 'NONE',  ( -19.65312891409030271, 93.06504152958497400, -10.00000000000000888 ) ) ;
#97927 = CARTESIAN_POINT ( 'NONE',  ( 192.5712965840290849, 297.1037255674836501, 11.03742858512898906 ) ) ;
#97928 = CARTESIAN_POINT ( 'NONE',  ( 39.83579079637758014, 182.2592609112380160, 2.679491924311254714 ) ) ;
#97929 = CARTESIAN_POINT ( 'NONE',  ( 191.0702043019150835, 299.7036936669546776, -8.800021049343948576 ) ) ;
#97930 = ORIENTED_EDGE ( 'NONE', *, *, #19483, .F. ) ;
#97931 = CARTESIAN_POINT ( 'NONE',  ( 80.66320740626021291, 55.52576771489578533, -16.04266746477125949 ) ) ;
#97932 = B_SPLINE_CURVE_WITH_KNOTS ( 'NONE', 3,
 ( #62621, #68737, #32236, #61628 ),
 .UNSPECIFIED., .F., .F.,
 ( 4, 4 ),
 ( 0.008172245353423012934, 0.01420657290482196973 ),
 .UNSPECIFIED. ) ;
#97933 = CARTESIAN_POINT ( 'NONE',  ( 35.24645901769773815, 32.30066082961424456, -10.00000000000000533 ) ) ;
#97935 = DIRECTION ( 'NONE',  ( -0.2776767122488493222, -0.9606745773021527768, 0.000000000000000000 ) ) ;
#97934 = CARTESIAN_POINT ( 'NONE',  ( 149.4171629335945681, 271.8488776066536730, -11.42564036194071520 ) ) ;
#97937 = ORIENTED_EDGE ( 'NONE', *, *, #20259, .F. ) ;
#97936 = CARTESIAN_POINT ( 'NONE',  ( 198.6755293322981117, 286.5308843062557571, 17.86676876308990103 ) ) ;
#97938 = LINE ( 'NONE', #14806, #17548 ) ;
#97939 = CARTESIAN_POINT ( 'NONE',  ( 51.48077938449444702, 188.9824982072973967, 3.021315404115420679E-15 ) ) ;
#97940 = ORIENTED_EDGE ( 'NONE', *, *, #98038, .F. ) ;
#97941 = CARTESIAN_POINT ( 'NONE',  ( 149.5090996232239036, 271.6896385891362797, -11.55286514765376005 ) ) ;
#97942 = CARTESIAN_POINT ( 'NONE',  ( 72.42456163296586169, 70.48275826165811964, 7.406847684272648280 ) ) ;
#97943 = CARTESIAN_POINT ( 'NONE',  ( 86.16814719413950741, 44.54916269947106144, 7.429840375059775681 ) ) ;
#97944 = DIRECTION ( 'NONE',  ( 0.2774202615135334393, -0.9607486656258038549, 0.000000000000000000 ) ) ;
#97945 = VECTOR ( 'NONE', #42195, 1000.000000000000000 ) ;
#97946 = CARTESIAN_POINT ( 'NONE',  ( 160.1964060607056979, 253.1786808433599845, -14.64952422815191113 ) ) ;
#97947 = CARTESIAN_POINT ( 'NONE',  ( 148.0419010042100751, 274.2309011420633169, -10.20829995470312568 ) ) ;
#97948 = VERTEX_POINT ( 'NONE', #10826 ) ;
#97949 = CARTESIAN_POINT ( 'NONE',  ( 170.1313062173066726, 255.2739091071986479, -11.62815245866028313 ) ) ;
#97950 = CARTESIAN_POINT ( 'NONE',  ( 85.56881463994550074, 46.99119872501016459, 11.02191848255706219 ) ) ;
#97951 = CARTESIAN_POINT ( 'NONE',  ( 153.4495116231415750, 264.8646448025247082, -16.73555355292144498 ) ) ;
#97952 = CARTESIAN_POINT ( 'NONE',  ( 206.9258336080761183, 272.2409381227055292, 6.776000910836894597 ) ) ;
#97953 = CARTESIAN_POINT ( 'NONE',  ( 30.67581576542834654, 198.5177522451419350, 5.000000000000046185 ) ) ;
#97954 = CARTESIAN_POINT ( 'NONE',  ( 117.0885659928033817, 250.6589784336661069, -6.496448406907676862E-16 ) ) ;
#97955 = CARTESIAN_POINT ( 'NONE',  ( 180.8000599349354900, 294.0875826803771247, -2.709611528315936102 ) ) ;
#97956 = CARTESIAN_POINT ( 'NONE',  ( 167.7145385494464165, 281.8102352406253317, -10.91421457602037925 ) ) ;
#97957 = CARTESIAN_POINT ( 'NONE',  ( 208.3379394461497895, 269.7950990654974817, 2.541397148058371691 ) ) ;
#97958 = ADVANCED_FACE ( 'NONE', ( #85884 ), #87403, .T. ) ;
#97959 = DIRECTION ( 'NONE',  ( 0.3940053768033583426, -0.6824373310787393843, 0.6156614753256619554 ) ) ;
#97960 = B_SPLINE_CURVE_WITH_KNOTS ( 'NONE', 3,
 ( #84483, #45431, #37827, #59631 ),
 .UNSPECIFIED., .F., .F.,
 ( 4, 4 ),
 ( 0.002796930759027657122, 0.003029742318773366843 ),
 .UNSPECIFIED. ) ;
#97961 = EDGE_LOOP ( 'NONE', ( #56633, #39528, #28856, #41702 ) ) ;
#97962 = CARTESIAN_POINT ( 'NONE',  ( 7.365298646897277202, 168.3927522451418213, 10.00000000000009948 ) ) ;
#97963 = CARTESIAN_POINT ( 'NONE',  ( 180.5010753389648812, 267.3347324538273710, 15.01776452798817374 ) ) ;
#97964 = CARTESIAN_POINT ( 'NONE',  ( 71.40111858386666199, 71.76360913945114817, -2.046226491198976039 ) ) ;
#97965 = CARTESIAN_POINT ( 'NONE',  ( 82.04258323635852435, 41.40673436471046642, -5.930946022421568209 ) ) ;
#97966 = EDGE_CURVE ( 'NONE', #59762, #6045, #5701, .T. ) ;
#97967 = CARTESIAN_POINT ( 'NONE',  ( 207.1007598919583472, 271.9379569114424271, -6.086525981869248092 ) ) ;
#97968 = CARTESIAN_POINT ( 'NONE',  ( 59.82969263072505584, 216.8967562850347122, -4.648177544792955347E-16 ) ) ;
#97969 = DIRECTION ( 'NONE',  ( -0.9738769792773346312, -0.2270762630343691746, 0.000000000000000000 ) ) ;
#97970 = CARTESIAN_POINT ( 'NONE',  ( 99.95784806818352308, 218.5177522451417929, 5.000000000000051514 ) ) ;
#97971 = EDGE_LOOP ( 'NONE', ( #88392, #19758, #56778 ) ) ;
#97972 = ADVANCED_FACE ( 'NONE', ( #32101 ), #10329, .T. ) ;
#97973 = CARTESIAN_POINT ( 'NONE',  ( 73.43762515466688967, 73.52662068827324049, 2.033788753608857291E-15 ) ) ;
#97974 = CARTESIAN_POINT ( 'NONE',  ( 162.6774150396764469, 248.8814472377480911, 10.88033986792731689 ) ) ;
#97975 = CARTESIAN_POINT ( 'NONE',  ( 162.7007457333762090, 248.8410372908842021, -10.94671474643812914 ) ) ;
#97976 = AXIS2_PLACEMENT_3D ( 'NONE', #76611, #54795, #77100 ) ;
#97977 = CARTESIAN_POINT ( 'NONE',  ( 6.454167755106333892, 174.5333772461660828, 9.188101187500095079 ) ) ;
#97978 = CARTESIAN_POINT ( 'NONE',  ( 14.08999532346373407, 7.944730856513903205, 1.475505719884397138E-15 ) ) ;
#97979 = CARTESIAN_POINT ( 'NONE',  ( 79.05889743344327769, 46.07589703579929363, -12.67661131050572720 ) ) ;
#97980 = CARTESIAN_POINT ( 'NONE',  ( 71.48056072480412126, 59.16358519354559320, -15.78944119181872452 ) ) ;
#97981 = CARTESIAN_POINT ( 'NONE',  ( 73.46727755934470849, 69.83818549023170874, 9.221945012360034610 ) ) ;
#97982 = CARTESIAN_POINT ( 'NONE',  ( 53.97765888354242492, 189.7202760586659736, -5.415160957724236172E-17 ) ) ;
#97983 = CARTESIAN_POINT ( 'NONE',  ( 164.4405316900629259, 245.8276396196081350, -6.144538123479245328 ) ) ;
#97984 = CARTESIAN_POINT ( 'NONE',  ( 203.7313627084707832, 276.2715032248725038, 13.33488798586162360 ) ) ;
#97985 = CARTESIAN_POINT ( 'NONE',  ( 71.36111289249075185, 71.40279321753016006, 3.762213664179777428 ) ) ;
#97986 = CARTESIAN_POINT ( 'NONE',  ( 66.32789846179778692, 68.06826338654373387, -4.695580419454262966 ) ) ;
#97987 = ORIENTED_EDGE ( 'NONE', *, *, #53326, .F. ) ;
#97988 = VECTOR ( 'NONE', #68009, 1000.000000000000227 ) ;
#97989 = CARTESIAN_POINT ( 'NONE',  ( 14.74455677852503932, 185.9865022471903444, -10.00000000000009415 ) ) ;
#97990 = FACE_OUTER_BOUND ( 'NONE', #8670, .T. ) ;
#97991 = CARTESIAN_POINT ( 'NONE',  ( 130.0249940097159254, 252.0024278399160949, -9.188101187500093303 ) ) ;
#97992 = CARTESIAN_POINT ( 'NONE',  ( 26.97531487256933858, 21.28920272979927830, -7.433330006724141015 ) ) ;
#97993 = CARTESIAN_POINT ( 'NONE',  ( 77.71695824120645568, 49.45779813244274692, 15.33409790704233977 ) ) ;
#97994 = CARTESIAN_POINT ( 'NONE',  ( 83.75130605492059033, 51.70531176359354220, -14.84358514963803977 ) ) ;
#97995 = PLANE ( 'NONE',  #86966 ) ;
#97997 = CARTESIAN_POINT ( 'NONE',  ( 189.4804681487932783, 289.7638976020832047, 15.63394399629991582 ) ) ;
#97996 = CARTESIAN_POINT ( 'NONE',  ( 196.0034224882197975, 291.1591091234520263, 17.53794140922627776 ) ) ;
#97998 = CARTESIAN_POINT ( 'NONE',  ( 69.12867519028084473, 64.30014342229272017, 12.00737124844781967 ) ) ;
#97999 = ORIENTED_EDGE ( 'NONE', *, *, #26832, .F. ) ;
#98000 = CARTESIAN_POINT ( 'NONE',  ( 190.8604783348975502, 300.0669496974951471, 7.597731640149610222 ) ) ;
#98001 = CARTESIAN_POINT ( 'NONE',  ( -51.75017079496729622, 30.85748650210271293, -10.00000000000000000 ) ) ;
#98002 = CARTESIAN_POINT ( 'NONE',  ( 151.6041069312964567, 268.5621543234237834, -14.59499063436561528 ) ) ;
#98003 = CARTESIAN_POINT ( 'NONE',  ( 173.0384568215392562, 268.2350346299093644, -16.30935032955606445 ) ) ;
#98004 = CARTESIAN_POINT ( 'NONE',  ( 193.8643712729062543, 270.7948579697045943, -13.84106480611635526 ) ) ;
#98005 = VERTEX_POINT ( 'NONE', #78730 ) ;
#98006 = CARTESIAN_POINT ( 'NONE',  ( 71.23450976540344470, 70.68244710050896629, 5.511218535461621215 ) ) ;
#98007 = DIRECTION ( 'NONE',  ( -0.8660254037844382635, -0.5000000000000005551, 0.000000000000000000 ) ) ;
#98008 = VECTOR ( 'NONE', #68702, 1000.000000000000000 ) ;
#98009 = EDGE_CURVE ( 'NONE', #89564, #39796, #7172, .T. ) ;
#98010 = CARTESIAN_POINT ( 'NONE',  ( 85.30253499385175076, 44.82337869870082159, 7.816767979061977734 ) ) ;
#98011 = CARTESIAN_POINT ( 'NONE',  ( 196.1975761016102808, 270.9518507311354369, 12.17928950200870020 ) ) ;
#98012 = VECTOR ( 'NONE', #37614, 1000.000000000000000 ) ;
#98013 = CARTESIAN_POINT ( 'NONE',  ( 185.7675376949824795, 296.6512829522437187, 4.668071064500018963 ) ) ;
#98014 = CARTESIAN_POINT ( 'NONE',  ( 140.3182403272686258, 258.4865022471902876, 10.00000000000009415 ) ) ;
#98015 = FACE_OUTER_BOUND ( 'NONE', #60339, .T. ) ;
#98016 = CARTESIAN_POINT ( 'NONE',  ( 153.2583947049096764, 265.1956690150883560, -17.64103123457563882 ) ) ;
#98017 = EDGE_CURVE ( 'NONE', #79399, #86304, #64931, .T. ) ;
#98018 = LINE ( 'NONE', #50401, #84268 ) ;
#98019 = CARTESIAN_POINT ( 'NONE',  ( 17.31863740857695078, 12.12755873383625271, -6.180339887498949025 ) ) ;
#98020 = CARTESIAN_POINT ( 'NONE',  ( -20.51833308425736391, 22.81063138990083061, -10.00000000000000000 ) ) ;
#98021 = VERTEX_POINT ( 'NONE', #40193 ) ;
#98022 = DIRECTION ( 'NONE',  ( -5.963328051300290638E-15, 1.097929109219269329E-14, -1.000000000000000000 ) ) ;
#98023 = CARTESIAN_POINT ( 'NONE',  ( -59.85755863633952600, 35.44530052843370527, -10.00000000000000000 ) ) ;
#98024 = CARTESIAN_POINT ( 'NONE',  ( 9.830230629461709668, 30.95267373526312227, -10.00000000000000000 ) ) ;
#98025 = VERTEX_POINT ( 'NONE', #71135 ) ;
#98027 = EDGE_CURVE ( 'NONE', #77732, #53564, #22567, .T. ) ;
#98026 = CARTESIAN_POINT ( 'NONE',  ( 161.5631100156346633, 265.8146362027571854, -17.76550717985403693 ) ) ;
#98028 = CARTESIAN_POINT ( 'NONE',  ( 204.6941148245495583, 272.9778480757090620, -9.756815831893453250 ) ) ;
#98029 = CARTESIAN_POINT ( 'NONE',  ( 204.2799274532736433, 276.8237820148827950, 13.55359442435934803 ) ) ;
#98030 = CARTESIAN_POINT ( 'NONE',  ( -14.06329310883398875, 23.28858607597029007, -10.00000000000000000 ) ) ;
#98031 = ORIENTED_EDGE ( 'NONE', *, *, #27670, .F. ) ;
#98032 = CARTESIAN_POINT ( 'NONE',  ( 88.13136219740870558, 215.5643266524159856, -9.188101187500093303 ) ) ;
#98033 = CARTESIAN_POINT ( 'NONE',  ( 203.0984285455635074, 278.8701981521235211, 16.46020897279243300 ) ) ;
#98034 = CARTESIAN_POINT ( 'NONE',  ( 179.1756939090309402, 269.5685363826416960, -17.30465729557930388 ) ) ;
#98035 = CARTESIAN_POINT ( 'NONE',  ( -22.42236680055709641, 157.8615022471902591, 0.000000000000000000 ) ) ;
#98036 = EDGE_CURVE ( 'NONE', #77716, #77081, #5595, .T. ) ;
#98037 = ORIENTED_EDGE ( 'NONE', *, *, #303, .F. ) ;
#98038 = EDGE_CURVE ( 'NONE', #20654, #26223, #37096, .T. ) ;
#98039 = CARTESIAN_POINT ( 'NONE',  ( -14.26183375581750568, 174.1199935810940644, 2.679491924311255158 ) ) ;
#98040 = ORIENTED_EDGE ( 'NONE', *, *, #82849, .F. ) ;
#98041 = DIRECTION ( 'NONE',  ( 0.000000000000000000, 0.000000000000000000, -1.000000000000000000 ) ) ;
#98042 = EDGE_LOOP ( 'NONE', ( #44647, #18579 ) ) ;
#98043 = CARTESIAN_POINT ( 'NONE',  ( 75.78736691889224630, 62.67330692550549287, 15.04515854727457480 ) ) ;
#98044 = CARTESIAN_POINT ( 'NONE',  ( 155.5211745099813356, 261.2764194263634749, -17.18163098020766810 ) ) ;
#98045 = ORIENTED_EDGE ( 'NONE', *, *, #74575, .T. ) ;
#98046 = CARTESIAN_POINT ( 'NONE',  ( 182.8487395599695731, 279.9155653989188295, -17.44888926691034925 ) ) ;
#98047 = CARTESIAN_POINT ( 'NONE',  ( 82.65509249134085223, 40.87170141247805333, 3.272232117641559856 ) ) ;
#98048 = CYLINDRICAL_SURFACE ( 'NONE', #46237, 10.00000000000010658 ) ;
#98049 = CARTESIAN_POINT ( 'NONE',  ( -23.57959705543464324, 99.68515928958061068, 45.19939659820781230 ) ) ;
#98050 = CARTESIAN_POINT ( 'NONE',  ( 25.69932979004302709, 23.03677371833802567, 10.00000000000000533 ) ) ;
#98051 = CARTESIAN_POINT ( 'NONE',  ( 156.9594519734722269, 258.7852497842161483, -18.40072354977459312 ) ) ;
#98052 = ORIENTED_EDGE ( 'NONE', *, *, #69067, .F. ) ;
#98054 = CARTESIAN_POINT ( 'NONE',  ( 76.65905396365022284, 59.59921405739184763, 15.92423336072870299 ) ) ;
#98053 = B_SPLINE_CURVE_WITH_KNOTS ( 'NONE', 3,
 ( #72282, #63654, #94593, #25147 ),
 .UNSPECIFIED., .F., .F.,
 ( 4, 4 ),
 ( 0.03384845726238354391, 0.04271176938863220640 ),
 .UNSPECIFIED. ) ;
#98055 = CARTESIAN_POINT ( 'NONE',  ( 12.71236424662705566, 15.84335787977761534, 9.188101187500006262 ) ) ;
#98056 = ORIENTED_EDGE ( 'NONE', *, *, #64639, .F. ) ;
#98057 = CIRCLE ( 'NONE', #44641, 70.00000000000001421 ) ;
#98058 = CARTESIAN_POINT ( 'NONE',  ( 166.9003224155486294, 284.2591062721578510, 9.432497891095570353 ) ) ;
#98060 = VERTEX_POINT ( 'NONE', #28002 ) ;
#98059 = CARTESIAN_POINT ( 'NONE',  ( 199.8975600284485097, 270.2813002518563508, 9.754130713005407571 ) ) ;
#98061 = CARTESIAN_POINT ( 'NONE',  ( -16.06007122719572777, 105.4852662834641990, 11.75378467557247397 ) ) ;
#98062 = CARTESIAN_POINT ( 'NONE',  ( 162.7644741734472120, 248.7306563947940958, 9.865755277559742353 ) ) ;
#98063 = CARTESIAN_POINT ( 'NONE',  ( 159.9894443651313338, 253.5371490153152081, -16.36035038356864391 ) ) ;
#98064 = CARTESIAN_POINT ( 'NONE',  ( 157.5297984379545255, 279.9475811940735639, -6.869905029983002898 ) ) ;
#98065 = CARTESIAN_POINT ( 'NONE',  ( 79.71918192488826094, 50.71085193480788433, -15.38226593809065790 ) ) ;
#98066 = AXIS2_PLACEMENT_3D ( 'NONE', #52692, #46585, #77523 ) ;
#98067 = CARTESIAN_POINT ( 'NONE',  ( 159.3291946290163992, 279.0199804063916531, 10.96233109238993109 ) ) ;
#98068 = CARTESIAN_POINT ( 'NONE',  ( 84.92581716621455712, 42.43763314791823404, 1.843432607090159658 ) ) ;
#98069 = CARTESIAN_POINT ( 'NONE',  ( 88.26412553154668217, 44.25805425434632667, -1.894382960065053023 ) ) ;
#98070 = ORIENTED_EDGE ( 'NONE', *, *, #81599, .F. ) ;
#98071 = CARTESIAN_POINT ( 'NONE',  ( 181.4968897611953480, 271.1066667875069243, -15.95701483517411567 ) ) ;
#98072 = ORIENTED_EDGE ( 'NONE', *, *, #93908, .T. ) ;
#98073 = CARTESIAN_POINT ( 'NONE',  ( 193.3401853099748564, 294.2072595941227178, -14.34885575185585260 ) ) ;
#98074 = CARTESIAN_POINT ( 'NONE',  ( 171.4019447439835915, 279.6636507153484672, -14.71532880965975565 ) ) ;
#98075 = LINE ( 'NONE', #73281, #80653 ) ;
#98076 = CARTESIAN_POINT ( 'NONE',  ( 85.18987148710466784, 44.62537788682696061, -7.596096801918241326 ) ) ;
#98077 = CARTESIAN_POINT ( 'NONE',  ( 164.6388426154193780, 274.3663210464239341, 14.78880850689299997 ) ) ;
#98079 = CARTESIAN_POINT ( 'NONE',  ( 88.03979860270585789, 44.27742478294888429, 2.803906792406219761 ) ) ;
#98078 = CARTESIAN_POINT ( 'NONE',  ( -6.076397627723526540, 176.4869531367911293, 4.594050593750046652 ) ) ;
#98080 = EDGE_CURVE ( 'NONE', #88625, #98426, #11345, .T. ) ;
#98081 = CARTESIAN_POINT ( 'NONE',  ( 189.0710311799717829, 297.0389175199307488, 8.160305977522897436 ) ) ;
#98082 = EDGE_LOOP ( 'NONE', ( #81750, #51657, #35170, #99871 ) ) ;
#98083 = VECTOR ( 'NONE', #69287, 1000.000000000000227 ) ;
#98084 = ORIENTED_EDGE ( 'NONE', *, *, #59559, .F. ) ;
#98085 = FACE_OUTER_BOUND ( 'NONE', #90120, .T. ) ;
#98086 = CARTESIAN_POINT ( 'NONE',  ( 80.53966528798085278, 57.74330293187745156, 16.24346292769213562 ) ) ;
#98087 = ADVANCED_FACE ( 'NONE', ( #73137 ), #3731, .T. ) ;
#98088 = CARTESIAN_POINT ( 'NONE',  ( 44.10470679282202866, 121.9603419428074602, -10.00000000000000000 ) ) ;
#98089 = VECTOR ( 'NONE', #83787, 999.9999999999998863 ) ;
#98090 = CARTESIAN_POINT ( 'NONE',  ( 81.64670023727850889, 42.65128533460878657, -7.584980231169042852 ) ) ;
#98091 = CARTESIAN_POINT ( 'NONE',  ( 68.85919161853215087, 67.18729119566384611, 9.802711484835468170 ) ) ;
#98092 = CYLINDRICAL_SURFACE ( 'NONE', #6179, 70.00000000000002842 ) ;
#98093 = CARTESIAN_POINT ( 'NONE',  ( 11.29875767934929520, 168.1423013555409796, -4.594050593750043987 ) ) ;
#98094 = CARTESIAN_POINT ( 'NONE',  ( 110.4040191812834735, 243.7369531367911009, -4.594050593750048428 ) ) ;
#98095 = CARTESIAN_POINT ( 'NONE',  ( -13.11024591527734628, 6.000000000000000000, 32.50000000000000000 ) ) ;
#98096 = CARTESIAN_POINT ( 'NONE',  ( 186.4048238715421917, 296.5436351738768508, -7.262416587777808630 ) ) ;
#98097 = EDGE_CURVE ( 'NONE', #30966, #17413, #27024, .T. ) ;
#98098 = CARTESIAN_POINT ( 'NONE',  ( 78.98010352777859566, 56.10884667310566698, 16.15057212009154952 ) ) ;
#98099 = CARTESIAN_POINT ( 'NONE',  ( 175.9236718092338663, 281.9243915816493313, -14.20169403765913430 ) ) ;
#98100 = CARTESIAN_POINT ( 'NONE',  ( 76.02315037475985093, 54.93625610767154654, -16.12727872574887655 ) ) ;
#98101 = CARTESIAN_POINT ( 'NONE',  ( 193.7275870247597425, 295.1009717758319084, 14.48058678254265885 ) ) ;
#98102 = CARTESIAN_POINT ( 'NONE',  ( 183.9879157655500705, 275.0531484184239162, 16.36130672943231801 ) ) ;
#98103 = CARTESIAN_POINT ( 'NONE',  ( 147.8308140999695866, 274.5965143850199865, -7.866624397492971710 ) ) ;
#98104 = EDGE_CURVE ( 'NONE', #58060, #94071, #33072, .T. ) ;
#98105 = CARTESIAN_POINT ( 'NONE',  ( 84.38175156668881982, 50.02035787987339432, 13.81135446509517628 ) ) ;
#98106 = CARTESIAN_POINT ( 'NONE',  ( 192.7546399067283858, 265.3065417519427456, 7.788706340340938006 ) ) ;
#98107 = DIRECTION ( 'NONE',  ( 0.8434505012732891327, -0.5372068985985168910, 0.000000000000000000 ) ) ;
#98108 = CARTESIAN_POINT ( 'NONE',  ( 184.0492996101627341, 268.5858911698572342, -15.15661456208596114 ) ) ;
#98109 = ADVANCED_FACE ( 'NONE', ( #96962 ), #27528, .F. ) ;
#98110 = LINE ( 'NONE', #52982, #15716 ) ;
#98111 = CARTESIAN_POINT ( 'NONE',  ( -66.69146994933839778, 41.22495595238228105, 10.00000000000000000 ) ) ;
#98112 = CARTESIAN_POINT ( 'NONE',  ( 105.9391831106087380, 219.7202760586659736, -5.415160957724236172E-17 ) ) ;
#98113 = CARTESIAN_POINT ( 'NONE',  ( 14.61458989734527947, 10.29860640527290805, -2.839279412974138328 ) ) ;
#98114 = CARTESIAN_POINT ( 'NONE',  ( 150.6431064791187850, 269.7254810985950257, 15.11064854015152470 ) ) ;
#98115 = CARTESIAN_POINT ( 'NONE',  ( 157.5215017335775940, 258.4853116787141971, -16.92298772477023761 ) ) ;
#98117 = CARTESIAN_POINT ( 'NONE',  ( 200.1153681990099074, 284.0370102343983376, 18.51598427690537108 ) ) ;
#98116 = CARTESIAN_POINT ( 'NONE',  ( 195.7291534503633272, 291.6341570319625021, 16.44925029361851543 ) ) ;
#98118 = CARTESIAN_POINT ( 'NONE',  ( 197.0696450891457516, 289.3123574064699710, 17.43500942416782706 ) ) ;
#98119 = CARTESIAN_POINT ( 'NONE',  ( 75.82286285680700644, 65.49053554218845363, 14.29367836297802974 ) ) ;
#98120 = CARTESIAN_POINT ( 'NONE',  ( 173.2732189505960037, 267.9125929267007677, -16.31862377501282779 ) ) ;
#98121 = VECTOR ( 'NONE', #88408, 1000.000000000000000 ) ;
#98122 = CARTESIAN_POINT ( 'NONE',  ( 43.68478726420265446, 28.14754757982094802, -5.678558825948275768 ) ) ;
#98123 = CARTESIAN_POINT ( 'NONE',  ( 192.4259603496955719, 297.3554553095298729, -12.40738485318142814 ) ) ;
#98124 = CARTESIAN_POINT ( 'NONE',  ( 81.98204644731730184, 41.14170830008083612, -5.380964918418895238 ) ) ;
#98125 = ORIENTED_EDGE ( 'NONE', *, *, #98974, .T. ) ;
#98126 = CARTESIAN_POINT ( 'NONE',  ( 25.16147942602835386, 23.03085787977763843, 9.188101187500006262 ) ) ;
#98127 = CYLINDRICAL_SURFACE ( 'NONE', #18393, 17.82106496071139645 ) ;
#98128 = VECTOR ( 'NONE', #57039, 1000.000000000000000 ) ;
#98129 = CARTESIAN_POINT ( 'NONE',  ( 65.92723761088207368, 68.94945291059251247, -2.624861928015910895 ) ) ;
#98130 = CARTESIAN_POINT ( 'NONE',  ( 191.5300323225266368, 288.3933188615314975, -15.83635432281777611 ) ) ;
#98131 = ADVANCED_FACE ( 'NONE', ( #19927 ), #50799, .T. ) ;
#98132 =( BOUNDED_CURVE ( )  B_SPLINE_CURVE ( 2, ( #63351, #63847, #7277, #60971, #100004, #17242, #84822, #79599, #87728 ),
 .UNSPECIFIED., .F., .T. ) 
 B_SPLINE_CURVE_WITH_KNOTS ( ( 3, 2, 2, 2, 3 ),
 ( 0.004032258064516129788, 0.005376344086021505805, 0.008064516129032257841, 0.01075268817204301161, 0.01209677419354838676 ),
 .UNSPECIFIED. ) 
 CURVE ( )  GEOMETRIC_REPRESENTATION_ITEM ( )  RATIONAL_B_SPLINE_CURVE ( ( 0.9330127018922194093, 0.9330127018922194093, 1.000000000000000000, 0.8660254037844387076, 1.000000000000000000, 0.8660254037844387076, 1.000000000000000000, 0.9330127018922192983, 0.9330127018922194093 ) ) 
 REPRESENTATION_ITEM ( '' )  );
#98133 = VECTOR ( 'NONE', #42331, 1000.000000000000000 ) ;
#98134 = CARTESIAN_POINT ( 'NONE',  ( 70.48220200685271664, 60.91291783368861701, 14.45533156906698125 ) ) ;
#98135 = CARTESIAN_POINT ( 'NONE',  ( 198.4706398937704819, 286.8857632237200619, 17.04020736381253798 ) ) ;
#98136 = CARTESIAN_POINT ( 'NONE',  ( -27.42236680055714260, 166.5217562850347406, 1.224646799147364892E-15 ) ) ;
#98137 = CARTESIAN_POINT ( 'NONE',  ( 171.4736130609155680, 253.3145436162068052, -8.798943912126190980 ) ) ;
#98138 = CARTESIAN_POINT ( 'NONE',  ( 147.3907811248416522, 249.2365022471902023, -10.00000000000009059 ) ) ;
#98139 = CARTESIAN_POINT ( 'NONE',  ( 204.7242223814549504, 276.0542406257275161, -13.93608974681376189 ) ) ;
#98140 = ADVANCED_FACE ( 'NONE', ( #35608 ), #74129, .T. ) ;
#98141 = ORIENTED_EDGE ( 'NONE', *, *, #34831, .T. ) ;
#98142 = CARTESIAN_POINT ( 'NONE',  ( 70.46985782873493065, 64.39753548552634754, 13.11825968515873164 ) ) ;
#98143 = ORIENTED_EDGE ( 'NONE', *, *, #16168, .T. ) ;
#98144 = CARTESIAN_POINT ( 'NONE',  ( 196.6049509491368781, 265.3221703615579941, -4.491441117979137587 ) ) ;
#98145 = CARTESIAN_POINT ( 'NONE',  ( 84.29971156775336283, 42.10555697619372495, 2.085675295296966603 ) ) ;
#98146 = ORIENTED_EDGE ( 'NONE', *, *, #16841, .F. ) ;
#98148 = ADVANCED_FACE ( 'NONE', ( #80584 ), #78551, .T. ) ;
#98147 = CARTESIAN_POINT ( 'NONE',  ( 86.97523469022577558, 43.65653777248807899, 2.440289623876037872 ) ) ;
#98149 = ORIENTED_EDGE ( 'NONE', *, *, #23194, .F. ) ;
#98151 = EDGE_CURVE ( 'NONE', #64147, #69624, #858, .T. ) ;
#98150 = CARTESIAN_POINT ( 'NONE',  ( 47.79785968963117426, 191.7365022471902023, 10.00000000000009948 ) ) ;
#98152 = CARTESIAN_POINT ( 'NONE',  ( 205.5867850959394900, 274.5602381795258111, 12.00218932530894378 ) ) ;
#98153 = CARTESIAN_POINT ( 'NONE',  ( 192.3746808059117654, 279.8490869531318026, -16.68648498102840350 ) ) ;
#98154 = CARTESIAN_POINT ( 'NONE',  ( 204.1006587545853677, 272.9409856097431657, 11.03402274723170606 ) ) ;
#98155 = PLANE ( 'NONE',  #1319 ) ;
#98156 = PLANE ( 'NONE',  #12471 ) ;
#98157 = EDGE_CURVE ( 'NONE', #17199, #21265, #72466, .T. ) ;
#98158 = CARTESIAN_POINT ( 'NONE',  ( 43.01361757626970928, 27.76004757982093452, 5.678558825948272215 ) ) ;
#98159 = AXIS2_PLACEMENT_3D ( 'NONE', #86060, #24191, #79933 ) ;
#98160 = DIRECTION ( 'NONE',  ( 1.000000000000000000, 0.000000000000000000, 0.000000000000000000 ) ) ;
#98161 = EDGE_CURVE ( 'NONE', #62590, #74723, #68489, .T. ) ;
#98162 = CARTESIAN_POINT ( 'NONE',  ( 167.8678039839016662, 276.4972622578981145, 15.08462999136594718 ) ) ;
#98163 = B_SPLINE_CURVE_WITH_KNOTS ( 'NONE', 3,
 ( #34217, #33212, #18029, #19542, #17511, #48922, #63607, #71233, #10929, #79859, #64621, #1825, #94547, #86980, #64110, #41801, #95062, #25622, #56506, #87495, #72235, #2841, #49411, #72748, #3341, #65112, #96060, #26619, #29115, #99017, #21995, #81848, #20024, #13901, #12932, #90953, #82363, #89944 ),
 .UNSPECIFIED., .F., .F.,
 ( 4, 2, 2, 2, 2, 2, 2, 2, 2, 2, 2, 2, 2, 2, 2, 2, 2, 2, 4 ),
 ( 0.0009759269190796634021, 0.001069240376951313210, 0.001162553834822963126, 0.001349180750566163645, 0.001722434582052570105, 0.002468942245025379772, 0.003961957570971087576, 0.004708465233943942563, 0.005081719065430376561, 0.005268345981173551060, 0.005361659439045146983, 0.005454972896916742038, 0.005501629625852569490, 0.005548286354788396074, 0.005641599812660188888, 0.005828226728403780588, 0.006201480559890833882, 0.006574734391377886310, 0.006947988222864938737 ),
 .UNSPECIFIED. ) ;
#98164 = CARTESIAN_POINT ( 'NONE',  ( 23.46864935082046344, 158.3759306620404743, -22.49999999999983658 ) ) ;
#98165 = VECTOR ( 'NONE', #15650, 1000.000000000000000 ) ;
#98166 = EDGE_LOOP ( 'NONE', ( #84098, #89091, #56019 ) ) ;
#98167 = EDGE_LOOP ( 'NONE', ( #34741, #6720, #4887, #64161 ) ) ;
#98168 = CARTESIAN_POINT ( 'NONE',  ( 197.4075646047015482, 273.1427705089788560, -14.69744958829762815 ) ) ;
#98170 = CARTESIAN_POINT ( 'NONE',  ( 162.2256012757624433, 272.3419497268096734, -16.04947957637165956 ) ) ;
#98169 = CARTESIAN_POINT ( 'NONE',  ( -12.68721568607400485, 24.67147432707382748, -10.00000000000000000 ) ) ;
#98171 = CARTESIAN_POINT ( 'NONE',  ( 165.0807124393095364, 244.7188140358855151, -1.586079993046279446 ) ) ;
#98172 = CARTESIAN_POINT ( 'NONE',  ( 66.40574244791143599, 68.75251593721850440, -2.129884441287897001 ) ) ;
#98173 = CARTESIAN_POINT ( 'NONE',  ( 74.70219116882620369, 60.88919038526882588, -15.38845729014155417 ) ) ;
#98174 = CARTESIAN_POINT ( 'NONE',  ( 82.43030793700373238, 40.39877996038060814, 0.9710434448888033421 ) ) ;
#98175 = CARTESIAN_POINT ( 'NONE',  ( 171.0137737332507584, 287.8132002576012383, -4.438399254829208829 ) ) ;
#98176 = CARTESIAN_POINT ( 'NONE',  ( 76.77173841120222164, 63.31185858333683569, -15.44871830894366838 ) ) ;
#98177 = CARTESIAN_POINT ( 'NONE',  ( 178.2715496052864523, 255.5664410081183746, 4.888700057109781838 ) ) ;
#98178 = CARTESIAN_POINT ( 'NONE',  ( 106.6698052711106186, 223.2048013555410080, 4.594050593750051981 ) ) ;
#98179 = FACE_OUTER_BOUND ( 'NONE', #80910, .T. ) ;
#98180 = CARTESIAN_POINT ( 'NONE',  ( 188.4925541850777506, 273.6131829772801325, 15.65818043819186478 ) ) ;
#98181 = VERTEX_POINT ( 'NONE', #63332 ) ;
#98182 = ORIENTED_EDGE ( 'NONE', *, *, #39884, .T. ) ;
#98183 = CARTESIAN_POINT ( 'NONE',  ( 87.14453225490829880, 46.27907944775106586, -9.173786573548373013 ) ) ;
#98184 = LINE ( 'NONE', #53053, #62504 ) ;
#98185 = CARTESIAN_POINT ( 'NONE',  ( 157.8740713127050981, 257.2010826190796706, 17.31862062017425075 ) ) ;
#98186 = CARTESIAN_POINT ( 'NONE',  ( 206.1798448551755598, 273.5330285446045195, -10.53862763475382813 ) ) ;
#98188 = B_SPLINE_CURVE_WITH_KNOTS ( 'NONE', 3,
 ( #69950, #567, #24369, #85731 ),
 .UNSPECIFIED., .F., .F.,
 ( 4, 4 ),
 ( 0.009256042836502432342, 0.01507217474330474830 ),
 .UNSPECIFIED. ) ;
#98187 = CARTESIAN_POINT ( 'NONE',  ( 73.99737204167014681, 54.85251815435404410, -16.13421978449814986 ) ) ;
#98189 = ORIENTED_EDGE ( 'NONE', *, *, #61760, .T. ) ;
#98190 = ORIENTED_EDGE ( 'NONE', *, *, #64950, .F. ) ;
#98191 = CARTESIAN_POINT ( 'NONE',  ( 163.1369207721744772, 248.0855599626920593, -11.24692769914530110 ) ) ;
#98192 = ORIENTED_EDGE ( 'NONE', *, *, #8507, .T. ) ;
#98193 = B_SPLINE_CURVE_WITH_KNOTS ( 'NONE', 3,
 ( #3568, #26855, #96286, #50147, #33975, #72977, #57236, #58237, #56745, #11176, #12156, #87727, #88711, #95313, #43018, #2569, #42043, #82094, #34449, #42529, #3084, #18265, #64349, #49159, #80095, #10661, #57731, #65347, #73462, #81100, #41537, #19280, #95806, #50634, #11667, #34935, #65830, #88211, #19765, #51132, #73957, #96796, #27355, #64859, #72482, #4542, #89217, #27845, #18762, #81587, #97278, #49640 ),
 .UNSPECIFIED., .F., .F.,
 ( 4, 2, 2, 2, 2, 2, 2, 2, 2, 2, 2, 2, 2, 2, 2, 2, 2, 2, 2, 2, 2, 2, 2, 2, 2, 4 ),
 ( 0.0001991101052095526139, 0.001225461298171744411, 0.001738636894652840310, 0.001866930793773159550, 0.001995224692893479007, 0.002123518592013798247, 0.002251812491134116186, 0.002380106390254435426, 0.002508400289374754667, 0.002764988087615294268, 0.003278163684096418139, 0.004304514877058586951, 0.005330866070020754896, 0.005844041666501914763, 0.006100629464742417934, 0.006357217262982921106, 0.006421364212543102627, 0.006485511162103285016, 0.006549658111663465669, 0.006613805061223648057, 0.006870392859464352457, 0.007383568455945755185, 0.007640156254186507290, 0.007896744052427259394, 0.008153331850668011499, 0.008409919648908761869 ),
 .UNSPECIFIED. ) ;
#98194 = DIRECTION ( 'NONE',  ( 0.000000000000000000, 0.000000000000000000, 1.000000000000000000 ) ) ;
#98195 = CARTESIAN_POINT ( 'NONE',  ( 103.5583290153452083, 219.0494855054051868, -2.679491924311248496 ) ) ;
#98196 = VECTOR ( 'NONE', #38953, 1000.000000000000114 ) ;
#98197 = CARTESIAN_POINT ( 'NONE',  ( 84.13204908911603752, 50.42604040346916605, 13.71367173376234838 ) ) ;
#98199 = CARTESIAN_POINT ( 'NONE',  ( 69.61708508526400863, 62.59193294829653098, -13.35423466821234584 ) ) ;
#98198 = CARTESIAN_POINT ( 'NONE',  ( 184.1873351008822226, 288.8905979614012836, -14.49962578542382907 ) ) ;
#98200 = DIRECTION ( 'NONE',  ( 0.3002896333693469422, 0.9538480676139692305, 0.000000000000000000 ) ) ;
#98201 = VERTEX_POINT ( 'NONE', #2042 ) ;
#98202 = CARTESIAN_POINT ( 'NONE',  ( 59.25465409031482977, 215.0177522451419065, 5.000000000000046185 ) ) ;
#98203 = CARTESIAN_POINT ( 'NONE',  ( 82.58901599275658612, 52.38560239326635326, 14.96489765216765377 ) ) ;
#98204 = CARTESIAN_POINT ( 'NONE',  ( 82.29231835864526090, 40.76292279040190181, -3.679577836841430916 ) ) ;
#98205 = CARTESIAN_POINT ( 'NONE',  ( 170.2455760408510912, 248.6530624101944511, -0.2700544060848846795 ) ) ;
#98206 = CARTESIAN_POINT ( 'NONE',  ( 178.3183837364390172, 285.6435033645693125, 14.40467033256238949 ) ) ;
#98207 = CARTESIAN_POINT ( 'NONE',  ( 71.91048869424076884, 72.26696636997301937, 3.280994121815376641 ) ) ;
#98208 = CARTESIAN_POINT ( 'NONE',  ( 196.4434894085402163, 280.3196924634482912, -16.68800359730008864 ) ) ;
#98209 = LINE ( 'NONE', #29302, #13939 ) ;
#98210 = VECTOR ( 'NONE', #93465, 1000.000000000000000 ) ;
#98211 = CARTESIAN_POINT ( 'NONE',  ( 80.04809861183208852, 50.31413521909311726, 14.67867987935995977 ) ) ;
#98212 = CARTESIAN_POINT ( 'NONE',  ( 69.60898357418011528, 70.31892478126285084, -3.724007916725324385 ) ) ;
#98213 = CARTESIAN_POINT ( 'NONE',  ( 61.47358386746269332, 215.4869531367911009, 4.594050593750046652 ) ) ;
#98214 = CARTESIAN_POINT ( 'NONE',  ( 159.2651917302844993, 254.7915913763855258, -16.53922207549818424 ) ) ;
#98215 = CARTESIAN_POINT ( 'NONE',  ( 77.59172485204311442, 61.78102913438976174, 15.67081180326514556 ) ) ;
#98216 = CARTESIAN_POINT ( 'NONE',  ( 208.3764315856425640, 269.7284287242038658, -1.833640725398759441 ) ) ;
#98217 = EDGE_CURVE ( 'NONE', #29718, #23380, #86678, .T. ) ;
#98218 = CARTESIAN_POINT ( 'NONE',  ( 197.3443028699994954, 288.4215049135930826, -16.72861298487629256 ) ) ;
#98219 = VECTOR ( 'NONE', #76283, 999.9999999999998863 ) ;
#98220 = CARTESIAN_POINT ( 'NONE',  ( 161.7767236248226084, 250.4414905302161287, -13.15904643207033153 ) ) ;
#98221 = CARTESIAN_POINT ( 'NONE',  ( 195.3506579275178581, 288.6704280282520472, 17.27067453383686768 ) ) ;
#98222 = AXIS2_PLACEMENT_3D ( 'NONE', #80912, #66153, #11484 ) ;
#98223 = CARTESIAN_POINT ( 'NONE',  ( -20.93739514293010728, 95.10073009761491392, 45.19938842315524852 ) ) ;
#98224 = ADVANCED_FACE ( 'NONE', ( #96272 ), #55702, .F. ) ;
#98225 = CARTESIAN_POINT ( 'NONE',  ( 34.89708068152319242, 43.08080186712595605, -3.090169943749475845 ) ) ;
#98226 = CARTESIAN_POINT ( 'NONE',  ( 38.90713653809340400, 79.99999999999998579, 10.00000000000000000 ) ) ;
#98227 = CARTESIAN_POINT ( 'NONE',  ( 82.09289782346584730, 54.09536945811088060, 15.61809530791954082 ) ) ;
#98228 = CARTESIAN_POINT ( 'NONE',  ( 71.91048869424076884, 72.26696636997301937, 3.280994121815385078 ) ) ;
#98229 = EDGE_CURVE ( 'NONE', #19444, #10367, #94769, .T. ) ;
#98230 = CARTESIAN_POINT ( 'NONE',  ( 28.37560933628243731, 181.0643266524159856, -9.188101187500093303 ) ) ;
#98231 = CARTESIAN_POINT ( 'NONE',  ( 196.4390255720217908, 290.4046224503736653, 16.34739044515864848 ) ) ;
#98232 = CARTESIAN_POINT ( 'NONE',  ( 46.58353466793526110, 27.86426979415093896, -3.090169943749474069 ) ) ;
#98233 = B_SPLINE_CURVE_WITH_KNOTS ( 'NONE', 3,
 ( #16773, #79629, #95347, #63381, #32487, #54764, #94320, #85747, #63880, #8681, #41059, #16275, #25903, #47170, #1088, #55750, #47666, #71503, #10194, #39551, #71001, #2600, #1604, #33487, #94815, #49193, #86742, #10690, #64384, #78598, #56775, #87758, #86238, #41569, #48181, #72512, #79126, #34006, #62870, #2095, #93827, #32973, #55255, #9184, #44051, #51163, #35472, #49673 ),
 .UNSPECIFIED., .F., .F.,
 ( 4, 2, 2, 2, 2, 2, 2, 2, 2, 2, 2, 2, 2, 2, 2, 2, 2, 2, 2, 2, 2, 2, 2, 4 ),
 ( 0.001675801244915591480, 0.002130441261090271210, 0.002585081277264950940, 0.002812401285352291239, 0.002926061289395960954, 0.003039721293439630670, 0.003153381297483300819, 0.003267041301526970969, 0.003494361309614205449, 0.003949001325788674410, 0.004403641341963143371, 0.005312921374312083028, 0.006222201406661022685, 0.006676841422835528943, 0.007131481439010035200, 0.007245141443053576547, 0.007301971445075379312, 0.007358801447097183812, 0.007472461451140789343, 0.007586121455184395741, 0.008040761471358938428, 0.008495401487533481982, 0.008722721495620708657, 0.008950041503707935331 ),
 .UNSPECIFIED. ) ;
#98234 = CARTESIAN_POINT ( 'NONE',  ( 43.83595887736691310, 122.5461495720015677, 10.00000000000000000 ) ) ;
#98235 = CARTESIAN_POINT ( 'NONE',  ( 71.84094281513496583, 72.11187483614946814, -1.688609671837987714 ) ) ;
#98236 = CARTESIAN_POINT ( 'NONE',  ( 58.36173894231862391, 198.3768266524160140, 9.188101187500096856 ) ) ;
#98237 = B_SPLINE_CURVE_WITH_KNOTS ( 'NONE', 3,
 ( #67906, #44084, #44582, #15174 ),
 .UNSPECIFIED., .F., .F.,
 ( 4, 4 ),
 ( 0.008175067078588206526, 0.01423883080510260878 ),
 .UNSPECIFIED. ) ;
#98238 = CARTESIAN_POINT ( 'NONE',  ( 20.42541317417268942, 33.83396525600390703, -2.839279412974133887 ) ) ;
#98239 = CARTESIAN_POINT ( 'NONE',  ( 151.3898985249405200, 268.4319993325432847, -14.65018536945715510 ) ) ;
#98240 = CARTESIAN_POINT ( 'NONE',  ( -6.929581007982106300, 155.2592609112379876, 2.679491924311252937 ) ) ;
#98241 = CARTESIAN_POINT ( 'NONE',  ( 40.44261144040436307, 35.30066082961425167, -10.00000000000000533 ) ) ;
#98242 = CARTESIAN_POINT ( 'NONE',  ( 200.9253810108797893, 268.8241845523467646, -6.444322578389119371 ) ) ;
#98243 = CARTESIAN_POINT ( 'NONE',  ( 175.5883609201405022, 291.0961144979737014, 2.242416747171071645 ) ) ;
#98244 = CARTESIAN_POINT ( 'NONE',  ( 180.1079967660572265, 276.2603422707981622, 17.03935691071084335 ) ) ;
#98245 = CARTESIAN_POINT ( 'NONE',  ( 73.28922804852240347, 64.01006259886945315, 13.80277416833904525 ) ) ;
#98246 = CARTESIAN_POINT ( 'NONE',  ( 69.29708453640807875, 67.89305789087417509, -8.400680196542618106 ) ) ;
#98247 = CARTESIAN_POINT ( 'NONE',  ( 191.4207474145670460, 266.7759722589373723, 10.87581393504784444 ) ) ;
#98248 = LINE ( 'NONE', #45015, #23464 ) ;
#98249 = CARTESIAN_POINT ( 'NONE',  ( 90.23310447506860044, 236.2365022471903444, 2.944929066748280225E-16 ) ) ;
#98250 = CARTESIAN_POINT ( 'NONE',  ( 161.4396252346964218, 251.0253620690641299, 14.51972485405798885 ) ) ;
#98251 = EDGE_CURVE ( 'NONE', #35007, #59341, #11456, .T. ) ;
#98252 = CARTESIAN_POINT ( 'NONE',  ( 165.1203120823259098, 270.0476859643460443, -16.31784969181675748 ) ) ;
#98253 = VERTEX_POINT ( 'NONE', #71952 ) ;
#98254 = CARTESIAN_POINT ( 'NONE',  ( 59.55217677675723564, 211.3149278399160949, -9.188101187500095079 ) ) ;
#98255 = ORIENTED_EDGE ( 'NONE', *, *, #69275, .F. ) ;
#98256 = CARTESIAN_POINT ( 'NONE',  ( 166.0902180206555556, 265.3285796677840267, 16.55597451408016596 ) ) ;
#98257 = CARTESIAN_POINT ( 'NONE',  ( 162.3203620077491962, 250.6751068356387577, 12.61930170232072435 ) ) ;
#98258 = DIRECTION ( 'NONE',  ( -1.000000000000000000, 0.000000000000000000, 0.000000000000000000 ) ) ;
#98259 = ORIENTED_EDGE ( 'NONE', *, *, #56472, .F. ) ;
#98260 = CARTESIAN_POINT ( 'NONE',  ( 177.8194257969418288, 292.8449071177858514, 6.006967295066290013 ) ) ;
#98262 = EDGE_CURVE ( 'NONE', #39107, #45874, #69561, .T. ) ;
#98261 = CARTESIAN_POINT ( 'NONE',  ( 79.24276467137505620, 45.83258386654563310, -12.43720478848687527 ) ) ;
#98263 = CARTESIAN_POINT ( 'NONE',  ( 150.5780525126727980, 271.8381578737140103, 12.98431582152410968 ) ) ;
#98264 = CARTESIAN_POINT ( 'NONE',  ( 177.2352494820021889, 274.8154387795073603, -16.96091352554584475 ) ) ;
#98265 = CARTESIAN_POINT ( 'NONE',  ( -13.11024591527734451, 27.99999999999999645, 48.00000000000000000 ) ) ;
#98266 = VECTOR ( 'NONE', #4259, 1000.000000000000000 ) ;
#98267 = CARTESIAN_POINT ( 'NONE',  ( 204.4814917997891541, 276.4746623257233296, 13.21872368206963877 ) ) ;
#98268 = VERTEX_POINT ( 'NONE', #3555 ) ;
#98269 = AXIS2_PLACEMENT_3D ( 'NONE', #91409, #36168, #6777 ) ;
#98270 = CARTESIAN_POINT ( 'NONE',  ( 26.78885238572174998, 16.26216523072495335, -2.296566073217252530E-15 ) ) ;
#98271 = CARTESIAN_POINT ( 'NONE',  ( 76.22732431156450161, 61.39392654391182447, 15.52879837349084724 ) ) ;
#98272 = CARTESIAN_POINT ( 'NONE',  ( 174.9188381007038799, 255.1700493696978356, 8.143286963564044356 ) ) ;
#98273 = CARTESIAN_POINT ( 'NONE',  ( 75.15236017364199483, 67.01938754673118126, -12.72247072481832042 ) ) ;
#98274 = EDGE_CURVE ( 'NONE', #11685, #92469, #72963, .T. ) ;
#98275 = ORIENTED_EDGE ( 'NONE', *, *, #91175, .T. ) ;
#98276 = CARTESIAN_POINT ( 'NONE',  ( 77.55346118162754010, 59.95786661728646294, 16.37051007951880521 ) ) ;
#98277 = CARTESIAN_POINT ( 'NONE',  ( 167.0235062565406565, 261.5460872093962053, 16.43802016297843238 ) ) ;
#98278 = CARTESIAN_POINT ( 'NONE',  ( 206.8313602288537538, 272.4045708154811791, -9.607337080360906612 ) ) ;
#98279 = VERTEX_POINT ( 'NONE', #95296 ) ;
#98280 = CIRCLE ( 'NONE', #25438, 15.50000000000000000 ) ;
#98282 = CARTESIAN_POINT ( 'NONE',  ( 149.2678550509543811, 265.6471520882315076, -1.519623991172851672E-15 ) ) ;
#98281 = CARTESIAN_POINT ( 'NONE',  ( 162.7117101085248407, 283.4291563370742892, -3.114432215248377211 ) ) ;
#98283 = CARTESIAN_POINT ( 'NONE',  ( 162.6425574510925003, 248.9418223522047526, -10.70838742014210077 ) ) ;
#98284 = CARTESIAN_POINT ( 'NONE',  ( 66.07789273159161780, 69.13191440305783431, -2.042338407063129857 ) ) ;
#98285 = DIRECTION ( 'NONE',  ( 0.5000000000000014433, -0.8660254037844378194, 0.000000000000000000 ) ) ;
#98286 = CARTESIAN_POINT ( 'NONE',  ( 81.76364840784469834, 55.63774643643142781, 16.32517576395870407 ) ) ;
#98287 = CARTESIAN_POINT ( 'NONE',  ( 205.1786601861764723, 272.2841766866060311, 10.06407076913277088 ) ) ;
#98288 = CARTESIAN_POINT ( 'NONE',  ( 127.7791744883563183, 235.3923013555409796, 4.594050593750050204 ) ) ;
#98289 = CARTESIAN_POINT ( 'NONE',  ( 28.46864935082048831, 149.7156766241961350, 21.50000000000008527 ) ) ;
#98290 = VERTEX_POINT ( 'NONE', #26840 ) ;
#98291 = CARTESIAN_POINT ( 'NONE',  ( 170.4674085893365714, 263.7776824676311662, 15.83595988821661571 ) ) ;
#98292 = CARTESIAN_POINT ( 'NONE',  ( 79.08607190154688737, 46.03631599640020511, 13.24059178838384376 ) ) ;
#98293 = ORIENTED_EDGE ( 'NONE', *, *, #81793, .F. ) ;
#98294 = AXIS2_PLACEMENT_3D ( 'NONE', #30276, #93099, #30784 ) ;
#98295 = CARTESIAN_POINT ( 'NONE',  ( 75.48286763772496499, 43.98415679381830756, 1.224646799147354045E-15 ) ) ;
#98296 = ORIENTED_EDGE ( 'NONE', *, *, #10202, .T. ) ;
#98297 = ORIENTED_EDGE ( 'NONE', *, *, #26633, .F. ) ;
#98298 = FACE_BOUND ( 'NONE', #5223, .T. ) ;
#98299 = CARTESIAN_POINT ( 'NONE',  ( 75.10826011298540550, 67.04338188511664498, -12.68672718483817263 ) ) ;
#98300 = CARTESIAN_POINT ( 'NONE',  ( 194.1740526473003001, 284.7360119068420090, 17.59213183599199937 ) ) ;
#98301 = CARTESIAN_POINT ( 'NONE',  ( -30.93189967759662196, 96.24030206069060966, 12.57434963852382559 ) ) ;
#98302 = CARTESIAN_POINT ( 'NONE',  ( 81.88283113365912413, 55.39261312399677450, 16.27191101227217729 ) ) ;
#98303 = CARTESIAN_POINT ( 'NONE',  ( 194.2199708651012600, 294.2481379475345875, 15.50834247347371253 ) ) ;
#98304 = CARTESIAN_POINT ( 'NONE',  ( 172.0455612308954869, 276.6794935234722743, 15.97629919534607268 ) ) ;
#98305 = VERTEX_POINT ( 'NONE', #10649 ) ;
#98306 = EDGE_CURVE ( 'NONE', #43056, #44968, #70298, .T. ) ;
#98307 = CARTESIAN_POINT ( 'NONE',  ( 70.45877369499376641, 64.12567799070421870, -12.70804357532220585 ) ) ;
#98308 = AXIS2_PLACEMENT_3D ( 'NONE', #86310, #86815, #16845 ) ;
#98309 = CARTESIAN_POINT ( 'NONE',  ( 153.3859906278383676, 264.9746663937372091, -17.41799046551451013 ) ) ;
#98310 = DIRECTION ( 'NONE',  ( -0.9213551052231903071, 0.3887219701524006754, 0.000000000000000000 ) ) ;
#98311 = ORIENTED_EDGE ( 'NONE', *, *, #9042, .F. ) ;
#98312 = CARTESIAN_POINT ( 'NONE',  ( 28.46864935082050252, 149.7156766241961350, -37.49999999999994316 ) ) ;
#98313 = EDGE_CURVE ( 'NONE', #96690, #26854, #29742, .T. ) ;
#98314 = CARTESIAN_POINT ( 'NONE',  ( 76.25165189308367530, 51.01334316971484384, -16.04164650862850294 ) ) ;
#98315 = LINE ( 'NONE', #8461, #69112 ) ;
#98316 = B_SPLINE_CURVE_WITH_KNOTS ( 'NONE', 3,
 ( #19164, #49532, #97657, #43420, #66725, #50039, #88601, #95699, #51019, #35829, #26246, #72869, #74367, #26738, #89110, #41933, #57120, #65233, #19658, #4430, #41422, #96178, #57623, #72367 ),
 .UNSPECIFIED., .F., .F.,
 ( 4, 2, 2, 2, 2, 2, 2, 2, 2, 2, 2, 4 ),
 ( 0.000000000000000000, 0.1249999999999770739, 0.2499999999999541478, 0.3749999999999312217, 0.4374999999999381051, 0.4999999999999450440, 0.5624999999999519273, 0.6249999999999588107, 0.6874999999999658051, 0.7499999999999727995, 0.8749999999999863443, 1.000000000000000000 ),
 .UNSPECIFIED. ) ;
#98317 = LINE ( 'NONE', #53554, #59107 ) ;
#98318 = CARTESIAN_POINT ( 'NONE',  ( 191.0907015319009474, 260.9773198129059324, -3.629663310244437557 ) ) ;
#98319 = CARTESIAN_POINT ( 'NONE',  ( 195.3647503060396957, 279.2613744222268792, 16.32278432642107902 ) ) ;
#98320 = CARTESIAN_POINT ( 'NONE',  ( 207.6932907333322191, 270.9116633891313199, 2.120963121341169710 ) ) ;
#98321 = CARTESIAN_POINT ( 'NONE',  ( 129.3483248890680954, 254.6744531367911577, 4.594050593750047540 ) ) ;
#98322 = EDGE_LOOP ( 'NONE', ( #98542, #4192, #8697, #24460 ) ) ;
#98323 = CARTESIAN_POINT ( 'NONE',  ( 87.95873400847938228, 44.36334681983743877, 4.762736470890962970 ) ) ;
#98324 = CARTESIAN_POINT ( 'NONE',  ( 182.1029699310405761, 257.8865440850851769, 6.538144971207902501 ) ) ;
#98325 = CARTESIAN_POINT ( 'NONE',  ( 155.9473334272112197, 262.0296148265339298, -16.96532868042320885 ) ) ;
#98326 = CARTESIAN_POINT ( 'NONE',  ( 72.94799734335821029, 70.82305301834774980, 7.343759151627872406 ) ) ;
#98327 = CARTESIAN_POINT ( 'NONE',  ( 4.061437313896076873, 69.78113336816737444, -10.00000000000000000 ) ) ;
#98328 = ORIENTED_EDGE ( 'NONE', *, *, #55295, .T. ) ;
#98329 = CARTESIAN_POINT ( 'NONE',  ( 77.47913788626532039, 60.68569559966617533, 15.87193550285029353 ) ) ;
#98330 = CARTESIAN_POINT ( 'NONE',  ( 182.1025678104670646, 275.6566577031950374, -16.43659905335109173 ) ) ;
#98331 = CARTESIAN_POINT ( 'NONE',  ( 164.8584712946003776, 247.1261223207595492, -5.618710548772211766 ) ) ;
#98332 = VECTOR ( 'NONE', #66202, 1000.000000000000227 ) ;
#98333 = CARTESIAN_POINT ( 'NONE',  ( 81.59908028989202933, 54.82413755204365913, 15.82053572924470686 ) ) ;
#98334 = CARTESIAN_POINT ( 'NONE',  ( 73.48095451340876139, 69.18981038965245034, -10.00245108973057562 ) ) ;
#98335 = CARTESIAN_POINT ( 'NONE',  ( 184.5457051153594534, 294.3635293766698169, 10.03055039675435367 ) ) ;
#98336 = CARTESIAN_POINT ( 'NONE',  ( 183.8274263638271577, 281.3324037098167310, 17.41033114534894111 ) ) ;
#98337 = VECTOR ( 'NONE', #1362, 1000.000000000000227 ) ;
#98338 = AXIS2_PLACEMENT_3D ( 'NONE', #6154, #82214, #98875 ) ;
#98339 = CARTESIAN_POINT ( 'NONE',  ( 192.9333490033828298, 268.2698727311234848, 12.60046548449609283 ) ) ;
#98340 = B_SPLINE_SURFACE_WITH_KNOTS ( 'NONE', 3, 1, ( 
 ( #18071, #48967 ),
 ( #10978, #54284 ),
 ( #23394, #68999 ),
 ( #22413, #38601 ),
 ( #46186, #78125 ),
 ( #91854, #69998 ),
 ( #84749, #15289 ),
 ( #30510, #8713 ),
 ( #45690, #84260 ),
 ( #85254, #53305 ),
 ( #31495, #1118 ),
 ( #99430, #76144 ),
 ( #39085, #61892 ),
 ( #83757, #77105 ),
 ( #60891, #14807 ),
 ( #613, #76617 ),
 ( #7203, #6718 ),
 ( #37597, #60393 ),
 ( #85779, #45205 ),
 ( #92843, #99926 ),
 ( #119, #15799 ),
 ( #53788, #68508 ),
 ( #61401, #31003 ),
 ( #7708, #39582 ),
 ( #30007, #46705 ),
 ( #69505, #92353 ),
 ( #62387, #91349 ),
 ( #21910, #77631 ),
 ( #8215, #16308 ),
 ( #22902, #93344 ),
 ( #23900, #54802 ) ),
 .UNSPECIFIED., .F., .F., .F.,
 ( 4, 3, 3, 3, 3, 3, 3, 3, 3, 3, 4 ),
 ( 2, 2 ),
 ( 0.000000000000000000, 0.1122669598086729614, 0.2243161639709527755, 0.3396355846218981900, 0.4553962076584977536, 0.5677860799922215262, 0.6749047109689575441, 0.7773884377078212893, 0.8775581155834120128, 0.9782364162377664707, 1.000000000000000000 ),
 ( 0.000000000000000000, 1.000000000000000000 ),
 .UNSPECIFIED. ) ;
#98341 = EDGE_CURVE ( 'NONE', #38602, #45464, #23365, .T. ) ;
#98342 = CARTESIAN_POINT ( 'NONE',  ( 18.89319741406618647, 35.00034080476290654, -1.878358725466461243E-16 ) ) ;
#98343 = CARTESIAN_POINT ( 'NONE',  ( 190.0707697440390689, 301.4347651000360884, 4.271360729158901748 ) ) ;
#98344 = CARTESIAN_POINT ( 'NONE',  ( 81.99822479814268661, 41.74554429046528981, 5.407556307920054373 ) ) ;
#98345 = DIRECTION ( 'NONE',  ( -0.8660254037844387076, -0.4999999999999998890, -0.000000000000000000 ) ) ;
#98346 = CARTESIAN_POINT ( 'NONE',  ( 159.2511875226268216, 254.8158473755685520, 15.75855490706745599 ) ) ;
#98347 = EDGE_CURVE ( 'NONE', #69911, #38470, #24888, .T. ) ;
#98348 = CARTESIAN_POINT ( 'NONE',  ( 161.2538201723544944, 251.3471858773438328, 13.36125779146621362 ) ) ;
#98349=STYLED_ITEM('',(#100324),#76389);
#98350 = CARTESIAN_POINT ( 'NONE',  ( 141.9600801517287607, 252.7677522451418497, 10.00000000000009592 ) ) ;
#98351 = EDGE_CURVE ( 'NONE', #59656, #63028, #35427, .T. ) ;
#98352 = CARTESIAN_POINT ( 'NONE',  ( 172.9104462670787257, 284.5517195599988440, -12.97937505523477064 ) ) ;
#98353 = VERTEX_POINT ( 'NONE', #82080 ) ;
#98354 = AXIS2_PLACEMENT_3D ( 'NONE', #18663, #49543, #1956 ) ;
#98355 = CARTESIAN_POINT ( 'NONE',  ( 66.58989550534374757, 68.03006047888345620, -6.526755023989535331 ) ) ;
#98356 = CARTESIAN_POINT ( 'NONE',  ( 198.8533049117289977, 286.2229679703367538, -18.60939981449148561 ) ) ;
#98357 = CARTESIAN_POINT ( 'NONE',  ( 12.46239254174337852, 171.8768266524159856, -9.188101187500093303 ) ) ;
#98358 = CARTESIAN_POINT ( 'NONE',  ( 178.6255663458269112, 259.3103340517776587, -10.56300147729930927 ) ) ;
#98359 = CARTESIAN_POINT ( 'NONE',  ( 31.41050339915249268, 17.94473085651393518, 1.475505719884397138E-15 ) ) ;
#98360 = CARTESIAN_POINT ( 'NONE',  ( 85.52132300739873472, 49.04541414811975386, 12.30295808577816352 ) ) ;
#98361 = CARTESIAN_POINT ( 'NONE',  ( 63.56442718099752653, 219.0530062829863027, -4.648177544792955347E-16 ) ) ;
#98362 = DIRECTION ( 'NONE',  ( 0.1857746241280557320, -0.9825923819316327856, 0.000000000000000000 ) ) ;
#98363 = CARTESIAN_POINT ( 'NONE',  ( -61.61048871844075592, 38.59675092633816007, 10.00000000000000000 ) ) ;
#98364 = B_SPLINE_SURFACE_WITH_KNOTS ( 'NONE', 3, 1, ( 
 ( #16576, #79926 ),
 ( #1892, #87048 ),
 ( #46981, #24675 ),
 ( #63177, #72305 ),
 ( #71803, #94121 ),
 ( #95129, #55557 ),
 ( #48488, #79429 ),
 ( #47963, #86542 ),
 ( #33279, #87561 ),
 ( #18092, #41366 ),
 ( #62160, #23661 ),
 ( #54552, #16078 ),
 ( #70270, #881 ),
 ( #31759, #17073 ),
 ( #47474, #78398 ),
 ( #9494, #40361 ),
 ( #34282, #43861 ),
 ( #27694, #34769 ),
 ( #20589, #82439 ),
 ( #11508, #49475 ),
 ( #19611, #35776 ),
 ( #66183, #51471 ),
 ( #65179, #19106 ),
 ( #97128, #13002 ),
 ( #74312, #2913 ),
 ( #4377, #96127 ),
 ( #33806, #58565 ),
 ( #66671, #96625 ),
 ( #12496, #81423 ),
 ( #97607, #89536 ),
 ( #27190, #4894 ),
 ( #41878, #28174 ),
 ( #42852, #64689 ),
 ( #65670, #35276 ) ),
 .UNSPECIFIED., .T., .F., .F.,
 ( 4, 2, 2, 2, 2, 2, 2, 2, 2, 2, 2, 2, 2, 2, 2, 2, 4 ),
 ( 2, 2 ),
 ( 0.000000000000000000, 0.06250000000000000000, 0.1250000000000000000, 0.1875000000000000000, 0.2500000000000000000, 0.3125000000000000000, 0.3750000000000000000, 0.4375000000000000000, 0.5000000000000000000, 0.5625000000000000000, 0.6250000000000000000, 0.6875000000000000000, 0.7500000000000000000, 0.8125000000000000000, 0.8750000000000000000, 0.9375000000000000000, 1.000000000000000000 ),
 ( 0.000000000000000000, 1.000000000000000000 ),
 .UNSPECIFIED. ) ;
#98366 = CARTESIAN_POINT ( 'NONE',  ( 77.00817486789590305, 205.2677522451417929, -5.000000000000041744 ) ) ;
#98365 = CARTESIAN_POINT ( 'NONE',  ( 199.4209461648062529, 270.9799452176341674, -11.09900091224045582 ) ) ;
#98367 = FACE_BOUND ( 'NONE', #27676, .T. ) ;
#98368 = CARTESIAN_POINT ( 'NONE',  ( 150.2982063762752603, 270.3228656002555681, 14.90512853129094495 ) ) ;
#98369 = CARTESIAN_POINT ( 'NONE',  ( 45.12761469462908792, 206.8615022471902876, 5.000000000000046185 ) ) ;
#98370 = FACE_OUTER_BOUND ( 'NONE', #75119, .T. ) ;
#98371 = AXIS2_PLACEMENT_3D ( 'NONE', #89557, #34308, #64719 ) ;
#98372 = EDGE_CURVE ( 'NONE', #57256, #56387, #43520, .T. ) ;
#98373 = CARTESIAN_POINT ( 'NONE',  ( 148.3930300673291640, 273.6227277647267897, 8.375036249079425232 ) ) ;
#98374 = CARTESIAN_POINT ( 'NONE',  ( 12.78680497239753144, 184.3149278399160949, -9.188101187500095079 ) ) ;
#98375 = CARTESIAN_POINT ( 'NONE',  ( 164.4110119407497734, 285.3093287471372719, 4.354449836773983229 ) ) ;
#98376 = LINE ( 'NONE', #52245, #75947 ) ;
#98377 = CARTESIAN_POINT ( 'NONE',  ( 36.38853680410606728, 41.98502408145596121, -5.678558825948271327 ) ) ;
#98378 = CARTESIAN_POINT ( 'NONE',  ( 202.1480882124455718, 280.0251659497182004, -15.78546128548377681 ) ) ;
#98379 = CARTESIAN_POINT ( 'NONE',  ( 206.8986117509267899, 272.2880877623646825, 6.975890063856878598 ) ) ;
#98380 = CARTESIAN_POINT ( 'NONE',  ( 186.0194694746173241, 266.9068538997193514, 13.20651731842044718 ) ) ;
#98381 = DIRECTION ( 'NONE',  ( -0.8660254037844378194, -0.5000000000000014433, -0.000000000000000000 ) ) ;
#98382 = CARTESIAN_POINT ( 'NONE',  ( 160.2301616673542242, 280.0696522150809074, 9.247322956015198159 ) ) ;
#98383 = APPLICATION_PROTOCOL_DEFINITION ( 'draft international standard', 'automotive_design', 1998, #29179 ) ;
#98384 = CARTESIAN_POINT ( 'NONE',  ( 18.12859834787737157, 11.26216523072493736, -2.296566073217252530E-15 ) ) ;
#98385 = CARTESIAN_POINT ( 'NONE',  ( 71.73821799984663983, 72.51259063078049394, 0.9720659048468339725 ) ) ;
#98386 = CARTESIAN_POINT ( 'NONE',  ( 82.99898243690306288, 53.45938235784409187, 15.65150354709845359 ) ) ;
#98387 = FACE_OUTER_BOUND ( 'NONE', #95191, .T. ) ;
#98388 = CARTESIAN_POINT ( 'NONE',  ( 193.9495889092963807, 294.7164532324382549, 15.46986001312306058 ) ) ;
#98389 = ORIENTED_EDGE ( 'NONE', *, *, #54975, .F. ) ;
#98390 = CARTESIAN_POINT ( 'NONE',  ( 182.6812089762738651, 289.5349527171500199, 12.27369044368959905 ) ) ;
#98391 = CARTESIAN_POINT ( 'NONE',  ( 2.405479210251257438, 24.49540643055184930, 3.479690158560446702E-15 ) ) ;
#98392 = CARTESIAN_POINT ( 'NONE',  ( 81.34586158848874504, 42.06304956376642679, 7.923271043321312490 ) ) ;
#98393 = CARTESIAN_POINT ( 'NONE',  ( 182.8075329105516289, 285.5996758505444291, -15.91971760981349071 ) ) ;
#98394 = ORIENTED_EDGE ( 'NONE', *, *, #46881, .F. ) ;
#98395 = FACE_OUTER_BOUND ( 'NONE', #6690, .T. ) ;
#98396 = CARTESIAN_POINT ( 'NONE',  ( 82.46408787962569420, 40.41550683742634931, 0.9310554388106409007 ) ) ;
#98397 = DIRECTION ( 'NONE',  ( 0.5000000000000014433, -0.8660254037844378194, 0.000000000000000000 ) ) ;
#98398 = CARTESIAN_POINT ( 'NONE',  ( 203.5080190724872011, 278.1607665491929993, -15.47044080916498743 ) ) ;
#98399 = EDGE_LOOP ( 'NONE', ( #26825, #3097, #14927, #39227, #61846, #11491, #79804, #44431, #57753, #64782, #99928, #62990, #37702, #23310, #81188, #96069, #58530, #75052, #22229, #78366, #44033, #72972 ) ) ;
#98400 = ORIENTED_EDGE ( 'NONE', *, *, #54455, .F. ) ;
#98401 = DIRECTION ( 'NONE',  ( 2.816764622163176506E-16, 1.626259812849726205E-16, -1.000000000000000000 ) ) ;
#98402 = CARTESIAN_POINT ( 'NONE',  ( 153.1164404339926080, 265.4415410246681972, 16.15325778160653414 ) ) ;
#98403 = EDGE_LOOP ( 'NONE', ( #77454, #2740, #16789, #6704 ) ) ;
#98404 = CARTESIAN_POINT ( 'NONE',  ( 190.8094645593471341, 300.1553081486349015, 8.399847186519689757 ) ) ;
#98405 = VECTOR ( 'NONE', #50970, 1000.000000000000114 ) ;
#98406 = DIRECTION ( 'NONE',  ( 0.000000000000000000, 1.000000000000000000, 0.000000000000000000 ) ) ;
#98407 = CARTESIAN_POINT ( 'NONE',  ( 45.83126033165601854, 207.2677522451419350, -5.000000000000047962 ) ) ;
#98408 = VERTEX_POINT ( 'NONE', #5530 ) ;
#98409 = CARTESIAN_POINT ( 'NONE',  ( 87.57040987469007121, 45.45830532627585541, -6.786269783605160200 ) ) ;
#98410 = CARTESIAN_POINT ( 'NONE',  ( 149.3629284598386278, 271.9428144707212027, -12.99253781774931049 ) ) ;
#98412 = EDGE_CURVE ( 'NONE', #32891, #20583, #45335, .T. ) ;
#98411 = AXIS2_PLACEMENT_3D ( 'NONE', #74298, #66659, #27682 ) ;
#98413 = CARTESIAN_POINT ( 'NONE',  ( 80.98043300753074902, 43.03517487223756177, 9.572663320340296877 ) ) ;
#98414 = VERTEX_POINT ( 'NONE', #14130 ) ;
#98415 = CARTESIAN_POINT ( 'NONE',  ( 165.0297293518065658, 244.8071193337670195, 2.517333243890161665 ) ) ;
#98416 = CARTESIAN_POINT ( 'NONE',  ( 149.4378998887816294, 275.3713422307953351, -8.174376149720645301 ) ) ;
#98417 = EDGE_LOOP ( 'NONE', ( #41817, #141, #35948, #97322 ) ) ;
#98418 = CARTESIAN_POINT ( 'NONE',  ( 174.5168695141670696, 276.9147204147473076, -15.82766731710391284 ) ) ;
#98419 = CARTESIAN_POINT ( 'NONE',  ( 172.2673562241199363, 264.0187931579786778, -15.69345930386550947 ) ) ;
#98420 = ORIENTED_EDGE ( 'NONE', *, *, #80960, .T. ) ;
#98421 = CARTESIAN_POINT ( 'NONE',  ( 158.7066903866863754, 275.0672323892235340, -12.54353524617913074 ) ) ;
#98422 = CARTESIAN_POINT ( 'NONE',  ( 91.96515528263753936, 217.2365022471902876, 10.00000000000009948 ) ) ;
#98423 = CARTESIAN_POINT ( 'NONE',  ( 162.7006039569504594, 261.3497057169571463, 17.57720365097131676 ) ) ;
#98425 = ORIENTED_EDGE ( 'NONE', *, *, #43374, .F. ) ;
#98424 = B_SPLINE_CURVE_WITH_KNOTS ( 'NONE', 3,
 ( #64418, #50210, #81162, #17829, #25933, #65902, #50696, #33010, #3150, #41601, #63911, #95867, #26425, #80664, #94849, #25410, #48730, #49227, #10226, #2633, #18331, #42105, #57305, #44083, #83137, #13707, #36496, #75023, #35506, #21311, #91232, #76030, #58784, #27904, #28916, #66899, #52188, #82159, #99316, #91732, #45096, #36996, #6100, #51721, #6607, #51192 ),
 .UNSPECIFIED., .F., .F.,
 ( 4, 1, 1, 1, 2, 2, 1, 1, 1, 2, 2, 1, 1, 2, 2, 1, 1, 2, 2, 1, 1, 2, 2, 1, 2, 2, 1, 2, 2, 4 ),
 ( 0.000000000000000000, 0.06249999999999465705, 0.09374999999999200639, 0.1093749999999922146, 0.1171874999999923117, 0.1249999999999924227, 0.1875000000000008327, 0.2187500000000050515, 0.2343750000000056621, 0.2421875000000053568, 0.2500000000000050515, 0.3125000000000046629, 0.3437500000000054401, 0.3593750000000048850, 0.3750000000000042744, 0.4375000000000038858, 0.4687500000000037748, 0.4843750000000032752, 0.5000000000000027756, 0.5625000000000078826, 0.5937500000000111022, 0.6093750000000122125, 0.6250000000000133227, 0.6875000000000107692, 0.7187500000000102141, 0.7500000000000095479, 0.8125000000000073275, 0.8437500000000063283, 0.8750000000000053291, 1.000000000000000000 ),
 .UNSPECIFIED. ) ;
#98426 = VERTEX_POINT ( 'NONE', #68315 ) ;
#98427 = AXIS2_PLACEMENT_3D ( 'NONE', #31305, #31795, #46495 ) ;
#98428 =( BOUNDED_CURVE ( )  B_SPLINE_CURVE ( 2, ( #13686, #46052, #60748, #99296, #67884, #90735, #45071, #44559, #75494 ),
 .UNSPECIFIED., .F., .T. ) 
 B_SPLINE_CURVE_WITH_KNOTS ( ( 3, 2, 2, 2, 3 ),
 ( 0.06048387096774193727, 0.06182795698924731242, 0.06451612903225806273, 0.06720430107526881303, 0.06854838709677418818 ),
 .UNSPECIFIED. ) 
 CURVE ( )  GEOMETRIC_REPRESENTATION_ITEM ( )  RATIONAL_B_SPLINE_CURVE ( ( 0.9330127018922194093, 0.9330127018922194093, 1.000000000000000000, 0.8660254037844387076, 1.000000000000000000, 0.8660254037844387076, 1.000000000000000000, 0.9330127018922194093, 0.9330127018922194093 ) ) 
 REPRESENTATION_ITEM ( '' )  );
#98429 = CARTESIAN_POINT ( 'NONE',  ( 76.84516209278983467, 52.46037536181771088, -16.28082285436079957 ) ) ;
#98430 = CARTESIAN_POINT ( 'NONE',  ( 147.5634954182374372, 275.0595239235922236, 4.682022975662822439 ) ) ;
#98431 = CARTESIAN_POINT ( 'NONE',  ( -13.11024591527734628, 27.99999999999999645, 32.50000000000000000 ) ) ;
#98432 = CARTESIAN_POINT ( 'NONE',  ( 190.0274641710971082, 301.5097725526222803, 3.738976720635653450 ) ) ;
#98433 = CARTESIAN_POINT ( 'NONE',  ( 152.7314557461996571, 266.1083540640618708, 17.39314074348802208 ) ) ;
#98434 = CARTESIAN_POINT ( 'NONE',  ( 147.2428775945425912, 275.6148502840442234, 0.4280630669697413349 ) ) ;
#98435 = CARTESIAN_POINT ( 'NONE',  ( 146.6834825911944620, 276.5837508513432681, 0.6716460511724984261 ) ) ;
#98436 = CIRCLE ( 'NONE', #19191, 17.82106496071138935 ) ;
#98437 = ORIENTED_EDGE ( 'NONE', *, *, #30491, .T. ) ;
#98438 = CARTESIAN_POINT ( 'NONE',  ( 75.39974219951720613, 57.58420828353521159, -16.06839496810986034 ) ) ;
#98439 = CARTESIAN_POINT ( 'NONE',  ( 149.9885642792388865, 274.4180868986143196, -10.02378587638088092 ) ) ;
#98440 = CARTESIAN_POINT ( 'NONE',  ( 41.82599275875796252, 62.29945068332010294, 10.00000000000000000 ) ) ;
#98441 = CARTESIAN_POINT ( 'NONE',  ( 67.00187114328801385, 67.08813303294822106, 8.529924657525400633 ) ) ;
#98442 = CARTESIAN_POINT ( 'NONE',  ( 171.1714030391351855, 288.3798238850056919, 4.167722100051413747 ) ) ;
#98443 = CARTESIAN_POINT ( 'NONE',  ( 165.4826352078684408, 255.7221904534726775, -15.26429383359580960 ) ) ;
#98444 = ORIENTED_EDGE ( 'NONE', *, *, #25704, .F. ) ;
#98445 = CARTESIAN_POINT ( 'NONE',  ( 190.6416006417717597, 300.4460569826327969, -3.339060657009423672 ) ) ;
#98446 = CARTESIAN_POINT ( 'NONE',  ( 78.56665040545209422, 53.37396691067563381, -15.81981728764792905 ) ) ;
#98447 = CARTESIAN_POINT ( 'NONE',  ( 202.5155473443252561, 279.0643611876510022, 15.50872832146021807 ) ) ;
#98448 = CARTESIAN_POINT ( 'NONE',  ( 78.89634812866061964, 46.30573133001255570, 12.89508449444912230 ) ) ;
#98449 = CARTESIAN_POINT ( 'NONE',  ( 171.2741013746033332, 249.3936815359432728, 2.927055546763141169 ) ) ;
#98450 = CARTESIAN_POINT ( 'NONE',  ( 77.42830020291178528, 55.47891526150226582, -16.57918540093258031 ) ) ;
#98451 = ORIENTED_EDGE ( 'NONE', *, *, #77743, .F. ) ;
#98452 = CARTESIAN_POINT ( 'NONE',  ( 170.7628550155183973, 255.3019951891120058, -12.90626094114390909 ) ) ;
#98453 = DIRECTION ( 'NONE',  ( 0.8660254037844390407, 0.4999999999999993339, 0.000000000000000000 ) ) ;
#98454 = VECTOR ( 'NONE', #74861, 1000.000000000000000 ) ;
#98455 = CARTESIAN_POINT ( 'NONE',  ( 155.5311623832600958, 261.6886619413561448, 17.00987194985870943 ) ) ;
#98456 = CARTESIAN_POINT ( 'NONE',  ( 44.60439100962805981, 209.8927522451419350, 2.944929066748280225E-16 ) ) ;
#98457 = CARTESIAN_POINT ( 'NONE',  ( 111.8924135700967497, 247.6589784336661069, -6.496448406907676862E-16 ) ) ;
#98458 = CARTESIAN_POINT ( 'NONE',  ( 180.5928094756065434, 294.4055607231725844, -3.443643769660447163 ) ) ;
#98459 = DIRECTION ( 'NONE',  ( 1.000000000000000000, 0.000000000000000000, 0.000000000000000000 ) ) ;
#98460 = CARTESIAN_POINT ( 'NONE',  ( 157.1338510812060747, 258.4831816688264325, 17.88958125218800888 ) ) ;
#98461 = DIRECTION ( 'NONE',  ( -0.8660254037844379305, -0.5000000000000014433, -0.000000000000000000 ) ) ;
#98462 = CARTESIAN_POINT ( 'NONE',  ( 33.57141466322406131, 196.3149278399160949, -9.188101187500095079 ) ) ;
#98463 = VECTOR ( 'NONE', #99835, 1000.000000000000000 ) ;
#98464 = CARTESIAN_POINT ( 'NONE',  ( 147.6166281148981625, 275.4172840431396594, -2.962624894996066960 ) ) ;
#98465 = ORIENTED_EDGE ( 'NONE', *, *, #33774, .T. ) ;
#98466 = CARTESIAN_POINT ( 'NONE',  ( 94.74134171723733289, 237.0530062829862743, -4.648177544792955347E-16 ) ) ;
#98467 = CARTESIAN_POINT ( 'NONE',  ( 178.0159405646096218, 265.6579100072215169, 15.49631030714943414 ) ) ;
#98468 = ADVANCED_FACE ( 'NONE', ( #30826 ), #57222, .F. ) ;
#98469 = DIRECTION ( 'NONE',  ( -0.000000000000000000, -0.000000000000000000, -1.000000000000000000 ) ) ;
#98470 = CARTESIAN_POINT ( 'NONE',  ( 146.7879906441258129, 276.4027375938661635, 4.347255311287614887 ) ) ;
#98471 = CARTESIAN_POINT ( 'NONE',  ( 81.87537396349165419, 41.14590722702494219, -5.544662510333616900 ) ) ;
#98472 = DIRECTION ( 'NONE',  ( -0.8660254037844379305, -0.5000000000000014433, -0.000000000000000000 ) ) ;
#98473 = EDGE_CURVE ( 'NONE', #82623, #74796, #79470, .T. ) ;
#98474 = CARTESIAN_POINT ( 'NONE',  ( 176.4155233639579876, 285.5687499269977252, -12.04987988516876385 ) ) ;
#98475 = CARTESIAN_POINT ( 'NONE',  ( 182.0096190830649618, 262.8089543526228340, 12.58302938569931939 ) ) ;
#98476 = B_SPLINE_CURVE_WITH_KNOTS ( 'NONE', 3,
 ( #83439, #12022, #37293, #50994 ),
 .UNSPECIFIED., .F., .F.,
 ( 4, 4 ),
 ( 0.02524082176100830507, 0.03448714665262276463 ),
 .UNSPECIFIED. ) ;
#98477 = CARTESIAN_POINT ( 'NONE',  ( 102.9889369814290632, 220.2677522451417929, -5.000000000000041744 ) ) ;
#98478 = VECTOR ( 'NONE', #54433, 1000.000000000000227 ) ;
#98479 = VERTEX_POINT ( 'NONE', #62705 ) ;
#98480 = CARTESIAN_POINT ( 'NONE',  ( 171.6154833087297789, 255.2606305366970503, 12.53362356821959978 ) ) ;
#98481 = EDGE_CURVE ( 'NONE', #90103, #54173, #40896, .T. ) ;
#98482 = CARTESIAN_POINT ( 'NONE',  ( 155.3653809515997750, 279.8371988227073643, -2.156620399925142539 ) ) ;
#98483 = CARTESIAN_POINT ( 'NONE',  ( 163.4084407101100851, 247.6152736349200438, -10.68829614238923931 ) ) ;
#98484 = CARTESIAN_POINT ( 'NONE',  ( 7.915412076110063033, 181.5024278399160664, -9.188101187500093303 ) ) ;
#98485 = AXIS2_PLACEMENT_3D ( 'NONE', #65372, #32481, #59237 ) ;
#98486 = CARTESIAN_POINT ( 'NONE',  ( 10.13172230794903683, 17.80066082961419838, 10.00000000000000533 ) ) ;
#98487 = CARTESIAN_POINT ( 'NONE',  ( 192.8217334130199276, 272.2506572471322670, 14.19735341291291064 ) ) ;
#98488 = CARTESIAN_POINT ( 'NONE',  ( 71.56806419291221744, 59.47990913521268652, -15.71253939761329832 ) ) ;
#98489 = CARTESIAN_POINT ( 'NONE',  ( 73.05912352472128646, 69.60491006942920933, 9.219028434792557292 ) ) ;
#98490 = CARTESIAN_POINT ( 'NONE',  ( 61.28457468009112574, 200.0643266524160424, 9.188101187500095079 ) ) ;
#98491 = CARTESIAN_POINT ( 'NONE',  ( 163.8455942243524248, 246.8581015375447691, -7.178103170949780676 ) ) ;
#98492 = CARTESIAN_POINT ( 'NONE',  ( 164.4990934228277411, 245.7262077230798809, 6.470820838822735510 ) ) ;
#98493 = CARTESIAN_POINT ( 'NONE',  ( 70.70474417252469834, 70.58686583719459406, 5.013298563372670991 ) ) ;
#98494 = CARTESIAN_POINT ( 'NONE',  ( 164.8329445879545290, 245.1479605429143760, -2.955380775890217304 ) ) ;
#98495 = ORIENTED_EDGE ( 'NONE', *, *, #12126, .F. ) ;
#98496 = VECTOR ( 'NONE', #41910, 1000.000000000000000 ) ;
#98497 = CARTESIAN_POINT ( 'NONE',  ( 165.2263101757220909, 269.2500600554935772, 17.42067060345640073 ) ) ;
#98498 = CARTESIAN_POINT ( 'NONE',  ( 22.68312297988245518, 177.2365022471902023, -10.00000000000009059 ) ) ;
#98499 = CARTESIAN_POINT ( 'NONE',  ( 208.2764314485352770, 269.9016340424377063, 2.433736665191914117 ) ) ;
#98500 = CARTESIAN_POINT ( 'NONE',  ( 135.5734031224162663, 239.8923013555409796, 4.594050593750050204 ) ) ;
#98501 = CARTESIAN_POINT ( 'NONE',  ( 27.04628097738780212, 27.56628583063842086, 9.188101187500006262 ) ) ;
#98502 = FACE_OUTER_BOUND ( 'NONE', #46266, .T. ) ;
#98503 = CARTESIAN_POINT ( 'NONE',  ( 83.80076462262509551, 51.77978008689729705, -14.86347872566931549 ) ) ;
#98504 = CARTESIAN_POINT ( 'NONE',  ( 63.68045258478197468, 219.1199935810940644, 2.679491924311251605 ) ) ;
#98506 = CARTESIAN_POINT ( 'NONE',  ( 189.0837441151423377, 289.7671154662007780, 14.43762572592019211 ) ) ;
#98505 = CARTESIAN_POINT ( 'NONE',  ( 88.28217478145764119, 43.95791727297698515, 2.470383038495647998 ) ) ;
#98507 = CARTESIAN_POINT ( 'NONE',  ( 68.94975261236909603, 64.36897199676705839, 12.51175351931266633 ) ) ;
#98508 = ORIENTED_EDGE ( 'NONE', *, *, #29598, .F. ) ;
#98509 = CARTESIAN_POINT ( 'NONE',  ( 167.6010540021560189, 247.4270797612363708, 3.638657435017179864 ) ) ;
#98510 = CARTESIAN_POINT ( 'NONE',  ( 163.9926361355883273, 246.6034174764422175, 7.548074001043944214 ) ) ;
#98511 = CARTESIAN_POINT ( 'NONE',  ( 68.30758603522241401, 67.25884571155089020, -9.331438848602806146 ) ) ;
#98512 = CARTESIAN_POINT ( 'NONE',  ( 169.6866200653663270, 266.0524855449860979, -17.34380911347102483 ) ) ;
#98513 = CARTESIAN_POINT ( 'NONE',  ( 194.5288312044114889, 271.4546633457422331, -13.52122573599391764 ) ) ;
#98515 = ORIENTED_EDGE ( 'NONE', *, *, #94508, .T. ) ;
#98514 = CONICAL_SURFACE ( 'NONE', #51561, 11.91750000000000043, 0.7853981633974482790 ) ;
#98516 = CARTESIAN_POINT ( 'NONE',  ( 144.9899443387551798, 254.5170451491295296, 0.000000000000000000 ) ) ;
#98517 = CARTESIAN_POINT ( 'NONE',  ( 86.54822389131679472, 42.74345947012793090, -2.172736160200603931E-06 ) ) ;
#98518 = LINE ( 'NONE', #29108, #70004 ) ;
#98519 = CARTESIAN_POINT ( 'NONE',  ( 192.4071554788542926, 293.6259026860700487, -14.64098184119582591 ) ) ;
#98520 = CARTESIAN_POINT ( 'NONE',  ( 88.45958475239287111, 43.85926912372239173, -0.5941283661710181629 ) ) ;
#98521 = CARTESIAN_POINT ( 'NONE',  ( 67.78857209169460418, 69.02767894211700650, 4.439189011663660978 ) ) ;
#98522 = DIRECTION ( 'NONE',  ( 0.000000000000000000, 0.6050222638427442678, -0.7962085532412978006 ) ) ;
#98523 = ORIENTED_EDGE ( 'NONE', *, *, #84952, .T. ) ;
#98524 = CARTESIAN_POINT ( 'NONE',  ( 194.5423442527744271, 283.0110300053098058, 17.49863978369591422 ) ) ;
#98525 = CARTESIAN_POINT ( 'NONE',  ( 12.45916558416763209, 19.14441083166259361, 10.00000000000000533 ) ) ;
#98526 = CARTESIAN_POINT ( 'NONE',  ( 172.3604664900529428, 278.3133719434953264, 16.43090493882906244 ) ) ;
#98527 = ORIENTED_EDGE ( 'NONE', *, *, #61063, .F. ) ;
#98528 = DIRECTION ( 'NONE',  ( 0.5000000000000005551, -0.8660254037844383745, 0.000000000000000000 ) ) ;
#98529 = DIRECTION ( 'NONE',  ( -0.000000000000000000, 0.000000000000000000, 1.000000000000000000 ) ) ;
#98530 = CARTESIAN_POINT ( 'NONE',  ( 83.84264525447930794, 45.19566160288086110, -9.473173988316984762 ) ) ;
#98531 = EDGE_LOOP ( 'NONE', ( #94183, #63160, #69053, #44418 ) ) ;
#98532 = CARTESIAN_POINT ( 'NONE',  ( 147.2229325088103735, 275.6493961858936927, -0.4918294119671829390 ) ) ;
#98533 = CARTESIAN_POINT ( 'NONE',  ( -19.65312891409030271, 93.06504152958497400, 177.5919119679930134 ) ) ;
#98534 = CARTESIAN_POINT ( 'NONE',  ( 204.1780753366177237, 277.0001950557890495, 14.05599973203924158 ) ) ;
#98535 = EDGE_CURVE ( 'NONE', #49424, #50507, #93663, .T. ) ;
#98536 = CARTESIAN_POINT ( 'NONE',  ( 49.43738778531180600, 210.8967562850346837, -4.648177544792955347E-16 ) ) ;
#98537 = ORIENTED_EDGE ( 'NONE', *, *, #66425, .T. ) ;
#98538 = CARTESIAN_POINT ( 'NONE',  ( 90.89164462408909628, 223.2833772461660260, -9.188101187500095079 ) ) ;
#98539 = CARTESIAN_POINT ( 'NONE',  ( 171.9473113485260285, 253.3425154589238275, -10.37853918848434809 ) ) ;
#98540 = CARTESIAN_POINT ( 'NONE',  ( 181.3431098572050644, 271.2290024631702750, -15.98888968998948812 ) ) ;
#98541 = CARTESIAN_POINT ( 'NONE',  ( 81.21353692635089772, 42.35982027868730171, -7.518915552659992230 ) ) ;
#98542 = ORIENTED_EDGE ( 'NONE', *, *, #5709, .F. ) ;
#98543 = ORIENTED_EDGE ( 'NONE', *, *, #96274, .F. ) ;
#98544 = CARTESIAN_POINT ( 'NONE',  ( 88.25809008468522165, 43.73205518618092214, 0.2003341539982119168 ) ) ;
#98545 = VERTEX_POINT ( 'NONE', #95682 ) ;
#98546 = DIRECTION ( 'NONE',  ( -0.8660254037844387076, -0.4999999999999998890, -0.000000000000000000 ) ) ;
#98548 = EDGE_CURVE ( 'NONE', #75611, #104, #97408, .T. ) ;
#98547 = VERTEX_POINT ( 'NONE', #26229 ) ;
#98549 = CARTESIAN_POINT ( 'NONE',  ( 75.58424500764920140, 61.59228886874195297, 15.33674465601570169 ) ) ;
#98550 = CARTESIAN_POINT ( 'NONE',  ( 87.89265348834460667, 45.03651295921149256, 6.473805411810645616 ) ) ;
#98551 = ORIENTED_EDGE ( 'NONE', *, *, #64559, .T. ) ;
#98552 = CARTESIAN_POINT ( 'NONE',  ( 207.2631600302859738, 271.6566716207027525, -6.785208696633175940 ) ) ;
#98553 = PLANE ( 'NONE',  #25538 ) ;
#98554 = AXIS2_PLACEMENT_3D ( 'NONE', #64550, #17443, #2262 ) ;
#98556 = EDGE_CURVE ( 'NONE', #14427, #89858, #13039, .T. ) ;
#98555 = DIRECTION ( 'NONE',  ( -0.8660254037844387076, -0.4999999999999998890, -0.000000000000000000 ) ) ;
#98557 = CARTESIAN_POINT ( 'NONE',  ( 199.4720805209845196, 266.1420231043892954, 4.760232788326643316 ) ) ;
#98559 = CARTESIAN_POINT ( 'NONE',  ( 82.83063800212752881, 53.40025595410719461, -15.30243353670389261 ) ) ;
#98558 = VECTOR ( 'NONE', #64494, 1000.000000000000000 ) ;
#98560 = CARTESIAN_POINT ( 'NONE',  ( 195.6062856355109432, 291.8469703299019216, -17.24264465766131593 ) ) ;
#98561 = ORIENTED_EDGE ( 'NONE', *, *, #85203, .T. ) ;
#98562 = CYLINDRICAL_SURFACE ( 'NONE', #14016, 10.00000000000010658 ) ;
#98563 = CARTESIAN_POINT ( 'NONE',  ( 8.860943796042899834, 20.51421378149916919, -9.188101187500004485 ) ) ;
#98564 = AXIS2_PLACEMENT_3D ( 'NONE', #49591, #3995, #3030 ) ;
#98565 = EDGE_LOOP ( 'NONE', ( #96042, #4695, #47346, #76167 ) ) ;
#98566 = CARTESIAN_POINT ( 'NONE',  ( 167.0583404026868948, 284.2888315039880354, 9.398654938006481885 ) ) ;
#98567 = AXIS2_PLACEMENT_3D ( 'NONE', #12233, #57808, #11250 ) ;
#98569 = ORIENTED_EDGE ( 'NONE', *, *, #72669, .T. ) ;
#98568 = CARTESIAN_POINT ( 'NONE',  ( 206.7927593038066618, 270.4714295788825780, 5.070506503021109168 ) ) ;
#98570 = CARTESIAN_POINT ( 'NONE',  ( 202.2576150004249200, 280.3265299319959354, 16.24828394350762295 ) ) ;
#98571 = CARTESIAN_POINT ( 'NONE',  ( 188.4457029989130490, 260.4214235001608131, 2.263077359424293444 ) ) ;
#98572 = CARTESIAN_POINT ( 'NONE',  ( 152.2916497645251184, 277.1968680821945554, -5.228018422121015973 ) ) ;
#98573 = CARTESIAN_POINT ( 'NONE',  ( 66.60661563016273590, 67.77273566365288104, -7.043189648870077590 ) ) ;
#98574 = CARTESIAN_POINT ( 'NONE',  ( 40.96864935082037817, 128.0650415295850735, -10.00000000000000888 ) ) ;
#98575 = CARTESIAN_POINT ( 'NONE',  ( 84.34251726751226386, 42.03111163911867720, 1.049105841315436827 ) ) ;
#98576 = CARTESIAN_POINT ( 'NONE',  ( 194.4679394788272475, 262.6816651586079843, -0.8071362648469233569 ) ) ;
#98577 = AXIS2_PLACEMENT_3D ( 'NONE', #39331, #17047, #8457 ) ;
#98578 = ORIENTED_EDGE ( 'NONE', *, *, #83687, .F. ) ;
#98579 = CARTESIAN_POINT ( 'NONE',  ( 155.4639880231617042, 261.3754693270417420, -18.58538060562953120 ) ) ;
#98580 = CARTESIAN_POINT ( 'NONE',  ( 74.93756780616698165, 67.42216207915812731, -12.80861374294490140 ) ) ;
#98581 = ORIENTED_EDGE ( 'NONE', *, *, #56796, .F. ) ;
#98582 = CARTESIAN_POINT ( 'NONE',  ( 4.352251933111777049, 179.9865022471903160, -10.00000000000009592 ) ) ;
#98583 = CARTESIAN_POINT ( 'NONE',  ( -8.728340106763610606, 175.7677522451419350, -5.000000000000047962 ) ) ;
#98584 = CARTESIAN_POINT ( 'NONE',  ( 194.9646308670422172, 268.7998031773939260, -10.80984512674310416 ) ) ;
#98585 = CARTESIAN_POINT ( 'NONE',  ( 171.5476497511431830, 279.6901843683210132, -14.62984903706609963 ) ) ;
#98586 = CARTESIAN_POINT ( 'NONE',  ( 203.5086680611402983, 278.1596424678725157, -14.69722159556002872 ) ) ;
#98587 = CARTESIAN_POINT ( 'NONE',  ( 167.2900023830132170, 283.1360949131732809, -11.47530909209802275 ) ) ;
#98588 = CARTESIAN_POINT ( 'NONE',  ( 162.8049643890749962, 273.4538889149586680, 14.88131869267027874 ) ) ;
#98590 = CARTESIAN_POINT ( 'NONE',  ( 33.48063555417975579, 19.73415679381824006, -6.890680421881970419E-14 ) ) ;
#98589 = CARTESIAN_POINT ( 'NONE',  ( 1.204062292545672097, 165.3768266524159856, 9.188101187500098632 ) ) ;
#98591 = CARTESIAN_POINT ( 'NONE',  ( 185.0690397135245746, 295.5174023956343490, 8.503999811686171029 ) ) ;
#98592 = EDGE_LOOP ( 'NONE', ( #56119, #6371, #60996, #9316 ) ) ;
#98593 = B_SPLINE_SURFACE_WITH_KNOTS ( 'NONE', 3, 1, ( 
 ( #34633, #96481 ),
 ( #59403, #4748 ),
 ( #3754, #97947 ),
 ( #35631, #82285 ),
 ( #58421, #12858 ),
 ( #49345, #89397 ),
 ( #19948, #81281 ),
 ( #88405, #41728 ),
 ( #88913, #27049 ),
 ( #80285, #10853 ),
 ( #72673, #50824 ),
 ( #57426, #74156 ),
 ( #66533, #97459 ),
 ( #34150, #11855 ),
 ( #51317, #18961 ),
 ( #49839, #11373 ),
 ( #42224, #65042 ),
 ( #95991, #26552 ),
 ( #35127, #89872 ),
 ( #28027, #73162 ),
 ( #19473, #73647 ),
 ( #42712, #4227 ),
 ( #66037, #81774 ),
 ( #12348, #43213 ),
 ( #46196, #99439 ),
 ( #36613, #38609 ),
 ( #60901, #53312 ),
 ( #61901, #60400 ),
 ( #29528, #20957 ),
 ( #91864, #91356 ),
 ( #92361, #6221 ),
 ( #84267, #31011 ),
 ( #75635, #37117 ),
 ( #14814, #7211 ) ),
 .UNSPECIFIED., .T., .F., .F.,
 ( 4, 2, 2, 2, 2, 2, 2, 2, 2, 2, 2, 2, 2, 2, 2, 2, 4 ),
 ( 2, 2 ),
 ( 0.000000000000000000, 0.06250000000000000000, 0.1250000000000000000, 0.1875000000000000000, 0.2500000000000000000, 0.3125000000000000000, 0.3750000000000000000, 0.4375000000000000000, 0.5000000000000000000, 0.5625000000000000000, 0.6250000000000000000, 0.6875000000000000000, 0.7500000000000000000, 0.8125000000000000000, 0.8750000000000000000, 0.9375000000000000000, 1.000000000000000000 ),
 ( 0.000000000000000000, 1.000000000000000000 ),
 .UNSPECIFIED. ) ;
#98594 = ORIENTED_EDGE ( 'NONE', *, *, #51965, .F. ) ;
#98595 = CARTESIAN_POINT ( 'NONE',  ( 0.000000000000000000, 0.000000000000000000, 36.50000000000000000 ) ) ;
#98596 = CARTESIAN_POINT ( 'NONE',  ( -33.12036098009135543, 24.37273002035946590, 177.5919119679930134 ) ) ;
#98597 = EDGE_CURVE ( 'NONE', #32823, #42173, #21136, .T. ) ;
#98598 = CARTESIAN_POINT ( 'NONE',  ( 171.6388997907716316, 289.6077812978417683, 2.686983444171377577 ) ) ;
#98599 = DIRECTION ( 'NONE',  ( -0.3177184104407523857, 0.9481851146622171100, 0.000000000000000000 ) ) ;
#98600 = DIRECTION ( 'NONE',  ( -0.8660254037844387076, -0.4999999999999998890, -0.000000000000000000 ) ) ;
#98601 = CARTESIAN_POINT ( 'NONE',  ( 152.1649379268514792, 277.7140263207647308, 3.704665498480741004 ) ) ;
#98602 = B_SPLINE_CURVE_WITH_KNOTS ( 'NONE', 3,
 ( #94744, #11135, #87691, #11627, #4009, #88671, #72440, #12115, #3046, #34893, #10117, #79560, #81064, #33933, #56708, #25832, #40982, #73917, #96250, #2531, #80557, #33413, #18223, #49117, #80054, #50595, #26813, #42487, #58202, #73422, #57695, #89180, #64819, #42978, #95766, #81545, #10621, #32902, #63811, #59690, #20218, #67296, #75417, #35898, #51088, #90659, #6510, #44487 ),
 .UNSPECIFIED., .F., .F.,
 ( 4, 2, 2, 2, 2, 2, 2, 2, 2, 2, 2, 2, 2, 2, 2, 2, 2, 2, 2, 2, 2, 2, 2, 4 ),
 ( 0.0003268706731840239797, 0.001346441947956916827, 0.001856227585343372954, 0.002111120404036600801, 0.002238566813383220146, 0.002366013222729838623, 0.002620906041422961519, 0.002875798860116085282, 0.003385584497502390922, 0.004405155772275003503, 0.005424727047047616518, 0.005934512684433878790, 0.006189405503127002987, 0.006444298321820127184, 0.006508021526493336026, 0.006571744731166544000, 0.006635467935839751974, 0.006699191140512959948, 0.006954083959205918479, 0.007463869596591793040, 0.007718762415284729887, 0.007973655233977666734, 0.008228548052670604449, 0.008483440871363540428 ),
 .UNSPECIFIED. ) ;
#98603 = CARTESIAN_POINT ( 'NONE',  ( 26.45420224557697608, 176.8923013555409796, 4.594050593750050204 ) ) ;
#98604 = CARTESIAN_POINT ( 'NONE',  ( 117.8466853168797428, 238.8458772461660544, 9.188101187500095079 ) ) ;
#98605 = CARTESIAN_POINT ( 'NONE',  ( -19.42194755839791753, 24.31068691715150010, 10.00000000000000000 ) ) ;
#98606 = LINE ( 'NONE', #61556, #60862 ) ;
#98607 = EDGE_CURVE ( 'NONE', #55413, #29620, #74346, .T. ) ;
#98608 = CARTESIAN_POINT ( 'NONE',  ( 206.2998527406910512, 271.9071720711702369, -8.006848967205936418 ) ) ;
#98609 = EDGE_CURVE ( 'NONE', #84087, #11048, #82897, .T. ) ;
#98610 = CARTESIAN_POINT ( 'NONE',  ( 175.3896052792100306, 281.5987068202503565, -14.18719490586176235 ) ) ;
#98611 = CARTESIAN_POINT ( 'NONE',  ( 38.72117548675866061, 22.75978393459168103, -1.583844403245396437 ) ) ;
#98612 = CARTESIAN_POINT ( 'NONE',  ( -38.55282132941486140, 44.90941061628357289, 59.99999999999999289 ) ) ;
#98613 = CARTESIAN_POINT ( 'NONE',  ( -17.42236680055705023, 149.2012482093457777, 0.000000000000000000 ) ) ;
#98614 = CARTESIAN_POINT ( 'NONE',  ( -19.54314961412049811, 92.97549661224779527, 59.99999999999999289 ) ) ;
#98615 = DIRECTION ( 'NONE',  ( -0.000000000000000000, 0.000000000000000000, 1.000000000000000000 ) ) ;
#98616 = CARTESIAN_POINT ( 'NONE',  ( 84.49275162666286576, 50.19829916693547744, 13.87667126673719231 ) ) ;
#98617 = CARTESIAN_POINT ( 'NONE',  ( 187.4789422952534892, 298.9514069382850039, -0.5906970195174623406 ) ) ;
#98618 = CARTESIAN_POINT ( 'NONE',  ( 46.99867368304095550, 76.19044720721625197, 10.00000000000000000 ) ) ;
#98619 = CARTESIAN_POINT ( 'NONE',  ( 164.7195526368693947, 253.2027545570438178, -12.99489340351435551 ) ) ;
#98620 = B_SPLINE_CURVE_WITH_KNOTS ( 'NONE', 3,
 ( #1619, #93331, #32504, #24889 ),
 .UNSPECIFIED., .F., .F.,
 ( 4, 4 ),
 ( 0.02660023401806649312, 0.03583121442840941917 ),
 .UNSPECIFIED. ) ;
#98621 = DIRECTION ( 'NONE',  ( -0.000000000000000000, -0.000000000000000000, 1.000000000000000000 ) ) ;
#98622 = DIRECTION ( 'NONE',  ( -0.8660254037844378194, -0.5000000000000014433, -0.000000000000000000 ) ) ;
#98623 = CARTESIAN_POINT ( 'NONE',  ( 101.1217432541752856, 223.0643266524159571, -9.188101187500093303 ) ) ;
#98624 = CARTESIAN_POINT ( 'NONE',  ( 7.453652514893187586, 19.70171378149916919, -9.188101187500004485 ) ) ;
#98625 = CARTESIAN_POINT ( 'NONE',  ( 67.63254175845027305, 65.87441213026522746, 10.48036353779758123 ) ) ;
#98626 = AXIS2_PLACEMENT_3D ( 'NONE', #2851, #11451, #42306 ) ;
#98627 = DIRECTION ( 'NONE',  ( -0.8660254037844387076, -0.4999999999999998890, -0.000000000000000000 ) ) ;
#98629 = CARTESIAN_POINT ( 'NONE',  ( 200.4404104491965768, 283.4740205424688497, 17.49842356273781263 ) ) ;
#98628 = CARTESIAN_POINT ( 'NONE',  ( 157.7529601300917363, 257.4108533407307959, 16.91445305439664892 ) ) ;
#98630 = CARTESIAN_POINT ( 'NONE',  ( 203.7909709648339458, 272.4802963485253713, -9.740038563755955892 ) ) ;
#98631 = CARTESIAN_POINT ( 'NONE',  ( 76.06516313603486878, 65.42396348981594656, 14.39793886682781832 ) ) ;
#98632 = CARTESIAN_POINT ( 'NONE',  ( 173.5499876061905979, 267.4222840943004940, -16.96674921312246198 ) ) ;
#98633 = CARTESIAN_POINT ( 'NONE',  ( 40.42214693012152793, 25.19860640527295104, 2.839279412974134775 ) ) ;
#98634 = CARTESIAN_POINT ( 'NONE',  ( 147.3715240516018810, 275.3920280842035595, -3.728968767617475866 ) ) ;
#98635 = DIRECTION ( 'NONE',  ( -0.8660254037844378194, -0.5000000000000013323, -0.000000000000000000 ) ) ;
#98636 = ORIENTED_EDGE ( 'NONE', *, *, #19298, .T. ) ;
#98637 = CARTESIAN_POINT ( 'NONE',  ( 19.57800816787531417, 26.70171378149919050, -9.188101187500004485 ) ) ;
#98638 = LINE ( 'NONE', #36301, #28057 ) ;
#98639 = CARTESIAN_POINT ( 'NONE',  ( 192.4867975473904949, 297.2500821921321972, -13.04960750009181325 ) ) ;
#98640 = DIRECTION ( 'NONE',  ( 0.6879669212057208938, 0.7257420446182799578, 0.000000000000000000 ) ) ;
#98641 = CARTESIAN_POINT ( 'NONE',  ( 70.37850334050121148, 61.05907127409049906, 14.36771776055900496 ) ) ;
#98642 = DIRECTION ( 'NONE',  ( 0.000000000000000000, -0.000000000000000000, 1.000000000000000000 ) ) ;
#98643 = CARTESIAN_POINT ( 'NONE',  ( 157.5879965179223916, 268.7330653384368588, 15.67728094257759786 ) ) ;
#98644 = LINE ( 'NONE', #29228, #66306 ) ;
#98645 = VECTOR ( 'NONE', #10671, 1000.000000000000114 ) ;
#98646 = CARTESIAN_POINT ( 'NONE',  ( 142.0502911348375221, 259.4865022471902876, -10.00000000000009415 ) ) ;
#98647 = VERTEX_POINT ( 'NONE', #42401 ) ;
#98648 = CARTESIAN_POINT ( 'NONE',  ( 72.97386446981147401, 70.68132344495337804, 8.316175787459499702 ) ) ;
#98649 = EDGE_LOOP ( 'NONE', ( #61852, #86761, #55326, #71246 ) ) ;
#98650 = CARTESIAN_POINT ( 'NONE',  ( 163.1008115941903895, 248.1481028935802442, 11.25332017433677834 ) ) ;
#98651 = CARTESIAN_POINT ( 'NONE',  ( 66.06293672572081732, 68.52299781147171132, 4.587403909294850202 ) ) ;
#98652 = ORIENTED_EDGE ( 'NONE', *, *, #80993, .T. ) ;
#98653 = CARTESIAN_POINT ( 'NONE',  ( 87.37689300401315506, 44.00708636583175348, 3.108306139222640319 ) ) ;
#98654 = ORIENTED_EDGE ( 'NONE', *, *, #61510, .F. ) ;
#98655 = FACE_OUTER_BOUND ( 'NONE', #34420, .T. ) ;
#98656 = CARTESIAN_POINT ( 'NONE',  ( 158.4451082418582359, 256.2120176447879203, 16.27803009664086176 ) ) ;
#98657 = CARTESIAN_POINT ( 'NONE',  ( 190.5362692644993672, 278.6201753252890967, -16.51120110810393982 ) ) ;
#98658 = CARTESIAN_POINT ( 'NONE',  ( 88.19119485691749105, 44.51220553762047416, -4.804906155116621669 ) ) ;
#98659 = CARTESIAN_POINT ( 'NONE',  ( 200.7484899876179441, 282.9404111291507888, -16.88964748465601673 ) ) ;
#98660 = VECTOR ( 'NONE', #59596, 999.9999999999998863 ) ;
#98661 = PLANE ( 'NONE',  #56104 ) ;
#98662 = EDGE_CURVE ( 'NONE', #40485, #52219, #56692, .T. ) ;
#98663 = CARTESIAN_POINT ( 'NONE',  ( 36.06377727768690988, 41.79752408145595410, -5.678558825948271327 ) ) ;
#98664 = CARTESIAN_POINT ( 'NONE',  ( 75.45938151893163592, 59.84466625416695251, -15.73511245645754464 ) ) ;
#98665 = EDGE_CURVE ( 'NONE', #59818, #63171, #77309, .T. ) ;
#98666 = CARTESIAN_POINT ( 'NONE',  ( 165.3709094149136263, 274.8634007614296593, 14.74939627246788554 ) ) ;
#98667 = CARTESIAN_POINT ( 'NONE',  ( -6.542761065016642341, 25.57183462804972507, -10.00000000000000000 ) ) ;
#98668 = VERTEX_POINT ( 'NONE', #15484 ) ;
#98669 = ORIENTED_EDGE ( 'NONE', *, *, #69275, .T. ) ;
#98670 = CARTESIAN_POINT ( 'NONE',  ( 72.04618005861752295, 72.23985218540053665, -1.584352113898356951 ) ) ;
#98671 = CARTESIAN_POINT ( 'NONE',  ( 87.23257741107988750, 46.04474800944700519, -8.789869334516776433 ) ) ;
#98673 = CARTESIAN_POINT ( 'NONE',  ( 165.9041802389429563, 274.0587237628353137, -15.17960966916681365 ) ) ;
#98672 = CARTESIAN_POINT ( 'NONE',  ( 174.2444115436975665, 257.3183303361469143, -11.90217922001411743 ) ) ;
#98674 = CARTESIAN_POINT ( 'NONE',  ( 206.4738852556816369, 273.0237356314501085, -9.746110091792012042 ) ) ;
#98675 = CARTESIAN_POINT ( 'NONE',  ( 197.4417221320944122, 273.1026795264489238, -13.30033383848224204 ) ) ;
#98676 = CARTESIAN_POINT ( 'NONE',  ( 73.61711655523605202, 61.23855026575265725, -15.07042752294893617 ) ) ;
#98677 = CARTESIAN_POINT ( 'NONE',  ( 82.21611827071926371, 40.83382032456969313, 1.069328909644415848 ) ) ;
#98679 = ADVANCED_FACE ( 'NONE', ( #76327 ), #29708, .T. ) ;
#98678 = PLANE ( 'NONE',  #81895 ) ;
#98680 = CARTESIAN_POINT ( 'NONE',  ( 77.28420460057618868, 63.06679313565820166, -15.26332939213814655 ) ) ;
#98681 = CARTESIAN_POINT ( 'NONE',  ( 78.86792953187128319, 59.60067377931095933, 16.50582274385373083 ) ) ;
#98682 = CARTESIAN_POINT ( 'NONE',  ( 118.6048046409561465, 227.0327760586659451, 1.948934522072303157E-15 ) ) ;
#98683 = VERTEX_POINT ( 'NONE', #60585 ) ;
#98684 = CARTESIAN_POINT ( 'NONE',  ( 70.81316579126399802, 61.41551742065354347, -14.85192641751565468 ) ) ;
#98685 = CARTESIAN_POINT ( 'NONE',  ( 36.80649086932150027, 23.11110640527294535, -2.839279412974138328 ) ) ;
#98686 = CARTESIAN_POINT ( 'NONE',  ( 191.9871034619986574, 275.2958097524751224, 16.51095949440587418 ) ) ;
#98687 = ORIENTED_EDGE ( 'NONE', *, *, #1085, .F. ) ;
#98688 = CARTESIAN_POINT ( 'NONE',  ( 164.0123586716512705, 248.3359725020313533, -9.617851509444742319 ) ) ;
#98689 = EDGE_CURVE ( 'NONE', #61758, #85319, #100125, .T. ) ;
#98690 = CARTESIAN_POINT ( 'NONE',  ( 35.19234511847571412, 113.9167680888089080, 59.99999999999999289 ) ) ;
#98691 = CARTESIAN_POINT ( 'NONE',  ( 157.7861133721078772, 257.3534302411229646, 18.03837896619386783 ) ) ;
#98692 = CARTESIAN_POINT ( 'NONE',  ( 206.5237403681858552, 272.9373840435757188, -10.81420335655575116 ) ) ;
#98693 = CARTESIAN_POINT ( 'NONE',  ( 13.31457613402888995, 31.18528772668516424, -1.583844403245363575 ) ) ;
#98694 = ADVANCED_FACE ( 'NONE', ( #99126 ), #73448, .F. ) ;
#98695 = ORIENTED_EDGE ( 'NONE', *, *, #78407, .T. ) ;
#98696 = CARTESIAN_POINT ( 'NONE',  ( 195.2812657889309662, 292.4099212176463425, 15.19213940613456337 ) ) ;
#98697 = EDGE_LOOP ( 'NONE', ( #14906, #76308, #66123, #44314 ) ) ;
#98698 = CARTESIAN_POINT ( 'NONE',  ( 32.30839531297598910, 123.0650415295850593, 10.00000000000000888 ) ) ;
#98699 = EDGE_LOOP ( 'NONE', ( #76459, #79250, #17438, #62726, #64903, #66232, #12919, #49913, #84639, #93940, #20683, #52270, #20925, #27688, #54295, #11733, #51350, #94461, #48004, #21514 ) ) ;
#98700 = VECTOR ( 'NONE', #95972, 1000.000000000000000 ) ;
#98701 = FACE_OUTER_BOUND ( 'NONE', #95955, .T. ) ;
#98702 = CARTESIAN_POINT ( 'NONE',  ( 186.1263547150109900, 286.8862237501084564, -16.18252752151998308 ) ) ;
#98703 = CARTESIAN_POINT ( 'NONE',  ( 82.85927426857082878, 45.93892428374152814, 10.86312220312391830 ) ) ;
#98705 = CARTESIAN_POINT ( 'NONE',  ( -22.42236680055709641, 157.8615022471902591, 0.000000000000000000 ) ) ;
#98704 = CARTESIAN_POINT ( 'NONE',  ( -49.59353317285164309, 78.63960484736190892, -10.00000000000000000 ) ) ;
#98706 = CARTESIAN_POINT ( 'NONE',  ( 201.1679199471075492, 282.2139371290980989, -16.62385308864941535 ) ) ;
#98707 = ORIENTED_EDGE ( 'NONE', *, *, #28259, .F. ) ;
#98708 = CARTESIAN_POINT ( 'NONE',  ( 157.4243923570103050, 257.9799494174374104, 18.06359219958597606 ) ) ;
#98709 = PLANE ( 'NONE',  #64293 ) ;
#98710 = ADVANCED_FACE ( 'NONE', ( #33076 ), #63969, .F. ) ;
#98711 = CARTESIAN_POINT ( 'NONE',  ( 189.5599828453989346, 263.0657735508838186, -9.804501003715218488 ) ) ;
#98712 = CARTESIAN_POINT ( 'NONE',  ( 173.5113001039477751, 251.2546712883042517, -0.9897563821454024025 ) ) ;
#98713 = CARTESIAN_POINT ( 'NONE',  ( 189.0912321849916111, 270.0745130361697193, -14.07025751438627381 ) ) ;
#98714 = CARTESIAN_POINT ( 'NONE',  ( 72.15865790475056940, 72.27389710013802926, 3.820985825366547406 ) ) ;
#98715 = DIRECTION ( 'NONE',  ( 0.9724945078367536189, 0.2329258084183680466, 0.000000000000000000 ) ) ;
#98716 = CARTESIAN_POINT ( 'NONE',  ( 147.6095992045671323, 244.4824982072973967, 3.021315404115420679E-15 ) ) ;
#98717 = ADVANCED_FACE ( 'NONE', ( #11303 ), #18387, .F. ) ;
#98718 = CARTESIAN_POINT ( 'NONE',  ( 194.3252252352508265, 294.0658320307167628, 14.07225870721148731 ) ) ;
#98719 = CARTESIAN_POINT ( 'NONE',  ( 191.4382082719228322, 282.7680930013282250, -17.46921905594915003 ) ) ;
#98720 = CARTESIAN_POINT ( 'NONE',  ( 82.44310520575160695, 54.28011738120410001, -15.96781897959229113 ) ) ;
#98721 = CARTESIAN_POINT ( 'NONE',  ( 83.28711936893076029, 209.7048013555409796, 4.594050593750051981 ) ) ;
#98722 = CARTESIAN_POINT ( 'NONE',  ( 159.8597520197352537, 253.7617827468940277, -16.74905990210778839 ) ) ;
#98723 = DIRECTION ( 'NONE',  ( -3.977257660627182967E-15, 7.954515321254365934E-15, 1.000000000000000000 ) ) ;
#98724 = LINE ( 'NONE', #91625, #72197 ) ;
#98725 = EDGE_CURVE ( 'NONE', #82418, #91683, #1681, .T. ) ;
#98726 = CARTESIAN_POINT ( 'NONE',  ( -29.37075727991403440, 94.88921800892813962, 44.57229221387616036 ) ) ;
#98727 = EDGE_CURVE ( 'NONE', #53284, #19489, #21776, .T. ) ;
#98728 = EDGE_CURVE ( 'NONE', #94724, #81988, #11636, .T. ) ;
#98729 = CARTESIAN_POINT ( 'NONE',  ( 161.1747502674735415, 251.4841389699472529, -13.25152330924089839 ) ) ;
#98730 = CARTESIAN_POINT ( 'NONE',  ( 65.74726825304114186, 69.08659106095529978, 2.128305819671951817E-12 ) ) ;
#98731 = CARTESIAN_POINT ( 'NONE',  ( -20.78084767303474578, 95.21720048508885270, 45.19937752447436452 ) ) ;
#98732 = EDGE_CURVE ( 'NONE', #94434, #13291, #18893, .T. ) ;
#98733 = ADVANCED_FACE ( 'NONE', ( #25992 ), #82217, .T. ) ;
#98734 = CARTESIAN_POINT ( 'NONE',  ( 34.48165468218606833, 44.00034080476292786, -1.878358725466461243E-16 ) ) ;
#98735 = CARTESIAN_POINT ( 'NONE',  ( 149.7247407264208618, 272.0633196944937140, -11.44969454563192279 ) ) ;
#98736 =( BOUNDED_CURVE ( )  B_SPLINE_CURVE ( 2, ( #54984, #94034, #78810, #63088, #25082, #1804, #70687, #24584, #16981, #47872, #71213, #32688, #63589 ),
 .UNSPECIFIED., .F., .T. ) 
 B_SPLINE_CURVE_WITH_KNOTS ( ( 3, 2, 2, 2, 2, 2, 3 ),
 ( 0.5375000000000000888, 0.5400000000000000355, 0.5450000000000000400, 0.5500000000000000444, 0.5550000000000000488, 0.5600000000000000533, 0.5625000000000000000 ),
 .UNSPECIFIED. ) 
 CURVE ( )  GEOMETRIC_REPRESENTATION_ITEM ( )  RATIONAL_B_SPLINE_CURVE ( ( 0.9755282581475767101, 0.9755282581475772652, 1.000000000000000000, 0.9510565162951535312, 1.000000000000000000, 0.9510565162951535312, 1.000000000000000000, 0.9510565162951535312, 1.000000000000000000, 0.9510565162951535312, 1.000000000000000000, 0.9755282581475768211, 0.9755282581475768211 ) ) 
 REPRESENTATION_ITEM ( '' )  );
#98737 = CARTESIAN_POINT ( 'NONE',  ( 157.2464636617698375, 258.2881309577184652, 18.14284729738657731 ) ) ;
#98738 = CARTESIAN_POINT ( 'NONE',  ( 71.90028047037452552, 71.95896194932872447, 2.840402229763955066 ) ) ;
#98739 = CARTESIAN_POINT ( 'NONE',  ( 168.0185004389765595, 274.8492260674121326, -16.75068961788599609 ) ) ;
#98740 = CARTESIAN_POINT ( 'NONE',  ( 199.2580273620699813, 277.9411595627967699, 16.03392482410259845 ) ) ;
#98741 = CARTESIAN_POINT ( 'NONE',  ( 147.8163551302855296, 274.6215580551378821, -9.286329195885331345 ) ) ;
#98742 = CARTESIAN_POINT ( 'NONE',  ( 71.93703274728032682, 72.16823338693137657, -1.679264843172269650 ) ) ;
#98743 = CARTESIAN_POINT ( 'NONE',  ( 49.53858449761714411, 211.6589784336661637, -6.496448406907676862E-16 ) ) ;
#98744 = CARTESIAN_POINT ( 'NONE',  ( 26.45569963029868177, 20.98920272979927049, 7.433330006724137462 ) ) ;
#98745 = CARTESIAN_POINT ( 'NONE',  ( 171.3554945684980453, 286.6428740666748354, 7.414102809553750006 ) ) ;
#98746 = LINE ( 'NONE', #28826, #2212 ) ;
#98747 = CARTESIAN_POINT ( 'NONE',  ( 44.42076818640806835, 30.81029122506298634, 8.090169943749479842 ) ) ;
#98748 = CARTESIAN_POINT ( 'NONE',  ( 157.6921299354026189, 257.5162143285667753, -18.18720974599499840 ) ) ;
#98749 = CARTESIAN_POINT ( 'NONE',  ( 180.9962514683335257, 255.6518059654043782, 5.281628127585873855 ) ) ;
#98750 = CARTESIAN_POINT ( 'NONE',  ( 75.50150731818223448, 56.53949938707354050, 16.58547563118056090 ) ) ;
#98751 = CARTESIAN_POINT ( 'NONE',  ( 176.1626442602351403, 274.9078016565098892, 17.19964070129887546 ) ) ;
#98752 = CARTESIAN_POINT ( 'NONE',  ( 72.59582657278434681, 61.38205835117237541, 14.77812198616874895 ) ) ;
#98753 = CARTESIAN_POINT ( 'NONE',  ( 73.53566697132028196, 67.45690392929650159, -11.63657775242925929 ) ) ;
#98754 = CARTESIAN_POINT ( 'NONE',  ( 163.5147782259477083, 255.5762155980353896, -14.85420212278641117 ) ) ;
#98755 = LINE ( 'NONE', #59199, #28309 ) ;
#98756 = CARTESIAN_POINT ( 'NONE',  ( 88.35671610020233402, 228.4865022471903160, 10.00000000000009237 ) ) ;
#98757 = CARTESIAN_POINT ( 'NONE',  ( 161.1089126327036354, 251.5981730984191529, 13.95161017039218976 ) ) ;
#98758 = CARTESIAN_POINT ( 'NONE',  ( 165.2395056520857111, 269.6740676042253995, -16.28644685873352671 ) ) ;
#98759 = EDGE_LOOP ( 'NONE', ( #7598, #55506, #34858, #20400 ) ) ;
#98760 = CARTESIAN_POINT ( 'NONE',  ( 55.84441874286383722, 212.2369531367911293, -4.594050593750048428 ) ) ;
#98761 = ORIENTED_EDGE ( 'NONE', *, *, #51100, .T. ) ;
#98762 = CARTESIAN_POINT ( 'NONE',  ( 163.2151044353641680, 263.6560547264549541, 16.97092589136012108 ) ) ;
#98763 = CARTESIAN_POINT ( 'NONE',  ( 182.5291792280718823, 296.7636338796572204, 0.3805386115670883473 ) ) ;
#98765 = CARTESIAN_POINT ( 'NONE',  ( 204.9574235042572923, 272.8759434632493708, -10.91876598039351265 ) ) ;
#98764 = AXIS2_PLACEMENT_3D ( 'NONE', #37062, #83202, #21863 ) ;
#98766 = ORIENTED_EDGE ( 'NONE', *, *, #7196, .F. ) ;
#98768 = FACE_OUTER_BOUND ( 'NONE', #57552, .T. ) ;
#98767 = B_SPLINE_CURVE_WITH_KNOTS ( 'NONE', 3,
 ( #54559, #78915, #8002, #100210, #38877, #40367, #1401, #85022 ),
 .UNSPECIFIED., .F., .F.,
 ( 4, 2, 2, 4 ),
 ( 0.1555655374897298437, 0.5777827687448640059, 0.7888913843724321140, 1.000000000000000000 ),
 .UNSPECIFIED. ) ;
#98769 = CARTESIAN_POINT ( 'NONE',  ( 79.26966485285926467, 46.35457182308554280, -12.78027692334229748 ) ) ;
#98770 = CARTESIAN_POINT ( 'NONE',  ( 72.16589213194404806, 62.31695436414708666, 14.80019564645472840 ) ) ;
#98771 = CARTESIAN_POINT ( 'NONE',  ( 72.89831966083461623, 70.30981352087286496, -8.130391679937307714 ) ) ;
#98772 = CARTESIAN_POINT ( 'NONE',  ( -48.62867196056776464, 76.78809661315139579, -10.00000000000000000 ) ) ;
#98773 = CARTESIAN_POINT ( 'NONE',  ( 116.5487100721118026, 226.5494855054051584, -2.679491924311248496 ) ) ;
#98774 = ORIENTED_EDGE ( 'NONE', *, *, #31734, .T. ) ;
#98775 = CARTESIAN_POINT ( 'NONE',  ( 26.41418602390824333, 17.11110640527292759, -2.839279412974138328 ) ) ;
#98776 = CARTESIAN_POINT ( 'NONE',  ( 79.96602959028801649, 44.47270156346923642, 11.66712872020432457 ) ) ;
#98777 = CARTESIAN_POINT ( 'NONE',  ( 69.22385677126450787, 69.96866776554797696, -4.197617061747116907 ) ) ;
#98778 = DIRECTION ( 'NONE',  ( -0.8660254037844387076, -0.4999999999999998890, -0.000000000000000000 ) ) ;
#98779 = VERTEX_POINT ( 'NONE', #60826 ) ;
#98780 = CARTESIAN_POINT ( 'NONE',  ( 182.2841300395537871, 284.0799011696702223, 14.96127849592191161 ) ) ;
#98781 = CARTESIAN_POINT ( 'NONE',  ( 159.9788992190088948, 253.5554137441726255, -15.81862932303382330 ) ) ;
#98782 = ORIENTED_EDGE ( 'NONE', *, *, #39427, .T. ) ;
#98783 = AXIS2_PLACEMENT_3D ( 'NONE', #55670, #71414, #2516 ) ;
#98784 = ORIENTED_EDGE ( 'NONE', *, *, #98229, .T. ) ;
#98786 = DIRECTION ( 'NONE',  ( -0.8615733660689046669, -0.5076330711061851630, 0.000000000000000000 ) ) ;
#98785 = CARTESIAN_POINT ( 'NONE',  ( 72.46264091457396717, 68.04234003238872219, 11.10956356103667986 ) ) ;
#98787 = CARTESIAN_POINT ( 'NONE',  ( 207.7625791259561652, 270.7916523727319031, -1.015623356719550063 ) ) ;
#98788 = CARTESIAN_POINT ( 'NONE',  ( 204.3276935076901850, 276.7410487817560920, 13.46217427333259309 ) ) ;
#98789 = CARTESIAN_POINT ( 'NONE',  ( -13.42108286626701386, 23.34301056334149038, 10.00000000000000000 ) ) ;
#98790 = CYLINDRICAL_SURFACE ( 'NONE', #45156, 70.00000000000002842 ) ;
#98791 = CARTESIAN_POINT ( 'NONE',  ( 161.1500805419174469, 263.0475797279946164, -17.31870440403353228 ) ) ;
#98793 = EDGE_CURVE ( 'NONE', #32891, #89364, #78015, .T. ) ;
#98792 = CARTESIAN_POINT ( 'NONE',  ( 122.6094779419291712, 253.8464784336661353, 1.353441290958777525E-15 ) ) ;
#98794 = CARTESIAN_POINT ( 'NONE',  ( 76.27746593522670082, 214.8458772461660544, 9.188101187500095079 ) ) ;
#98795 = ORIENTED_EDGE ( 'NONE', *, *, #8469, .F. ) ;
#98796 = CARTESIAN_POINT ( 'NONE',  ( 170.3407533412963915, 263.8712159389925205, 15.90218549753505428 ) ) ;
#98797 = CARTESIAN_POINT ( 'NONE',  ( 128.2864073861747727, 233.3262482093457493, 3.021315404115420679E-15 ) ) ;
#98798 = ORIENTED_EDGE ( 'NONE', *, *, #62774, .F. ) ;
#98799 = B_SPLINE_CURVE_WITH_KNOTS ( 'NONE', 3,
 ( #75535, #6120, #37506, #37016, #98847, #52705, #60298, #67924, #29424, #21820, #74558, #83665, #14228, #36016, #66917, #76049 ),
 .UNSPECIFIED., .F., .F.,
 ( 4, 2, 2, 2, 2, 2, 2, 4 ),
 ( 0.001006769657979127586, 0.001259641240578331274, 0.001512512823177534962, 0.001765384405776738433, 0.002018255988375941903, 0.002271127570975146025, 0.002523999153574349279, 0.003029742318772843390 ),
 .UNSPECIFIED. ) ;
#98800 = CARTESIAN_POINT ( 'NONE',  ( 169.3971321688942169, 259.0209908423287288, 15.77637843574870224 ) ) ;
#98801 = VERTEX_POINT ( 'NONE', #21855 ) ;
#98802 = EDGE_LOOP ( 'NONE', ( #86443, #73956, #30250, #1143 ) ) ;
#98803 = CARTESIAN_POINT ( 'NONE',  ( 89.56554322277027325, 212.5177522451417929, 5.000000000000051514 ) ) ;
#98804 = CARTESIAN_POINT ( 'NONE',  ( 80.09302555852339367, 44.25273809412914261, -11.40411237053047167 ) ) ;
#98805 = CARTESIAN_POINT ( 'NONE',  ( 72.93609909127609114, 224.4637435831424739, 2.679491924311251605 ) ) ;
#98806 = ADVANCED_FACE ( 'NONE', ( #43141 ), #83699, .T. ) ;
#98807 = CARTESIAN_POINT ( 'NONE',  ( 85.76034556165906508, 42.63951191185048373, -3.229101607542598007 ) ) ;
#98808 = CARTESIAN_POINT ( 'NONE',  ( 109.3091660502225011, 245.4637435831425023, 2.679491924311251605 ) ) ;
#98809 = CARTESIAN_POINT ( 'NONE',  ( 194.1493756275458793, 294.3704124857528655, 13.94613522129020744 ) ) ;
#98810 = CARTESIAN_POINT ( 'NONE',  ( 70.74076148756792293, 64.84648076579460962, 12.32345133226214884 ) ) ;
#98811 = EDGE_CURVE ( 'NONE', #37839, #67744, #99372, .T. ) ;
#98812 = CARTESIAN_POINT ( 'NONE',  ( 182.9932251654942945, 257.3252772383810338, -6.270752636691518056 ) ) ;
#98813 = ORIENTED_EDGE ( 'NONE', *, *, #8161, .F. ) ;
#98814 = B_SPLINE_CURVE_WITH_KNOTS ( 'NONE', 3,
 ( #18686, #19696, #95733, #3974, #28263, #57159, #57659, #73880, #88639, #11097, #42941, #89626, #88140, #90108, #49569, #50073 ),
 .UNSPECIFIED., .F., .F.,
 ( 4, 2, 2, 2, 2, 2, 2, 4 ),
 ( 1.156196775494863067E-16, 0.0003787177898467221381, 0.0007574355796933285919, 0.001136153369539935317, 0.001514871159386541608, 0.001893588949233148116, 0.002272306739079755274, 0.003029742318773115308 ),
 .UNSPECIFIED. ) ;
#98815 = CARTESIAN_POINT ( 'NONE',  ( 161.8900357011995652, 250.2452282568197859, -12.82231662042267217 ) ) ;
#98816 = ORIENTED_EDGE ( 'NONE', *, *, #64436, .F. ) ;
#98817 = B_SPLINE_CURVE_WITH_KNOTS ( 'NONE', 3,
 ( #90419, #58455, #41765, #49874, #97979, #27085, #74196, #89428, #82325, #50859 ),
 .UNSPECIFIED., .F., .F.,
 ( 4, 2, 2, 2, 4 ),
 ( 0.000000000000000000, 0.2500000000000000000, 0.5000000000000000000, 0.7500000000000000000, 1.000000000000000000 ),
 .UNSPECIFIED. ) ;
#98818 = CARTESIAN_POINT ( 'NONE',  ( 163.7258651212256382, 261.0251292819381774, -16.78914756408816089 ) ) ;
#98819 = CARTESIAN_POINT ( 'NONE',  ( 81.82036482989325066, 42.35048943672428834, -7.944650131338358179 ) ) ;
#98820 = CARTESIAN_POINT ( 'NONE',  ( 206.4943150373521803, 272.9883502116088039, 11.34100825923693101 ) ) ;
#98821 = CARTESIAN_POINT ( 'NONE',  ( 157.6304115535352537, 270.8650229002738001, -16.00510772102553858 ) ) ;
#98822 = CARTESIAN_POINT ( 'NONE',  ( 142.6909626358283560, 247.0643266524159856, -9.188101187500093303 ) ) ;
#98823 = ORIENTED_EDGE ( 'NONE', *, *, #78443, .F. ) ;
#98824 = CARTESIAN_POINT ( 'NONE',  ( 88.18953256495667858, 44.42393962918851713, 4.547252263720217513 ) ) ;
#98825 = CARTESIAN_POINT ( 'NONE',  ( 72.86837948048784597, 67.33958022161600354, -11.94987273000593575 ) ) ;
#98826 = CARTESIAN_POINT ( 'NONE',  ( 41.82599275875796252, 62.29945068332010294, 10.00000000000000000 ) ) ;
#98827 = CARTESIAN_POINT ( 'NONE',  ( 148.9701624811553984, 277.3468434241520981, -1.218048504557616152 ) ) ;
#98828 = CARTESIAN_POINT ( 'NONE',  ( 74.75920290338640939, 66.43904096090548705, -12.97148193089175905 ) ) ;
#98829 = ORIENTED_EDGE ( 'NONE', *, *, #67909, .F. ) ;
#98830 = CARTESIAN_POINT ( 'NONE',  ( 206.7325995683429767, 270.5756292972641859, -5.459556455514786855 ) ) ;
#98831 = CARTESIAN_POINT ( 'NONE',  ( 185.4538201292061785, 277.6915352341014227, -16.99660624438589451 ) ) ;
#98832 = EDGE_CURVE ( 'NONE', #24657, #1218, #812, .T. ) ;
#98833 = DIRECTION ( 'NONE',  ( -0.000000000000000000, -0.000000000000000000, -1.000000000000000000 ) ) ;
#98834 = CARTESIAN_POINT ( 'NONE',  ( 72.59839265552557208, 71.34777361097565063, -5.944036940999890106 ) ) ;
#98835 = CARTESIAN_POINT ( 'NONE',  ( 81.34519720517472763, 53.17022275404438147, 15.42862813885395923 ) ) ;
#98836 = CARTESIAN_POINT ( 'NONE',  ( 202.6452040468594475, 267.4133178899479049, 0.8753174002111273611 ) ) ;
#98837 = EDGE_CURVE ( 'NONE', #77239, #93313, #5658, .T. ) ;
#98838 = CARTESIAN_POINT ( 'NONE',  ( 190.9559560067148425, 299.9015775189195665, -4.895152914295826108 ) ) ;
#98839 = EDGE_CURVE ( 'NONE', #31470, #82130, #83953, .T. ) ;
#98840 = CARTESIAN_POINT ( 'NONE',  ( 72.04834849415195208, 72.28436413801230742, -0.8995985284803106330 ) ) ;
#98841 = CARTESIAN_POINT ( 'NONE',  ( 205.1793861064249711, 275.2658739283173759, -14.08953480709093675 ) ) ;
#98842 = CARTESIAN_POINT ( 'NONE',  ( 196.3021051436114135, 270.7336484030830093, 11.92689920574754581 ) ) ;
#98843 = EDGE_CURVE ( 'NONE', #30467, #60494, #57549, .T. ) ;
#98844 = EDGE_CURVE ( 'NONE', #1717, #23755, #33329, .T. ) ;
#98845 = CARTESIAN_POINT ( 'NONE',  ( 19.72404941274043466, 33.16126292948894871, -6.180339887498951690 ) ) ;
#98846 = FACE_OUTER_BOUND ( 'NONE', #32565, .T. ) ;
#98847 = CARTESIAN_POINT ( 'NONE',  ( 205.4355683657304326, 274.4353959702803536, 11.00905889885928879 ) ) ;
#98848 = CARTESIAN_POINT ( 'NONE',  ( 71.98367679655076756, 69.26045741849536341, -9.475566133687880921 ) ) ;
#98849 = CARTESIAN_POINT ( 'NONE',  ( 159.9671766634011192, 253.5757178060795809, 16.49140845334465411 ) ) ;
#98850 = AXIS2_PLACEMENT_3D ( 'NONE', #86856, #78710, #17388 ) ;
#98851 = CARTESIAN_POINT ( 'NONE',  ( 72.11651558246516913, 71.81869578167429324, -3.920535044530327529 ) ) ;
#98852 = CARTESIAN_POINT ( 'NONE',  ( 148.4552706801120507, 256.5177522451418213, -10.00000000000009592 ) ) ;
#98853 = CARTESIAN_POINT ( 'NONE',  ( 174.7421405500457752, 284.6308697351560681, -12.06511137246073417 ) ) ;
#98854 = ORIENTED_EDGE ( 'NONE', *, *, #34831, .F. ) ;
#98855 = CARTESIAN_POINT ( 'NONE',  ( 66.64741794046514656, 68.07194284811899365, -6.509155038794735226 ) ) ;
#98856 = CARTESIAN_POINT ( 'NONE',  ( 72.47494455774663891, 70.67364856651921912, -7.881577117668181032 ) ) ;
#98857 = CARTESIAN_POINT ( 'NONE',  ( 202.5051313019488646, 273.9765361377286581, -13.12135839583134000 ) ) ;
#98858 = CARTESIAN_POINT ( 'NONE',  ( 151.3681950933278983, 268.4695907787949523, -15.50699599486383917 ) ) ;
#98859 = CARTESIAN_POINT ( 'NONE',  ( 9.864316330390064280, 170.3768266524159856, -9.188101187500093303 ) ) ;
#98860 = CARTESIAN_POINT ( 'NONE',  ( 22.08843299157899764, 31.49103043416549852, -8.090169943749479842 ) ) ;
#98861 = CARTESIAN_POINT ( 'NONE',  ( 85.33961507832758286, 48.52663690637297123, 12.44665103731247235 ) ) ;
#98862 = CARTESIAN_POINT ( 'NONE',  ( 204.8878784573704195, 275.7707799872745795, -14.13380496213581594 ) ) ;
#98863 = CARTESIAN_POINT ( 'NONE',  ( 78.00798602660121617, 154.0685146834693171, 4.041334437186263538E-16 ) ) ;
#98864 = LINE ( 'NONE', #98363, #83150 ) ;
#98865 = DIRECTION ( 'NONE',  ( -0.8660254037844359321, -0.5000000000000051070, -0.000000000000000000 ) ) ;
#98866 = CARTESIAN_POINT ( 'NONE',  ( 150.7576929667484080, 269.5270114801595582, 13.75028158740543205 ) ) ;
#98867 = CARTESIAN_POINT ( 'NONE',  ( 57.68498304950349365, 204.1115022471902591, 10.00000000000009592 ) ) ;
#98868 = CARTESIAN_POINT ( 'NONE',  ( 81.81922014299045998, 41.23558842254242052, 5.835146561875444782 ) ) ;
#98869 = CARTESIAN_POINT ( 'NONE',  ( 190.1063449786324213, 301.3731469862293011, 0.2163967485516588019 ) ) ;
#98870 = CARTESIAN_POINT ( 'NONE',  ( 7.969365115964081703, 187.6589784336661637, -6.496448406907675876E-16 ) ) ;
#98871 = CARTESIAN_POINT ( 'NONE',  ( 164.5437530064905332, 284.7883962438557433, 4.221428904827313033 ) ) ;
#98872 = EDGE_CURVE ( 'NONE', #36590, #24906, #59332, .T. ) ;
#98873 = CARTESIAN_POINT ( 'NONE',  ( 152.9489295551198893, 265.7316783776963121, 17.71675637597311237 ) ) ;
#98874 = CARTESIAN_POINT ( 'NONE',  ( 34.28181963472369631, 41.83396525600392835, -2.839279412974133887 ) ) ;
#98875 = DIRECTION ( 'NONE',  ( -0.8218955677251095215, -0.5696381972391070247, 0.000000000000000000 ) ) ;
#98876 = CARTESIAN_POINT ( 'NONE',  ( 48.98810889288134263, 89.24608170897542436, 10.00000000000000000 ) ) ;
#98877 = FACE_OUTER_BOUND ( 'NONE', #96959, .T. ) ;
#98878 = CARTESIAN_POINT ( 'NONE',  ( 173.2106840999569215, 256.4575935151219710, 12.77520126633179487 ) ) ;
#98879 = CARTESIAN_POINT ( 'NONE',  ( 163.5517623707881398, 281.2794412073851049, 8.859983951043487238 ) ) ;
#98880 = CARTESIAN_POINT ( 'NONE',  ( 19.64056747690256088, 19.84335787977763133, 9.188101187500006262 ) ) ;
#98881 = CARTESIAN_POINT ( 'NONE',  ( 189.8480911035503880, 301.8204558191226283, -0.8992086515915015399 ) ) ;
#98882 = CARTESIAN_POINT ( 'NONE',  ( 71.77793909028444830, 59.04410539788438683, 15.36942587551596695 ) ) ;
#98883 = CARTESIAN_POINT ( 'NONE',  ( 155.3017250444513024, 261.6565170503553190, 18.58368563027307374 ) ) ;
#98884 = VERTEX_POINT ( 'NONE', #52251 ) ;
#98885 = CARTESIAN_POINT ( 'NONE',  ( 185.4369573720926496, 290.9562819449305380, 12.20735569394162923 ) ) ;
#98886 = CARTESIAN_POINT ( 'NONE',  ( 179.0484917649878298, 259.9789987921100192, 12.89662402083353854 ) ) ;
#98887 = B_SPLINE_CURVE_WITH_KNOTS ( 'NONE', 3,
 ( #50184, #11704, #90734, #58277, #83115, #75493, #8571, #22770, #93193, #85619, #14670, #85099, #15141, #84119, #6576, #61249, #31844, #46543, #38447, #53164 ),
 .UNSPECIFIED., .F., .F.,
 ( 4, 2, 2, 2, 2, 2, 2, 2, 2, 4 ),
 ( 1.040834085586084257E-17, 0.0003687798516324237216, 0.0007375597032648370348, 0.001106339554897250348, 0.001475119406529663661, 0.001659509332345890376, 0.001843899258162117307, 0.002212679109794577891, 0.002581458961427039126, 0.002950238813059499494 ),
 .UNSPECIFIED. ) ;
#98888 = B_SPLINE_CURVE_WITH_KNOTS ( 'NONE', 3,
 ( #60848, #90833, #46147, #83212, #6175, #13777, #37073, #67977, #98897, #29479, #60352, #21871, #99393, #29971, #2084, #40556, #69958, #93303, #87251, #78083, #87746, #24375, #63869, #2591, #18287, #94806, #573, #55739, #8672, #77590, #17267, #32962, #63372, #17785, #86730, #62859, #41049, #71491, #56259, #1593, #79619, #8177, #16266, #10183, #93816, #48170, #39046, #62349 ),
 .UNSPECIFIED., .F., .F.,
 ( 4, 2, 2, 2, 2, 2, 2, 2, 2, 2, 2, 2, 2, 2, 2, 2, 2, 2, 2, 2, 2, 2, 2, 4 ),
 ( 0.001274896852544186261, 0.001747937982023140945, 0.002220979111502095846, 0.002457499676241543807, 0.002575759958611299229, 0.002694020240981054651, 0.002812280523350810073, 0.002930540805720565495, 0.003167061370460208612, 0.003640102499939553392, 0.004113143629418897738, 0.005059225888377677505, 0.006005308147336457271, 0.006478349276815923916, 0.006714869841555615171, 0.006951390406295307293, 0.007010520547480196714, 0.007069650688665086134, 0.007128780829849976422, 0.007187910971034865842, 0.007424431535774564037, 0.007897472665253960425, 0.008370513794733356813, 0.008843554924212754936 ),
 .UNSPECIFIED. ) ;
#98889 = CARTESIAN_POINT ( 'NONE',  ( 88.28069365579224836, 44.35490120276798365, 2.424033814871950465 ) ) ;
#98890 = VERTEX_POINT ( 'NONE', #13282 ) ;
#98891 = CARTESIAN_POINT ( 'NONE',  ( 196.4843898260797914, 289.9262166352153258, -16.29546860276009212 ) ) ;
#98892 = CARTESIAN_POINT ( 'NONE',  ( 69.05335124041866379, 70.45577847891635770, -1.018671009100705627 ) ) ;
#98893 = CYLINDRICAL_SURFACE ( 'NONE', #59036, 10.00000000000001421 ) ;
#98894 = CARTESIAN_POINT ( 'NONE',  ( 155.3250150347760723, 261.6161776038049425, -18.57420904020362684 ) ) ;
#98895 = VERTEX_POINT ( 'NONE', #90811 ) ;
#98896 = ORIENTED_EDGE ( 'NONE', *, *, #30513, .F. ) ;
#98898 = CARTESIAN_POINT ( 'NONE',  ( 163.8670932201372352, 246.8208641845333773, 5.912697114930636211 ) ) ;
#98897 = CARTESIAN_POINT ( 'NONE',  ( 186.3734546673078682, 271.9784816327500607, -16.50000383220312372 ) ) ;
#98899 = ORIENTED_EDGE ( 'NONE', *, *, #43309, .F. ) ;
#98900 = CARTESIAN_POINT ( 'NONE',  ( 151.0715479399129606, 268.9833987204304435, 14.24612252017116987 ) ) ;
#98901 = CARTESIAN_POINT ( 'NONE',  ( -13.11024591527723615, 27.99999999999999645, -32.50000000000017053 ) ) ;
#98902 = CARTESIAN_POINT ( 'NONE',  ( 80.20448007545800806, 58.22194284664072939, -16.60717859687067843 ) ) ;
#98903 = CARTESIAN_POINT ( 'NONE',  ( -11.09347868418370631, 60.95190685555260046, -10.00000000000000000 ) ) ;
#98904 = ORIENTED_EDGE ( 'NONE', *, *, #37707, .F. ) ;
#98905 = CARTESIAN_POINT ( 'NONE',  ( 44.73065482718366326, 120.5373619841236774, 177.5919119679930134 ) ) ;
#98906 = EDGE_CURVE ( 'NONE', #4426, #81254, #36546, .T. ) ;
#98907 = ORIENTED_EDGE ( 'NONE', *, *, #10886, .F. ) ;
#98908 = CARTESIAN_POINT ( 'NONE',  ( 164.5813345449211624, 245.5837619211427523, 1.447064457712487373 ) ) ;
#98909 = DIRECTION ( 'NONE',  ( 0.000000000000000000, 0.000000000000000000, 1.000000000000000000 ) ) ;
#98910 = ORIENTED_EDGE ( 'NONE', *, *, #7775, .T. ) ;
#98911 = CARTESIAN_POINT ( 'NONE',  ( 190.8072577185990610, 300.1591305089344814, 3.698484652594827171 ) ) ;
#98912 = CARTESIAN_POINT ( 'NONE',  ( -34.16292631813982439, 25.86630820016798538, -10.00000000000000000 ) ) ;
#98913 = ORIENTED_EDGE ( 'NONE', *, *, #64890, .T. ) ;
#98914 = EDGE_CURVE ( 'NONE', #26456, #2381, #21365, .T. ) ;
#98915 = DIRECTION ( 'NONE',  ( -0.4999999999999996669, 0.8660254037844387076, 0.000000000000000000 ) ) ;
#98916 = CARTESIAN_POINT ( 'NONE',  ( 184.7894305693181138, 292.1317680087225881, 12.52679022050396895 ) ) ;
#98917 = CARTESIAN_POINT ( 'NONE',  ( 186.1370921618058674, 283.3846817430978149, 17.26256540491417368 ) ) ;
#98918 = CARTESIAN_POINT ( 'NONE',  ( 76.54518344956915143, 148.6051630683315921, 8.938084663576957867E-16 ) ) ;
#98919 = ORIENTED_EDGE ( 'NONE', *, *, #28439, .T. ) ;
#98920 = EDGE_CURVE ( 'NONE', #76357, #81989, #99720, .T. ) ;
#98921 = CIRCLE ( 'NONE', #8295, 70.00000000000001421 ) ;
#98922 = ORIENTED_EDGE ( 'NONE', *, *, #96231, .F. ) ;
#98923 = EDGE_CURVE ( 'NONE', #38705, #14302, #47636, .T. ) ;
#98924 = CARTESIAN_POINT ( 'NONE',  ( 156.6880320546838448, 266.5988282340034061, -16.21688391091432280 ) ) ;
#98925 = CARTESIAN_POINT ( 'NONE',  ( 82.56006566965427851, 42.71737122084187632, -6.803253249287812388 ) ) ;
#98926 = CARTESIAN_POINT ( 'NONE',  ( 147.4963928429778264, 275.1757489932608109, 4.929816573182678852 ) ) ;
#98927 = CARTESIAN_POINT ( 'NONE',  ( 190.4744901378711290, 300.7355008658671522, 0.04566709859947504224 ) ) ;
#98928 = CARTESIAN_POINT ( 'NONE',  ( 174.7951948700959406, 260.5428239264330728, -14.87950749134391515 ) ) ;
#98929 = CARTESIAN_POINT ( 'NONE',  ( 192.2431834237441706, 297.6720342317289578, 11.07782187406058938 ) ) ;
#98930 = CARTESIAN_POINT ( 'NONE',  ( 191.0825225312146927, 299.6823578679484967, 9.402918570603322479 ) ) ;
#98931 = CARTESIAN_POINT ( 'NONE',  ( 146.5046981847821428, 276.8934145268504494, 0.02269072295920678689 ) ) ;
#98933 = CARTESIAN_POINT ( 'NONE',  ( 79.55398215537849183, 56.00914138994535563, -16.14968118437373690 ) ) ;
#98932 = B_SPLINE_CURVE_WITH_KNOTS ( 'NONE', 3,
 ( #12770, #73561, #43635, #65945, #81690, #4653, #74574, #36033, #66933, #97863, #91273, #21348, #38010, #37035, #91772, #21838, #68428, #7127, #75554, #52723, #76070, #90795, #29934, #20865 ),
 .UNSPECIFIED., .F., .F.,
 ( 4, 2, 2, 2, 2, 2, 2, 2, 2, 2, 2, 4 ),
 ( 0.0003514956339727903431, 0.002330141894556584173, 0.002824803459702569276, 0.002886636155345798874, 0.002948468850989028906, 0.002979385198810643055, 0.003010301546632258071, 0.003072134242275503715, 0.003319465024848496700, 0.003814126589994490477, 0.004061457372567502111, 0.004308788155140514178 ),
 .UNSPECIFIED. ) ;
#98934 = CARTESIAN_POINT ( 'NONE',  ( 45.29894525614688661, 66.96469553601603764, -10.00000000000000000 ) ) ;
#98935 = DIRECTION ( 'NONE',  ( 0.8575671445351807920, -0.5143720371616018472, 0.000000000000000000 ) ) ;
#98936 = LINE ( 'NONE', #29518, #81696 ) ;
#98937 = CARTESIAN_POINT ( 'NONE',  ( 190.1365087082723448, 300.4060458655738444, 1.955324997898008732 ) ) ;
#98938 = CARTESIAN_POINT ( 'NONE',  ( 176.6582871775508465, 289.9246802630469233, -9.262345648488825134 ) ) ;
#98939 = ORIENTED_EDGE ( 'NONE', *, *, #62630, .F. ) ;
#98940 = CYLINDRICAL_SURFACE ( 'NONE', #41617, 17.82106496071139645 ) ;
#98941 = CARTESIAN_POINT ( 'NONE',  ( 74.08065690531797998, 54.82731643721707826, -16.13522336645905142 ) ) ;
#98942 = CARTESIAN_POINT ( 'NONE',  ( 82.39721099668476256, 40.42262220707492304, 1.474573639734337860 ) ) ;
#98943 = CARTESIAN_POINT ( 'NONE',  ( 78.90892980406610491, 46.27727789011839121, 12.87123018350744097 ) ) ;
#98944 = CYLINDRICAL_SURFACE ( 'NONE', #30556, 16.60714546451156792 ) ;
#98945 = CARTESIAN_POINT ( 'NONE',  ( 185.0684497205900527, 286.3477220876792444, 16.15350733335134237 ) ) ;
#98946 = VERTEX_POINT ( 'NONE', #39522 ) ;
#98947 = DIRECTION ( 'NONE',  ( -0.000000000000000000, -0.000000000000000000, 1.000000000000000000 ) ) ;
#98948 = DIRECTION ( 'NONE',  ( -0.8660254037844379305, -0.5000000000000014433, -0.000000000000000000 ) ) ;
#98949 = EDGE_CURVE ( 'NONE', #17524, #32720, #81632, .T. ) ;
#98950 = CARTESIAN_POINT ( 'NONE',  ( 72.15585720070407660, 71.46694910313807725, 5.049726176867119776 ) ) ;
#98951 = CARTESIAN_POINT ( 'NONE',  ( 45.83126033165601854, 207.2677522451419350, -5.000000000000047962 ) ) ;
#98952 = CARTESIAN_POINT ( 'NONE',  ( 116.5476472112030990, 238.0958772461660544, -9.188101187500095079 ) ) ;
#98953 = CARTESIAN_POINT ( 'NONE',  ( 34.05451400132101014, 48.17084265633776852, 177.5919119679930134 ) ) ;
#98954 = CARTESIAN_POINT ( 'NONE',  ( 66.74197533670303528, 67.35026328120331129, -6.853813334782631550 ) ) ;
#98955 = CARTESIAN_POINT ( 'NONE',  ( 84.47821962090468162, 50.67508502715828200, 13.74210141425526999 ) ) ;
#98956 = CARTESIAN_POINT ( 'NONE',  ( 175.9814757996596200, 252.6576015325999833, -4.798176622748077769 ) ) ;
#98957 = CARTESIAN_POINT ( 'NONE',  ( 26.64321143294855077, 192.3149278399161233, 9.188101187500093303 ) ) ;
#98958 = DIRECTION ( 'NONE',  ( -0.9515606131578207005, -0.3074612162317590380, 0.000000000000000000 ) ) ;
#98959 = ORIENTED_EDGE ( 'NONE', *, *, #77280, .T. ) ;
#98960 = CARTESIAN_POINT ( 'NONE',  ( 191.3524005040257236, 298.6585226206977950, 8.123788837531561668 ) ) ;
#98961 = CARTESIAN_POINT ( 'NONE',  ( 74.05623475345210238, 67.87786276047000911, -11.59565021290446651 ) ) ;
#98962 = B_SPLINE_SURFACE_WITH_KNOTS ( 'NONE', 3, 1, ( 
 ( #29508, #111 ),
 ( #59384, #13330 ),
 ( #36598, #22405 ),
 ( #38593, #21902 ),
 ( #14310, #76136 ),
 ( #76608, #5708 ),
 ( #6206, #82764 ),
 ( #52301, #53299 ),
 ( #45196, #7700 ),
 ( #61392, #15283 ),
 ( #69498, #14800 ),
 ( #6710, #37588 ),
 ( #99422, #67502 ),
 ( #20941, #60386 ),
 ( #84252, #68498 ),
 ( #59897, #91341 ),
 ( #90360, #77098 ),
 ( #90864, #51822 ),
 ( #44194, #45682 ),
 ( #7194, #92345 ),
 ( #75132, #98434 ),
 ( #38079, #29999 ),
 ( #83240, #60882 ),
 ( #29025, #21416 ),
 ( #91844, #68992 ),
 ( #13807, #44687 ),
 ( #75618, #37101 ),
 ( #68006, #99918 ),
 ( #98930, #30503 ),
 ( #22894, #61881 ),
 ( #41081, #93850 ),
 ( #39573, #9731 ),
 ( #31488, #1625 ),
 ( #604, #23387 ) ),
 .UNSPECIFIED., .T., .F., .F.,
 ( 4, 2, 2, 2, 2, 2, 2, 2, 2, 2, 2, 2, 2, 2, 2, 2, 4 ),
 ( 2, 2 ),
 ( 0.000000000000000000, 0.06250000000000000000, 0.1250000000000000000, 0.1875000000000000000, 0.2500000000000000000, 0.3125000000000000000, 0.3750000000000000000, 0.4375000000000000000, 0.5000000000000000000, 0.5625000000000000000, 0.6250000000000000000, 0.6875000000000000000, 0.7500000000000000000, 0.8125000000000000000, 0.8750000000000000000, 0.9375000000000000000, 1.000000000000000000 ),
 ( 0.000000000000000000, 1.000000000000000000 ),
 .UNSPECIFIED. ) ;
#98963 = DIRECTION ( 'NONE',  ( -0.5000000000000013323, 0.8660254037844378194, 0.000000000000000000 ) ) ;
#98964 = CARTESIAN_POINT ( 'NONE',  ( 146.8881680668833951, 276.2292252078784145, 4.973452195244782104 ) ) ;
#98965 = CARTESIAN_POINT ( 'NONE',  ( 81.71413070705057180, 41.63923530988346755, -5.548261066783312323 ) ) ;
#98966 = FACE_OUTER_BOUND ( 'NONE', #37570, .T. ) ;
#98967 = CARTESIAN_POINT ( 'NONE',  ( 178.8036298231600654, 287.2060828167640238, -12.28353354550265841 ) ) ;
#98968 = LINE ( 'NONE', #83284, #32131 ) ;
#98969 = CARTESIAN_POINT ( 'NONE',  ( 110.7831656154889970, 234.7677522451418497, 10.00000000000009592 ) ) ;
#98970 = ORIENTED_EDGE ( 'NONE', *, *, #2311, .T. ) ;
#98971 = CARTESIAN_POINT ( 'NONE',  ( 194.7982713327389774, 266.3824398888097562, -7.721487577295030214 ) ) ;
#98972 = CARTESIAN_POINT ( 'NONE',  ( 156.1210910306064932, 280.0783503266571302, -1.584537544745406201 ) ) ;
#98973 = CARTESIAN_POINT ( 'NONE',  ( 163.0056347026689707, 248.3129541054019569, -11.27842346302751508 ) ) ;
#98974 = EDGE_CURVE ( 'NONE', #81759, #27140, #4047, .T. ) ;
#98975 = CARTESIAN_POINT ( 'NONE',  ( 15.00651571324267763, 167.2202760586659736, -5.415160957724236172E-17 ) ) ;
#98976 = CARTESIAN_POINT ( 'NONE',  ( 67.44819667686662967, 68.73639689937741082, -6.116911733827506303 ) ) ;
#98977 = CARTESIAN_POINT ( 'NONE',  ( 192.6343007834967693, 272.1501977007545179, 14.19046712901153739 ) ) ;
#98978 = CARTESIAN_POINT ( 'NONE',  ( 71.74055746682908818, 59.25036641841931129, -15.30500015931909985 ) ) ;
#98979 = CARTESIAN_POINT ( 'NONE',  ( 73.11332203459717505, 69.70319764633998716, 9.138078346488789805 ) ) ;
#98981 = CARTESIAN_POINT ( 'NONE',  ( 59.71473008784930414, 205.2833772461660828, -9.188101187500095079 ) ) ;
#98980 = CARTESIAN_POINT ( 'NONE',  ( 174.8448227160035913, 286.3557171739080900, 10.48088963969321519 ) ) ;
#98982 = DIRECTION ( 'NONE',  ( -0.8755176446347037178, 0.4831861483251572165, 0.000000000000000000 ) ) ;
#98983 = CARTESIAN_POINT ( 'NONE',  ( 72.64791381987437546, 57.16179493898301445, 16.36434895450253535 ) ) ;
#98984 = CARTESIAN_POINT ( 'NONE',  ( -29.67776128939880564, 96.09974013826338535, 44.62810019855511001 ) ) ;
#98985 = CARTESIAN_POINT ( 'NONE',  ( 66.13364871532078837, 68.62542172597147783, -4.396739254649349782 ) ) ;
#98986 = VERTEX_POINT ( 'NONE', #34937 ) ;
#98987 = AXIS2_PLACEMENT_3D ( 'NONE', #87492, #78328, #24604 ) ;
#98988 = CARTESIAN_POINT ( 'NONE',  ( 13.51768745649706993, 188.6115022471903160, -5.000000000000047962 ) ) ;
#98989 = CARTESIAN_POINT ( 'NONE',  ( 207.5230514910949182, 271.2065264061283756, 2.678931747975364708 ) ) ;
#98990 = CARTESIAN_POINT ( 'NONE',  ( 131.1618259000655371, 246.5333772461660544, 9.188101187500095079 ) ) ;
#98991 = CARTESIAN_POINT ( 'NONE',  ( 26.89353023359722883, 24.03085787977764198, 9.188101187500006262 ) ) ;
#98992 = CARTESIAN_POINT ( 'NONE',  ( 186.6441056357332116, 263.8218773865065714, 12.43495875309242571 ) ) ;
#98993 = CARTESIAN_POINT ( 'NONE',  ( 83.73048316204189234, 51.68689211301329323, -14.84080274415373069 ) ) ;
#98994 = CARTESIAN_POINT ( 'NONE',  ( 75.20389695419315501, 52.88180760346911313, -15.99093876381489920 ) ) ;
#98996 = CARTESIAN_POINT ( 'NONE',  ( 74.68831750804957892, 67.03523027571368686, 12.97943796060243038 ) ) ;
#98995 = CARTESIAN_POINT ( 'NONE',  ( 69.48582975785168969, 69.23567760989607223, 7.408010502022341903 ) ) ;
#98997 = CARTESIAN_POINT ( 'NONE',  ( 68.60540934294387228, 64.14349346637945359, 11.89531485900240249 ) ) ;
#98998 = ORIENTED_EDGE ( 'NONE', *, *, #13604, .F. ) ;
#98999 = CARTESIAN_POINT ( 'NONE',  ( 80.69646656315177324, 49.01814528795178916, 14.42895880536565301 ) ) ;
#99000 = CARTESIAN_POINT ( 'NONE',  ( 181.8774662184618194, 285.1120569720015965, 15.89814067624403116 ) ) ;
#99001 = CARTESIAN_POINT ( 'NONE',  ( 75.08824155956695279, 66.10533156918239683, -13.73658325454725215 ) ) ;
#99002 = DIRECTION ( 'NONE',  ( -0.9919422576440852790, -0.1266907948509091164, 0.000000000000000000 ) ) ;
#99003 = CARTESIAN_POINT ( 'NONE',  ( 10.86724236217879458, 11.98920272979924206, 7.433330006724137462 ) ) ;
#99004 = ORIENTED_EDGE ( 'NONE', *, *, #10512, .T. ) ;
#99005 = CARTESIAN_POINT ( 'NONE',  ( 182.7190055043868142, 259.1992038300794547, 9.912833159430794794 ) ) ;
#99006 = CARTESIAN_POINT ( 'NONE',  ( 171.2938040444012131, 284.3570267106589426, -11.29644022524450619 ) ) ;
#99007 = CARTESIAN_POINT ( 'NONE',  ( 75.27786518154783835, 53.33848916356247116, 16.02953000850719434 ) ) ;
#99008 = CARTESIAN_POINT ( 'NONE',  ( 71.63453813518017910, 72.07236434383469259, 0.7172108931481424587 ) ) ;
#99009 = LINE ( 'NONE', #29595, #3727 ) ;
#99010 = DIRECTION ( 'NONE',  ( 0.000000000000000000, -1.000000000000000000, 0.000000000000000000 ) ) ;
#99011 = CARTESIAN_POINT ( 'NONE',  ( 35.43895548624280423, 191.2677522451418781, 10.00000000000009592 ) ) ;
#99012 = CARTESIAN_POINT ( 'NONE',  ( 163.3473224498206093, 247.7211335670114352, -10.00320358166632850 ) ) ;
#99013 = CARTESIAN_POINT ( 'NONE',  ( 200.6680263064462792, 283.0797783131037022, -17.21821073473145347 ) ) ;
#99014 =( BOUNDED_CURVE ( )  B_SPLINE_CURVE ( 2, ( #55467, #99614, #30191, #92049, #22595, #53483, #84435, #14980, #80336 ),
 .UNSPECIFIED., .F., .T. ) 
 B_SPLINE_CURVE_WITH_KNOTS ( ( 3, 2, 2, 2, 3 ),
 ( 0.7459677419354838745, 0.7473118279569892497, 0.7500000000000000000, 0.7526881720430107503, 0.7540322580645161255 ),
 .UNSPECIFIED. ) 
 CURVE ( )  GEOMETRIC_REPRESENTATION_ITEM ( )  RATIONAL_B_SPLINE_CURVE ( ( 0.9330127018922194093, 0.9330127018922194093, 1.000000000000000000, 0.8660254037844387076, 1.000000000000000000, 0.8660254037844387076, 1.000000000000000000, 0.9330127018922194093, 0.9330127018922194093 ) ) 
 REPRESENTATION_ITEM ( '' )  );
#99015 = DIRECTION ( 'NONE',  ( 0.4999999999999997780, -0.8660254037844388186, 0.000000000000000000 ) ) ;
#99016 = CARTESIAN_POINT ( 'NONE',  ( 17.73406340791407843, 11.20801979619927558, -3.090169943749474069 ) ) ;
#99017 = CARTESIAN_POINT ( 'NONE',  ( 191.8988907218820827, 287.7686841597946454, -15.96143006346140858 ) ) ;
#99018 = VERTEX_POINT ( 'NONE', #2571 ) ;
#99019 = CARTESIAN_POINT ( 'NONE',  ( 190.2935937139882299, 301.0488226629397559, 4.649863831023156813 ) ) ;
#99020 = CYLINDRICAL_SURFACE ( 'NONE', #87186, 17.82106496071139645 ) ;
#99021 = CARTESIAN_POINT ( 'NONE',  ( 84.94009691319403998, 45.09646382260235953, -8.562744380091208640 ) ) ;
#99022 = EDGE_LOOP ( 'NONE', ( #56488, #57442, #29637, #80158 ) ) ;
#99023 = CARTESIAN_POINT ( 'NONE',  ( 159.5606259118165724, 264.0648208006689401, -17.79391822139266566 ) ) ;
#99024 = CYLINDRICAL_SURFACE ( 'NONE', #91247, 70.00000000000002842 ) ;
#99025 = CARTESIAN_POINT ( 'NONE',  ( 204.9768178125733016, 275.6167325052707611, 13.98665089523138505 ) ) ;
#99027 = CIRCLE ( 'NONE', #73150, 17.82106496071138935 ) ;
#99026 = CARTESIAN_POINT ( 'NONE',  ( 69.64468245311012140, 62.54413290503185863, 13.39146398752162703 ) ) ;
#99028 = ORIENTED_EDGE ( 'NONE', *, *, #7007, .F. ) ;
#99029 = CARTESIAN_POINT ( 'NONE',  ( 94.03063961704269502, 237.3464784336661637, 1.353441290958777525E-15 ) ) ;
#99030 = CARTESIAN_POINT ( 'NONE',  ( 202.8929259191885990, 279.2261391420940413, 15.95194794840659824 ) ) ;
#99031 = B_SPLINE_CURVE_WITH_KNOTS ( 'NONE', 3,
 ( #1551, #84672, #77023, #18246, #87210, #56213, #24825, #41006, #18741, #95291, #34914, #17745, #71449, #72960, #71948, #10141, #48645, #79580, #32924, #65330, #49625, #96269, #2550, #63828, #33435, #26341, #42026, #79071, #17220, #19263, #3552, #4028, #64332, #73444, #94270, #9656, #80579, #55700, #33953, #34430, #88693, #86688, #11159, #41518, #26835, #64840, #3067, #40514 ),
 .UNSPECIFIED., .F., .F.,
 ( 4, 2, 2, 2, 2, 2, 2, 2, 2, 2, 2, 2, 2, 2, 2, 2, 2, 2, 2, 2, 2, 2, 2, 4 ),
 ( 0.0004917448815929795127, 0.0009375404226552196867, 0.001160438193186298953, 0.001271887078451796899, 0.001383335963717294628, 0.001494784848982792357, 0.001606233734248289869, 0.001829131504779285327, 0.002274927045841276460, 0.003166518127965259159, 0.004058109210089241858, 0.004949700292213225425, 0.005395495833275181646, 0.005618393603806124195, 0.005729842489071552969, 0.005785566931704267356, 0.005841291374336981743, 0.005897015816969696130, 0.005952740259602410516, 0.006064189144867911281, 0.006287086915398848626, 0.006732882456460760612, 0.007178677997522671730, 0.007624473538584582849 ),
 .UNSPECIFIED. ) ;
#99032 = CARTESIAN_POINT ( 'NONE',  ( 73.42123007364070020, 69.75766128465485849, -9.876216450746401421 ) ) ;
#99033 = CARTESIAN_POINT ( 'NONE',  ( 178.1909066280907155, 269.2453967466507265, -16.39845926520222719 ) ) ;
#99034 = CARTESIAN_POINT ( 'NONE',  ( 81.38192781600989179, 42.01391432718669705, -7.810538413258424129 ) ) ;
#99035 = EDGE_LOOP ( 'NONE', ( #29027, #32080, #78599, #15773 ) ) ;
#99036 = ORIENTED_EDGE ( 'NONE', *, *, #18282, .T. ) ;
#99037 = ADVANCED_FACE ( 'NONE', ( #11178 ), #33455, .F. ) ;
#99038 = ORIENTED_EDGE ( 'NONE', *, *, #67122, .F. ) ;
#99039 = CARTESIAN_POINT ( 'NONE',  ( 81.20490824193147716, 49.21687788665059315, 13.87893507568480622 ) ) ;
#99040 = VERTEX_POINT ( 'NONE', #57733 ) ;
#99041 = ADVANCED_FACE ( 'NONE', ( #57238 ), #65349, .F. ) ;
#99042 = CARTESIAN_POINT ( 'NONE',  ( 71.17622542568626898, 71.72302770732439114, 1.525814289146208091 ) ) ;
#99043 = VERTEX_POINT ( 'NONE', #19282 ) ;
#99044 = CARTESIAN_POINT ( 'NONE',  ( 164.4414259850711915, 245.8260906552167171, -6.983224448873608381 ) ) ;
#99045 = CARTESIAN_POINT ( 'NONE',  ( 82.40646201738856291, 41.30234202567336865, 3.324496349298553532 ) ) ;
#99046 = EDGE_CURVE ( 'NONE', #95936, #6127, #41030, .T. ) ;
#99047 = CARTESIAN_POINT ( 'NONE',  ( 153.2283961777204695, 265.2476279883323400, -17.66880461074566000 ) ) ;
#99048 = EDGE_CURVE ( 'NONE', #4844, #83200, #64861, .T. ) ;
#99049 = CARTESIAN_POINT ( 'NONE',  ( -23.46523063411318688, 99.79279178993846244, 45.19944471151773513 ) ) ;
#99050 = CARTESIAN_POINT ( 'NONE',  ( 69.86572752188030222, 68.44440742063116545, -8.131768615182894067 ) ) ;
#99051 = CARTESIAN_POINT ( 'NONE',  ( 165.0375907685516665, 264.5099736516525581, -16.99518358851781485 ) ) ;
#99052 = ORIENTED_EDGE ( 'NONE', *, *, #62199, .F. ) ;
#99053 = CARTESIAN_POINT ( 'NONE',  ( 76.26964293081611856, 57.53102226905608063, 16.11233859593322748 ) ) ;
#99054 = CARTESIAN_POINT ( 'NONE',  ( 13.73114039420206645, 19.87878583063839955, -9.188101187500006262 ) ) ;
#99055 = ORIENTED_EDGE ( 'NONE', *, *, #32161, .T. ) ;
#99056 = DIRECTION ( 'NONE',  ( -0.000000000000000000, 0.000000000000000000, -1.000000000000000000 ) ) ;
#99057 = CARTESIAN_POINT ( 'NONE',  ( 85.68854969368454988, 48.82517353895561030, 12.04942435251151167 ) ) ;
#99059 = VERTEX_POINT ( 'NONE', #64351 ) ;
#99058 = CARTESIAN_POINT ( 'NONE',  ( 124.2269133023873025, 230.9824982072973683, 3.021315404115420679E-15 ) ) ;
#99060 = CARTESIAN_POINT ( 'NONE',  ( 162.6626107288841467, 248.9070890562113902, 10.12509462564867313 ) ) ;
#99061 = CARTESIAN_POINT ( 'NONE',  ( 188.5695376368248617, 260.2104469467469698, 2.212583216593476898 ) ) ;
#99062 = CARTESIAN_POINT ( 'NONE',  ( 161.2972242823068711, 281.6108077277488633, -6.333146725496678897 ) ) ;
#99063 = CARTESIAN_POINT ( 'NONE',  ( -19.65312891409030271, 93.06504152958497400, 59.99999999999999289 ) ) ;
#99064 = CARTESIAN_POINT ( 'NONE',  ( 158.2221939799978543, 257.7339154173171778, 16.96189593371927984 ) ) ;
#99065 = CARTESIAN_POINT ( 'NONE',  ( 171.9391425390357142, 254.6921945179661009, 11.15667454778956369 ) ) ;
#99066 = CARTESIAN_POINT ( 'NONE',  ( 194.8270828572394180, 263.2003066260025435, -0.7951096159142986286 ) ) ;
#99067 = ORIENTED_EDGE ( 'NONE', *, *, #96726, .T. ) ;
#99068 = CARTESIAN_POINT ( 'NONE',  ( 181.8960946995764232, 270.3917867799183341, -16.61744280869827861 ) ) ;
#99069 = CARTESIAN_POINT ( 'NONE',  ( 74.23328924489679537, 62.52147022964773981, -14.75899811459794186 ) ) ;
#99070 = CARTESIAN_POINT ( 'NONE',  ( 193.5443425788056402, 294.1820684295764750, -14.23539291189358558 ) ) ;
#99071 = CARTESIAN_POINT ( 'NONE',  ( -7.357133217438262207, 179.8927522451419350, 2.944929066748280225E-16 ) ) ;
#99072 = CARTESIAN_POINT ( 'NONE',  ( 82.84394531096333480, 53.42394160290496075, -15.30708917581039863 ) ) ;
#99073 = CARTESIAN_POINT ( 'NONE',  ( 204.1031112175353996, 277.1300367187844813, -15.72043984417398299 ) ) ;
#99074 = CARTESIAN_POINT ( 'NONE',  ( 72.12725721317737282, 72.31402113146141630, 1.179144219167332919 ) ) ;
#99075 = CARTESIAN_POINT ( 'NONE',  ( 161.7796304268777305, 250.9944936524672414, -12.70549294170103849 ) ) ;
#99077 = CARTESIAN_POINT ( 'NONE',  ( 181.2440676231241241, 294.5520841294345473, -6.623935519155441654 ) ) ;
#99076 = CARTESIAN_POINT ( 'NONE',  ( -5.021015940802497468, 180.1589784336661637, -6.496448406907675876E-16 ) ) ;
#99078 = CARTESIAN_POINT ( 'NONE',  ( 162.8185578269781502, 249.0392105293238956, 10.15993992013319236 ) ) ;
#99079 = VERTEX_POINT ( 'NONE', #79092 ) ;
#99081 = VERTEX_POINT ( 'NONE', #55720 ) ;
#99080 = B_SPLINE_CURVE_WITH_KNOTS ( 'NONE', 3,
 ( #61639, #98688, #14063, #68747, #99671, #6467, #37346, #68248, #92113, #84495, #15039, #45930 ),
 .UNSPECIFIED., .F., .F.,
 ( 4, 2, 2, 2, 2, 4 ),
 ( 0.000000000000000000, 0.0004890028609250972628, 0.0009780057218501945256, 0.001467008582775291680, 0.001711510013237798949, 0.001956011443700306218 ),
 .UNSPECIFIED. ) ;
#99082 = CARTESIAN_POINT ( 'NONE',  ( -19.65312891409030271, 93.06504152958497400, 177.5919119679930134 ) ) ;
#99083 = CARTESIAN_POINT ( 'NONE',  ( 195.4436462626574667, 265.1414692012189676, -7.795071168451356058 ) ) ;
#99084 = CARTESIAN_POINT ( 'NONE',  ( 175.5914919541931738, 291.0691946881663625, 3.106523132310328617 ) ) ;
#99085 = DIRECTION ( 'NONE',  ( -0.000000000000000000, -0.000000000000000000, 1.000000000000000000 ) ) ;
#99086 = CARTESIAN_POINT ( 'NONE',  ( 202.6926917162147674, 279.5729549550576962, -16.99192271786972697 ) ) ;
#99087 = CARTESIAN_POINT ( 'NONE',  ( 83.77489950824539733, 45.17479857692421064, 9.492654013345440234 ) ) ;
#99088 = CARTESIAN_POINT ( 'NONE',  ( 149.8701220700901331, 277.0052374769863377, 3.110135497610186039 ) ) ;
#99089 = CARTESIAN_POINT ( 'NONE',  ( 23.17945691357580529, 178.0643266524160140, -9.188101187500093303 ) ) ;
#99090 = CARTESIAN_POINT ( 'NONE',  ( 115.5194155920915620, 231.3768266524159856, 9.188101187500098632 ) ) ;
#99091 = CARTESIAN_POINT ( 'NONE',  ( 181.7851089240506042, 293.9661549358203843, -6.312394866988652709 ) ) ;
#99092 = CARTESIAN_POINT ( 'NONE',  ( 167.0546803224166297, 282.1702852132879684, 12.27869116404093752 ) ) ;
#99093 = CARTESIAN_POINT ( 'NONE',  ( 206.6389649419900536, 271.5030152196637800, -6.665702415263554670 ) ) ;
#99094 = CARTESIAN_POINT ( 'NONE',  ( 175.2840916747148583, 281.5314111190519952, -14.18821149970558793 ) ) ;
#99095 = EDGE_CURVE ( 'NONE', #93932, #87229, #72979, .T. ) ;
#99096 = VECTOR ( 'NONE', #78172, 1000.000000000000000 ) ;
#99097 = CARTESIAN_POINT ( 'NONE',  ( 83.27851594750828212, 52.38278085640094872, -14.83539284712679951 ) ) ;
#99098 = CARTESIAN_POINT ( 'NONE',  ( 155.2098048002210930, 261.8157275836062468, 16.98811268941991059 ) ) ;
#99099 = CARTESIAN_POINT ( 'NONE',  ( 161.6127771116929921, 250.7254542206800352, -12.96229604595372464 ) ) ;
#99100 = CARTESIAN_POINT ( 'NONE',  ( 190.0718788718888561, 284.8848510743849829, 17.19586970428585460 ) ) ;
#99101 = CARTESIAN_POINT ( 'NONE',  ( 70.90515648226063661, 61.13412645828226033, -14.46341648420804482 ) ) ;
#99102 = CARTESIAN_POINT ( 'NONE',  ( 169.9825419676943454, 279.0846337363201997, 13.95515977481708880 ) ) ;
#99103 = CARTESIAN_POINT ( 'NONE',  ( 194.7543982349976943, 266.2713905260540059, 7.866109266362086849 ) ) ;
#99104 = PLANE ( 'NONE',  #95060 ) ;
#99105 = DIRECTION ( 'NONE',  ( -0.8660254037844377084, -0.5000000000000014433, -0.000000000000000000 ) ) ;
#99106 = DIRECTION ( 'NONE',  ( 0.5000000000000001110, -0.8660254037844387076, 0.000000000000000000 ) ) ;
#99107 = CARTESIAN_POINT ( 'NONE',  ( 189.2799346409867098, 299.6783261569402157, -5.455465579895408368 ) ) ;
#99108 = ADVANCED_FACE ( 'NONE', ( #79600 ), #81102, .T. ) ;
#99109 = CARTESIAN_POINT ( 'NONE',  ( 89.32180003184730310, 228.5024278399160949, 9.188101187500095079 ) ) ;
#99110 = CARTESIAN_POINT ( 'NONE',  ( 12.59929316974766955, 12.98920272979924739, 7.433330006724137462 ) ) ;
#99111 = CARTESIAN_POINT ( 'NONE',  ( 191.0816511748900268, 299.6838671013740623, 7.311127128005925790 ) ) ;
#99112 = CARTESIAN_POINT ( 'NONE',  ( 159.1262782119615622, 259.2998576110095996, -17.50214152247988864 ) ) ;
#99113 = VECTOR ( 'NONE', #3554, 1000.000000000000227 ) ;
#99115 = CARTESIAN_POINT ( 'NONE',  ( 200.0556816868432009, 284.1403903059980394, 18.52209780479840973 ) ) ;
#99114 = PLANE ( 'NONE',  #40370 ) ;
#99116 = CARTESIAN_POINT ( 'NONE',  ( 193.8212943487757514, 292.9386659295947197, 15.46346239154970625 ) ) ;
#99117 = CARTESIAN_POINT ( 'NONE',  ( 82.86586985908988368, 152.2544130683315871, 0.000000000000000000 ) ) ;
#99118 = CARTESIAN_POINT ( 'NONE',  ( 173.4448748457378144, 267.6069952321146275, -16.52737671724458224 ) ) ;
#99119 = CARTESIAN_POINT ( 'NONE',  ( 32.72297390791170812, 40.93396525600392977, 2.839279412974139660 ) ) ;
#99120 = CARTESIAN_POINT ( 'NONE',  ( 193.2053309019613891, 296.0055459150826778, -12.79465285318189061 ) ) ;
#99121 = CARTESIAN_POINT ( 'NONE',  ( 74.86346528667428402, 202.4824982072973967, 3.021315404115420679E-15 ) ) ;
#99122 = ORIENTED_EDGE ( 'NONE', *, *, #6573, .T. ) ;
#99123 = CARTESIAN_POINT ( 'NONE',  ( 23.51484842749693627, 36.68290643055188838, 3.479690158560446702E-15 ) ) ;
#99124 = LINE ( 'NONE', #29220, #71771 ) ;
#99125 = CARTESIAN_POINT ( 'NONE',  ( 147.4323331177958494, 275.2867036919951147, -5.064030047414062707 ) ) ;
#99126 = FACE_OUTER_BOUND ( 'NONE', #35072, .T. ) ;
#99127 = ORIENTED_EDGE ( 'NONE', *, *, #12141, .F. ) ;
#99128 = CARTESIAN_POINT ( 'NONE',  ( 70.34371006524575876, 61.11933499459465224, 14.86285179514932508 ) ) ;
#99129 = CARTESIAN_POINT ( 'NONE',  ( 76.04102746794296763, 65.42908112640478180, -14.38850911432199098 ) ) ;
#99130 = CARTESIAN_POINT ( 'NONE',  ( 181.4567237428606745, 263.7202305692823074, -12.89642589240160930 ) ) ;
#99131 = CARTESIAN_POINT ( 'NONE',  ( 169.3297900994355416, 252.0805612567175729, -8.701650770669226986 ) ) ;
#99132 = CARTESIAN_POINT ( 'NONE',  ( 139.4522149234843198, 237.9865022471901455, 1.119607411625061291E-15 ) ) ;
#99133 = ORIENTED_EDGE ( 'NONE', *, *, #7018, .F. ) ;
#99134 = CARTESIAN_POINT ( 'NONE',  ( 187.8790403671745821, 279.1610126101560923, 17.78295330846802358 ) ) ;
#99135 = VERTEX_POINT ( 'NONE', #18765 ) ;
#99136 = CARTESIAN_POINT ( 'NONE',  ( 78.41424692880730163, 61.43889907920149795, 16.20108440401020999 ) ) ;
#99137 = CARTESIAN_POINT ( 'NONE',  ( 185.2989352822014553, 292.6601518327293547, -10.61375395971920987 ) ) ;
#99138 = ORIENTED_EDGE ( 'NONE', *, *, #26184, .F. ) ;
#99139 = CARTESIAN_POINT ( 'NONE',  ( 86.48988058553197789, 47.46618689836390104, -10.40901836545075909 ) ) ;
#99140 = FACE_OUTER_BOUND ( 'NONE', #71564, .T. ) ;
#99141 = CARTESIAN_POINT ( 'NONE',  ( 193.0800879007482251, 280.2392748681166381, -16.82455177969006854 ) ) ;
#99142 = CARTESIAN_POINT ( 'NONE',  ( 153.3865286338695739, 264.9737345399563537, -17.77729132017696756 ) ) ;
#99143 = CARTESIAN_POINT ( 'NONE',  ( 153.0308080659177392, 265.5898606369461277, -17.74682723936668438 ) ) ;
#99144 = CARTESIAN_POINT ( 'NONE',  ( 38.77491099913230954, 28.10170272979929962, -7.433330006724141015 ) ) ;
#99145 = CARTESIAN_POINT ( 'NONE',  ( 81.39533252797791363, 55.41833949407015325, -16.32393128051839781 ) ) ;
#99146 = ADVANCED_FACE ( 'NONE', ( #25872 ), #25037, .F. ) ;
#99147 = DIRECTION ( 'NONE',  ( -0.5609510170580175314, -0.8278489937552474531, 0.000000000000000000 ) ) ;
#99148 = CARTESIAN_POINT ( 'NONE',  ( 87.47559087308273718, 45.51532872389798712, 7.025594959947058626 ) ) ;
#99149 = ORIENTED_EDGE ( 'NONE', *, *, #87123, .T. ) ;
#99150 = ORIENTED_EDGE ( 'NONE', *, *, #17424, .F. ) ;
#99151 = CARTESIAN_POINT ( 'NONE',  ( 72.03307586204233814, 72.23070632498334476, -1.602297053105369740 ) ) ;
#99152 = CARTESIAN_POINT ( 'NONE',  ( 159.0487832953843679, 273.6111705420391900, 15.08300900083998464 ) ) ;
#99153 = CARTESIAN_POINT ( 'NONE',  ( 79.62893888804012477, 55.87931252087706469, 16.13392464427525042 ) ) ;
#99155 = CARTESIAN_POINT ( 'NONE',  ( 74.14312167556930433, 66.30466486950707861, 1.224646799147354045E-15 ) ) ;
#99154 = CARTESIAN_POINT ( 'NONE',  ( 204.9608076533459950, 275.6444629144898499, 14.31488288944633069 ) ) ;
#99156 = CARTESIAN_POINT ( 'NONE',  ( 201.1403430031335517, 280.2617017971787732, 16.85780947333721613 ) ) ;
#99158 = CARTESIAN_POINT ( 'NONE',  ( 200.6588745812038610, 274.7719103742660991, -13.77739516878223291 ) ) ;
#99157 = B_SPLINE_CURVE_WITH_KNOTS ( 'NONE', 3,
 ( #55606, #1448, #41416, #32328, #32825, #86100, #47029, #70322, #17125, #77946, #79973, #93162, #86590, #936, #8535, #39407, #31812, #62713, #10542, #95179, #25225, #63229, #93671, #23712, #24235, #47522, #55113, #16626, #33332, #24723, #10042, #63733, #78450, #9032, #39904, #94171, #94668, #78965, #25749, #9552, #72360, #2966, #40414, #56112, #87103, #40905, #71853, #20144, #51015, #73835 ),
 .UNSPECIFIED., .F., .F.,
 ( 4, 2, 2, 2, 2, 2, 2, 2, 2, 2, 2, 2, 2, 2, 2, 2, 2, 2, 2, 2, 2, 2, 2, 2, 4 ),
 ( 0.001009582141182736046, 0.001495460752160263432, 0.001981339363137791035, 0.002224278668626549632, 0.002467217974115308663, 0.002588687626859688395, 0.002710157279604067694, 0.002831626932348446993, 0.002953096585092826291, 0.003196035890581580552, 0.003438975196070333945, 0.003924853807047937009, 0.004896611029003164819, 0.005868368250958392630, 0.006354246861935971408, 0.006597186167424759495, 0.006840125472913548450, 0.006900860299285765422, 0.006961595125657983260, 0.007022329952030199364, 0.007083064778402416335, 0.007326004083891550500, 0.007811882694869918577, 0.008297761305848286653, 0.008783639916826653862 ),
 .UNSPECIFIED. ) ;
#99159 = CARTESIAN_POINT ( 'NONE',  ( 78.67410342229302955, 59.31965170277735666, -16.17003662270398223 ) ) ;
#99160 = CARTESIAN_POINT ( 'NONE',  ( 189.9925954911225290, 301.5701668779311717, 0.1154287172046158938 ) ) ;
#99161 = CARTESIAN_POINT ( 'NONE',  ( 167.2553560077112422, 286.2123104937505786, -4.790173979167302143 ) ) ;
#99162 = EDGE_CURVE ( 'NONE', #66118, #51689, #86708, .T. ) ;
#99163 = CARTESIAN_POINT ( 'NONE',  ( 165.8632497677002675, 265.9352524487321148, 17.74980745403146187 ) ) ;
#99164 = CARTESIAN_POINT ( 'NONE',  ( 183.8772343404243088, 284.9676589712560713, -15.02407609951014145 ) ) ;
#99165 = CARTESIAN_POINT ( 'NONE',  ( 108.9156247924702114, 239.8149278399160949, -9.188101187500095079 ) ) ;
#99166 = VERTEX_POINT ( 'NONE', #9676 ) ;
#99167 = CYLINDRICAL_SURFACE ( 'NONE', #67378, 70.00000000000002842 ) ;
#99168 = CARTESIAN_POINT ( 'NONE',  ( 35.97235683590213284, 38.95586893147758190, 7.433330006724141015 ) ) ;
#99169 = CARTESIAN_POINT ( 'NONE',  ( 188.5580838624726709, 273.6491553406668800, 15.66046095124196214 ) ) ;
#99170 = ORIENTED_EDGE ( 'NONE', *, *, #15196, .T. ) ;
#99171 = VECTOR ( 'NONE', #85012, 1000.000000000000114 ) ;
#99172 = CARTESIAN_POINT ( 'NONE',  ( 74.13689204002625388, 68.84749506857346546, -11.26202041109552177 ) ) ;
#99173 = AXIS2_PLACEMENT_3D ( 'NONE', #75212, #36679, #67588 ) ;
#99175 = B_SPLINE_SURFACE_WITH_KNOTS ( 'NONE', 3, 1, ( 
 ( #55320, #63444 ),
 ( #40624, #48756 ),
 ( #55808, #71560 ),
 ( #93378, #86801 ),
 ( #39612, #17335 ),
 ( #39115, #86300 ),
 ( #94874, #2157 ),
 ( #41120, #33036 ),
 ( #47723, #78658 ),
 ( #9245, #48240 ),
 ( #79186, #79688 ),
 ( #63936, #25436 ),
 ( #10249, #72053 ),
 ( #2656, #18353 ),
 ( #54828, #33547 ),
 ( #25957, #64443 ),
 ( #95402, #56829 ),
 ( #87815, #77662 ),
 ( #8250, #643 ),
 ( #31525, #62417 ),
 ( #23930, #85811 ),
 ( #70533, #16340 ),
 ( #47236, #8742 ),
 ( #88300, #88803 ),
 ( #89771, #3653 ),
 ( #34056, #80689 ),
 ( #72567, #4636 ),
 ( #35022, #27925 ),
 ( #18855, #64946 ),
 ( #58808, #50719 ),
 ( #3171, #65925 ),
 ( #20343, #49736 ),
 ( #80184, #81672 ),
 ( #96375, #51215 ) ),
 .UNSPECIFIED., .T., .F., .F.,
 ( 4, 2, 2, 2, 2, 2, 2, 2, 2, 2, 2, 2, 2, 2, 2, 2, 4 ),
 ( 2, 2 ),
 ( 0.000000000000000000, 0.06250000000000000000, 0.1250000000000000000, 0.1875000000000000000, 0.2500000000000000000, 0.3125000000000000000, 0.3750000000000000000, 0.4375000000000000000, 0.5000000000000000000, 0.5625000000000000000, 0.6250000000000000000, 0.6875000000000000000, 0.7500000000000000000, 0.8125000000000000000, 0.8750000000000000000, 0.9375000000000000000, 1.000000000000000000 ),
 ( 0.000000000000000000, 1.000000000000000000 ),
 .UNSPECIFIED. ) ;
#99174 = CARTESIAN_POINT ( 'NONE',  ( 180.7379841144351076, 294.0691683996430470, -2.595035569306750389 ) ) ;
#99176 = CARTESIAN_POINT ( 'NONE',  ( 192.2058537381976464, 297.7366911437259773, 11.16662451037985981 ) ) ;
#99177 = CARTESIAN_POINT ( 'NONE',  ( 69.97903499771932445, 71.34659005825866984, 2.366570824083385816 ) ) ;
#99178 = DIRECTION ( 'NONE',  ( 0.4999999999999998890, -0.8660254037844385966, 0.000000000000000000 ) ) ;
#99179 = ORIENTED_EDGE ( 'NONE', *, *, #30810, .F. ) ;
#99180 = DIRECTION ( 'NONE',  ( 0.5000000000000014433, -0.8660254037844378194, 0.000000000000000000 ) ) ;
#99181 = ORIENTED_EDGE ( 'NONE', *, *, #2461, .T. ) ;
#99182 = CARTESIAN_POINT ( 'NONE',  ( 44.60439100962815218, 189.8927522451418213, -10.00000000000009237 ) ) ;
#99183 = EDGE_LOOP ( 'NONE', ( #10880, #44279, #80141, #64111 ) ) ;
#99184 = CARTESIAN_POINT ( 'NONE',  ( 206.5280879940269756, 272.9298537347264642, 11.21709153681466731 ) ) ;
#99185 = CIRCLE ( 'NONE', #11840, 70.00000000000001421 ) ;
#99186 = B_SPLINE_CURVE_WITH_KNOTS ( 'NONE', 3,
 ( #98720, #84038, #6500, #7475, #37377, #14597, #53085, #6983, #21695, #54065, #99701, #37868, #68282, #29304, #45476, #52577, #60662, #388, #15564, #30288, #91131, #91620, #22191, #61177, #92143, #22697, #38875, #77397, #53574, #100208, #54557 ),
 .UNSPECIFIED., .F., .F.,
 ( 4, 3, 3, 3, 3, 3, 3, 3, 3, 3, 4 ),
 ( 0.000000000000000000, 0.1333490885032429241, 0.3007194338854423110, 0.4699862290245206409, 0.5844252810809303922, 0.6686540514502636867, 0.7354980260655383795, 0.8028463152565493699, 0.8633854507757111607, 0.9437142632667171460, 1.000000000000000000 ),
 .UNSPECIFIED. ) ;
#99187 = DIRECTION ( 'NONE',  ( 0.8660254037844382635, 0.5000000000000005551, 0.000000000000000000 ) ) ;
#99188 = CARTESIAN_POINT ( 'NONE',  ( 189.5477897539192611, 288.2056741401361819, -16.43566040691730024 ) ) ;
#99189 = CARTESIAN_POINT ( 'NONE',  ( -22.42236680055709641, 157.8615022471902591, 0.000000000000000000 ) ) ;
#99191 = CARTESIAN_POINT ( 'NONE',  ( 158.7400172634752664, 280.5852593085238027, 5.670427242979651616 ) ) ;
#99190 = CARTESIAN_POINT ( 'NONE',  ( 3.113790753877906159, 26.87087736965100859, 177.5919119679930134 ) ) ;
#99192 = CARTESIAN_POINT ( 'NONE',  ( 153.4361244163197000, 264.8878321249116539, -17.23169627811277493 ) ) ;
#99193 = EDGE_LOOP ( 'NONE', ( #39682, #87104 ) ) ;
#99194 = DIRECTION ( 'NONE',  ( 0.5000000000000006661, -0.8660254037844383745, 0.000000000000000000 ) ) ;
#99195 = B_SPLINE_SURFACE_WITH_KNOTS ( 'NONE', 3, 1, ( 
 ( #92593, #76852 ),
 ( #92115, #14571 ),
 ( #76380, #31244 ),
 ( #15533, #62131 ),
 ( #7448, #46954 ),
 ( #99176, #84988 ),
 ( #93588, #93077 ),
 ( #47444, #68749 ),
 ( #24156, #70245 ),
 ( #54032, #55041 ),
 ( #38342, #86022 ),
 ( #16548, #37348 ),
 ( #30763, #68251 ),
 ( #29762, #60635 ),
 ( #91590, #99673 ),
 ( #22667, #15042 ),
 ( #69249, #80404 ),
 ( #17555, #79403 ),
 ( #94590, #70753 ),
 ( #48461, #94096 ),
 ( #63652, #39822 ),
 ( #2375, #95105 ),
 ( #66523, #78879 ),
 ( #1864, #72279 ),
 ( #26163, #87536 ),
 ( #79898, #86515 ),
 ( #1366, #25145 ),
 ( #88022, #33253 ),
 ( #40335, #8954 ),
 ( #2884, #9969 ),
 ( #71274, #32748 ),
 ( #17046, #72794 ),
 ( #47937, #56029 ),
 ( #40830, #10463 ) ),
 .UNSPECIFIED., .T., .F., .F.,
 ( 4, 2, 2, 2, 2, 2, 2, 2, 2, 2, 2, 2, 2, 2, 2, 2, 4 ),
 ( 2, 2 ),
 ( 0.000000000000000000, 0.06250000000000000000, 0.1250000000000000000, 0.1875000000000000000, 0.2500000000000000000, 0.3125000000000000000, 0.3750000000000000000, 0.4375000000000000000, 0.5000000000000000000, 0.5625000000000000000, 0.6250000000000000000, 0.6875000000000000000, 0.7500000000000000000, 0.8125000000000000000, 0.8750000000000000000, 0.9375000000000000000, 1.000000000000000000 ),
 ( 0.000000000000000000, 1.000000000000000000 ),
 .UNSPECIFIED. ) ;
#99196 = CARTESIAN_POINT ( 'NONE',  ( 82.37514789520893999, 41.30464489057703048, -3.406265280166828280 ) ) ;
#99197 = LINE ( 'NONE', #75402, #44809 ) ;
#99198 = CARTESIAN_POINT ( 'NONE',  ( 189.0471581402334209, 270.0386385729072458, -14.06369957967176809 ) ) ;
#99199 = LINE ( 'NONE', #44471, #28753 ) ;
#99200 = DIRECTION ( 'NONE',  ( -0.8660254037844385966, -0.4999999999999999445, 0.000000000000000000 ) ) ;
#99201 = CARTESIAN_POINT ( 'NONE',  ( 51.02741275436266477, 210.2677522451419350, -5.000000000000047962 ) ) ;
#99202 = CARTESIAN_POINT ( 'NONE',  ( 155.5888570658010508, 261.1591898008976500, 17.34682632352454945 ) ) ;
#99203 = LINE ( 'NONE', #76409, #41756 ) ;
#99204 = CARTESIAN_POINT ( 'NONE',  ( 71.86034221268614886, 70.72569178174764204, -6.256625118109824690 ) ) ;
#99205 = CARTESIAN_POINT ( 'NONE',  ( 79.22710464504368133, 225.7369531367911293, -4.594050593750048428 ) ) ;
#99206 = CARTESIAN_POINT ( 'NONE',  ( -25.62627769214124740, 24.57763045674671432, 10.00000000000000000 ) ) ;
#99207 = CARTESIAN_POINT ( 'NONE',  ( 197.1070472075671489, 287.4405515990786739, 17.55387095912554329 ) ) ;
#99208 = CARTESIAN_POINT ( 'NONE',  ( 49.43738778531180600, 210.8967562850346837, -4.648177544792955347E-16 ) ) ;
#99209 = CARTESIAN_POINT ( 'NONE',  ( 66.97748580466556234, 68.05911003901715617, 6.908000617270682042 ) ) ;
#99210 = ADVANCED_FACE ( 'NONE', ( #40537 ), #4716, .F. ) ;
#99211 = CARTESIAN_POINT ( 'NONE',  ( 161.4143265314674522, 251.0691807084224365, -12.94469757303959234 ) ) ;
#99212 = FACE_OUTER_BOUND ( 'NONE', #60359, .T. ) ;
#99214 = FACE_OUTER_BOUND ( 'NONE', #73531, .T. ) ;
#99213 = CARTESIAN_POINT ( 'NONE',  ( 73.17137018064387632, 69.60265530810194434, -9.888782888319330056 ) ) ;
#99215 = CARTESIAN_POINT ( 'NONE',  ( 6.396987757676564357, 15.64441083166258295, -10.00000000000000533 ) ) ;
#99216 = EDGE_CURVE ( 'NONE', #37919, #86487, #50308, .T. ) ;
#99217 = CARTESIAN_POINT ( 'NONE',  ( 35.65891684237410431, 42.36126292948898708, 6.180339887498949913 ) ) ;
#99218 = DIRECTION ( 'NONE',  ( 0.4999999999999998890, -0.8660254037844385966, 0.000000000000000000 ) ) ;
#99219 = CARTESIAN_POINT ( 'NONE',  ( 82.60915189404757086, 54.13479165414026539, 15.54566119520439926 ) ) ;
#99220 = FACE_OUTER_BOUND ( 'NONE', #52916, .T. ) ;
#99221 = EDGE_CURVE ( 'NONE', #39339, #60148, #71645, .T. ) ;
#99222 = CARTESIAN_POINT ( 'NONE',  ( 57.11665387649598813, 203.7833772461660828, -9.188101187500095079 ) ) ;
#99223 = CARTESIAN_POINT ( 'NONE',  ( 157.8092552871339365, 257.3133472685137235, 17.04082256169242626 ) ) ;
#99224 = CARTESIAN_POINT ( 'NONE',  ( 42.17466224797323804, 36.30066082961425877, -10.00000000000000533 ) ) ;
#99225 = CARTESIAN_POINT ( 'NONE',  ( 81.47939018540962763, 50.17275021362014797, -14.26619682564655456 ) ) ;
#99226 = CARTESIAN_POINT ( 'NONE',  ( 140.0925393287100178, 257.8149278399160949, -9.188101187500095079 ) ) ;
#99227 = CARTESIAN_POINT ( 'NONE',  ( 49.94514132322986910, 190.4548013555409796, -4.594050593750042211 ) ) ;
#99228 = CONICAL_SURFACE ( 'NONE', #55523, 17.82106496071138935, 0.7853981633974672638 ) ;
#99229 = CARTESIAN_POINT ( 'NONE',  ( 22.71615395846560759, 25.06628583063842086, -9.188101187500006262 ) ) ;
#99230 = CARTESIAN_POINT ( 'NONE',  ( 198.9369963555428740, 286.0780101374919013, -18.58432392708837710 ) ) ;
#99231 = CARTESIAN_POINT ( 'NONE',  ( 196.9431415128477170, 289.5314680279574304, -16.61413060656005669 ) ) ;
#99232 = CARTESIAN_POINT ( 'NONE',  ( 11.38685760444945672, 12.28920272979924988, -7.433330006724141015 ) ) ;
#99233 = CARTESIAN_POINT ( 'NONE',  ( 63.72375369157850855, 192.0095308348468564, 0.000000000000000000 ) ) ;
#99234 = CARTESIAN_POINT ( 'NONE',  ( 76.85865272105424140, 63.69649487134743282, 15.33129195839047298 ) ) ;
#99235 = CARTESIAN_POINT ( 'NONE',  ( 175.1821364343245477, 291.7930096221122085, 1.896737885627243436 ) ) ;
#99236 = CARTESIAN_POINT ( 'NONE',  ( 176.2722938307433367, 274.9184840992016916, 16.82248187572799125 ) ) ;
#99237 = CARTESIAN_POINT ( 'NONE',  ( 182.1765326276830592, 281.0659326347872593, -16.99519206479797973 ) ) ;
#99238 = CARTESIAN_POINT ( 'NONE',  ( 153.2535461983702021, 276.7944624501984663, 7.180768696100536808 ) ) ;
#99239 = AXIS2_PLACEMENT_3D ( 'NONE', #37527, #60816, #29942 ) ;
#99240 = B_SPLINE_CURVE_WITH_KNOTS ( 'NONE', 3,
 ( #94899, #56350, #17880, #48778, #41143, #2682, #39635, #33572, #87837, #18376, #80208, #3198, #34082, #90302, #20872, #73085, #65458, #51763, #35048, #66455, #12777, #43131, #18882, #81698, #88830, #43643, #96906, #19875, #89321, #19395, #74581, #44134, #66940, #97870, #5160, #36039, #50744, #12271, #65954, #74072, #27477, #4662, #82705, #42150, #28442, #50254, #26475, #57351, #89793, #73569, #35554, #97380 ),
 .UNSPECIFIED., .F., .F.,
 ( 4, 2, 2, 2, 2, 2, 2, 2, 2, 2, 2, 2, 2, 2, 2, 2, 2, 2, 2, 2, 2, 2, 2, 2, 2, 4 ),
 ( 0.0006742088093967555989, 0.0008834669511509028999, 0.001092725092905050092, 0.001197354163782128351, 0.001301983234659206609, 0.001406612305536284867, 0.001511241376413363126, 0.001720499518167624593, 0.001929757659921886061, 0.002348273943430352617, 0.003185306510447285296, 0.004022339077464217975, 0.004859371644481151088, 0.005277887927989698309, 0.005487146069744016155, 0.005591775140621175512, 0.005644089676059718327, 0.005696404211498261143, 0.005748718746936803958, 0.005801033282375345906, 0.005905662353252520008, 0.006114920495006899437, 0.006324178636761279733, 0.006533436778515659162, 0.006951953062024276639, 0.007370469345532895851 ),
 .UNSPECIFIED. ) ;
#99241 = EDGE_CURVE ( 'NONE', #91430, #87128, #81705, .T. ) ;
#99242 = PLANE ( 'NONE',  #8866 ) ;
#99243 = CARTESIAN_POINT ( 'NONE',  ( 100.5532405368332007, 228.8615022471902591, -10.00000000000009592 ) ) ;
#99244 = CARTESIAN_POINT ( 'NONE',  ( 200.1662314894802819, 283.9489124310637180, 17.19420058542677054 ) ) ;
#99245 = CARTESIAN_POINT ( 'NONE',  ( 194.6164141854688694, 285.4975589841284318, -17.28892555162024181 ) ) ;
#99246 = ORIENTED_EDGE ( 'NONE', *, *, #38842, .T. ) ;
#99247 = VECTOR ( 'NONE', #34203, 1000.000000000000000 ) ;
#99248 = CARTESIAN_POINT ( 'NONE',  ( 58.36173894231861681, 198.3768266524159856, 9.188101187500098632 ) ) ;
#99249 = VERTEX_POINT ( 'NONE', #33117 ) ;
#99250 = CARTESIAN_POINT ( 'NONE',  ( 166.5849221621933225, 264.6761944418691996, 17.19226874345410394 ) ) ;
#99251 = CARTESIAN_POINT ( 'NONE',  ( 190.7403173041394950, 300.2750747078583800, -4.254144485856557800 ) ) ;
#99252 = LINE ( 'NONE', #83078, #27246 ) ;
#99253 = EDGE_LOOP ( 'NONE', ( #100188, #83876, #71234, #7562 ) ) ;
#99255 = DIRECTION ( 'NONE',  ( -0.000000000000000000, -0.000000000000000000, -1.000000000000000000 ) ) ;
#99254 = AXIS2_PLACEMENT_3D ( 'NONE', #36531, #37523, #29441 ) ;
#99256 = CARTESIAN_POINT ( 'NONE',  ( 79.42038935749546624, 46.23329716661052657, -13.24303890372938497 ) ) ;
#99257 = CARTESIAN_POINT ( 'NONE',  ( 194.4666154385731431, 293.8209370148700827, -14.56896502715340702 ) ) ;
#99258 = CARTESIAN_POINT ( 'NONE',  ( 87.33294734268930881, 44.88192199842172414, 6.808005391826766228 ) ) ;
#99259 = DIRECTION ( 'NONE',  ( 0.6123724356957995774, 0.3535533905932699006, 0.7071067811865450192 ) ) ;
#99260 = CARTESIAN_POINT ( 'NONE',  ( 156.9781162866021589, 258.7529222455866034, 16.87007551417546480 ) ) ;
#99261 = ORIENTED_EDGE ( 'NONE', *, *, #73429, .F. ) ;
#99262 = CARTESIAN_POINT ( 'NONE',  ( 28.14623683147711830, 18.11110640527293114, -2.839279412974138328 ) ) ;
#99263 = CARTESIAN_POINT ( 'NONE',  ( 68.59458243152100465, 69.79431807905237406, -3.474663545031335232 ) ) ;
#99264 = CARTESIAN_POINT ( 'NONE',  ( 74.81832046901195099, 67.48663194201290594, -12.71244991431774807 ) ) ;
#99265 = EDGE_CURVE ( 'NONE', #53524, #48279, #90356, .T. ) ;
#99266 = ADVANCED_FACE ( 'NONE', ( #82265 ), #50803, .F. ) ;
#99267 = EDGE_LOOP ( 'NONE', ( #85083, #20774, #83759, #82688, #60525 ) ) ;
#99268 = DIRECTION ( 'NONE',  ( -0.2168075248790319320, -0.9762143704923770260, 0.000000000000000000 ) ) ;
#99269 = CARTESIAN_POINT ( 'NONE',  ( 206.2041691044954348, 273.4908977089264113, -9.455375957961031474 ) ) ;
#99270 = VERTEX_POINT ( 'NONE', #76132 ) ;
#99271 = ORIENTED_EDGE ( 'NONE', *, *, #69648, .T. ) ;
#99272 = EDGE_CURVE ( 'NONE', #12902, #20280, #28006, .T. ) ;
#99273 = CARTESIAN_POINT ( 'NONE',  ( 81.20257704785798580, 49.55865801952204208, -14.05600544740383739 ) ) ;
#99275 = FACE_OUTER_BOUND ( 'NONE', #67021, .T. ) ;
#99274 = CARTESIAN_POINT ( 'NONE',  ( 162.9186055433422382, 283.5390355093646804, -3.110742804078471924 ) ) ;
#99276 = CARTESIAN_POINT ( 'NONE',  ( 189.7094295309238419, 300.0606247079692253, 5.078421157105148076 ) ) ;
#99277 = CARTESIAN_POINT ( 'NONE',  ( 164.2712161151136172, 246.1209027979328710, 7.276091357954241445 ) ) ;
#99278 = CARTESIAN_POINT ( 'NONE',  ( 198.5966822647444587, 286.6674514332866579, 17.25284514431582750 ) ) ;
#99279 = CARTESIAN_POINT ( 'NONE',  ( 182.1983635332545646, 295.7656116556308916, 4.955917269626422872 ) ) ;
#99280 = CARTESIAN_POINT ( 'NONE',  ( 122.2307653756559773, 247.5024278399160949, -9.188101187500093303 ) ) ;
#99281 = ADVANCED_FACE ( 'NONE', ( #81753 ), #43191, .F. ) ;
#99282 = CARTESIAN_POINT ( 'NONE',  ( 203.2651555929824383, 267.8361268713933327, 2.564698397200394719 ) ) ;
#99283 = CARTESIAN_POINT ( 'NONE',  ( 182.7190055043868142, 259.1992038300794547, 9.912833159430794794 ) ) ;
#99284 = CARTESIAN_POINT ( 'NONE',  ( 69.62006919151632189, 204.8768266524160140, -9.188101187500091527 ) ) ;
#99285 = VERTEX_POINT ( 'NONE', #91839 ) ;
#99286 = DIRECTION ( 'NONE',  ( 0.5000000000000014433, -0.8660254037844378194, 0.000000000000000000 ) ) ;
#99287 = CARTESIAN_POINT ( 'NONE',  ( 181.3346534254663140, 271.3440730695800767, -17.45372068697093226 ) ) ;
#99288 = VERTEX_POINT ( 'NONE', #66997 ) ;
#99289 = CARTESIAN_POINT ( 'NONE',  ( 164.5139018292655919, 259.6662038739244736, -17.01387605652571366 ) ) ;
#99290 = VERTEX_POINT ( 'NONE', #74135 ) ;
#99291 = EDGE_LOOP ( 'NONE', ( #61097, #24966, #33124, #36351 ) ) ;
#99292 = ADVANCED_FACE ( 'NONE', ( #44682 ), #50792, .F. ) ;
#99293 = CARTESIAN_POINT ( 'NONE',  ( 79.26890985290187075, 228.1199935810940929, 2.679491924311251605 ) ) ;
#99294 = CARTESIAN_POINT ( 'NONE',  ( 66.62939956341956815, 67.53919750792978505, 6.361161503035429376 ) ) ;
#99295 = EDGE_CURVE ( 'NONE', #98305, #3124, #61387, .T. ) ;
#99296 = CARTESIAN_POINT ( 'NONE',  ( 0.4370954166217684844, 164.3927522451417644, -10.00000000000009237 ) ) ;
#99297 = CARTESIAN_POINT ( 'NONE',  ( 86.97967072741523964, 43.07970033450948222, -1.614587236035697204 ) ) ;
#99298 = CARTESIAN_POINT ( 'NONE',  ( 114.8426596992764388, 237.1115022471902307, 10.00000000000009592 ) ) ;
#99299 = DIRECTION ( 'NONE',  ( 0.06958655048003267729, -0.1205274409548735270, -0.9902680687415703620 ) ) ;
#99300 = CARTESIAN_POINT ( 'NONE',  ( 72.28935250795022682, 68.85540587544358004, 9.499973692823946436 ) ) ;
#99301 = B_SPLINE_CURVE_WITH_KNOTS ( 'NONE', 3,
 ( #88237, #57262, #58262, #96313 ),
 .UNSPECIFIED., .F., .F.,
 ( 4, 4 ),
 ( 0.008596905824991037462, 0.01496866495574719277 ),
 .UNSPECIFIED. ) ;
#99302 = ORIENTED_EDGE ( 'NONE', *, *, #98313, .T. ) ;
#99303 = CARTESIAN_POINT ( 'NONE',  ( 17.48767303752208235, 28.83478043621388309, -8.090169943749479842 ) ) ;
#99304 = LINE ( 'NONE', #68870, #73754 ) ;
#99305 = ORIENTED_EDGE ( 'NONE', *, *, #12211, .T. ) ;
#99306 = CARTESIAN_POINT ( 'NONE',  ( 76.20260252794534495, 51.02260908202766387, -15.56074846367122788 ) ) ;
#99307 = B_SPLINE_CURVE_WITH_KNOTS ( 'NONE', 3,
 ( #42252, #34661, #65561, #11884, #79815, #27078, #73677, #19503, #96510, #10380, #41250, #57960, #72189, #29072, #75667, #97489, #59937, #14356, #67049, #28548, #44731, #83289, #6250, #4779, #75178, #5265, #74188, #97015, #51351, #21947, #36643 ),
 .UNSPECIFIED., .F., .F.,
 ( 4, 3, 3, 3, 3, 3, 3, 3, 3, 3, 4 ),
 ( 0.000000000000000000, 0.1333490885032387052, 0.3007194338854507487, 0.4699862290245374608, 0.5844252810809412724, 0.6686540514502781196, 0.7354980260655558100, 0.8028463152565722405, 0.8633854507757224850, 0.9437142632667419040, 1.000000000000000000 ),
 .UNSPECIFIED. ) ;
#99308 = B_SPLINE_CURVE_WITH_KNOTS ( 'NONE', 3,
 ( #14449, #77234, #7330, #92960, #37237, #83382, #46309, #22037, #38210, #5849 ),
 .UNSPECIFIED., .F., .F.,
 ( 4, 2, 2, 2, 4 ),
 ( 0.000000000000000000, 0.0002622400424273337374, 0.0005244800848546674749, 0.0007867201272820012123, 0.001048960169709334950 ),
 .UNSPECIFIED. ) ;
#99309 = CARTESIAN_POINT ( 'NONE',  ( 183.9632230134671715, 275.2220319246098938, 16.38282608893444703 ) ) ;
#99310 = AXIS2_PLACEMENT_3D ( 'NONE', #41791, #96051, #86965 ) ;
#99311 = CARTESIAN_POINT ( 'NONE',  ( 198.9782417033094930, 281.1264296331257810, 17.13350274969746323 ) ) ;
#99312 = CARTESIAN_POINT ( 'NONE',  ( 147.4771086736140262, 275.6046378290653251, -0.0003692388140982706527 ) ) ;
#99313 = CARTESIAN_POINT ( 'NONE',  ( 138.6044920356617922, 241.6423013555409796, -4.594050593750043987 ) ) ;
#99314 = ORIENTED_EDGE ( 'NONE', *, *, #7604, .T. ) ;
#99315 = CARTESIAN_POINT ( 'NONE',  ( 0.9806730298622799991, 159.8262482093458061, 3.021315404115420679E-15 ) ) ;
#99316 = CARTESIAN_POINT ( 'NONE',  ( 86.37275258873019368, 44.84559259891241823, 6.849086954479022715 ) ) ;
#99317 = DIRECTION ( 'NONE',  ( -1.000000000000000000, 0.000000000000000000, 0.000000000000000000 ) ) ;
#99318 =( BOUNDED_CURVE ( )  B_SPLINE_CURVE ( 2, ( #44919, #44429, #51541, #67233, #73854, #22135, #60115, #66735, #5940 ),
 .UNSPECIFIED., .F., .T. ) 
 B_SPLINE_CURVE_WITH_KNOTS ( ( 3, 2, 2, 2, 3 ),
 ( 0.5040322580645161255, 0.5053763440860215006, 0.5080645161290322509, 0.5107526881720430012, 0.5120967741935483764 ),
 .UNSPECIFIED. ) 
 CURVE ( )  GEOMETRIC_REPRESENTATION_ITEM ( )  RATIONAL_B_SPLINE_CURVE ( ( 0.9330127018922194093, 0.9330127018922194093, 1.000000000000000000, 0.8660254037844387076, 1.000000000000000000, 0.8660254037844387076, 1.000000000000000000, 0.9330127018922194093, 0.9330127018922194093 ) ) 
 REPRESENTATION_ITEM ( '' )  );
#99319 = CARTESIAN_POINT ( 'NONE',  ( 72.82183928371372872, 70.95611737677427300, 7.748181657111721243 ) ) ;
#99320 = VECTOR ( 'NONE', #81606, 999.9999999999998863 ) ;
#99321 = CARTESIAN_POINT ( 'NONE',  ( -56.06787742410713093, 34.75406423768147590, -10.00000000000000000 ) ) ;
#99322 = ORIENTED_EDGE ( 'NONE', *, *, #47301, .T. ) ;
#99323 = CARTESIAN_POINT ( 'NONE',  ( 195.7165112625155530, 265.4114503779815664, 4.502320798389543022 ) ) ;
#99324 = DIRECTION ( 'NONE',  ( 1.000000000000000000, 0.000000000000000000, 0.000000000000000000 ) ) ;
#99325 = CARTESIAN_POINT ( 'NONE',  ( 87.35606880162970356, 45.77061481740687299, 8.290963297571641633 ) ) ;
#99326 = CARTESIAN_POINT ( 'NONE',  ( 185.0302441327199290, 263.6005475928211581, -12.60236960991709232 ) ) ;
#99327 = CARTESIAN_POINT ( 'NONE',  ( 184.3405100053359149, 263.3003275659135625, -13.11914462798110748 ) ) ;
#99328 = CARTESIAN_POINT ( 'NONE',  ( 198.5696159774462615, 266.1063467524069779, 0.3741886566019196891 ) ) ;
#99329 = ORIENTED_EDGE ( 'NONE', *, *, #9117, .F. ) ;
#99330 = AXIS2_PLACEMENT_3D ( 'NONE', #65832, #73959, #51652 ) ;
#99331 = CARTESIAN_POINT ( 'NONE',  ( 146.7879906441258129, 276.4027375938661635, 4.347255311287614887 ) ) ;
#99332 = CARTESIAN_POINT ( 'NONE',  ( 186.8085655849630200, 282.2086298501483839, 17.42445011646567110 ) ) ;
#99333 = EDGE_CURVE ( 'NONE', #79062, #2126, #54787, .T. ) ;
#99334 = CARTESIAN_POINT ( 'NONE',  ( 164.3274319858398087, 246.0235340536434592, -1.770631424362269168 ) ) ;
#99336 = FACE_BOUND ( 'NONE', #31077, .T. ) ;
#99335 = DIRECTION ( 'NONE',  ( 0.9377374661009790779, 0.3473448497826262527, 0.000000000000000000 ) ) ;
#99337 = EDGE_CURVE ( 'NONE', #10175, #73010, #92341, .T. ) ;
#99338 = CARTESIAN_POINT ( 'NONE',  ( 29.09658290004530201, 18.92755873383627119, 6.180339887498953466 ) ) ;
#99339 = CARTESIAN_POINT ( 'NONE',  ( 148.9275518150011806, 272.6969089400084272, 12.34519124974546500 ) ) ;
#99340 = DIRECTION ( 'NONE',  ( 1.000000000000000000, 0.000000000000000000, 0.000000000000000000 ) ) ;
#99341 = CARTESIAN_POINT ( 'NONE',  ( 73.37627859927840746, 69.07053839721005772, -10.62591557373302820 ) ) ;
#99342 = CARTESIAN_POINT ( 'NONE',  ( 19.39713158799116499, 193.5530062829863311, -4.648177544792955347E-16 ) ) ;
#99343 = CARTESIAN_POINT ( 'NONE',  ( 140.5888732624033821, 258.6427522451418781, -10.00000000000009415 ) ) ;
#99344 = CARTESIAN_POINT ( 'NONE',  ( -22.42236680055709641, 157.8615022471902591, 0.000000000000000000 ) ) ;
#99345 = EDGE_LOOP ( 'NONE', ( #34350, #23119, #2083, #95852 ) ) ;
#99346 = EDGE_CURVE ( 'NONE', #51044, #941, #42987, .T. ) ;
#99347 = CARTESIAN_POINT ( 'NONE',  ( 66.71850186762439705, 67.38486778997553017, -6.761415606802787970 ) ) ;
#99348 = CARTESIAN_POINT ( 'NONE',  ( 72.85625868234195934, 71.07309412281132666, -7.586526616956824398 ) ) ;
#99349 = CARTESIAN_POINT ( 'NONE',  ( 199.2299651681423143, 285.5705732690366858, -17.65328173313980642 ) ) ;
#99350 = CARTESIAN_POINT ( 'NONE',  ( 3.260525530768699998, 178.8149278399161233, 9.188101187500093303 ) ) ;
#99351 = CARTESIAN_POINT ( 'NONE',  ( 178.7807591103801315, 273.8421904428736866, -16.83327263018412978 ) ) ;
#99352 = CARTESIAN_POINT ( 'NONE',  ( 20.87599742628078303, 30.79103043416549568, 8.090169943749478065 ) ) ;
#99353 = CARTESIAN_POINT ( 'NONE',  ( 85.04377965201177858, 48.84687674572032989, 12.36303725827022504 ) ) ;
#99354 = CARTESIAN_POINT ( 'NONE',  ( 205.2391015854675516, 275.1624436846170738, -14.01434138479280911 ) ) ;
#99355 = DIRECTION ( 'NONE',  ( 0.3613624741150711084, 0.7937185950816926239, -0.4893137583626469000 ) ) ;
#99356 = CARTESIAN_POINT ( 'NONE',  ( 123.0699010352285825, 251.8615022471902876, 5.000000000000046185 ) ) ;
#99357 = CARTESIAN_POINT ( 'NONE',  ( 178.3085564311570295, 254.9668335614806551, -3.913436853880700728 ) ) ;
#99358 = EDGE_CURVE ( 'NONE', #98253, #86118, #63792, .T. ) ;
#99359 = CARTESIAN_POINT ( 'NONE',  ( 198.1857676047573307, 287.3791765019590798, 18.47549341984830562 ) ) ;
#99360 = EDGE_CURVE ( 'NONE', #21753, #78482, #69494, .T. ) ;
#99361 = CARTESIAN_POINT ( 'NONE',  ( 51.18979252112020362, 200.3615022471902307, -10.00000000000009592 ) ) ;
#99362 = DIRECTION ( 'NONE',  ( 0.5344452582589497291, -0.8452030915256549815, 0.000000000000000000 ) ) ;
#99363 = CARTESIAN_POINT ( 'NONE',  ( 147.6121581866023007, 274.9752375363476631, 8.700660424766859080 ) ) ;
#99364 = CARTESIAN_POINT ( 'NONE',  ( 10.56744132731740216, 189.1589784336661637, -6.496448406907675876E-16 ) ) ;
#99365 = CARTESIAN_POINT ( 'NONE',  ( 72.47494455774665312, 70.67364856651920491, -7.881577117668186361 ) ) ;
#99366 = CARTESIAN_POINT ( 'NONE',  ( 152.7153488183568300, 266.1362520814392951, 17.33540622643059237 ) ) ;
#99367 = CARTESIAN_POINT ( 'NONE',  ( 86.76444126019433156, 45.86660341771495553, -8.261827951889216592 ) ) ;
#99368 = B_SPLINE_CURVE_WITH_KNOTS ( 'NONE', 3,
 ( #48811, #25495, #57888, #4185 ),
 .UNSPECIFIED., .F., .F.,
 ( 4, 4 ),
 ( 0.04775794113389541379, 0.04887120950165265570 ),
 .UNSPECIFIED. ) ;
#99369 = CARTESIAN_POINT ( 'NONE',  ( 25.34687108590969729, 93.06504152958497400, -20.00000000000000355 ) ) ;
#99370 = CARTESIAN_POINT ( 'NONE',  ( 164.4858674010174298, 245.7491158648375347, -2.958464974013825355 ) ) ;
#99371 = CARTESIAN_POINT ( 'NONE',  ( 188.9070770133223505, 267.7838735664225851, 14.12628498767583629 ) ) ;
#99372 = LINE ( 'NONE', #28970, #96317 ) ;
#99373 = CARTESIAN_POINT ( 'NONE',  ( 160.6500289177108129, 280.8499340018469752, 9.543921644910932756 ) ) ;
#99374 = ITEM_DEFINED_TRANSFORMATION ( 'NONE', 'NONE', #890,  #68784 ) ;
#99375 = CARTESIAN_POINT ( 'NONE',  ( 20.84336723938811176, 14.96004757982089828, -5.678558825948276656 ) ) ;
#99376 = CARTESIAN_POINT ( 'NONE',  ( 190.1158090214649405, 301.3567547831981983, -1.340987185199551845 ) ) ;
#99377 = CARTESIAN_POINT ( 'NONE',  ( 72.00843944767480309, 59.19984693747115045, 15.86336254811915225 ) ) ;
#99378 = CARTESIAN_POINT ( 'NONE',  ( 155.3738696901333469, 261.5315588585399951, 17.02116401938635804 ) ) ;
#99379 = ORIENTED_EDGE ( 'NONE', *, *, #36636, .T. ) ;
#99380 = CARTESIAN_POINT ( 'NONE',  ( 185.4471464075789982, 290.9481437133458144, 12.22111610210481381 ) ) ;
#99381 = CARTESIAN_POINT ( 'NONE',  ( 160.9155581428462085, 282.2930683307629920, -7.657675304491033508 ) ) ;
#99382 = DIRECTION ( 'NONE',  ( -0.8660254037844387076, -0.4999999999999998890, -0.000000000000000000 ) ) ;
#99383 = CARTESIAN_POINT ( 'NONE',  ( 88.14460040508836869, 44.32472722906683771, 2.727550722552130047 ) ) ;
#99384 = VERTEX_POINT ( 'NONE', #107 ) ;
#99385 = CARTESIAN_POINT ( 'NONE',  ( 82.44310520575160695, 54.28011738120408580, -15.96781897959229113 ) ) ;
#99386 = CARTESIAN_POINT ( 'NONE',  ( 166.8965953329662568, 259.4083194189263963, 16.50658842888446642 ) ) ;
#99387 = CARTESIAN_POINT ( 'NONE',  ( 195.6914848190668863, 279.7035040353765680, -17.46620344769279853 ) ) ;
#99388 = CARTESIAN_POINT ( 'NONE',  ( 155.5587153255869453, 261.2113968263770971, -18.30500480654006878 ) ) ;
#99389 = VECTOR ( 'NONE', #29811, 1000.000000000000114 ) ;
#99390 = VERTEX_POINT ( 'NONE', #70491 ) ;
#99391 = VERTEX_POINT ( 'NONE', #30993 ) ;
#99392 = ADVANCED_FACE ( 'NONE', ( #86254 ), #15785, .F. ) ;
#99394 = DIRECTION ( 'NONE',  ( -1.000000000000000000, 0.000000000000000000, 0.000000000000000000 ) ) ;
#99393 = CARTESIAN_POINT ( 'NONE',  ( 186.2308893754327244, 271.9687482497705560, -16.31403051770207213 ) ) ;
#99395 = EDGE_LOOP ( 'NONE', ( #90832, #35744, #80398, #66737 ) ) ;
#99396 = CARTESIAN_POINT ( 'NONE',  ( 150.6571681785161445, 269.7011255207979730, 15.24894850018880454 ) ) ;
#99397 = CARTESIAN_POINT ( 'NONE',  ( 23.20344070249937829, 32.13478043621388736, 8.090169943749478065 ) ) ;
#99398 = CARTESIAN_POINT ( 'NONE',  ( 80.34072333937859867, 58.10214405650913250, -16.60604606379114401 ) ) ;
#99399 = CARTESIAN_POINT ( 'NONE',  ( 188.9516232634142909, 259.5449388965931234, 2.625812016075142807 ) ) ;
#99400 = ORIENTED_EDGE ( 'NONE', *, *, #98372, .T. ) ;
#99401 = CARTESIAN_POINT ( 'NONE',  ( 190.5893431400089923, 300.5365696307625853, -0.3099240395267599535 ) ) ;
#99402 = VECTOR ( 'NONE', #4849, 1000.000000000000000 ) ;
#99403 = EDGE_CURVE ( 'NONE', #76337, #47702, #16793, .T. ) ;
#99404 = CARTESIAN_POINT ( 'NONE',  ( 164.4261001824251878, 245.8526357240660900, 1.583002802772015549 ) ) ;
#99405 = EDGE_CURVE ( 'NONE', #6345, #17132, #93640, .T. ) ;
#99406 = DIRECTION ( 'NONE',  ( -0.8099771808667467488, -0.5864613938488684175, 0.000000000000000000 ) ) ;
#99407 = VERTEX_POINT ( 'NONE', #8203 ) ;
#99408 = CARTESIAN_POINT ( 'NONE',  ( 148.9230895364621574, 272.7046378331555161, 12.20434325797056019 ) ) ;
#99409 = CARTESIAN_POINT ( 'NONE',  ( 78.20719261189692872, 47.49265493982247222, -14.37061554849372236 ) ) ;
#99410 = ORIENTED_EDGE ( 'NONE', *, *, #61202, .F. ) ;
#99411 = CARTESIAN_POINT ( 'NONE',  ( 177.2105452297388979, 293.7001946432246768, 0.5067388932645889854 ) ) ;
#99412 = CARTESIAN_POINT ( 'NONE',  ( 31.27486418823966119, 41.55466486950703597, 7.012934429366973338E-14 ) ) ;
#99413 = CARTESIAN_POINT ( 'NONE',  ( 78.26820067796158753, 47.38613455463863033, -14.29902697151583268 ) ) ;
#99414 = CARTESIAN_POINT ( 'NONE',  ( 30.67947171958994090, 41.21091486745863364, -1.111400068045478839E-16 ) ) ;
#99415 = ORIENTED_EDGE ( 'NONE', *, *, #84509, .F. ) ;
#99416 = EDGE_LOOP ( 'NONE', ( #33462, #29105, #28028, #95840 ) ) ;
#99417 = CARTESIAN_POINT ( 'NONE',  ( 73.15705624839024779, 69.75081864091815476, 9.110835657918801900 ) ) ;
#99418 = CARTESIAN_POINT ( 'NONE',  ( 190.3791419447713906, 300.9006487807255326, -5.688668718458480988 ) ) ;
#99419 = CARTESIAN_POINT ( 'NONE',  ( 190.1063449786324213, 301.3731469862293011, 0.2163967485516588019 ) ) ;
#99420 = CARTESIAN_POINT ( 'NONE',  ( 149.6877696051026305, 271.3801731027346591, 11.89134584187677390 ) ) ;
#99421 = CARTESIAN_POINT ( 'NONE',  ( 153.3616370783189211, 265.0168479788495688, 17.48287904751960653 ) ) ;
#99422 = CARTESIAN_POINT ( 'NONE',  ( 191.8109306323408134, 298.4207180281530896, 8.739483817295738532 ) ) ;
#99423 = CARTESIAN_POINT ( 'NONE',  ( 191.7247331938518187, 298.5700163710982338, -9.650650827884682315 ) ) ;
#99424 = CARTESIAN_POINT ( 'NONE',  ( 190.1751179328237242, 301.2540287353828035, 3.252640783176552475 ) ) ;
#99425 = CARTESIAN_POINT ( 'NONE',  ( 70.36027467213139630, 68.40961035810749991, 8.603903390954418029 ) ) ;
#99427 = CARTESIAN_POINT ( 'NONE',  ( 49.93886538132678510, 83.40144735776343055, 10.00000000000000000 ) ) ;
#99426 = CARTESIAN_POINT ( 'NONE',  ( 196.9728329903666122, 289.4800408803428695, -17.53478045286815856 ) ) ;
#99428 = CARTESIAN_POINT ( 'NONE',  ( 67.13193361080226396, 66.73346850515530093, 8.231172206884084019 ) ) ;
#99429 = CARTESIAN_POINT ( 'NONE',  ( 170.8130694511098682, 289.0930926786006125, 4.372098042472422286 ) ) ;
#99430 = CARTESIAN_POINT ( 'NONE',  ( 78.26950878785386578, 47.45902659347659380, 14.33551611744975496 ) ) ;
#99431 = CARTESIAN_POINT ( 'NONE',  ( 97.73839765093606502, 236.4244531367911009, -4.594050593750046652 ) ) ;
#99432 = ORIENTED_EDGE ( 'NONE', *, *, #89878, .T. ) ;
#99433 = DIRECTION ( 'NONE',  ( 0.1577859398657057433, -0.9874733399847793747, 0.000000000000000000 ) ) ;
#99434 = CARTESIAN_POINT ( 'NONE',  ( 76.71746701126402002, 53.99703153088297114, -16.04219463284572811 ) ) ;
#99435 = CARTESIAN_POINT ( 'NONE',  ( 185.1491161497484370, 292.9437783688060222, -11.97406807593424993 ) ) ;
#99436 = CARTESIAN_POINT ( 'NONE',  ( 79.29640206768742416, 46.16325967563768273, 12.64040162897574682 ) ) ;
#99437 = B_SPLINE_CURVE_WITH_KNOTS ( 'NONE', 3,
 ( #51902, #83833, #5792, #22974, #7789, #38675, #14399, #13414, #7281, #75710, #38161, #69081 ),
 .UNSPECIFIED., .F., .F.,
 ( 4, 2, 2, 2, 2, 4 ),
 ( 0.001256110456608531753, 0.001699454778389175797, 0.001921126939279406420, 0.002142799100169636827, 0.002586143421950230347, 0.003029487743730823867 ),
 .UNSPECIFIED. ) ;
#99438 = CARTESIAN_POINT ( 'NONE',  ( 191.2247497985414668, 298.1499797848484832, -9.475781189105788371 ) ) ;
#99439 = CARTESIAN_POINT ( 'NONE',  ( 148.1409269118794327, 274.0593832387140765, -8.913879232967422794 ) ) ;
#99440 = CARTESIAN_POINT ( 'NONE',  ( 165.7154513341344568, 284.2511262621020478, -8.535179277079183890 ) ) ;
#99441 = ORIENTED_EDGE ( 'NONE', *, *, #92503, .T. ) ;
#99442 = CARTESIAN_POINT ( 'NONE',  ( 167.5494526128936741, 253.3644281013700663, -11.97820646762932384 ) ) ;
#99443 = CARTESIAN_POINT ( 'NONE',  ( 160.0061168334508750, 253.5082714530983026, -16.02306982074888708 ) ) ;
#99445 = ADVANCED_FACE ( 'NONE', ( #33505 ), #94336, .T. ) ;
#99444 = CARTESIAN_POINT ( 'NONE',  ( 72.42305745289550600, 71.58531713934188190, 5.137390628988434571 ) ) ;
#99446 = CARTESIAN_POINT ( 'NONE',  ( 41.86197723097736656, 201.6427522451419350, -10.00000000000009415 ) ) ;
#99447 = CARTESIAN_POINT ( 'NONE',  ( 115.2486091055264410, 237.3458772461660544, 9.188101187500095079 ) ) ;
#99448 = B_SPLINE_CURVE_WITH_KNOTS ( 'NONE', 3,
 ( #57940, #35640, #57435, #65050 ),
 .UNSPECIFIED., .F., .F.,
 ( 4, 4 ),
 ( 0.009420313403532103169, 0.01473026445887711325 ),
 .UNSPECIFIED. ) ;
#99449 = CARTESIAN_POINT ( 'NONE',  ( 199.1216527653377000, 285.7581758537840528, -18.37739894744384728 ) ) ;
#99450 = DIRECTION ( 'NONE',  ( 0.000000000000000000, -0.000000000000000000, -1.000000000000000000 ) ) ;
#99451 = CARTESIAN_POINT ( 'NONE',  ( 84.13998513135167912, 50.47308649807090575, 13.73828926769780168 ) ) ;
#99452 = CARTESIAN_POINT ( 'NONE',  ( 175.6350414609877362, 253.2567788339581512, -4.713150756204576908 ) ) ;
#99453 = CARTESIAN_POINT ( 'NONE',  ( 27.69859311986958872, 195.9869531367911293, 4.594050593750046652 ) ) ;
#99454 = CARTESIAN_POINT ( 'NONE',  ( -47.89831220414404811, 41.63518499402012196, 59.99999999999999289 ) ) ;
#99455 = VERTEX_POINT ( 'NONE', #24891 ) ;
#99456 = CARTESIAN_POINT ( 'NONE',  ( 197.2717555009968464, 267.1836181950307605, -9.366199491810448308 ) ) ;
#99457 = CARTESIAN_POINT ( 'NONE',  ( 177.9286246128441462, 265.4632741294796006, 15.77837218392110685 ) ) ;
#99458 = CARTESIAN_POINT ( 'NONE',  ( -19.65312891409030271, 93.06504152958497400, 177.5919119679930134 ) ) ;
#99459 = CARTESIAN_POINT ( 'NONE',  ( 190.2287563641723978, 301.1611242470490311, -4.521471513871881953 ) ) ;
#99460 = CARTESIAN_POINT ( 'NONE',  ( 81.65920565125229302, 41.50680973589543044, -5.311456715237594217 ) ) ;
#99461=STYLED_ITEM('',(#100310),#46005);
#99462 = LINE ( 'NONE', #83282, #30091 ) ;
#99463 = LINE ( 'NONE', #53339, #24034 ) ;
#99464 = CARTESIAN_POINT ( 'NONE',  ( 106.0200258946745322, 242.0177522451419350, 5.000000000000046185 ) ) ;
#99465 = B_SPLINE_SURFACE_WITH_KNOTS ( 'NONE', 3, 1, ( 
 ( #16961, #78789 ),
 ( #47850, #40255 ),
 ( #48885, #32670 ),
 ( #25583, #71195 ),
 ( #79819, #63569 ),
 ( #95536, #50364 ),
 ( #33690, #88437 ),
 ( #2803, #43250 ),
 ( #66567, #10888 ),
 ( #35665, #87945 ),
 ( #34179, #72196 ),
 ( #97020, #51355 ),
 ( #81318, #35163 ),
 ( #18998, #18489 ),
 ( #64584, #49873 ),
 ( #66073, #56958 ),
 ( #10386, #11402 ),
 ( #26084, #57458 ),
 ( #12384, #81809 ),
 ( #42256, #49374 ),
 ( #41255, #27590 ),
 ( #41764, #74195 ),
 ( #57967, #96514 ),
 ( #28060, #80834 ),
 ( #19507, #88952 ),
 ( #11889, #73190 ),
 ( #42747, #97493 ),
 ( #89427, #4784 ),
 ( #73681, #58933 ),
 ( #80317, #72710 ),
 ( #58454, #3784 ),
 ( #3300, #65073 ),
 ( #96022, #26585 ),
 ( #34666, #89903 ) ),
 .UNSPECIFIED., .T., .F., .F.,
 ( 4, 2, 2, 2, 2, 2, 2, 2, 2, 2, 2, 2, 2, 2, 2, 2, 4 ),
 ( 2, 2 ),
 ( 0.000000000000000000, 0.06250000000000000000, 0.1250000000000000000, 0.1875000000000000000, 0.2500000000000000000, 0.3125000000000000000, 0.3750000000000000000, 0.4375000000000000000, 0.5000000000000000000, 0.5625000000000000000, 0.6250000000000000000, 0.6875000000000000000, 0.7500000000000000000, 0.8125000000000000000, 0.8750000000000000000, 0.9375000000000000000, 1.000000000000000000 ),
 ( 0.000000000000000000, 1.000000000000000000 ),
 .UNSPECIFIED. ) ;
#99466 = ORIENTED_EDGE ( 'NONE', *, *, #67129, .F. ) ;
#99467 = LINE ( 'NONE', #40504, #25425 ) ;
#99469 = EDGE_CURVE ( 'NONE', #28472, #91263, #55766, .T. ) ;
#99468 = VECTOR ( 'NONE', #98640, 999.9999999999998863 ) ;
#99470 = CARTESIAN_POINT ( 'NONE',  ( 158.8128131472595328, 282.3092851352909634, -1.638803179544075617 ) ) ;
#99471 = CARTESIAN_POINT ( 'NONE',  ( 163.3020905273760093, 247.7994775548095845, -11.05431316445765155 ) ) ;
#99472 = CARTESIAN_POINT ( 'NONE',  ( 6.805730253569997501, 183.9244531367911293, -4.594050593750046652 ) ) ;
#99473 = CARTESIAN_POINT ( 'NONE',  ( 8.232026531027987204, 23.49103043416547365, -8.090169943749479842 ) ) ;
#99474 = CARTESIAN_POINT ( 'NONE',  ( 192.4454877273399802, 272.0519467580534752, 14.18723452604855417 ) ) ;
#99475 = CARTESIAN_POINT ( 'NONE',  ( 71.83472046041768522, 59.30219075837243281, -15.30575182286029090 ) ) ;
#99476 = CARTESIAN_POINT ( 'NONE',  ( 183.8274263638271577, 281.3324037098167310, 17.41033114534894111 ) ) ;
#99478 = CARTESIAN_POINT ( 'NONE',  ( 72.16419236301562989, 200.2202760586659736, -5.415160957724236172E-17 ) ) ;
#99477 = CARTESIAN_POINT ( 'NONE',  ( 176.9957387850661519, 287.7651793544013685, 10.62179850618674770 ) ) ;
#99479 = CARTESIAN_POINT ( 'NONE',  ( -64.54732778733693976, 39.35739861417317087, 10.00000000000000000 ) ) ;
#99480 = CARTESIAN_POINT ( 'NONE',  ( 72.86767929130979837, 57.08687649802552500, 16.39357647500863280 ) ) ;
#99481 = EDGE_CURVE ( 'NONE', #59744, #12032, #74263, .T. ) ;
#99482 = CARTESIAN_POINT ( 'NONE',  ( -31.44664044020622384, 96.87218780021319731, 44.42919983564367925 ) ) ;
#99483 = CARTESIAN_POINT ( 'NONE',  ( 66.48990478371278812, 68.27553924088019244, -4.345958332219852061 ) ) ;
#99484 = VERTEX_POINT ( 'NONE', #14851 ) ;
#99485 = EDGE_CURVE ( 'NONE', #86658, #4092, #39214, .T. ) ;
#99486 = CARTESIAN_POINT ( 'NONE',  ( 20.87890338866488804, 172.8615022471901739, 5.000000000000051514 ) ) ;
#99487 = CARTESIAN_POINT ( 'NONE',  ( 164.3545367017254364, 245.9765873086048487, -5.942639963102972267 ) ) ;
#99488 = CARTESIAN_POINT ( 'NONE',  ( 137.1160976468485444, 237.7202760586660020, -5.415160957724236172E-17 ) ) ;
#99489 = CARTESIAN_POINT ( 'NONE',  ( 23.51484842749693627, 36.68290643055188838, 3.479690158560446702E-15 ) ) ;
#99490 = CARTESIAN_POINT ( 'NONE',  ( 167.7835675164443217, 262.4791022244722853, -16.86277329496921240 ) ) ;
#99491 = CARTESIAN_POINT ( 'NONE',  ( 83.46712633478475141, 51.63463124265641824, -14.88389777197023456 ) ) ;
#99492 = CARTESIAN_POINT ( 'NONE',  ( 75.04743653155213678, 52.96478251149121519, -16.00915992499151486 ) ) ;
#99494 = CARTESIAN_POINT ( 'NONE',  ( 174.0063104898480901, 290.5518564105048540, -6.237772892647018175 ) ) ;
#99493 = DIRECTION ( 'NONE',  ( -0.6123724356957759296, -0.3535533905932816134, 0.7071067811865596742 ) ) ;
#99495 = CARTESIAN_POINT ( 'NONE',  ( 68.65488971998331635, 64.25850420776987448, 12.46639732624067776 ) ) ;
#99496 = ORIENTED_EDGE ( 'NONE', *, *, #77877, .T. ) ;
#99497 = B_SPLINE_CURVE_WITH_KNOTS ( 'NONE', 3,
 ( #37481, #68883, #5115, #35996, #91734, #28398, #22297, #36997, #53197, #75025 ),
 .UNSPECIFIED., .F., .F.,
 ( 4, 2, 2, 2, 4 ),
 ( 0.000000000000000000, 0.2500000000000000000, 0.5000000000000000000, 0.7500000000000000000, 1.000000000000000000 ),
 .UNSPECIFIED. ) ;
#99498 = FACE_OUTER_BOUND ( 'NONE', #4688, .T. ) ;
#99499 = DIRECTION ( 'NONE',  ( 0.4999999999999992784, -0.8660254037844390407, 0.000000000000000000 ) ) ;
#99500 = CARTESIAN_POINT ( 'NONE',  ( 172.8007671839257284, 268.7064279019212449, -17.42650422937455090 ) ) ;
#99501 = CARTESIAN_POINT ( 'NONE',  ( 183.8043731368310603, 268.5938253857621589, 16.29461355553033997 ) ) ;
#99502 = ORIENTED_EDGE ( 'NONE', *, *, #54181, .T. ) ;
#99503 = CARTESIAN_POINT ( 'NONE',  ( 206.4772459337023349, 273.0179147663701542, 8.756720646268034258 ) ) ;
#99504 = DIRECTION ( 'NONE',  ( -0.4999999999999987788, 0.8660254037844392627, 0.000000000000000000 ) ) ;
#99505 = DIRECTION ( 'NONE',  ( 0.000000000000000000, 0.000000000000000000, 1.000000000000000000 ) ) ;
#99506 = DIRECTION ( 'NONE',  ( 0.000000000000000000, -0.000000000000000000, 1.000000000000000000 ) ) ;
#99507 = CARTESIAN_POINT ( 'NONE',  ( 196.1406707052842648, 271.0373771141688053, 12.72512690933628754 ) ) ;
#99508 = CARTESIAN_POINT ( 'NONE',  ( 149.7139371938020247, 271.7509892204764128, 11.49682272138129413 ) ) ;
#99509 = CARTESIAN_POINT ( 'NONE',  ( 208.3682389855799499, 269.7426187237583690, -1.431169231381201890 ) ) ;
#99510 = CARTESIAN_POINT ( 'NONE',  ( 152.9607371460978129, 265.7112270302071124, -16.17698032818104537 ) ) ;
#99511 = EDGE_CURVE ( 'NONE', #81619, #38416, #36386, .T. ) ;
#99512 = CARTESIAN_POINT ( 'NONE',  ( 191.3384774259032781, 281.1688466949726717, 16.66770346665126823 ) ) ;
#99513 = CARTESIAN_POINT ( 'NONE',  ( 15.57129692638689633, 14.15404122711132295, 8.090169943749479842 ) ) ;
#99514 = CARTESIAN_POINT ( 'NONE',  ( -1.662747857324054612, 91.90478749174060624, 1.836970198720990540E-15 ) ) ;
#99515 = ORIENTED_EDGE ( 'NONE', *, *, #52956, .T. ) ;
#99516 = CARTESIAN_POINT ( 'NONE',  ( -22.42236680055709641, 157.8615022471902591, 0.000000000000000000 ) ) ;
#99517 = FACE_BOUND ( 'NONE', #95180, .T. ) ;
#99518 = CARTESIAN_POINT ( 'NONE',  ( 86.32434589076228804, 45.01235180047115136, -7.256408849351003276 ) ) ;
#99519 = ORIENTED_EDGE ( 'NONE', *, *, #55408, .T. ) ;
#99520 = CARTESIAN_POINT ( 'NONE',  ( 147.0660117096331874, 275.9211909828330249, -0.7354350123930680772 ) ) ;
#99521 = CARTESIAN_POINT ( 'NONE',  ( 79.51667384916918024, 59.44577157179899274, -16.20501564673238448 ) ) ;
#99522 = CARTESIAN_POINT ( 'NONE',  ( 163.7239493340838123, 247.0687966679708438, 6.286946239157660266 ) ) ;
#99523 = CARTESIAN_POINT ( 'NONE',  ( 74.90645597589340809, 53.20557315245935115, -16.51746201549747894 ) ) ;
#99524 = CARTESIAN_POINT ( 'NONE',  ( 69.34099915531938052, 62.98294482498759095, 13.60457744467920094 ) ) ;
#99525 = EDGE_LOOP ( 'NONE', ( #49447, #94998, #62852, #99679 ) ) ;
#99526 = CARTESIAN_POINT ( 'NONE',  ( 99.20033616346982797, 218.8923013555410080, 4.594050593750050204 ) ) ;
#99527 = CARTESIAN_POINT ( 'NONE',  ( 198.6773861772114458, 282.8274967129041784, 17.60335148736512068 ) ) ;
#99528 = CARTESIAN_POINT ( 'NONE',  ( 180.6861897690432102, 270.7994373234269574, -15.98932744349104773 ) ) ;
#99529 = CARTESIAN_POINT ( 'NONE',  ( 81.71162711794107736, 42.32891869010867936, -8.009813260606971852 ) ) ;
#99530 = ORIENTED_EDGE ( 'NONE', *, *, #10359, .F. ) ;
#99531 = EDGE_CURVE ( 'NONE', #54122, #54506, #64546, .T. ) ;
#99532 = ORIENTED_EDGE ( 'NONE', *, *, #50380, .T. ) ;
#99533 = EDGE_LOOP ( 'NONE', ( #87985, #23951, #28733, #60371 ) ) ;
#99534 = CARTESIAN_POINT ( 'NONE',  ( 82.07265110639774264, 53.99302234254209054, 15.59308437138325587 ) ) ;
#99535 = AXIS2_PLACEMENT_3D ( 'NONE', #40185, #63505, #72125 ) ;
#99536 = ORIENTED_EDGE ( 'NONE', *, *, #4231, .T. ) ;
#99537 = LINE ( 'NONE', #70100, #96248 ) ;
#99538 = VERTEX_POINT ( 'NONE', #79702 ) ;
#99539 = CARTESIAN_POINT ( 'NONE',  ( 164.0854748117396582, 246.4426161724408928, -5.757837433625331514 ) ) ;
#99540 = CARTESIAN_POINT ( 'NONE',  ( 170.5211436381359533, 282.8630515260593938, 11.84943660316123015 ) ) ;
#99541 = CARTESIAN_POINT ( 'NONE',  ( -23.56987677623957822, 99.64941792683403321, 45.19937671356586861 ) ) ;
#99542 = CARTESIAN_POINT ( 'NONE',  ( 68.47765775059954763, 68.38012035336416261, -6.864983774919721782 ) ) ;
#99543 = CARTESIAN_POINT ( 'NONE',  ( 166.9519864817992527, 247.0838024313254664, 1.931440104004218394 ) ) ;
#99544 = CARTESIAN_POINT ( 'NONE',  ( 16.17646586176480739, 17.84335787977762067, 9.188101187500006262 ) ) ;
#99545 = CARTESIAN_POINT ( 'NONE',  ( 198.8589187919461949, 276.4374630719800621, -15.82469577996627130 ) ) ;
#99546 = CYLINDRICAL_SURFACE ( 'NONE', #35393, 10.00000000000010658 ) ;
#99548 = VERTEX_POINT ( 'NONE', #56341 ) ;
#99547 = CYLINDRICAL_SURFACE ( 'NONE', #13693, 10.00000000000010658 ) ;
#99549 = CARTESIAN_POINT ( 'NONE',  ( 53.28814773936871774, 213.1199935810940929, 2.679491924311251605 ) ) ;
#99550 = CARTESIAN_POINT ( 'NONE',  ( 188.2270213252132862, 260.7737771934913553, 2.725760956200675267 ) ) ;
#99551 = FACE_OUTER_BOUND ( 'NONE', #69872, .T. ) ;
#99552 = CARTESIAN_POINT ( 'NONE',  ( 159.5180972751518595, 279.0588588540967976, -11.03979334413982016 ) ) ;
#99553 = EDGE_CURVE ( 'NONE', #19564, #7924, #67127, .T. ) ;
#99554 = CARTESIAN_POINT ( 'NONE',  ( 171.5550945788819774, 255.3501946510080529, 11.01174055729725509 ) ) ;
#99555 = CARTESIAN_POINT ( 'NONE',  ( 194.5772998931005588, 262.7959408956480729, -0.8050316457746058418 ) ) ;
#99556 = VERTEX_POINT ( 'NONE', #55823 ) ;
#99557 = CARTESIAN_POINT ( 'NONE',  ( 181.8940748684893833, 270.3951945721110519, -16.94533521498305717 ) ) ;
#99558 = CARTESIAN_POINT ( 'NONE',  ( 74.90372969979992490, 67.45002815973558086, -12.77473495645214996 ) ) ;
#99560 = EDGE_CURVE ( 'NONE', #79145, #8119, #18618, .T. ) ;
#99559 = PLANE ( 'NONE',  #46738 ) ;
#99561 = CARTESIAN_POINT ( 'NONE',  ( 0.2927578493243047641, 177.6427522451419350, -10.00000000000009415 ) ) ;
#99562 = CARTESIAN_POINT ( 'NONE',  ( 82.87058712783931469, 53.64812834419974052, -15.36646878253145410 ) ) ;
#99563 = CARTESIAN_POINT ( 'NONE',  ( 175.0012011881278511, 281.4042580864821161, -14.16808929002857731 ) ) ;
#99564 = CARTESIAN_POINT ( 'NONE',  ( 163.6464964730003544, 247.2029489585592330, -7.382887685002309297 ) ) ;
#99565 = CARTESIAN_POINT ( 'NONE',  ( 87.03783800038037555, 44.68001664617409574, -5.751117555205332188 ) ) ;
#99566 = CARTESIAN_POINT ( 'NONE',  ( 72.60240557621898461, 70.90654587215668414, 7.620139211458041295 ) ) ;
#99568 = CARTESIAN_POINT ( 'NONE',  ( 107.0484310652164481, 242.6115022471903160, -5.000000000000047962 ) ) ;
#99567 = CARTESIAN_POINT ( 'NONE',  ( -7.131779314644562717, 172.8149278399161233, 9.188101187500093303 ) ) ;
#99569 = AXIS2_PLACEMENT_3D ( 'NONE', #84744, #30998, #8210 ) ;
#99570 = CARTESIAN_POINT ( 'NONE',  ( 163.1187975016007385, 248.7328182447493532, 9.764213595475625951 ) ) ;
#99571 = VERTEX_POINT ( 'NONE', #17349 ) ;
#99572 = ORIENTED_EDGE ( 'NONE', *, *, #30809, .F. ) ;
#99573 = DIRECTION ( 'NONE',  ( -0.000000000000000000, -0.000000000000000000, 1.000000000000000000 ) ) ;
#99574 = CARTESIAN_POINT ( 'NONE',  ( 165.8206990081297931, 283.8978799598649516, 9.576760697357309837 ) ) ;
#99575 = CARTESIAN_POINT ( 'NONE',  ( 149.7671394830648239, 276.5111046941532322, 6.337641867686506281 ) ) ;
#99576 = AXIS2_PLACEMENT_3D ( 'NONE', #24170, #87036, #79914 ) ;
#99577 = CARTESIAN_POINT ( 'NONE',  ( 195.7212628913762842, 264.3281170330985219, -5.774310659065233331 ) ) ;
#99578 = CARTESIAN_POINT ( 'NONE',  ( 162.8324615148077044, 248.6128988652861551, -11.81889183148518363 ) ) ;
#99579 = CARTESIAN_POINT ( 'NONE',  ( 69.83368111771979159, 68.96669721808434872, 8.192437781470365721 ) ) ;
#99580 = CARTESIAN_POINT ( 'NONE',  ( 165.1399196574946018, 246.6162641258139843, 5.603258891903981187 ) ) ;
#99581 = CARTESIAN_POINT ( 'NONE',  ( 20.20266813594930611, 170.2202760586659736, -5.415160957724236172E-17 ) ) ;
#99582 = CARTESIAN_POINT ( 'NONE',  ( 109.2943373587434053, 246.1589784336661069, -6.496448406907675876E-16 ) ) ;
#99583 = CARTESIAN_POINT ( 'NONE',  ( 179.0238627954208539, 291.8726898088843313, -6.149396189656547662 ) ) ;
#99584 = CARTESIAN_POINT ( 'NONE',  ( 66.19744732046395086, 69.11389628680292674, 2.578796707733809868 ) ) ;
#99585 = CARTESIAN_POINT ( 'NONE',  ( 206.6283329956240209, 272.3565576962875525, -7.313808307417591692 ) ) ;
#99586 = DIRECTION ( 'NONE',  ( -1.000000000000000000, 0.000000000000000000, 0.000000000000000000 ) ) ;
#99587 = CARTESIAN_POINT ( 'NONE',  ( 77.61293521777909632, 54.42604728913457990, -16.03414782831392671 ) ) ;
#99588 = CARTESIAN_POINT ( 'NONE',  ( 157.1837449796689725, 258.3967629017010381, 16.97243084443542216 ) ) ;
#99589 = CARTESIAN_POINT ( 'NONE',  ( 154.9683083969241011, 262.2340116239618055, 18.33261662430134109 ) ) ;
#99590 = CARTESIAN_POINT ( 'NONE',  ( 207.7836085030675690, 270.7552284231231852, -5.468305433308493058 ) ) ;
#99591 = CIRCLE ( 'NONE', #94766, 0.1418229129681591871 ) ;
#99592 = CARTESIAN_POINT ( 'NONE',  ( 190.0437544431386812, 284.7811193207209612, 16.84871526811737397 ) ) ;
#99593 = CARTESIAN_POINT ( 'NONE',  ( 164.4161324736616905, 249.7809132986213569, -10.44438623667713628 ) ) ;
#99594 = CARTESIAN_POINT ( 'NONE',  ( 196.5611414140106774, 266.4300535012234832, 8.275873407104286983 ) ) ;
#99595 = ADVANCED_FACE ( 'NONE', ( #62430 ), #25974, .T. ) ;
#99596 = CARTESIAN_POINT ( 'NONE',  ( 71.47545345039505094, 71.75294895581234300, 2.393598420502136115 ) ) ;
#99597 = CARTESIAN_POINT ( 'NONE',  ( 207.2958410051070359, 271.0543211874339136, 2.987874948847863976 ) ) ;
#99598 = DIRECTION ( 'NONE',  ( 0.5000000000000013323, -0.8660254037844378194, 0.000000000000000000 ) ) ;
#99599 = ORIENTED_EDGE ( 'NONE', *, *, #28134, .T. ) ;
#99600 = B_SPLINE_CURVE_WITH_KNOTS ( 'NONE', 3,
 ( #4248, #89415, #19967, #50843, #81794, #12370, #53332, #47233, #30035, #46731, #83784, #77659, #7739, #31030, #23927, #99958 ),
 .UNSPECIFIED., .F., .F.,
 ( 4, 1, 2, 2, 2, 1, 2, 2, 4 ),
 ( 0.000000000000000000, 0.1250000000000009159, 0.1875000000000013878, 0.2500000000000018319, 0.5000000000000008882, 0.6250000000000004441, 0.6874999999999996669, 0.7499999999999988898, 1.000000000000000000 ),
 .UNSPECIFIED. ) ;
#99601 = VECTOR ( 'NONE', #57632, 1000.000000000000000 ) ;
#99602 = CARTESIAN_POINT ( 'NONE',  ( 53.19247626382384908, 191.5177522451418213, 5.000000000000051514 ) ) ;
#99603 = ADVANCED_FACE ( 'NONE', ( #70548 ), #48256, .F. ) ;
#99604 =( BOUNDED_CURVE ( )  B_SPLINE_CURVE ( 2, ( #39369, #85551, #24688, #85028, #8012, #38379, #70283, #397, #30802 ),
 .UNSPECIFIED., .F., .T. ) 
 B_SPLINE_CURVE_WITH_KNOTS ( ( 3, 2, 2, 2, 3 ),
 ( 0.3427419354838709964, 0.3440860215053763715, 0.3467741935483871218, 0.3494623655913978721, 0.3508064516129032473 ),
 .UNSPECIFIED. ) 
 CURVE ( )  GEOMETRIC_REPRESENTATION_ITEM ( )  RATIONAL_B_SPLINE_CURVE ( ( 0.9330127018922194093, 0.9330127018922207416, 1.000000000000000000, 0.8660254037844387076, 1.000000000000000000, 0.8660254037844387076, 1.000000000000000000, 0.9330127018922194093, 0.9330127018922194093 ) ) 
 REPRESENTATION_ITEM ( '' )  );
#99606 = EDGE_CURVE ( 'NONE', #4426, #32407, #4936, .T. ) ;
#99605 = CARTESIAN_POINT ( 'NONE',  ( 181.4357933614753051, 267.9132554559569712, 15.01118169234261224 ) ) ;
#99607 = ADVANCED_FACE ( 'NONE', ( #9263 ), #24945, .F. ) ;
#99608 = CARTESIAN_POINT ( 'NONE',  ( 96.62871582839601103, 238.8464784336661637, 1.353441290958777327E-15 ) ) ;
#99609 = CARTESIAN_POINT ( 'NONE',  ( 14.23992353553176926, 11.14754757982088407, -5.678558825948276656 ) ) ;
#99611 = CARTESIAN_POINT ( 'NONE',  ( 151.3284628043366524, 268.5384091220288383, 14.49047510809488237 ) ) ;
#99610 = PRODUCT_DEFINITION_FORMATION_WITH_SPECIFIED_SOURCE ( 'ANY', '', #32929, .NOT_KNOWN. ) ;
#99612 = LINE ( 'NONE', #90041, #99964 ) ;
#99614 = CARTESIAN_POINT ( 'NONE',  ( 102.6515957550817291, 241.6199935810941213, 2.679491924311251605 ) ) ;
#99613 = CARTESIAN_POINT ( 'NONE',  ( 19.57984158375645478, 11.70852965304478843, 1.583844403245364907 ) ) ;
#99615 = CARTESIAN_POINT ( 'NONE',  ( 201.5269734158617325, 270.9427678591820268, -9.880288512841804760 ) ) ;
#99616 = CARTESIAN_POINT ( 'NONE',  ( 198.7501991201633018, 286.4015524398827779, -18.58948563601804693 ) ) ;
#99617 = DIRECTION ( 'NONE',  ( 0.000000000000000000, 0.000000000000000000, 1.000000000000000000 ) ) ;
#99618 = CARTESIAN_POINT ( 'NONE',  ( 33.27084535048209801, 40.18502408145594273, 5.678558825948276656 ) ) ;
#99619 = CARTESIAN_POINT ( 'NONE',  ( 110.0000000000000000, 15.00000000000003908, -59.99999999999999289 ) ) ;
#99620 = FACE_BOUND ( 'NONE', #39832, .T. ) ;
#99621 = ORIENTED_EDGE ( 'NONE', *, *, #670, .F. ) ;
#99622 = CARTESIAN_POINT ( 'NONE',  ( 24.77416059058194620, 29.70171378149920471, -9.188101187500004485 ) ) ;
#99623 = CARTESIAN_POINT ( 'NONE',  ( 75.34437087341859751, 63.18109844114282225, -15.19900397454071417 ) ) ;
#99624 = CARTESIAN_POINT ( 'NONE',  ( 193.0065576635309412, 296.3498312632291913, -11.90044991639595295 ) ) ;
#99625 = CARTESIAN_POINT ( 'NONE',  ( -19.55020206325906074, 92.96747205679382375, 59.99999999999999289 ) ) ;
#99626 = ORIENTED_EDGE ( 'NONE', *, *, #97966, .T. ) ;
#99627 = CARTESIAN_POINT ( 'NONE',  ( 152.7751718343799325, 275.0649094835816300, 10.84773788932874794 ) ) ;
#99628 = CARTESIAN_POINT ( 'NONE',  ( 160.0072461633487535, 253.5063153963366744, 16.23938890643736244 ) ) ;
#99629 = CARTESIAN_POINT ( 'NONE',  ( 44.18794977381974576, 118.5901545549086791, -10.00000000000000000 ) ) ;
#99630 = CARTESIAN_POINT ( 'NONE',  ( 169.3468526685033737, 252.1302625595957636, -8.748020535966752220 ) ) ;
#99631 = CARTESIAN_POINT ( 'NONE',  ( 43.24043327773039636, 120.8247932685368227, -10.00000000000000000 ) ) ;
#99632 = VERTEX_POINT ( 'NONE', #95418 ) ;
#99633 = CARTESIAN_POINT ( 'NONE',  ( 187.8932624934218723, 279.1755607875103351, 16.84974327597278076 ) ) ;
#99634 = CARTESIAN_POINT ( 'NONE',  ( 37.81746515356308436, 24.76004757982092741, 5.678558825948272215 ) ) ;
#99635 = VERTEX_POINT ( 'NONE', #34551 ) ;
#99636 = CARTESIAN_POINT ( 'NONE',  ( 167.8545683410104061, 249.5148966473869621, 6.528852040077621766 ) ) ;
#99637 = CARTESIAN_POINT ( 'NONE',  ( 181.7466027418385579, 291.4440130176707839, -11.38303403918490275 ) ) ;
#99638 = ORIENTED_EDGE ( 'NONE', *, *, #56228, .T. ) ;
#99639 = CARTESIAN_POINT ( 'NONE',  ( 86.47758924397189162, 47.47278051051635117, -10.96120693267981849 ) ) ;
#99640 = LINE ( 'NONE', #69214, #673 ) ;
#99641 = CARTESIAN_POINT ( 'NONE',  ( 190.8728624356520811, 278.0230195662924189, -17.10495516205424238 ) ) ;
#99642 = CARTESIAN_POINT ( 'NONE',  ( 154.1115650569507807, 263.7179346178419905, -17.19893844996447996 ) ) ;
#99643 = CARTESIAN_POINT ( 'NONE',  ( 152.6873874250818517, 266.1846826352417565, -16.66598363829485763 ) ) ;
#99644 = CARTESIAN_POINT ( 'NONE',  ( 32.22500930073565684, 40.64646525600392835, -2.839279412974133887 ) ) ;
#99645 = DIRECTION ( 'NONE',  ( 0.000000000000000000, 0.000000000000000000, 1.000000000000000000 ) ) ;
#99646 = CARTESIAN_POINT ( 'NONE',  ( -3.153128914090298274, 64.48620320469859735, 0.000000000000000000 ) ) ;
#99647 = ORIENTED_EDGE ( 'NONE', *, *, #87580, .T. ) ;
#99649 = AXIS2_PLACEMENT_3D ( 'NONE', #95226, #2489, #31856 ) ;
#99648 = CARTESIAN_POINT ( 'NONE',  ( 164.3417294400100275, 285.2078986128140627, 5.660908321736507709 ) ) ;
#99650 = ORIENTED_EDGE ( 'NONE', *, *, #39996, .T. ) ;
#99651 = EDGE_LOOP ( 'NONE', ( #65396, #96938 ) ) ;
#99652 = CARTESIAN_POINT ( 'NONE',  ( 72.09584173509335869, 72.30798749734481135, -0.9909149686641507415 ) ) ;
#99653 = CARTESIAN_POINT ( 'NONE',  ( 169.5131043871994621, 269.1741712775740325, 17.46952269320804874 ) ) ;
#99655 = CARTESIAN_POINT ( 'NONE',  ( 190.6804423821413934, 299.9894766172849359, -4.019216027313348150 ) ) ;
#99654 = CARTESIAN_POINT ( 'NONE',  ( 174.4761736470610458, 257.0948179687508173, -12.20380311476513491 ) ) ;
#99656 = FACE_OUTER_BOUND ( 'NONE', #72361, .T. ) ;
#99657 = CARTESIAN_POINT ( 'NONE',  ( 197.7762623205388195, 272.5093575422661729, -13.29982618913853365 ) ) ;
#99658 = CARTESIAN_POINT ( 'NONE',  ( 200.9170142906816352, 276.9211817098563984, 15.63114281021921137 ) ) ;
#99659 = CARTESIAN_POINT ( 'NONE',  ( 147.6207754342248961, 274.9603120256437592, 8.795690793376332195 ) ) ;
#99660 = CARTESIAN_POINT ( 'NONE',  ( 6.792688375875571616, 72.93695720651483327, -10.00000000000000000 ) ) ;
#99661 = CARTESIAN_POINT ( 'NONE',  ( 77.09483478325637407, 62.91238899271372986, -15.27864818859707974 ) ) ;
#99662 = CARTESIAN_POINT ( 'NONE',  ( 186.7880454944370570, 286.9919446152004525, -15.66394447814424851 ) ) ;
#99663 = CARTESIAN_POINT ( 'NONE',  ( 104.0981849360367875, 243.1589784336661921, -6.496448406907675876E-16 ) ) ;
#99664 = ORIENTED_EDGE ( 'NONE', *, *, #5473, .T. ) ;
#99665 = DIRECTION ( 'NONE',  ( -0.000000000000000000, -0.000000000000000000, -1.000000000000000000 ) ) ;
#99666 = CARTESIAN_POINT ( 'NONE',  ( 160.6137493263213685, 283.7672525351333661, 2.212664548855189040 ) ) ;
#99667 = CARTESIAN_POINT ( 'NONE',  ( 188.0359106206746276, 273.7439271439645267, 15.87289339216772355 ) ) ;
#99668 = EDGE_CURVE ( 'NONE', #5812, #79283, #19869, .T. ) ;
#99669 = EDGE_LOOP ( 'NONE', ( #37307, #51802, #15148, #42699 ) ) ;
#99670 = AXIS2_PLACEMENT_3D ( 'NONE', #49356, #12364, #66052 ) ;
#99671 = CARTESIAN_POINT ( 'NONE',  ( 163.3967530586554062, 248.5504513908809372, -9.594069682937940158 ) ) ;
#99672 = CARTESIAN_POINT ( 'NONE',  ( 173.4505375608857491, 284.9503170016366198, -13.05978560202663452 ) ) ;
#99673 = CARTESIAN_POINT ( 'NONE',  ( 147.4105367463733955, 275.3244561147192826, 2.971302497651425512 ) ) ;
#99674 = CARTESIAN_POINT ( 'NONE',  ( 176.1640045926653499, 252.3529155287689321, -3.563159428949892682 ) ) ;
#99675 = CARTESIAN_POINT ( 'NONE',  ( 22.49293824011677856, 13.39040679176982707, 1.333680081654574804E-15 ) ) ;
#99676 = EDGE_LOOP ( 'NONE', ( #30254, #14159, #6817, #9237 ) ) ;
#99677 = VECTOR ( 'NONE', #56456, 1000.000000000000227 ) ;
#99678 = CARTESIAN_POINT ( 'NONE',  ( 148.3703817814266017, 273.6619557466142965, 8.838269745973029501 ) ) ;
#99679 = ORIENTED_EDGE ( 'NONE', *, *, #48309, .T. ) ;
#99680 = LINE ( 'NONE', #30263, #23671 ) ;
#99681 = ORIENTED_EDGE ( 'NONE', *, *, #68758, .F. ) ;
#99682 = CARTESIAN_POINT ( 'NONE',  ( 188.0206444253974496, 266.1040571081818484, -11.77042872245799288 ) ) ;
#99683 = B_SPLINE_CURVE_WITH_KNOTS ( 'NONE', 3,
 ( #87245, #17778, #33988, #18777, #80611, #63366, #64363, #33469, #25884, #81113, #56758, #87740, #26869, #88724, #17259, #32469, #94306, #24858, #18280, #49175, #80110, #20775, #81601, #83592, #82109, #5556, #51145, #89230, #27859, #59226, #75467, #98780, #12681, #19779, #13178, #29362, #96810, #43549, #4557, #42543, #35949, #13664, #65846, #60229, #36442, #74489, #50647, #12169 ),
 .UNSPECIFIED., .F., .F.,
 ( 4, 2, 2, 2, 2, 2, 2, 2, 2, 2, 2, 2, 2, 2, 2, 2, 2, 2, 2, 2, 2, 2, 2, 4 ),
 ( 0.001060904700683941307, 0.001544591180662389235, 0.002028277660640836946, 0.002270120900630112192, 0.002511964140619387439, 0.002632885760614010317, 0.002753807380608632761, 0.002874729000603255639, 0.002995650620597878518, 0.003479337100576584269, 0.003963023580555290019, 0.004930396540512700654, 0.005897769500470112156, 0.006381455980448894234, 0.006623299220438249278, 0.006865142460427603455, 0.006925603270424942649, 0.006986064080422280977, 0.007046524890419620171, 0.007106985700416958499, 0.007348828940406565945, 0.007832515420385781704, 0.008316201900365007005, 0.008799888380344232305 ),
 .UNSPECIFIED. ) ;
#99684 = CARTESIAN_POINT ( 'NONE',  ( 195.6634864761266499, 265.3502972643460680, 4.386002604212382749 ) ) ;
#99685 = CARTESIAN_POINT ( 'NONE',  ( -3.532187684056895538, 158.7677522451418213, -5.000000000000041744 ) ) ;
#99686 = CARTESIAN_POINT ( 'NONE',  ( 204.6620543660203282, 273.0012950431568584, -9.812076529084375665 ) ) ;
#99688 = CARTESIAN_POINT ( 'NONE',  ( 69.69439817196169429, 63.14336979073249978, -13.63090982781888272 ) ) ;
#99687 = CARTESIAN_POINT ( 'NONE',  ( 187.0714549478603317, 290.7469772780716539, -13.50987823813239608 ) ) ;
#99689 = CARTESIAN_POINT ( 'NONE',  ( 153.3859906278383676, 264.9746663937372091, -17.41799046551451013 ) ) ;
#99690 = EDGE_LOOP ( 'NONE', ( #49893, #29223, #11344, #13841 ) ) ;
#99691 = CARTESIAN_POINT ( 'NONE',  ( 147.5693121967435957, 275.0494489676833041, 4.210973343677100189 ) ) ;
#99692 = CARTESIAN_POINT ( 'NONE',  ( 72.01600188986182616, 64.47099181053039274, 13.09490519105059825 ) ) ;
#99693 = CARTESIAN_POINT ( 'NONE',  ( 190.4592742923115622, 264.3484275416739706, -9.369623864591236639 ) ) ;
#99694 = CARTESIAN_POINT ( 'NONE',  ( 170.2764733827664259, 249.3178093264847632, -0.2615362982353570676 ) ) ;
#99695 = CARTESIAN_POINT ( 'NONE',  ( 191.1572877534573252, 271.1716867410561349, -14.23756759126275107 ) ) ;
#99696 = CARTESIAN_POINT ( 'NONE',  ( 71.63103492117565452, 72.07843208848032646, 3.395715836721224790 ) ) ;
#99697 = FACE_OUTER_BOUND ( 'NONE', #88868, .T. ) ;
#99698 = CARTESIAN_POINT ( 'NONE',  ( 54.92452707139267432, 202.5177522451418497, -10.00000000000009592 ) ) ;
#99699 = CARTESIAN_POINT ( 'NONE',  ( 194.4459411895494725, 293.8567458645873103, 14.31012567920753042 ) ) ;
#99700 = CARTESIAN_POINT ( 'NONE',  ( 70.62955678152276562, 60.80479719363771807, -15.06269029744276011 ) ) ;
#99701 = CARTESIAN_POINT ( 'NONE',  ( 82.75931229668888989, 53.79267046329768220, -15.79052045153009054 ) ) ;
#99702 = CARTESIAN_POINT ( 'NONE',  ( 74.81622161422296813, 207.8768266524159856, -9.188101187500091527 ) ) ;
#99703 = CARTESIAN_POINT ( 'NONE',  ( 159.2289198208967775, 254.8544161663325838, -15.88961297684315888 ) ) ;
#99704 = DIRECTION ( 'NONE',  ( -0.8492021815265776707, 0.5280678506503699854, 0.000000000000000000 ) ) ;
#99705 = CARTESIAN_POINT ( 'NONE',  ( 208.3194307158603067, 269.8271571267425770, -2.120200867047394855 ) ) ;
#99706 = CARTESIAN_POINT ( 'NONE',  ( 197.1135888508448204, 287.5974573846697240, -17.44979364819638334 ) ) ;
#99707 = VECTOR ( 'NONE', #86031, 1000.000000000000114 ) ;
#99708 = CARTESIAN_POINT ( 'NONE',  ( 161.6923300915171922, 250.5876644177310482, -14.43081872899884566 ) ) ;
#99709 = CARTESIAN_POINT ( 'NONE',  ( 65.82437655349816907, 69.12761348810170148, -0.3171013769033947383 ) ) ;
#99710 = VECTOR ( 'NONE', #76735, 1000.000000000000000 ) ;
#99712 = CARTESIAN_POINT ( 'NONE',  ( 75.98723608679254937, 51.34446119143856890, 16.14806882545992650 ) ) ;
#99711 = CARTESIAN_POINT ( 'NONE',  ( 73.63081099101133020, 69.28728074657277602, -9.989675279431263988 ) ) ;
#99713 = CARTESIAN_POINT ( 'NONE',  ( 1.785612949696477214, 24.52903772873354526, -1.583844403245363130 ) ) ;
#99714 = CARTESIAN_POINT ( 'NONE',  ( 32.74960387461720046, 43.00034080476293497, -1.878358725466461243E-16 ) ) ;
#99715 = CARTESIAN_POINT ( 'NONE',  ( 161.4806224016576266, 251.9447911281216932, 13.79057941382466090 ) ) ;
#99716 = CARTESIAN_POINT ( 'NONE',  ( 195.8627871995700502, 291.4026965887302936, 17.41145040657729481 ) ) ;
#99717 = CIRCLE ( 'NONE', #55928, 60.00000000000002132 ) ;
#99718 = CARTESIAN_POINT ( 'NONE',  ( 71.86232962023154869, 72.24313703945740883, 3.263832247265283648 ) ) ;
#99719 = EDGE_CURVE ( 'NONE', #26183, #98253, #52832, .T. ) ;
#99720 = B_SPLINE_CURVE_WITH_KNOTS ( 'NONE', 3,
 ( #86210, #14751, #1056, #93795, #24356, #61834, #55227, #85714, #78570, #15231, #61339, #16748, #38539, #62330, #32455, #7141 ),
 .UNSPECIFIED., .F., .F.,
 ( 4, 2, 2, 2, 2, 2, 2, 4 ),
 ( 0.0003828982427913507776, 0.0007137219304090731964, 0.001044545618026795561, 0.001375369305644518142, 0.001706192993262240507, 0.002037016680879963088, 0.002367840368497685453, 0.003029487743733128013 ),
 .UNSPECIFIED. ) ;
#99721 = CARTESIAN_POINT ( 'NONE',  ( 28.70002176693659379, 193.5024278399160949, -9.188101187500093303 ) ) ;
#99722 = EDGE_CURVE ( 'NONE', #82234, #45423, #77828, .T. ) ;
#99723 = CARTESIAN_POINT ( 'NONE',  ( 58.68649846873780263, 198.5643266524160140, 9.188101187500095079 ) ) ;
#99724 = LINE ( 'NONE', #37395, #51480 ) ;
#99725 = CARTESIAN_POINT ( 'NONE',  ( 81.20566109157076085, 42.35759330780774690, -7.522846578067776235 ) ) ;
#99726 = CARTESIAN_POINT ( 'NONE',  ( 77.92063938556457003, 51.20134749865835744, -15.35941298590449478 ) ) ;
#99727 = CARTESIAN_POINT ( 'NONE',  ( -12.46307465703608841, 173.6115022471903160, -5.000000000000047962 ) ) ;
#99728 = CARTESIAN_POINT ( 'NONE',  ( 40.68897417663616523, 203.4869531367911293, 4.594050593750046652 ) ) ;
#99729 = CARTESIAN_POINT ( 'NONE',  ( 25.38156110457203596, 15.44966523072494624, -2.296566073217252530E-15 ) ) ;
#99730 = CARTESIAN_POINT ( 'NONE',  ( -15.51451749852110495, 173.3967562850347406, 6.972266317189433612E-15 ) ) ;
#99731 = CARTESIAN_POINT ( 'NONE',  ( 149.4171629335945681, 271.8488776066536730, -11.42564036194071520 ) ) ;
#99732 = CARTESIAN_POINT ( 'NONE',  ( 8.474262601947446072, 26.93396525600388713, 2.839279412974139660 ) ) ;
#99733 = CARTESIAN_POINT ( 'NONE',  ( 24.08258844821711264, 36.83705186507755514, 3.090169943749475401 ) ) ;
#99734 = CARTESIAN_POINT ( 'NONE',  ( 159.1311797733062861, 257.0237068946943282, -17.13424826516079946 ) ) ;
#99735 = CARTESIAN_POINT ( 'NONE',  ( 79.72073821783378378, 57.61809065330459134, -16.60743242947014764 ) ) ;
#99736 = VECTOR ( 'NONE', #60375, 1000.000000000000000 ) ;
#99737 = CARTESIAN_POINT ( 'NONE',  ( 198.4772197948566372, 286.8743665007300478, 18.43646439804394532 ) ) ;
#99738 = FACE_OUTER_BOUND ( 'NONE', #64083, .T. ) ;
#99739 = CARTESIAN_POINT ( 'NONE',  ( 150.9920758754981591, 275.7439016202259836, 7.274739978851465061 ) ) ;
#99740 = VECTOR ( 'NONE', #30808, 1000.000000000000000 ) ;
#99741 = LINE ( 'NONE', #30326, #42843 ) ;
#99742 = CARTESIAN_POINT ( 'NONE',  ( 110.0795199784619882, 244.3615022471903160, 5.000000000000046185 ) ) ;
#99743 = CARTESIAN_POINT ( 'NONE',  ( 170.9951952409888918, 289.7831227640691054, 3.187764637984034088 ) ) ;
#99744 = CARTESIAN_POINT ( 'NONE',  ( 193.5734017704282621, 284.8397916126203882, -16.87703258719347232 ) ) ;
#99745 = ORIENTED_EDGE ( 'NONE', *, *, #74431, .T. ) ;
#99746 = CARTESIAN_POINT ( 'NONE',  ( 76.98444351224314630, 49.61051850533189622, 15.02358826139107428 ) ) ;
#99747 = ORIENTED_EDGE ( 'NONE', *, *, #59772, .F. ) ;
#99748 = CARTESIAN_POINT ( 'NONE',  ( -25.58123355786713660, 60.36368672610149844, -10.00000000000000000 ) ) ;
#99749 = CARTESIAN_POINT ( 'NONE',  ( 190.0204217048978137, 278.5168619470970839, -16.50316915822402208 ) ) ;
#99750 = LINE ( 'NONE', #55611, #33765 ) ;
#99751 = ORIENTED_EDGE ( 'NONE', *, *, #87389, .F. ) ;
#99752 = CARTESIAN_POINT ( 'NONE',  ( -35.27139336136212933, 24.82964151130202879, 10.00000000000000000 ) ) ;
#99753 = CARTESIAN_POINT ( 'NONE',  ( 165.0156970625405108, 244.8314239717225007, -1.890480716182876719 ) ) ;
#99754 = CARTESIAN_POINT ( 'NONE',  ( 147.6054094044680198, 274.9869267698931594, -8.596541856229405809 ) ) ;
#99755 = CARTESIAN_POINT ( 'NONE',  ( 177.2889782269291743, 274.8653421391169900, -17.15541123409079205 ) ) ;
#99756 = VERTEX_POINT ( 'NONE', #42143 ) ;
#99757 = CARTESIAN_POINT ( 'NONE',  ( 22.57541804695698673, 15.96004757982090183, -5.678558825948275768 ) ) ;
#99758 = CARTESIAN_POINT ( 'NONE',  ( 67.35354516179901907, 69.34481251621004105, -2.022633262184513114 ) ) ;
#99759 = CARTESIAN_POINT ( 'NONE',  ( 17.38248943320504836, 35.13769309531820539, -10.00000000000000000 ) ) ;
#99760 = ORIENTED_EDGE ( 'NONE', *, *, #60933, .F. ) ;
#99761 = CARTESIAN_POINT ( 'NONE',  ( -2.073866539663252073, 26.60322154129611505, 10.00000000000000000 ) ) ;
#99762 = CARTESIAN_POINT ( 'NONE',  ( 159.9770824720811220, 253.5585604421560788, -16.42166711341322483 ) ) ;
#99763 = ORIENTED_EDGE ( 'NONE', *, *, #99917, .T. ) ;
#99764 = DIRECTION ( 'NONE',  ( 0.000000000000000000, 0.000000000000000000, 1.000000000000000000 ) ) ;
#99766 = CARTESIAN_POINT ( 'NONE',  ( 67.86860378211152067, 65.58690806592768752, -10.91583492544325651 ) ) ;
#99765 = CARTESIAN_POINT ( 'NONE',  ( 71.28935266707371454, 64.41332056999866040, 13.41646881138654379 ) ) ;
#99767 = CARTESIAN_POINT ( 'NONE',  ( 162.7070706717508699, 248.8300821762643693, -9.986337079333621247 ) ) ;
#99768 = CARTESIAN_POINT ( 'NONE',  ( 164.2851776226980860, 246.0967207574460929, 5.847738044744511754 ) ) ;
#99769 = CARTESIAN_POINT ( 'NONE',  ( 188.7077645169274547, 295.3037981044213893, -11.26831191883383276 ) ) ;
#99770 = CARTESIAN_POINT ( 'NONE',  ( 162.8135989904577059, 264.0325098608973349, -16.79570218761738687 ) ) ;
#99771 = CARTESIAN_POINT ( 'NONE',  ( 132.6230702210692698, 253.5024278399161517, -9.188101187500093303 ) ) ;
#99772 = CARTESIAN_POINT ( 'NONE',  ( 177.6377870308529339, 268.6994379071560388, 17.24334423480850731 ) ) ;
#99773 = CARTESIAN_POINT ( 'NONE',  ( 178.7646095310575447, 257.7369032172456969, 9.998786432605333729 ) ) ;
#99774 = CARTESIAN_POINT ( 'NONE',  ( 70.29673831216418023, 202.2048013555409796, 4.594050593750051981 ) ) ;
#99775 = ORIENTED_EDGE ( 'NONE', *, *, #75024, .F. ) ;
#99776 = CARTESIAN_POINT ( 'NONE',  ( 46.43574122514301195, 74.10519008736565638, -10.00000000000000000 ) ) ;
#99777 = CARTESIAN_POINT ( 'NONE',  ( -12.95261720355844126, 24.63757726406876714, 10.00000000000000000 ) ) ;
#99778 = CARTESIAN_POINT ( 'NONE',  ( -19.65312891409030271, 93.06504152958497400, -10.00000000000000888 ) ) ;
#99780 = EDGE_CURVE ( 'NONE', #61039, #20047, #53750, .T. ) ;
#99779 = CIRCLE ( 'NONE', #20530, 70.00000000000001421 ) ;
#99781 = ORIENTED_EDGE ( 'NONE', *, *, #62129, .F. ) ;
#99782 = DIRECTION ( 'NONE',  ( -1.000000000000000000, 0.000000000000000000, 0.000000000000000000 ) ) ;
#99783 = AXIS2_PLACEMENT_3D ( 'NONE', #99516, #81116, #18780 ) ;
#99784 = ORIENTED_EDGE ( 'NONE', *, *, #88991, .T. ) ;
#99785 = FACE_BOUND ( 'NONE', #87379, .T. ) ;
#99786 = CARTESIAN_POINT ( 'NONE',  ( 66.91020750161140995, 67.54755357892042866, 6.655502785743711236 ) ) ;
#99787 = CARTESIAN_POINT ( 'NONE',  ( 194.8739650922309750, 285.0886630353519990, 17.09777351973150061 ) ) ;
#99789 = B_SPLINE_SURFACE_WITH_KNOTS ( 'NONE', 3, 1, ( 
 ( #71784, #39831 ),
 ( #23643, #39338 ),
 ( #1375, #70762 ),
 ( #63159, #47946 ),
 ( #78887, #64165 ),
 ( #77882, #93087 ),
 ( #56558, #87545 ),
 ( #48972, #54534 ),
 ( #85516, #34265 ),
 ( #49459, #12478 ),
 ( #73770, #28156 ),
 ( #58545, #65160 ),
 ( #42346, #88031 ),
 ( #80415, #49968 ),
 ( #11493, #59027 ),
 ( #66164, #96110 ),
 ( #73276, #80923 ),
 ( #34752, #89045 ),
 ( #26666, #50950 ),
 ( #74294, #2895 ),
 ( #96611, #57551 ),
 ( #12985, #88528 ),
 ( #35256, #33791 ),
 ( #19088, #4361 ),
 ( #20077, #27678 ),
 ( #27173, #97109 ),
 ( #81405, #4877 ),
 ( #81901, #11975 ),
 ( #72291, #43345 ),
 ( #64675, #58062 ),
 ( #57050, #19592 ) ),
 .UNSPECIFIED., .F., .F., .F.,
 ( 4, 3, 3, 3, 3, 3, 3, 3, 3, 3, 4 ),
 ( 2, 2 ),
 ( 0.000000000000000000, 0.1122669598086710047, 0.2243161639709538580, 0.3396355846219000219, 0.4553962076585057472, 0.5677860799922334056, 0.6749047109689573221, 0.7773884377078262853, 0.8775581155834029090, 0.9782364162377802375, 1.000000000000000000 ),
 ( 0.000000000000000000, 1.000000000000000000 ),
 .UNSPECIFIED. ) ;
#99788 = CARTESIAN_POINT ( 'NONE',  ( 191.3610003135137276, 299.2000202002271294, -9.855749861282104618 ) ) ;
#99790 = CARTESIAN_POINT ( 'NONE',  ( 81.09101197059104038, 56.14579862160702106, 16.10884732327252067 ) ) ;
#99791 = CARTESIAN_POINT ( 'NONE',  ( 155.4812142336614329, 261.3456326552338282, 18.45193178807985745 ) ) ;
#99792 = AXIS2_PLACEMENT_3D ( 'NONE', #45331, #37238, #52935 ) ;
#99793 = CARTESIAN_POINT ( 'NONE',  ( 70.02414138031360835, 62.78214778883172187, 13.38063900663788885 ) ) ;
#99794 = CARTESIAN_POINT ( 'NONE',  ( 183.6215648671697522, 257.5753772875778509, -6.308267261209747012 ) ) ;
#99795 = VERTEX_POINT ( 'NONE', #20867 ) ;
#99796 = EDGE_CURVE ( 'NONE', #56872, #16138, #46926, .T. ) ;
#99797 = CARTESIAN_POINT ( 'NONE',  ( 23.01911539893306013, 18.45404122711133255, -8.090169943749478065 ) ) ;
#99798 = CARTESIAN_POINT ( 'NONE',  ( 161.9737235729598979, 250.1002766109539550, -13.93568599556967236 ) ) ;
#99799 = ORIENTED_EDGE ( 'NONE', *, *, #83257, .T. ) ;
#99800 = ADVANCED_FACE ( 'NONE', ( #39387 ), #13739, .F. ) ;
#99801 = CARTESIAN_POINT ( 'NONE',  ( 163.8012378421705364, 260.8922434983789458, -16.44114888586377887 ) ) ;
#99802 = CARTESIAN_POINT ( 'NONE',  ( 76.28044878355471781, 65.05107781017122193, -14.24546812274496865 ) ) ;
#99804 = CIRCLE ( 'NONE', #56091, 70.00000000000001421 ) ;
#99803 = CARTESIAN_POINT ( 'NONE',  ( 162.0267809142322619, 284.7786981385619356, 0.5395386606957954800 ) ) ;
#99805 = CARTESIAN_POINT ( 'NONE',  ( 198.3520206420438967, 280.8587880883060279, 16.77949005266407312 ) ) ;
#99806 = DIRECTION ( 'NONE',  ( -0.8660254037844359321, -0.5000000000000051070, -0.000000000000000000 ) ) ;
#99807 = ORIENTED_EDGE ( 'NONE', *, *, #19591, .T. ) ;
#99808 = CARTESIAN_POINT ( 'NONE',  ( 87.86423278622298483, 44.30858544867225390, 4.762156274856223170 ) ) ;
#99809 = CARTESIAN_POINT ( 'NONE',  ( 184.5672510228033616, 259.8720230735002019, 6.331763823368266486 ) ) ;
#99810 = CARTESIAN_POINT ( 'NONE',  ( 87.99887978206298556, 43.75530803335438890, -2.234124107031381534 ) ) ;
#99811 = CARTESIAN_POINT ( 'NONE',  ( 152.7375212135632125, 266.0978483664162582, -16.47968945089317572 ) ) ;
#99813 = B_SPLINE_CURVE_WITH_KNOTS ( 'NONE', 3,
 ( #94252, #40983, #41500, #71928, #10622, #87190, #39485, #9638, #47604, #70929 ),
 .UNSPECIFIED., .F., .F.,
 ( 4, 2, 2, 2, 4 ),
 ( 0.000000000000000000, 0.2500000000000000000, 0.5000000000000000000, 0.7500000000000000000, 1.000000000000000000 ),
 .UNSPECIFIED. ) ;
#99812 = CONICAL_SURFACE ( 'NONE', #85079, 7.298499999999999766, 0.7853981633976494514 ) ;
#99814 = CARTESIAN_POINT ( 'NONE',  ( 72.92174272670013124, 70.83184078151177232, 7.304935033769346830 ) ) ;
#99815 = DIRECTION ( 'NONE',  ( 0.4829524219151267173, -0.8756465943326184886, 0.000000000000000000 ) ) ;
#99816 = ORIENTED_EDGE ( 'NONE', *, *, #80926, .F. ) ;
#99817 = CARTESIAN_POINT ( 'NONE',  ( 195.7010779147650510, 265.4079040883964922, 4.749425292133099497 ) ) ;
#99818 = CARTESIAN_POINT ( 'NONE',  ( 79.10106959370823176, 223.1427522451419065, 10.00000000000009415 ) ) ;
#99819 = CARTESIAN_POINT ( 'NONE',  ( 82.07970695980237963, 40.78453283719851896, 1.444901518435459442 ) ) ;
#99820 = CARTESIAN_POINT ( 'NONE',  ( 81.44430196212617545, 53.75874631288562000, 15.58026608818520309 ) ) ;
#99821 = CARTESIAN_POINT ( 'NONE',  ( 198.5902130130228045, 266.0844563504680877, 1.367436427555045908 ) ) ;
#99822 = CARTESIAN_POINT ( 'NONE',  ( 195.1469348180016254, 263.6870364683385901, 0.8484810161304255915 ) ) ;
#99823 = ORIENTED_EDGE ( 'NONE', *, *, #57502, .T. ) ;
#99824 = B_SPLINE_CURVE_WITH_KNOTS ( 'NONE', 3,
 ( #37316, #76820, #92562, #15501, #44912, #68216, #22628, #45896, #83972, #5931, #53514, #84467, #28736, #7414, #38306, #52034, #69215, #100143, #61608, #84958, #46403, #77327, #7934, #38808, #66254, #58628, #20166, #7428, #100158, #30743, #44924 ),
 .UNSPECIFIED., .F., .F.,
 ( 4, 3, 3, 3, 3, 3, 3, 3, 3, 3, 4 ),
 ( 0.000000000000000000, 0.1333490885032312667, 0.3007194338854344284, 0.4699862290245184759, 0.5844252810809397181, 0.6686540514502811172, 0.7354980260655615831, 0.8028463152565572525, 0.8633854507757208196, 0.9437142632667274711, 1.000000000000000000 ),
 .UNSPECIFIED. ) ;
#99825 = CARTESIAN_POINT ( 'NONE',  ( -13.11024591527734628, 6.000000000000000000, -32.50000000000000000 ) ) ;
#99826 = CARTESIAN_POINT ( 'NONE',  ( 186.2853797466665924, 282.4387328436498024, 16.17679748871792356 ) ) ;
#99827 = DIRECTION ( 'NONE',  ( -0.9995565931350001154, -0.02977611660965746171, 0.000000000000000000 ) ) ;
#99829 = CARTESIAN_POINT ( 'NONE',  ( 192.9288088394134490, 268.5874188557070852, 12.31072070184183609 ) ) ;
#99828 = CARTESIAN_POINT ( 'NONE',  ( 4.102725850843912170, 28.55253618238880620, 10.00000000000000000 ) ) ;
#99830 = EDGE_CURVE ( 'NONE', #54647, #72257, #38398, .T. ) ;
#99831 = EDGE_CURVE ( 'NONE', #56545, #73834, #24697, .T. ) ;
#99832 = CARTESIAN_POINT ( 'NONE',  ( 19.30862341340331412, 34.08080186712593473, -3.090169943749475845 ) ) ;
#99833 = CARTESIAN_POINT ( 'NONE',  ( 23.74761253515288217, 184.5177522451418497, -10.00000000000009592 ) ) ;
#99834 = CARTESIAN_POINT ( 'NONE',  ( 166.2154959952744662, 286.5665612494071866, -3.304685761217393658 ) ) ;
#99835 = DIRECTION ( 'NONE',  ( -0.8660254037844384856, -0.5000000000000002220, 5.782411586589354927E-17 ) ) ;
#99836 = CARTESIAN_POINT ( 'NONE',  ( 198.2819808855875863, 287.2125302111982705, 18.53535247371401695 ) ) ;
#99837 = CARTESIAN_POINT ( 'NONE',  ( -13.54586673536430830, 172.1744531367911293, 4.594050593750047540 ) ) ;
#99838 = CARTESIAN_POINT ( 'NONE',  ( 82.65769392073423205, 206.9824982072973683, 3.021315404115420679E-15 ) ) ;
#99839 = VERTEX_POINT ( 'NONE', #17103 ) ;
#99840 = EDGE_CURVE ( 'NONE', #511, #41280, #33310, .T. ) ;
#99841 = CARTESIAN_POINT ( 'NONE',  ( 67.14616755622340349, 67.74531704592550341, -6.538387673602175099 ) ) ;
#99842 = CARTESIAN_POINT ( 'NONE',  ( 73.05406603573739233, 70.44702150824953435, -8.055181639695369711 ) ) ;
#99843 = CARTESIAN_POINT ( 'NONE',  ( -15.31269525828471068, 104.2312461070085021, 45.19948692389422717 ) ) ;
#99844 = CARTESIAN_POINT ( 'NONE',  ( 13.13906166239122619, 169.2048013555410080, 4.594050593750051981 ) ) ;
#99845 = AXIS2_PLACEMENT_3D ( 'NONE', #7728, #37616, #31019 ) ;
#99846 = CARTESIAN_POINT ( 'NONE',  ( 29.85625172820832418, 25.43677371833803136, -10.00000000000000355 ) ) ;
#99847 = CARTESIAN_POINT ( 'NONE',  ( 78.01508940618458610, 58.03693882041557117, 16.58331983307807178 ) ) ;
#99848 = CARTESIAN_POINT ( 'NONE',  ( 172.8784199730727948, 272.2467176060330871, -16.38460412274964639 ) ) ;
#99849 = CARTESIAN_POINT ( 'NONE',  ( 180.6988097879044517, 288.8653027392896320, 13.27852155705168435 ) ) ;
#99850 = CARTESIAN_POINT ( 'NONE',  ( 175.6666422034487596, 253.2183536273479660, -3.362340235260868226 ) ) ;
#99851 = CARTESIAN_POINT ( 'NONE',  ( 191.3785584962284361, 260.9239486072202681, -1.442731442779735751 ) ) ;
#99852 = AXIS2_PLACEMENT_3D ( 'NONE', #34988, #4096, #25923 ) ;
#99853 = CARTESIAN_POINT ( 'NONE',  ( 46.78749671854927783, 204.4865022471903444, 10.00000000000009237 ) ) ;
#99854 = CARTESIAN_POINT ( 'NONE',  ( 72.82007368749162879, 224.3967562850346837, -4.648177544792955347E-16 ) ) ;
#99855 = CARTESIAN_POINT ( 'NONE',  ( 189.9462859318020946, 301.6503773875500087, -1.164147598593831656 ) ) ;
#99856 = CARTESIAN_POINT ( 'NONE',  ( 27.26558041797736465, 195.7369531367911293, -4.594050593750048428 ) ) ;
#99857 = DIRECTION ( 'NONE',  ( -0.9954322480537355355, -0.09547062131716987921, 0.000000000000000000 ) ) ;
#99858 = B_SPLINE_CURVE_WITH_KNOTS ( 'NONE', 3,
 ( #29579, #60456, #68071, #68568, #30575, #75692 ),
 .UNSPECIFIED., .F., .F.,
 ( 4, 2, 4 ),
 ( 0.5973432594364098680, 0.7986716297182050450, 1.000000000000000000 ),
 .UNSPECIFIED. ) ;
#99859 = DIRECTION ( 'NONE',  ( -0.5000000000000002220, 0.8660254037844385966, 0.000000000000000000 ) ) ;
#99860 = CARTESIAN_POINT ( 'NONE',  ( 77.21496584386913753, 49.21051161565588217, -14.83638495795936230 ) ) ;
#99861 = DIRECTION ( 'NONE',  ( -0.2776767122488493222, -0.9606745773021527768, 0.000000000000000000 ) ) ;
#99862 = CARTESIAN_POINT ( 'NONE',  ( 165.0532575723395041, 244.7663672603923715, -2.144843157699870773 ) ) ;
#99863 = DIRECTION ( 'NONE',  ( 0.9171038997749326738, -0.3986482622784278118, 0.000000000000000000 ) ) ;
#99864 = B_SPLINE_CURVE_WITH_KNOTS ( 'NONE', 3,
 ( #2768, #2259, #33141, #26055 ),
 .UNSPECIFIED., .F., .F.,
 ( 4, 4 ),
 ( 0.001589885323195327788, 0.003217162196932791228 ),
 .UNSPECIFIED. ) ;
#99865 = CARTESIAN_POINT ( 'NONE',  ( 163.0755220416274085, 280.7677949813287341, -10.02769325734202788 ) ) ;
#99866 = CARTESIAN_POINT ( 'NONE',  ( 160.1410856478538562, 280.1664495048587469, 9.328772672254729059 ) ) ;
#99867 = APPLICATION_PROTOCOL_DEFINITION ( 'draft international standard', 'automotive_design', 1998, #51809 ) ;
#99868 = CARTESIAN_POINT ( 'NONE',  ( 22.95008440877049338, 15.11110640527292226, -2.839279412974138328 ) ) ;
#99869 = DIRECTION ( 'NONE',  ( -0.6056412518070772855, -0.7957378174433814566, 0.000000000000000000 ) ) ;
#99870 = CARTESIAN_POINT ( 'NONE',  ( 194.2764122224708103, 294.1503786489221284, 15.46903869661980835 ) ) ;
#99871 = ORIENTED_EDGE ( 'NONE', *, *, #30860, .T. ) ;
#99872 = VECTOR ( 'NONE', #4223, 999.9999999999998863 ) ;
#99873 = CARTESIAN_POINT ( 'NONE',  ( 182.0038524954867114, 289.2836466150820343, 12.40290735734220462 ) ) ;
#99874 = CARTESIAN_POINT ( 'NONE',  ( 170.8805640699686990, 257.7213711969266114, 14.63406020945912367 ) ) ;
#99875 = CARTESIAN_POINT ( 'NONE',  ( -22.42236680055709641, 157.8615022471902591, 0.000000000000000000 ) ) ;
#99876 = CARTESIAN_POINT ( 'NONE',  ( 3.035171627975086217, 165.8927522451417929, -10.00000000000009237 ) ) ;
#99877 = VERTEX_POINT ( 'NONE', #26715 ) ;
#99878 = DIRECTION ( 'NONE',  ( -0.8660254037844379305, -0.5000000000000014433, -0.000000000000000000 ) ) ;
#99879 = CARTESIAN_POINT ( 'NONE',  ( 70.93255652247181331, 71.20544545782429680, -3.405146336620568981 ) ) ;
#99880 = CARTESIAN_POINT ( 'NONE',  ( 20.24277936430438984, 35.18528772668519622, -1.583844403245329602 ) ) ;
#99881 = CARTESIAN_POINT ( 'NONE',  ( 87.12001986727355529, 45.26568023482430903, 7.736864742318747545 ) ) ;
#99882 = ORIENTED_EDGE ( 'NONE', *, *, #16457, .F. ) ;
#99883 =( BOUNDED_CURVE ( )  B_SPLINE_CURVE ( 2, ( #25852, #87711, #94765, #79072, #93266, #70430, #78549, #33436, #64333 ),
 .UNSPECIFIED., .F., .T. ) 
 B_SPLINE_CURVE_WITH_KNOTS ( ( 3, 2, 2, 2, 3 ),
 ( 0.7217741935483871218, 0.7231182795698924970, 0.7258064516129032473, 0.7284946236559139976, 0.7298387096774193727 ),
 .UNSPECIFIED. ) 
 CURVE ( )  GEOMETRIC_REPRESENTATION_ITEM ( )  RATIONAL_B_SPLINE_CURVE ( ( 0.9330127018922194093, 0.9330127018922194093, 1.000000000000000000, 0.8660254037844387076, 1.000000000000000000, 0.8660254037844387076, 1.000000000000000000, 0.9330127018922194093, 0.9330127018922194093 ) ) 
 REPRESENTATION_ITEM ( '' )  );
#99884 = ORIENTED_EDGE ( 'NONE', *, *, #40719, .F. ) ;
#99885 = VECTOR ( 'NONE', #24943, 1000.000000000000000 ) ;
#99886 = CARTESIAN_POINT ( 'NONE',  ( 202.4560076411394220, 279.0611292670678267, 15.58065739802832717 ) ) ;
#99887 = ORIENTED_EDGE ( 'NONE', *, *, #80799, .T. ) ;
#99888 = CARTESIAN_POINT ( 'NONE',  ( 151.0778907302193943, 268.9724126853576536, 15.84769371787143832 ) ) ;
#99889 = CARTESIAN_POINT ( 'NONE',  ( 69.87845213970547320, 64.52707096214295746, 12.80683109638561135 ) ) ;
#99890 = CARTESIAN_POINT ( 'NONE',  ( 79.83963992041674373, 57.91762201610768557, 16.26555694728131840 ) ) ;
#99891 = DIRECTION ( 'NONE',  ( -0.8321961394790272637, 0.5544813661758195567, 0.000000000000000000 ) ) ;
#99892 = EDGE_LOOP ( 'NONE', ( #62599, #75116, #4038, #67484 ) ) ;
#99893 = CARTESIAN_POINT ( 'NONE',  ( 190.1730848958311810, 301.2575500587478814, 0.2415986433272204748 ) ) ;
#99894 = CARTESIAN_POINT ( 'NONE',  ( 196.7130436017243653, 289.9300093007386749, -16.33278734947153765 ) ) ;
#99895 = EDGE_CURVE ( 'NONE', #37415, #8628, #88079, .T. ) ;
#99896 = VERTEX_POINT ( 'NONE', #64210 ) ;
#99897 = CARTESIAN_POINT ( 'NONE',  ( 23.46864935082052739, 158.3759306620404743, 30.52142883766500603 ) ) ;
#99898 = CARTESIAN_POINT ( 'NONE',  ( 75.11339288780999368, 66.05767765665923719, 13.31364908953946369 ) ) ;
#99899 = ORIENTED_EDGE ( 'NONE', *, *, #85082, .F. ) ;
#99900 = CARTESIAN_POINT ( 'NONE',  ( 149.6700657135140489, 271.4108371424580355, 12.58635654151485284 ) ) ;
#99901 = CARTESIAN_POINT ( 'NONE',  ( 78.13872641272456576, 47.65142855332742045, -13.92058812129615220 ) ) ;
#99902 = EDGE_CURVE ( 'NONE', #45796, #56872, #35385, .T. ) ;
#99903 = ORIENTED_EDGE ( 'NONE', *, *, #42132, .F. ) ;
#99904 = B_SPLINE_CURVE_WITH_KNOTS ( 'NONE', 3,
 ( #38366, #92620, #29787, #83527, #92139, #7472, #59671, #76406, #22187, #85017, #100204, #61670, #23170, #54060, #90645, #15560, #46462, #77393, #83029, #6981, #7994, #44473, #75405, #5989, #36884, #14091, #67791, #75914, #45473, #6496, #60659, #91615, #53081, #84034, #14593, #68775, #78907, #10486, #32773, #8979, #93107, #40857, #39850, #9995, #64181, #70783 ),
 .UNSPECIFIED., .F., .F.,
 ( 4, 1, 1, 1, 2, 2, 1, 1, 1, 2, 2, 1, 1, 2, 2, 1, 1, 2, 2, 1, 1, 2, 2, 1, 2, 2, 1, 2, 2, 4 ),
 ( 0.000000000000000000, 0.06250000000000537070, 0.09375000000000756339, 0.1093750000000093398, 0.1171875000000109079, 0.1250000000000124623, 0.1875000000000246192, 0.2187500000000298928, 0.2343750000000325573, 0.2421875000000332512, 0.2500000000000339173, 0.3125000000000261458, 0.3437500000000207612, 0.3593750000000193734, 0.3750000000000179856, 0.4375000000000117129, 0.4687500000000086042, 0.4843750000000079381, 0.5000000000000072164, 0.5625000000000056621, 0.5937500000000051070, 0.6093750000000064393, 0.6250000000000077716, 0.6875000000000088818, 0.7187500000000085487, 0.7500000000000082157, 0.8125000000000075495, 0.8437500000000069944, 0.8750000000000064393, 1.000000000000000000 ),
 .UNSPECIFIED. ) ;
#99905 = CARTESIAN_POINT ( 'NONE',  ( -18.09909136273254404, 77.89501454298846284, 13.64121249152874960 ) ) ;
#99906 =( BOUNDED_CURVE ( )  B_SPLINE_CURVE ( 2, ( #59329, #37047, #60822, #83696, #12784, #14256, #43649, #74588, #20880 ),
 .UNSPECIFIED., .F., .T. ) 
 B_SPLINE_CURVE_WITH_KNOTS ( ( 3, 2, 2, 2, 3 ),
 ( 0.9395161290322581182, 0.9408602150537634934, 0.9435483870967742437, 0.9462365591397849940, 0.9475806451612903691 ),
 .UNSPECIFIED. ) 
 CURVE ( )  GEOMETRIC_REPRESENTATION_ITEM ( )  RATIONAL_B_SPLINE_CURVE ( ( 0.9330127018922194093, 0.9330127018922194093, 1.000000000000000000, 0.8660254037844387076, 1.000000000000000000, 0.8660254037844387076, 1.000000000000000000, 0.9330127018922194093, 0.9330127018922194093 ) ) 
 REPRESENTATION_ITEM ( '' )  );
#99907 = CARTESIAN_POINT ( 'NONE',  ( 182.1983635332545646, 295.7656116556308916, 4.955917269626422872 ) ) ;
#99908 = LINE ( 'NONE', #83738, #62810 ) ;
#99909 = CARTESIAN_POINT ( 'NONE',  ( 37.82368544302515545, 30.03677371833804699, 10.00000000000000533 ) ) ;
#99910 = VERTEX_POINT ( 'NONE', #57596 ) ;
#99911 = ORIENTED_EDGE ( 'NONE', *, *, #68811, .F. ) ;
#99912 = CARTESIAN_POINT ( 'NONE',  ( 87.00516835857975195, 46.46822626729802863, 8.903213841956524988 ) ) ;
#99913 = CARTESIAN_POINT ( 'NONE',  ( 190.2287563641723978, 301.1611242470490311, -4.521471513871881953 ) ) ;
#99914 = CARTESIAN_POINT ( 'NONE',  ( 189.8123550829396891, 301.8823524224806647, -0.5679054518196169354 ) ) ;
#99915 = CARTESIAN_POINT ( 'NONE',  ( 190.8072577185990610, 300.1591305089344814, 3.698484652594827171 ) ) ;
#99916 = CARTESIAN_POINT ( 'NONE',  ( 44.24123536260515976, 207.8967562850346837, -4.648177544792955347E-16 ) ) ;
#99917 = EDGE_CURVE ( 'NONE', #2096, #59587, #88305, .T. ) ;
#99918 = CARTESIAN_POINT ( 'NONE',  ( 146.6463933050551134, 276.6479913793529590, 0.6147864833414898866 ) ) ;
#99919 = CARTESIAN_POINT ( 'NONE',  ( 146.7434471017767521, 276.4798892723637209, 0.7354350123930684102 ) ) ;
#99920 = CARTESIAN_POINT ( 'NONE',  ( 163.1897601067718711, 257.7021624904846249, 15.57231341026512794 ) ) ;
#99921 = CIRCLE ( 'NONE', #80575, 70.00000000000001421 ) ;
#99922 = LINE ( 'NONE', #29514, #51031 ) ;
#99924 = LINE ( 'NONE', #8212, #17537 ) ;
#99923 = CARTESIAN_POINT ( 'NONE',  ( 196.4242782546697015, 290.4301655533025155, -16.42402868779123537 ) ) ;
#99925 = CARTESIAN_POINT ( 'NONE',  ( 167.7815509137003289, 287.1807699922843540, 3.524367436705626577 ) ) ;
#99926 = CARTESIAN_POINT ( 'NONE',  ( 78.36804504979139097, 47.77122119819673429, 13.91184613103911971 ) ) ;
#99927 = AXIS2_PLACEMENT_3D ( 'NONE', #52396, #82365, #3822 ) ;
#99928 = ORIENTED_EDGE ( 'NONE', *, *, #16463, .T. ) ;
#99929 = CARTESIAN_POINT ( 'NONE',  ( 190.2594329105515101, 301.1079909101196108, -4.731131889240534960 ) ) ;
#99930 = CARTESIAN_POINT ( 'NONE',  ( 80.57784637102335523, 52.65210339806456119, -15.40762534923468507 ) ) ;
#99931 = CARTESIAN_POINT ( 'NONE',  ( 186.0400780920065529, 271.7087950812899066, 16.90619359840448510 ) ) ;
#99932 = EDGE_CURVE ( 'NONE', #24384, #13304, #83960, .T. ) ;
#99933 = CARTESIAN_POINT ( 'NONE',  ( 79.47840623843191565, 46.32194861651605322, 12.67777667027044153 ) ) ;
#99934 = ADVANCED_FACE ( 'NONE', ( #21128 ), #44884, .F. ) ;
#99935 = CARTESIAN_POINT ( 'NONE',  ( 191.9609695629217185, 297.7799465995823880, -9.691856174275585545 ) ) ;
#99936 = CARTESIAN_POINT ( 'NONE',  ( 75.57593539212651024, 56.11687789984598140, -16.60155272896149015 ) ) ;
#99937 = CARTESIAN_POINT ( 'NONE',  ( 168.6718440011762823, 286.3164514504627505, -7.916576175921965941 ) ) ;
#99938 = ORIENTED_EDGE ( 'NONE', *, *, #13785, .T. ) ;
#99939 = CARTESIAN_POINT ( 'NONE',  ( 207.8446715390582540, 270.6494641423232679, -2.429516028743652800 ) ) ;
#99940 = CARTESIAN_POINT ( 'NONE',  ( 159.9770824720811220, 253.5585604421560788, -16.42166711341322483 ) ) ;
#99942 = CARTESIAN_POINT ( 'NONE',  ( 72.09527832497458633, 71.67135281093830201, 5.495264124482698520 ) ) ;
#99941 = B_SPLINE_CURVE_WITH_KNOTS ( 'NONE', 3,
 ( #12001, #28674, #19619, #65677, #3894, #89543, #4900, #73303, #58087, #51478, #11012, #34776, #81926, #12502, #96631, #59051, #28180, #3416, #34290, #89067, #90023, #42859, #82445, #90534, #43868, #74810, #41885, #26689, #57577, #88550, #29189, #92991, #75300, #46343, #15444, #29676, #30676, #77266, #69657, #60551, #266, #5881, #7877, #60057, #13983, #61052, #31147, #91508, #91020, #67677 ),
 .UNSPECIFIED., .F., .F.,
 ( 4, 2, 2, 2, 2, 2, 2, 2, 2, 2, 2, 2, 2, 2, 2, 2, 2, 2, 2, 2, 2, 2, 2, 2, 4 ),
 ( 0.0001506307258450928651, 0.0006494207944938545484, 0.001148210863142616178, 0.001397605897466997101, 0.001647000931791377807, 0.001771698448953568268, 0.001896395966115758730, 0.002021093483277948757, 0.002145791000440139436, 0.002395186034764520359, 0.002644581069088901282, 0.003143371137737662694, 0.004140951275035124370, 0.005138531412332585611, 0.005637321480981316232, 0.005886716515305681977, 0.006011414032467863981, 0.006136111549630046853, 0.006198460308211138289, 0.006260809066792229725, 0.006385506583954454231, 0.006634901618278900640, 0.007133691686927773508, 0.007632481755576647243, 0.008131271824225520112 ),
 .UNSPECIFIED. ) ;
#99943 = CARTESIAN_POINT ( 'NONE',  ( 46.33644181719702715, 190.8927522451418213, 10.00000000000009592 ) ) ;
#99944 = CARTESIAN_POINT ( 'NONE',  ( 104.0981849360367875, 243.1589784336661921, -6.496448406907676862E-16 ) ) ;
#99945 = CARTESIAN_POINT ( 'NONE',  ( 50.57404612423096069, 211.5530062829863027, -4.648177544792955347E-16 ) ) ;
#99946 = CIRCLE ( 'NONE', #69183, 10.00000000000000711 ) ;
#99947 = CARTESIAN_POINT ( 'NONE',  ( 179.4404154152157105, 291.3709498135804097, -10.08759257512885199 ) ) ;
#99948 = CARTESIAN_POINT ( 'NONE',  ( 196.4994169513186364, 290.3000215130921902, 16.82935102260526961 ) ) ;
#99949 = CARTESIAN_POINT ( 'NONE',  ( 172.3026122979113097, 250.6309043013457654, -4.095500398866238179 ) ) ;
#99950 = CARTESIAN_POINT ( 'NONE',  ( 46.56179571999062716, 203.8149278399160949, -9.188101187500095079 ) ) ;
#99951 = CARTESIAN_POINT ( 'NONE',  ( 82.39727479921585029, 40.70401878418378772, 3.190012511311440591 ) ) ;
#99952 = AXIS2_PLACEMENT_3D ( 'NONE', #78235, #47799, #19571 ) ;
#99953 = CARTESIAN_POINT ( 'NONE',  ( 85.76446202722260637, 48.67826637139587120, -11.90703921041887092 ) ) ;
#99954 = EDGE_LOOP ( 'NONE', ( #4052, #82966, #5834 ) ) ;
#99955 = CARTESIAN_POINT ( 'NONE',  ( 71.46893541087592894, 64.81579267820899304, 12.67451618978475203 ) ) ;
#99956 = CARTESIAN_POINT ( 'NONE',  ( 178.5191218520901941, 266.0570017862503391, 15.28294881942528605 ) ) ;
#99957 = EDGE_CURVE ( 'NONE', #45703, #79111, #92386, .T. ) ;
#99958 = CARTESIAN_POINT ( 'NONE',  ( 72.52865609843787809, 57.51546068812135815, 16.29679984377914437 ) ) ;
#99959 = DIRECTION ( 'NONE',  ( 0.000000000000000000, -0.000000000000000000, 1.000000000000000000 ) ) ;
#99960 = CARTESIAN_POINT ( 'NONE',  ( 82.29093727742136366, 41.51380641987982756, -5.848022861974221165 ) ) ;
#99961 = DIRECTION ( 'NONE',  ( -0.8660254037844387076, -0.4999999999999998890, -0.000000000000000000 ) ) ;
#99962 = CARTESIAN_POINT ( 'NONE',  ( 182.1820416944426029, 262.5410710835092800, 12.93635752035984687 ) ) ;
#99963 = EDGE_CURVE ( 'NONE', #74797, #37080, #98476, .T. ) ;
#99964 = VECTOR ( 'NONE', #83938, 999.9999999999998863 ) ;
#99965 = CARTESIAN_POINT ( 'NONE',  ( 112.0822037211656266, 235.5177522451418781, -10.00000000000009592 ) ) ;
#99966 = DIRECTION ( 'NONE',  ( -0.8660254037844384856, -0.5000000000000002220, 0.000000000000000000 ) ) ;
#99967 = VERTEX_POINT ( 'NONE', #13521 ) ;
#99968 = EDGE_CURVE ( 'NONE', #2866, #53306, #79112, .T. ) ;
#99969 = CARTESIAN_POINT ( 'NONE',  ( 163.1332433029523372, 248.0919295262283981, 11.24052392390482957 ) ) ;
#99970 = CARTESIAN_POINT ( 'NONE',  ( 208.2124092825819162, 270.0125236866795149, -2.339659020816897694 ) ) ;
#99971 = EDGE_CURVE ( 'NONE', #66165, #28346, #12522, .T. ) ;
#99972 = CARTESIAN_POINT ( 'NONE',  ( 31.13589176296283156, 188.7833772461660544, -9.188101187500095079 ) ) ;
#99973 = CARTESIAN_POINT ( 'NONE',  ( 6.762080372528353145, 26.83705186507751961, 3.090169943749475401 ) ) ;
#99974 = CARTESIAN_POINT ( 'NONE',  ( -14.93908996228087993, 105.7294041250763712, 43.98345477057558384 ) ) ;
#99975 = CARTESIAN_POINT ( 'NONE',  ( 71.71501050605048988, 59.22539065487227106, -15.30803090024646629 ) ) ;
#99976 = CARTESIAN_POINT ( 'NONE',  ( 73.08217545248888314, 69.65520417138301923, 9.174460506038833785 ) ) ;
#99977 = ADVANCED_FACE ( 'NONE', ( #20122 ), #13031, .F. ) ;
#99979 = CARTESIAN_POINT ( 'NONE',  ( 58.76725448063633195, 213.9244531367911577, -4.594050593750046652 ) ) ;
#99978 = CARTESIAN_POINT ( 'NONE',  ( 194.8339595175698378, 275.1781515239682676, -15.70821246309850672 ) ) ;
#99980 = CARTESIAN_POINT ( 'NONE',  ( 161.4025183475459073, 251.0896330829197041, 14.50747140106038735 ) ) ;
#99981 = CARTESIAN_POINT ( 'NONE',  ( 12.69602586335324190, 7.734156793818200981, -2.889640176918245968E-15 ) ) ;
#99982 = CARTESIAN_POINT ( 'NONE',  ( 72.18947783407936925, 71.12613762078760260, 6.827359086789293485 ) ) ;
#99983 = CARTESIAN_POINT ( 'NONE',  ( 8.713816179971981768, 28.52903772873355592, -1.583844403245363575 ) ) ;
#99984 = VERTEX_POINT ( 'NONE', #68188 ) ;
#99985 = CARTESIAN_POINT ( 'NONE',  ( 8.321535033790441460, 185.6115022471903160, -5.000000000000047962 ) ) ;
#99986 = CARTESIAN_POINT ( 'NONE',  ( 208.1876422586379647, 270.0554214305024630, 3.377638779759113863 ) ) ;
#99987 = AXIS2_PLACEMENT_3D ( 'NONE', #89916, #5284, #11899 ) ;
#99988 = CARTESIAN_POINT ( 'NONE',  ( 142.3122500695552048, 240.7202760586659736, -5.415160957724236172E-17 ) ) ;
#99989 = CARTESIAN_POINT ( 'NONE',  ( 37.50591675755416077, 22.44966523072497111, -2.296566073217252530E-15 ) ) ;
#99990 = CARTESIAN_POINT ( 'NONE',  ( 167.4707736170151406, 262.2158691502890520, -17.12968171664879691 ) ) ;
#99991 = DIRECTION ( 'NONE',  ( 1.000000000000000000, 0.000000000000000000, 0.000000000000000000 ) ) ;
#99992 = PLANE ( 'NONE',  #98269 ) ;
#99994 = CARTESIAN_POINT ( 'NONE',  ( 184.5123196318015459, 277.1383014161853566, -17.82024832176989904 ) ) ;
#99993 = CARTESIAN_POINT ( 'NONE',  ( 88.33437046889027044, 43.98075787490868294, 2.428164790499232506 ) ) ;
#99995 = CARTESIAN_POINT ( 'NONE',  ( 69.05143677318314133, 64.19284986391214431, 12.05498079028883751 ) ) ;
#99996 = ORIENTED_EDGE ( 'NONE', *, *, #91059, .T. ) ;
#99997 = CARTESIAN_POINT ( 'NONE',  ( 150.6571681785161445, 269.7011255207979730, 15.24894850018880454 ) ) ;
#99998 = CARTESIAN_POINT ( 'NONE',  ( 181.6560639069089405, 287.6780009453752882, 13.46709141213204219 ) ) ;
#99999 = FACE_OUTER_BOUND ( 'NONE', #11821, .T. ) ;
#100000 = CARTESIAN_POINT ( 'NONE',  ( 14.23992353553176748, 11.14754757982088407, -5.678558825948275768 ) ) ;
#100001 = ORIENTED_EDGE ( 'NONE', *, *, #41012, .T. ) ;
#100002 = CARTESIAN_POINT ( 'NONE',  ( 159.8726974749943679, 253.7393605606583264, 15.54228686887359956 ) ) ;
#100003 = CIRCLE ( 'NONE', #62873, 60.00000000000002132 ) ;
#100004 = CARTESIAN_POINT ( 'NONE',  ( -11.32641631811688221, 164.2677522451418781, 10.00000000000009592 ) ) ;
#100005 = CARTESIAN_POINT ( 'NONE',  ( 204.6235849755581455, 276.2285497258825444, -13.59355699282649432 ) ) ;
#100006 = FACE_OUTER_BOUND ( 'NONE', #81022, .T. ) ;
#100007 = DIRECTION ( 'NONE',  ( -0.5000000000000014433, 0.8660254037844379305, -0.000000000000000000 ) ) ;
#100008 = CYLINDRICAL_SURFACE ( 'NONE', #52546, 10.00000000000010658 ) ;
#100009 = CARTESIAN_POINT ( 'NONE',  ( 163.2742264920156572, 247.8477394797576778, -9.850275379362519956 ) ) ;
#100010 = CARTESIAN_POINT ( 'NONE',  ( 201.4463813434794019, 281.7316278426353620, -17.16864527463587820 ) ) ;
#100011 = ORIENTED_EDGE ( 'NONE', *, *, #25834, .T. ) ;
#100012 = DIRECTION ( 'NONE',  ( -0.4340522123146939859, 0.9008877160804890094, 0.000000000000000000 ) ) ;
#100013 = CARTESIAN_POINT ( 'NONE',  ( 72.58864562337559789, 70.73533472328310268, 7.146465635081731271 ) ) ;
#100014 = ORIENTED_EDGE ( 'NONE', *, *, #14543, .T. ) ;
#100015 = CARTESIAN_POINT ( 'NONE',  ( 190.2318383114841254, 301.1557861577188078, 3.177919994438449525 ) ) ;
#100016 = CARTESIAN_POINT ( 'NONE',  ( 12.05626958406296367, 177.7677522451418497, 10.00000000000009592 ) ) ;
#100017 = CARTESIAN_POINT ( 'NONE',  ( 83.50635807372074737, 45.23064984798359234, -9.734465603773953646 ) ) ;
#100018 = ORIENTED_EDGE ( 'NONE', *, *, #46383, .T. ) ;
#100019 = DIRECTION ( 'NONE',  ( -1.000000000000000000, -1.804112415015878984E-15, 1.082076799516502204E-16 ) ) ;
#100020 = CARTESIAN_POINT ( 'NONE',  ( -74.97640825042664403, 52.25402898078436920, -10.00000000000000000 ) ) ;
#100021 = CIRCLE ( 'NONE', #54482, 70.00000000000001421 ) ;
#100022 = CARTESIAN_POINT ( 'NONE',  ( 164.3010377730689981, 246.0692501711882869, 7.247566249275159578 ) ) ;
#100023 = CARTESIAN_POINT ( 'NONE',  ( 69.46130432870167226, 62.64097780363807288, 13.27434566855037268 ) ) ;
#100024 = VERTEX_POINT ( 'NONE', #67199 ) ;
#100025 = CARTESIAN_POINT ( 'NONE',  ( 108.0499464844507997, 227.0643266524160140, 9.188101187500095079 ) ) ;
#100026 = CARTESIAN_POINT ( 'NONE',  ( 203.6508973255666035, 277.9132941555627667, 15.44333727097066422 ) ) ;
#100027 = B_SPLINE_CURVE_WITH_KNOTS ( 'NONE', 3,
 ( #62663, #94617, #63680, #39356, #24183, #77900, #85536, #31272, #25695, #32274 ),
 .UNSPECIFIED., .F., .F.,
 ( 4, 2, 2, 2, 4 ),
 ( 0.0002305552267270035902, 0.0005655946974594315644, 0.0009006341681918596199, 0.001235673638924287675, 0.001570713109656715623 ),
 .UNSPECIFIED. ) ;
#100028 = CARTESIAN_POINT ( 'NONE',  ( 190.8604783348975502, 300.0669496974951471, 7.597731640149610222 ) ) ;
#100029 = CARTESIAN_POINT ( 'NONE',  ( 133.6606700321278822, 254.6427522451419350, 10.00000000000009415 ) ) ;
#100030 = B_SPLINE_SURFACE_WITH_KNOTS ( 'NONE', 3, 1, ( 
 ( #19985, #82816 ),
 ( #50865, #44254 ),
 ( #75189, #67560 ),
 ( #12391, #43256 ),
 ( #4790, #29084 ),
 ( #66572, #97498 ),
 ( #28066, #58939 ),
 ( #37644, #61450 ),
 ( #163, #45741 ),
 ( #77157, #60948 ),
 ( #98983, #92889 ),
 ( #6265, #84306 ),
 ( #45257, #38133 ),
 ( #83806, #38653 ),
 ( #53837, #84797 ),
 ( #68555, #8267 ),
 ( #99480, #83305 ),
 ( #92401, #30056 ),
 ( #21469, #70045 ),
 ( #76663, #6766 ),
 ( #7759, #75679 ),
 ( #69557, #31050 ),
 ( #22948, #15338 ),
 ( #23443, #658 ),
 ( #46756, #46233 ),
 ( #29567, #54332 ),
 ( #31545, #60441 ),
 ( #85304, #61937 ),
 ( #62433, #52357 ),
 ( #91397, #37161 ),
 ( #15847, #14370 ) ),
 .UNSPECIFIED., .F., .F., .F.,
 ( 4, 3, 3, 3, 3, 3, 3, 3, 3, 3, 4 ),
 ( 2, 2 ),
 ( 0.000000000000000000, 0.1122669598086748349, 0.2243161639709607691, 0.3396355846219020203, 0.4553962076584979202, 0.5677860799922401780, 0.6749047109689670920, 0.7773884377078472685, 0.8775581155834267788, 0.9782364162377974459, 1.000000000000000000 ),
 ( 0.000000000000000000, 1.000000000000000000 ),
 .UNSPECIFIED. ) ;
#100031 = VERTEX_POINT ( 'NONE', #59582 ) ;
#100032 = VERTEX_POINT ( 'NONE', #75324 ) ;
#100033 = ORIENTED_EDGE ( 'NONE', *, *, #91277, .F. ) ;
#100034 = CARTESIAN_POINT ( 'NONE',  ( 80.59254746241511214, 47.17193347700782624, 12.85244557417913569 ) ) ;
#100035 = ORIENTED_EDGE ( 'NONE', *, *, #21958, .T. ) ;
#100036 = CARTESIAN_POINT ( 'NONE',  ( 71.54407124198378654, 72.00781235239621481, 0.8779155184672637890 ) ) ;
#100037 = VERTEX_POINT ( 'NONE', #90558 ) ;
#100038 = CARTESIAN_POINT ( 'NONE',  ( 164.3890147726454813, 245.9168695380243435, -6.010262808998044548 ) ) ;
#100039 = VECTOR ( 'NONE', #16338, 1000.000000000000114 ) ;
#100040 = CARTESIAN_POINT ( 'NONE',  ( 82.92853978564512829, 48.07410574265211523, 12.58457972543150838 ) ) ;
#100041 = CARTESIAN_POINT ( 'NONE',  ( 165.0577600008269883, 270.9917206407381514, 16.89019733054558969 ) ) ;
#100042 = CARTESIAN_POINT ( 'NONE',  ( 170.4487297494370068, 283.5218045407765999, 12.45913950463387643 ) ) ;
#100043 = CARTESIAN_POINT ( 'NONE',  ( 194.9757425430702824, 292.9391030023704161, -15.21392314336593365 ) ) ;
#100044 = EDGE_CURVE ( 'NONE', #55924, #82833, #29213, .T. ) ;
#100045 = CARTESIAN_POINT ( 'NONE',  ( 67.42130445940210848, 68.24928787039635836, -5.862114979198514320 ) ) ;
#100046 = CARTESIAN_POINT ( 'NONE',  ( 160.3361140697378175, 267.4248822269044581, -17.47555075248032708 ) ) ;
#100047 = CARTESIAN_POINT ( 'NONE',  ( 18.06126741312425921, 22.37878583063840310, 9.188101187500006262 ) ) ;
#100048 = CARTESIAN_POINT ( 'NONE',  ( 198.3719234351756029, 277.2891842173528403, -15.30621120788534917 ) ) ;
#100049 = CARTESIAN_POINT ( 'NONE',  ( 80.08571567400755953, 57.73203133054578728, 16.60244124437337021 ) ) ;
#100051 = ORIENTED_EDGE ( 'NONE', *, *, #98306, .T. ) ;
#100050 = CARTESIAN_POINT ( 'NONE',  ( 184.6894110187365641, 293.7322318964822330, -10.88359728165448814 ) ) ;
#100052 = CARTESIAN_POINT ( 'NONE',  ( 202.8167949821795446, 279.3580017930215149, 15.61966256214195070 ) ) ;
#100053 = CARTESIAN_POINT ( 'NONE',  ( 185.2624990347796938, 257.9745213621091011, 3.033248750312471653 ) ) ;
#100054 = EDGE_CURVE ( 'NONE', #28472, #79765, #46370, .T. ) ;
#100055 = CARTESIAN_POINT ( 'NONE',  ( 84.14312167556933275, 48.98415679381830756, 0.000000000000000000 ) ) ;
#100056 = CARTESIAN_POINT ( 'NONE',  ( 80.54383950798076341, 46.20957737348003036, -12.16794337218231625 ) ) ;
#100057 = EDGE_CURVE ( 'NONE', #58260, #8715, #34865, .T. ) ;
#100058 = B_SPLINE_CURVE_WITH_KNOTS ( 'NONE', 3,
 ( #6866, #75798, #14481, #83413, #45362, #37267, #6384, #99584, #45843, #44858 ),
 .UNSPECIFIED., .F., .F.,
 ( 4, 2, 2, 2, 4 ),
 ( 0.000000000000000000, 0.0002622400424273162818, 0.0005244800848546325635, 0.0007867201272819488453, 0.001048960169709265127 ),
 .UNSPECIFIED. ) ;
#100059 = CARTESIAN_POINT ( 'NONE',  ( 161.4726291907278721, 250.9681975403669867, 14.52346149734912117 ) ) ;
#100060 = CARTESIAN_POINT ( 'NONE',  ( 160.5742256730731583, 282.6976774816733382, 2.097923326525145793 ) ) ;
#100061 = VERTEX_POINT ( 'NONE', #53972 ) ;
#100062 = CARTESIAN_POINT ( 'NONE',  ( 154.9942266892510361, 262.1891198248060846, -17.67321467605961871 ) ) ;
#100063 = VECTOR ( 'NONE', #78744, 1000.000000000000114 ) ;
#100064 = CARTESIAN_POINT ( 'NONE',  ( 44.28334795397206847, 122.1950543691075808, -10.00000000000000000 ) ) ;
#100065 = CARTESIAN_POINT ( 'NONE',  ( 3.756859464462060760, 179.6427522451419065, 10.00000000000009237 ) ) ;
#100066 = DIRECTION ( 'NONE',  ( -0.8099771808667467488, -0.5864613938488684175, 0.000000000000000000 ) ) ;
#100067 = VECTOR ( 'NONE', #24353, 1000.000000000000114 ) ;
#100068 = CARTESIAN_POINT ( 'NONE',  ( -19.78222480474015654, 93.12376111456400452, 59.99999999999999289 ) ) ;
#100069 = CARTESIAN_POINT ( 'NONE',  ( 163.3870428549289784, 247.6523358072665815, -7.780367076891364420 ) ) ;
#100070 = AXIS2_PLACEMENT_3D ( 'NONE', #44558, #59251, #51170 ) ;
#100071 = CARTESIAN_POINT ( 'NONE',  ( 72.99046944781451884, 70.71697578006111939, 8.277156641257125358 ) ) ;
#100073 = CARTESIAN_POINT ( 'NONE',  ( 76.18323381967600483, 65.30312713656911683, 14.08662015396155631 ) ) ;
#100072 = CARTESIAN_POINT ( 'NONE',  ( -5.724140937729833567, 161.3768266524159856, -9.188101187500091527 ) ) ;
#100074 = CARTESIAN_POINT ( 'NONE',  ( 185.0750477229287867, 295.3417862086006380, 8.418566005137394725 ) ) ;
#100075 = VERTEX_POINT ( 'NONE', #61582 ) ;
#100076 = CIRCLE ( 'NONE', #15949, 14.99999999999967848 ) ;
#100077 = ORIENTED_EDGE ( 'NONE', *, *, #39277, .T. ) ;
#100078 = CARTESIAN_POINT ( 'NONE',  ( -14.65312891409034535, 84.40478749174073414, 0.000000000000000000 ) ) ;
#100079 = CARTESIAN_POINT ( 'NONE',  ( 84.06610288518851348, 46.28059437183595293, -10.55041466379507042 ) ) ;
#100080 = CARTESIAN_POINT ( 'NONE',  ( 200.1294354126899009, 267.3366221627135246, -6.812218948514619399 ) ) ;
#100081 = CARTESIAN_POINT ( 'NONE',  ( 162.0682692095595883, 276.6943036601504105, -14.28009534788524526 ) ) ;
#100082 = VECTOR ( 'NONE', #78610, 1000.000000000000000 ) ;
#100083 = CARTESIAN_POINT ( 'NONE',  ( 48.16808589598787904, 104.3116767361652535, -10.00000000000000000 ) ) ;
#100084 = CARTESIAN_POINT ( 'NONE',  ( 150.1307102130038231, 276.5622851665610824, 3.568617551434344559 ) ) ;
#100085 = EDGE_CURVE ( 'NONE', #88206, #11558, #46123, .T. ) ;
#100086 = CARTESIAN_POINT ( 'NONE',  ( 19.79611131033658111, 191.4244531367911293, -4.594050593750046652 ) ) ;
#100087 = CARTESIAN_POINT ( 'NONE',  ( 118.9835172072293403, 233.3768266524159856, -9.188101187500091527 ) ) ;
#100088 = CARTESIAN_POINT ( 'NONE',  ( 182.0098606054055210, 294.2529630713442543, -6.366687197579980584 ) ) ;
#100089 = CARTESIAN_POINT ( 'NONE',  ( 195.9586221255882776, 275.1547539371241555, 15.85971286464221741 ) ) ;
#100090 = CARTESIAN_POINT ( 'NONE',  ( 149.9971034782919901, 271.5943028541292961, -11.77181595469703801 ) ) ;
#100091 = ADVANCED_FACE ( 'NONE', ( #76319 ), #47386, .T. ) ;
#100092 = CARTESIAN_POINT ( 'NONE',  ( -22.42236680055709641, 157.8615022471902591, 0.000000000000000000 ) ) ;
#100093 = CARTESIAN_POINT ( 'NONE',  ( 190.3905927289960971, 299.7902959769909899, -5.393858292934030629 ) ) ;
#100095 = B_SPLINE_CURVE_WITH_KNOTS ( 'NONE', 3,
 ( #56260, #33477, #49182, #87252 ),
 .UNSPECIFIED., .F., .F.,
 ( 4, 4 ),
 ( 0.02312224046294886898, 0.03234813536990691768 ),
 .UNSPECIFIED. ) ;
#100094 = CARTESIAN_POINT ( 'NONE',  ( -3.985554314188680003, 180.0530062829863311, 2.649461200531984646E-14 ) ) ;
#100096 = CARTESIAN_POINT ( 'NONE',  ( 194.4904290197884507, 293.7796906822950973, 14.50206953321744940 ) ) ;
#100097 = CARTESIAN_POINT ( 'NONE',  ( 110.0000000000000000, 15.00000000000000000, -9.212605237762131694 ) ) ;
#100098 = CARTESIAN_POINT ( 'NONE',  ( 147.8163551302855296, 274.6215580551378821, -9.286329195885331345 ) ) ;
#100099 = EDGE_CURVE ( 'NONE', #34618, #79381, #51238, .T. ) ;
#100100 = CARTESIAN_POINT ( 'NONE',  ( 192.9863139185010823, 264.4497099342635806, 7.363406893430973099 ) ) ;
#100101 = DIRECTION ( 'NONE',  ( -0.9954322480537355355, -0.09547062131716987921, 0.000000000000000000 ) ) ;
#100102 = CARTESIAN_POINT ( 'NONE',  ( 192.5288239906588501, 265.2667636152285695, 7.994842260408330681 ) ) ;
#100103 = CARTESIAN_POINT ( 'NONE',  ( 70.88056709118352217, 71.17213353385920982, 3.411538048234739939 ) ) ;
#100104 = CARTESIAN_POINT ( 'NONE',  ( 81.01016297837040270, 44.71269449955610042, 10.65427976733958282 ) ) ;
#100105 = CARTESIAN_POINT ( 'NONE',  ( 180.7712245451587023, 266.8564272240600417, -14.74105925231339675 ) ) ;
#100106 = ORIENTED_EDGE ( 'NONE', *, *, #97400, .F. ) ;
#100107 = CARTESIAN_POINT ( 'NONE',  ( 152.3600061869313151, 268.0394768385043562, -15.51231027857158296 ) ) ;
#100108 = CARTESIAN_POINT ( 'NONE',  ( 82.23808269645344637, 41.50496305361099303, -5.898016901842483506 ) ) ;
#100109 = CARTESIAN_POINT ( 'NONE',  ( 93.32751462011533761, 218.5643266524159856, -9.188101187500093303 ) ) ;
#100110 = CARTESIAN_POINT ( 'NONE',  ( 16.58301002715608519, 15.28920272979925876, -7.433330006724141015 ) ) ;
#100111 = CARTESIAN_POINT ( 'NONE',  ( 76.60727682108817760, 59.69013731545161505, -16.33217914201613752 ) ) ;
#100112 = CARTESIAN_POINT ( 'NONE',  ( 78.72474258288104920, 57.32612289185250631, -16.60779307680520489 ) ) ;
#100114 = CARTESIAN_POINT ( 'NONE',  ( 194.8910033813863549, 278.9852380238355636, 16.30296749755410701 ) ) ;
#100113 = DIRECTION ( 'NONE',  ( -0.9377374661009826307, -0.3473448497826164827, 0.000000000000000000 ) ) ;
#100115 = CARTESIAN_POINT ( 'NONE',  ( 201.2627494921372318, 270.3193672810561452, -10.16707981755825507 ) ) ;
#100116 = DIRECTION ( 'NONE',  ( 0.000000000000000000, 0.000000000000000000, -1.000000000000000000 ) ) ;
#100117 = CARTESIAN_POINT ( 'NONE',  ( 149.9316386813282236, 271.7027146890849281, -11.63601498884044894 ) ) ;
#100118 = CARTESIAN_POINT ( 'NONE',  ( 35.63920408047906108, 43.68290643055190969, 3.479690158560446702E-15 ) ) ;
#100119 = CARTESIAN_POINT ( 'NONE',  ( 69.35253854976201637, 63.01665765323906498, 13.58811665770852350 ) ) ;
#100120 = DIRECTION ( 'NONE',  ( 0.000000000000000000, 0.000000000000000000, 1.000000000000000000 ) ) ;
#100121 = ORIENTED_EDGE ( 'NONE', *, *, #80960, .F. ) ;
#100122 = CARTESIAN_POINT ( 'NONE',  ( 30.43941648770709207, 23.28920272979928541, -7.433330006724141015 ) ) ;
#100123 = CARTESIAN_POINT ( 'NONE',  ( 71.95601730370395899, 64.15704748620612463, -13.81851237765602924 ) ) ;
#100124 = CARTESIAN_POINT ( 'NONE',  ( 198.0865539926831786, 269.0539714184355944, 9.273410383773954990 ) ) ;
#100125 = LINE ( 'NONE', #99625, #99468 ) ;
#100126 = CARTESIAN_POINT ( 'NONE',  ( 84.68112478133504339, 49.92754082849447883, -13.65492077727069820 ) ) ;
#100127 = CARTESIAN_POINT ( 'NONE',  ( 178.3110643035489886, 275.2106633751148479, 17.78055932151059793 ) ) ;
#100128 = CARTESIAN_POINT ( 'NONE',  ( 183.4588407225135427, 264.5390380599170044, -13.26433237259526621 ) ) ;
#100129 = CARTESIAN_POINT ( 'NONE',  ( 169.6418323749134345, 251.5059543197026812, -8.381711355332001290 ) ) ;
#100130 = LINE ( 'NONE', #69204, #17711 ) ;
#100131 = ORIENTED_EDGE ( 'NONE', *, *, #91967, .T. ) ;
#100132 = CARTESIAN_POINT ( 'NONE',  ( 187.2079099222287937, 278.7762914448292122, 17.37045700181085550 ) ) ;
#100133 = VECTOR ( 'NONE', #86282, 1000.000000000000000 ) ;
#100134 = CARTESIAN_POINT ( 'NONE',  ( 31.91767387367526609, 30.37878583063843152, 9.188101187500006262 ) ) ;
#100135 = ORIENTED_EDGE ( 'NONE', *, *, #8988, .T. ) ;
#100136 = CARTESIAN_POINT ( 'NONE',  ( 164.5318270625157595, 247.4890712181827155, 7.205085160949176171 ) ) ;
#100137 = ADVANCED_FACE ( 'NONE', ( #83943 ), #60577, .T. ) ;
#100138 = CARTESIAN_POINT ( 'NONE',  ( 162.8384627734353387, 250.8402808221231624, -13.07578932517241732 ) ) ;
#100139 = ORIENTED_EDGE ( 'NONE', *, *, #39316, .T. ) ;
#100140 = VECTOR ( 'NONE', #88060, 1000.000000000000000 ) ;
#100141 = CARTESIAN_POINT ( 'NONE',  ( 86.38728858051234738, 47.03042813232771380, -10.02272220952805171 ) ) ;
#100142 = CARTESIAN_POINT ( 'NONE',  ( 158.8847951277724917, 256.6110959850601603, 16.62687674433572127 ) ) ;
#100143 = CARTESIAN_POINT ( 'NONE',  ( 84.59313982267055110, 50.24721290632345472, 13.87151924479132425 ) ) ;
#100144 = CARTESIAN_POINT ( 'NONE',  ( 153.3367249302040705, 265.0599970851101830, -17.04307279798755559 ) ) ;
#100145 = CARTESIAN_POINT ( 'NONE',  ( 184.5457051153594534, 294.3635293766698169, 10.03055039675435367 ) ) ;
#100146 = VECTOR ( 'NONE', #43859, 1000.000000000000114 ) ;
#100147 = VECTOR ( 'NONE', #90011, 1000.000000000000114 ) ;
#100148 = DIRECTION ( 'NONE',  ( -1.000000000000000000, 0.000000000000000000, 0.000000000000000000 ) ) ;
#100149 = DIRECTION ( 'NONE',  ( -0.2633726137851616911, -0.9634420117996737032, 0.04913609882122788736 ) ) ;
#100150 = B_SPLINE_CURVE_WITH_KNOTS ( 'NONE', 3,
 ( #82255, #52774, #58392, #11827 ),
 .UNSPECIFIED., .F., .F.,
 ( 4, 4 ),
 ( 0.002886184705558822276, 0.005727001040976496295 ),
 .UNSPECIFIED. ) ;
#100151 = CARTESIAN_POINT ( 'NONE',  ( 182.5031894693219670, 295.9323099816722333, -5.011938148712897778 ) ) ;
#100152 = EDGE_LOOP ( 'NONE', ( #3260, #91567, #35646, #74615 ) ) ;
#100153 = CARTESIAN_POINT ( 'NONE',  ( 162.7890279636430364, 249.1383057319267493, 10.33273309180607491 ) ) ;
#100154 = ORIENTED_EDGE ( 'NONE', *, *, #31281, .F. ) ;
#100155 = ORIENTED_EDGE ( 'NONE', *, *, #90014, .T. ) ;
#100156 = CARTESIAN_POINT ( 'NONE',  ( 172.7281400051620039, 270.9921178062206195, 16.43065513605655070 ) ) ;
#100158 = CARTESIAN_POINT ( 'NONE',  ( 84.38707503008889432, 50.04123336203296901, 13.82163251822127670 ) ) ;
#100157 = VECTOR ( 'NONE', #97396, 1000.000000000000114 ) ;
#100160 = CARTESIAN_POINT ( 'NONE',  ( 185.5235952014877512, 282.2194209058775414, -17.36127342983063215 ) ) ;
#100159 = CARTESIAN_POINT ( 'NONE',  ( 152.6969771497951172, 279.2759573534439710, -2.920195053487867121 ) ) ;
#100161 = CARTESIAN_POINT ( 'NONE',  ( 164.7680996532798474, 245.2602752643843189, -0.9068639473870550027 ) ) ;
#100162 = CARTESIAN_POINT ( 'NONE',  ( 67.97361031329774050, 67.83730863021587254, 8.262493089567213289 ) ) ;
#100163 = CARTESIAN_POINT ( 'NONE',  ( 71.37138131485096437, 61.86292452661177776, -14.28234918560035283 ) ) ;
#100164 = CARTESIAN_POINT ( 'NONE',  ( 192.5551423381268989, 297.1317055421444024, -13.20528585388119858 ) ) ;
#100165 = CARTESIAN_POINT ( 'NONE',  ( 167.7051095246463319, 249.2567869413913684, -5.463550535418292498 ) ) ;
#100166 = CARTESIAN_POINT ( 'NONE',  ( 77.05176924353446566, 63.79896054814203410, -15.33469885150045542 ) ) ;
#100167 = EDGE_CURVE ( 'NONE', #83607, #51970, #60667, .T. ) ;
#100168 = CARTESIAN_POINT ( 'NONE',  ( 178.0611136682076676, 255.4120370626262684, 5.423495861868194545 ) ) ;
#100169 = CARTESIAN_POINT ( 'NONE',  ( 110.8370318831756975, 243.9869531367911009, 4.594050593750046652 ) ) ;
#100170 = CARTESIAN_POINT ( 'NONE',  ( 186.8172687208401044, 262.5460427968739623, -10.14177788183279993 ) ) ;
#100171 = CARTESIAN_POINT ( 'NONE',  ( 45.29353982640898835, 28.01110640527296525, 2.839279412974134775 ) ) ;
#100172 = CARTESIAN_POINT ( 'NONE',  ( 189.1495590004746532, 292.1788078851117234, -14.37282464736753163 ) ) ;
#100173 = VERTEX_POINT ( 'NONE', #84438 ) ;
#100174 = CARTESIAN_POINT ( 'NONE',  ( 86.81641918289878390, 45.77657501471897206, -8.750901752256124766 ) ) ;
#100175 = CARTESIAN_POINT ( 'NONE',  ( 72.45788798648760576, 63.70562264081633685, -13.69101706186916978 ) ) ;
#100176 = DIRECTION ( 'NONE',  ( 0.4330127018922192983, 0.2500000000000001110, -0.8660254037844387076 ) ) ;
#100177 = CARTESIAN_POINT ( 'NONE',  ( 204.6280226557913977, 269.5216201328459533, -5.879895947628904551 ) ) ;
#100178 = CARTESIAN_POINT ( 'NONE',  ( 72.10702934064696024, 62.09386435985037167, 14.38163237793472149 ) ) ;
#100179 = ADVANCED_FACE ( 'NONE', ( #38276 ), #31181, .F. ) ;
#100180 = CARTESIAN_POINT ( 'NONE',  ( 66.30949251709100167, 68.15851411720474573, 4.391545765355076014 ) ) ;
#100181 = CARTESIAN_POINT ( 'NONE',  ( 90.08876690777121610, 229.4865022471902876, -10.00000000000009592 ) ) ;
#100182 = ORIENTED_EDGE ( 'NONE', *, *, #60897, .T. ) ;
#100183 = CARTESIAN_POINT ( 'NONE',  ( 194.8996939547756426, 293.0708230211409386, 16.59726544114578672 ) ) ;
#100184 = EDGE_CURVE ( 'NONE', #96457, #92439, #15243, .T. ) ;
#100185 = EDGE_LOOP ( 'NONE', ( #89398, #92922, #39959, #77187 ) ) ;
#100186 = CARTESIAN_POINT ( 'NONE',  ( 79.33506288917006088, 49.62858129009378416, 15.04297270969400202 ) ) ;
#100187 = CARTESIAN_POINT ( 'NONE',  ( -19.65312891409030271, 93.06504152958497400, -10.00000000000000888 ) ) ;
#100188 = ORIENTED_EDGE ( 'NONE', *, *, #24862, .F. ) ;
#100189 = CARTESIAN_POINT ( 'NONE',  ( 191.8581106210131679, 267.6082157204258465, -12.54179644138010552 ) ) ;
#100190 = B_SPLINE_CURVE_WITH_KNOTS ( 'NONE', 3,
 ( #89588, #50523, #43423, #49534, #26248, #20152, #72871, #27247, #35831, #41424, #88603, #81476, #51021, #3939, #74369, #72369, #34822, #57122, #80994, #80488, #73843, #66727, #26740, #3462, #34340, #87619, #4952, #4432, #25757, #35330, #56636, #49047, #57625, #50041, #19167, #11559, #79983, #42417, #73351, #36322 ),
 .UNSPECIFIED., .F., .F.,
 ( 4, 2, 2, 2, 2, 2, 2, 2, 2, 2, 2, 2, 2, 2, 2, 2, 2, 2, 2, 4 ),
 ( 0.0008994082332149132882, 0.0009941114596324087359, 0.001088814686049904184, 0.001278221138884895079, 0.001657034044554877086, 0.002414659855894735717, 0.003929911478574387926, 0.004687537289914170228, 0.005066350195584095641, 0.005255756648419022785, 0.005350459874836527990, 0.005445163101254034063, 0.005492514714462768018, 0.005539866327671501972, 0.005634569554088842379, 0.005823976006923523192, 0.006013382459758203138, 0.006202788912592883952, 0.006581601818262287212, 0.006960414723931690473 ),
 .UNSPECIFIED. ) ;
#100191 = CARTESIAN_POINT ( 'NONE',  ( -167.0327448629461742, 42.61639673982678289, 21.50000000000000000 ) ) ;
#100192 = CARTESIAN_POINT ( 'NONE',  ( 172.9311764467664716, 268.4779053881692334, -17.72160738022306603 ) ) ;
#100193 = CARTESIAN_POINT ( 'NONE',  ( 204.6442892731280949, 273.0279791680289918, -9.871948230970470917 ) ) ;
#100195 = CARTESIAN_POINT ( 'NONE',  ( 156.8490694893153261, 280.4450466293991440, 5.967606550010729372 ) ) ;
#100194 = DIRECTION ( 'NONE',  ( -0.4340522123146939859, 0.9008877160804890094, 0.000000000000000000 ) ) ;
#100196 = CARTESIAN_POINT ( 'NONE',  ( 153.4613150239306094, 264.8442007126561748, -16.86932470306368259 ) ) ;
#100197 = VERTEX_POINT ( 'NONE', #62071 ) ;
#100198 = CARTESIAN_POINT ( 'NONE',  ( 146.7879906441258129, 276.4027375938661635, 4.347255311287614887 ) ) ;
#100199 = CARTESIAN_POINT ( 'NONE',  ( 72.52536759585930781, 66.09292853861980177, 12.21145593785944783 ) ) ;
#100200 = CARTESIAN_POINT ( 'NONE',  ( 163.6904632199346281, 247.9665650504956034, -8.459347815224287359 ) ) ;
#100201 = CARTESIAN_POINT ( 'NONE',  ( 173.8053086200644088, 250.7437096766582556, -1.005346080584223811 ) ) ;
#100202 = DIRECTION ( 'NONE',  ( -1.000000000000000000, 0.000000000000000000, 0.000000000000000000 ) ) ;
#100203 = CARTESIAN_POINT ( 'NONE',  ( 185.4902135326318842, 296.9785454517182188, -4.308934458819135394 ) ) ;
#100204 = CARTESIAN_POINT ( 'NONE',  ( 83.12205160167317786, 43.15010179414218072, 7.022328227257906619 ) ) ;
#100205 = DIRECTION ( 'NONE',  ( -0.4635919272833941562, 0.8029647720336182681, 0.3746065934159032440 ) ) ;
#100206 = CARTESIAN_POINT ( 'NONE',  ( 191.1373190028791953, 283.3211107657666616, -16.58886392611601224 ) ) ;
#100207 = ADVANCED_FACE ( 'NONE', ( #93019 ), #11162, .F. ) ;
#100208 = CARTESIAN_POINT ( 'NONE',  ( 82.37373412059557154, 53.49834611899161985, -15.77010555883211573 ) ) ;
#100209 = CARTESIAN_POINT ( 'NONE',  ( 82.23173768200972233, 206.0327760586659451, 1.948934522072303157E-15 ) ) ;
#100210 = CARTESIAN_POINT ( 'NONE',  ( 68.21508797852339967, 70.00125994838842303, 3.845405806848991581 ) ) ;
#100211 = CARTESIAN_POINT ( 'NONE',  ( 193.1569697810063531, 296.0893098336876506, -13.02398914535779539 ) ) ;
#100212 = CARTESIAN_POINT ( 'NONE',  ( 208.0421103033489771, 270.3074901711881353, -2.473242163239977476 ) ) ;
#100214 = CARTESIAN_POINT ( 'NONE',  ( 155.0619429961492983, 262.0718317407570339, -17.08853361476647592 ) ) ;
#100213 = VECTOR ( 'NONE', #99493, 1000.000000000000000 ) ;
#100215 = CARTESIAN_POINT ( 'NONE',  ( 161.8750289368003621, 250.2712207352165592, -13.97436367953006098 ) ) ;
#100216 =( LENGTH_UNIT ( ) NAMED_UNIT ( * ) SI_UNIT ( .MILLI., .METRE. ) );
#100217 = CARTESIAN_POINT ( 'NONE',  ( 162.7020145476934090, 284.0983276010327359, 6.051621772638641872 ) ) ;
#100219 = DIRECTION ( 'NONE',  ( 1.000000000000000000, 4.361590453884542650E-15, 0.000000000000000000 ) ) ;
#100218 = CARTESIAN_POINT ( 'NONE',  ( 73.20181606317161993, 69.60992630376679813, -9.900803345273253342 ) ) ;
#100220 = CARTESIAN_POINT ( 'NONE',  ( 168.7012044067234910, 251.7376076084256624, -8.789497580350094097 ) ) ;
#100221 = CARTESIAN_POINT ( 'NONE',  ( 164.5803890871363819, 245.5853995020621028, -4.343210071565205332 ) ) ;
#100222 = CARTESIAN_POINT ( 'NONE',  ( 157.8092552871339365, 257.3133472685137235, 17.04082256169242626 ) ) ;
#100223 = CARTESIAN_POINT ( 'NONE',  ( 71.78428500004714863, 71.86990601118780830, 2.934439384662759664 ) ) ;
#100224 = CARTESIAN_POINT ( 'NONE',  ( 22.82720022358212120, 193.1744531367911293, 4.594050593750047540 ) ) ;
#100225 = CARTESIAN_POINT ( 'NONE',  ( 54.68078388046974680, 208.5024278399160664, -9.188101187500093303 ) ) ;
#100226 = CARTESIAN_POINT ( 'NONE',  ( 163.8858323887012034, 247.1950272763415626, -6.367529170130759475 ) ) ;
#100227 = CARTESIAN_POINT ( 'NONE',  ( 88.36735937935253560, 44.19960262141069762, -0.01760381052272000021 ) ) ;
#100228 = CARTESIAN_POINT ( 'NONE',  ( 78.88022826351939898, 50.92667570739289573, -15.11721277857301615 ) ) ;
#100229 = CARTESIAN_POINT ( 'NONE',  ( 137.8731756836298814, 262.6589784336661069, -6.496448406907675876E-16 ) ) ;
#100230 = CARTESIAN_POINT ( 'NONE',  ( -86.81108781737714253, -8.000000000000000000, 14.21260523776213347 ) ) ;
#100231 = EDGE_CURVE ( 'NONE', #24879, #13459, #7319, .T. ) ;
#100233 = COLOUR_RGB ( '',0.7921568627450980005, 0.8196078431372548767, 0.9333333333333333481 ) ;
#100232 = CARTESIAN_POINT ( 'NONE',  ( 199.6771794652913457, 271.0505596696440307, -11.15657419087213320 ) ) ;
#100234 = CARTESIAN_POINT ( 'NONE',  ( 28.29779127713939602, 18.19860640527293327, 2.839279412974134775 ) ) ;
#100235 = CARTESIAN_POINT ( 'NONE',  ( -9.864998445682726214, 165.1115022471902591, 10.00000000000009592 ) ) ;
#100236 = CARTESIAN_POINT ( 'NONE',  ( 149.2923684163597784, 272.0650280510108701, -12.99082738998495756 ) ) ;
#100237 = CARTESIAN_POINT ( 'NONE',  ( 14.05589992062122917, 20.06628583063840310, -9.188101187500006262 ) ) ;
#100238 = CARTESIAN_POINT ( 'NONE',  ( 71.83943283659647250, 200.0327760586659451, 1.948934522072302763E-15 ) ) ;
#100239 = CARTESIAN_POINT ( 'NONE',  ( 76.78433436937763190, 63.87276104401836108, 14.88015038583110261 ) ) ;
#100240 = CARTESIAN_POINT ( 'NONE',  ( 77.10302869914188761, 58.74524960972312471, -16.50260201342292632 ) ) ;
#100241 = CARTESIAN_POINT ( 'NONE',  ( 159.5204760365350012, 254.3494259875849082, 16.90107507090185379 ) ) ;
#100242 = DIRECTION ( 'NONE',  ( 0.000000000000000000, 0.000000000000000000, 1.000000000000000000 ) ) ;
#100243 = CARTESIAN_POINT ( 'NONE',  ( 152.9995685277916380, 276.6655034792656807, 7.180448585384231919 ) ) ;
#100244 = DIRECTION ( 'NONE',  ( -0.6623377501714527993, 0.7492053821868994712, 0.000000000000000000 ) ) ;
#100245 = CARTESIAN_POINT ( 'NONE',  ( 87.69016599726111849, 45.25218132921752812, -6.273485624193584798 ) ) ;
#100246 = CARTESIAN_POINT ( 'NONE',  ( 114.3374782137354941, 243.4865022471903160, 10.00000000000009237 ) ) ;
#100247 = CARTESIAN_POINT ( 'NONE',  ( 161.4844649541891499, 250.9476973967054789, 12.93553496455142415 ) ) ;
#100248 = CARTESIAN_POINT ( 'NONE',  ( 164.6460902696047128, 245.4716017159096566, -3.036414139157908476 ) ) ;
#100249 = ORIENTED_EDGE ( 'NONE', *, *, #94262, .F. ) ;
#100250 = CARTESIAN_POINT ( 'NONE',  ( 77.10565071292846540, 49.52052776448268645, 14.96706466892251264 ) ) ;
#100251 = CARTESIAN_POINT ( 'NONE',  ( 82.47797010013799479, 53.85630837337446053, 15.85289899457425378 ) ) ;
#100252 = VERTEX_POINT ( 'NONE', #98001 ) ;
#100253 = CARTESIAN_POINT ( 'NONE',  ( 206.1798448551755598, 273.5330285446045195, -10.53862763475382813 ) ) ;
#100254 = CARTESIAN_POINT ( 'NONE',  ( 190.3891352057751192, 278.7747448885224912, -16.51623031618344939 ) ) ;
#100255 = CARTESIAN_POINT ( 'NONE',  ( 68.08284353701280622, 68.68927096942499588, -5.730510805714590816 ) ) ;
#100256 = ORIENTED_EDGE ( 'NONE', *, *, #6649, .F. ) ;
#100257 = ORIENTED_EDGE ( 'NONE', *, *, #63923, .T. ) ;
#100258 = CARTESIAN_POINT ( 'NONE',  ( 79.29258518970866021, 46.16987070222313605, -13.24981979442016566 ) ) ;
#100259 = CARTESIAN_POINT ( 'NONE',  ( 194.6782745185928434, 293.4543327343926080, -14.56555309295305634 ) ) ;
#100260 = B_SPLINE_CURVE_WITH_KNOTS ( 'NONE', 3,
 ( #7317, #69616, #16414, #100042, #69115, #76723, #30628, #77222, #38197, #61513, #47310, #78236, #54911, #14911, #23006, #83872, #99540, #14435, #37708, #61004, #53900, #46817, #45316, #70612, #84858, #77740, #76250, #8325, #1226, #15401, #46293, #39190, #68617, #61994, #85890, #38708, #70105, #92945, #221, #22524, #31599, #31106, #23499, #62492 ),
 .UNSPECIFIED., .F., .F.,
 ( 4, 2, 2, 2, 2, 2, 2, 2, 2, 2, 2, 2, 2, 2, 2, 2, 2, 2, 2, 2, 2, 4 ),
 ( 0.0003810264101704981731, 0.001396625271846183014, 0.001904424702684024730, 0.002158324418102970741, 0.002285274275812445265, 0.002412224133521920222, 0.002666123848940999373, 0.002920023564360078091, 0.003427822995198067692, 0.004443421856874149242, 0.005459020718550229925, 0.005966820149388226899, 0.006220719864807147323, 0.006474619580226067747, 0.006538094509080816068, 0.006601569437935564388, 0.006665044366790312709, 0.006728519295645061030, 0.006982419011064167069, 0.007490218441902337515, 0.007998017872740507961, 0.008505817303578678407 ),
 .UNSPECIFIED. ) ;
#100261 = DIRECTION ( 'NONE',  ( 0.5000000000000001110, -0.8660254037844384856, -0.000000000000000000 ) ) ;
#100262 = ORIENTED_EDGE ( 'NONE', *, *, #10832, .F. ) ;
#100263 = CARTESIAN_POINT ( 'NONE',  ( 30.25295400085950703, 18.26216523072495690, -2.296566073217252530E-15 ) ) ;
#100264 = LINE ( 'NONE', #47535, #97009 ) ;
#100265 = DIRECTION ( 'NONE',  ( 0.000000000000000000, 0.000000000000000000, -1.000000000000000000 ) ) ;
#100266 = ORIENTED_EDGE ( 'NONE', *, *, #70795, .T. ) ;
#100267 = CARTESIAN_POINT ( 'NONE',  ( -19.65312891409030271, 93.06504152958497400, 59.99999999999999289 ) ) ;
#100268 = DIRECTION ( 'NONE',  ( 0.000000000000000000, -0.000000000000000000, 1.000000000000000000 ) ) ;
#100269 = EDGE_LOOP ( 'NONE', ( #1821, #51960, #26731, #85868 ) ) ;
#100270 = CARTESIAN_POINT ( 'NONE',  ( 174.4336096923461525, 286.7838703873537156, 11.78196039751662028 ) ) ;
#100272 = CARTESIAN_POINT ( 'NONE',  ( 68.34576586436469370, 65.68917945663493185, -10.35820680181607045 ) ) ;
#100271 = CARTESIAN_POINT ( 'NONE',  ( 163.2660837978642689, 283.7406608692818963, -3.062460295508294905 ) ) ;
#100273 = CARTESIAN_POINT ( 'NONE',  ( 163.3473224498206093, 247.7211335670114352, -10.00320358166632850 ) ) ;
#100274 = CARTESIAN_POINT ( 'NONE',  ( 204.9780665305064531, 275.6145696623662502, 14.10615427165218883 ) ) ;
#100275 = CARTESIAN_POINT ( 'NONE',  ( 188.5443543987748853, 294.9864749104084467, -11.10675611966633802 ) ) ;
#100276 = CARTESIAN_POINT ( 'NONE',  ( 204.8057697639265768, 275.9129964160624695, -12.68356524114230766 ) ) ;
#100277 = CARTESIAN_POINT ( 'NONE',  ( 137.6570164284488271, 250.2833772461660544, -9.188101187500095079 ) ) ;
#100278 = VECTOR ( 'NONE', #84251, 1000.000000000000114 ) ;
#100279 = CARTESIAN_POINT ( 'NONE',  ( 177.6153776630306140, 268.7380174264160928, 17.31615970785065173 ) ) ;
#100280 = CARTESIAN_POINT ( 'NONE',  ( 178.8130962031900992, 258.0706443509022279, 9.810816441170940649 ) ) ;
#100281 = CARTESIAN_POINT ( 'NONE',  ( 67.18419919549008057, 209.5958772461660544, -9.188101187500095079 ) ) ;
#100282 = ORIENTED_EDGE ( 'NONE', *, *, #31149, .F. ) ;
#100283 = CARTESIAN_POINT ( 'NONE',  ( 191.5766842709549280, 298.8264446275616137, 8.039910086100929831 ) ) ;
#100284 = LINE ( 'NONE', #61753, #98165 ) ;
#100285 = DIRECTION ( 'NONE',  ( -0.4999999999999987788, 0.8660254037844392627, 0.000000000000000000 ) ) ;
#100286 = VERTEX_POINT ( 'NONE', #90441 ) ;
#100287 = CARTESIAN_POINT ( 'NONE',  ( 157.1930958003661090, 258.3805668051609814, -18.40493736487525211 ) ) ;
#100288 = ORIENTED_EDGE ( 'NONE', *, *, #20789, .F. ) ;
#100289 = VERTEX_POINT ( 'NONE', #83321 ) ;
#100290 = CARTESIAN_POINT ( 'NONE',  ( 66.65737934634273643, 67.84343153295068873, 6.966174453468623184 ) ) ;
#100291 = CARTESIAN_POINT ( 'NONE',  ( 197.8448660367628520, 287.0410319951262181, 16.94590693131541315 ) ) ;
#100292 = CARTESIAN_POINT ( 'NONE',  ( 147.1259762202154207, 275.8173294038533641, -0.6716460511724978710 ) ) ;
#100293 = CARTESIAN_POINT ( 'NONE',  ( 80.96706096228095362, 55.93477549883589006, 16.08860398440454986 ) ) ;
#100294 = CARTESIAN_POINT ( 'NONE',  ( 155.5660013421004919, 261.1987770755905558, 17.28709111629370199 ) ) ;
#100295 = ORIENTED_EDGE ( 'NONE', *, *, #72967, .T. ) ;
#100296 = NEXT_ASSEMBLY_USAGE_OCCURRENCE ( 'NAUO1', ' ', ' ', #21746, #71293, $ ) ;
#100297 = NEXT_ASSEMBLY_USAGE_OCCURRENCE ( 'NAUO2', ' ', ' ', #21746, #80580, $ ) ;
#100298 = NEXT_ASSEMBLY_USAGE_OCCURRENCE ( 'NAUO3', ' ', ' ', #21746, #32837, $ ) ;
#100299 = NEXT_ASSEMBLY_USAGE_OCCURRENCE ( 'NAUO4', ' ', ' ', #21746, #77462, $ ) ;
#100300 = NEXT_ASSEMBLY_USAGE_OCCURRENCE ( 'NAUO5', ' ', ' ', #21746, #3701, $ ) ;
#100301 = NEXT_ASSEMBLY_USAGE_OCCURRENCE ( 'NAUO6', ' ', ' ', #21746, #57543, $ ) ;
#100302 = NEXT_ASSEMBLY_USAGE_OCCURRENCE ( 'NAUO7', ' ', ' ', #21746, #21642, $ ) ;
#100303 = NEXT_ASSEMBLY_USAGE_OCCURRENCE ( 'NAUO8', ' ', ' ', #21746, #80010, $ ) ;
#100304=COLOUR_RGB('Dark Blue',0.08,0.2,0.34);
#100305=FILL_AREA_STYLE_COLOUR('',#100304);
#100306=FILL_AREA_STYLE('',(#100305));
#100307=SURFACE_STYLE_FILL_AREA(#100306);
#100308=SURFACE_SIDE_STYLE('',(#100307));
#100309=SURFACE_STYLE_USAGE(.BOTH.,#100308);
#100310=PRESENTATION_STYLE_ASSIGNMENT((#100309));
#100311=COLOUR_RGB('Light Blue',0.38,0.62,0.78);
#100312=FILL_AREA_STYLE_COLOUR('',#100311);
#100313=FILL_AREA_STYLE('',(#100312));
#100314=SURFACE_STYLE_FILL_AREA(#100313);
#100315=SURFACE_SIDE_STYLE('',(#100314));
#100316=SURFACE_STYLE_USAGE(.BOTH.,#100315);
#100317=PRESENTATION_STYLE_ASSIGNMENT((#100316));
#100318=COLOUR_RGB('Sky Blue',0.24,0.69,0.87);
#100319=FILL_AREA_STYLE_COLOUR('',#100318);
#100320=FILL_AREA_STYLE('',(#100319));
#100321=SURFACE_STYLE_FILL_AREA(#100320);
#100322=SURFACE_SIDE_STYLE('',(#100321));
#100323=SURFACE_STYLE_USAGE(.BOTH.,#100322);
#100324=PRESENTATION_STYLE_ASSIGNMENT((#100323));
#100325=COLOUR_RGB('Grey',0.48,0.52,0.57);
#100326=FILL_AREA_STYLE_COLOUR('',#100325);
#100327=FILL_AREA_STYLE('',(#100326));
#100328=SURFACE_STYLE_FILL_AREA(#100327);
#100329=SURFACE_SIDE_STYLE('',(#100328));
#100330=SURFACE_STYLE_USAGE(.BOTH.,#100329);
#100331=PRESENTATION_STYLE_ASSIGNMENT((#100330));
#100332=COLOUR_RGB('Black',0.12,0.14,0.17);
#100333=FILL_AREA_STYLE_COLOUR('',#100332);
#100334=FILL_AREA_STYLE('',(#100333));
#100335=SURFACE_STYLE_FILL_AREA(#100334);
#100336=SURFACE_SIDE_STYLE('',(#100335));
#100337=SURFACE_STYLE_USAGE(.BOTH.,#100336);
#100338=PRESENTATION_STYLE_ASSIGNMENT((#100337));
#100339=COLOUR_RGB('Off White',0.89,0.88,0.83);
#100340=FILL_AREA_STYLE_COLOUR('',#100339);
#100341=FILL_AREA_STYLE('',(#100340));
#100342=SURFACE_STYLE_FILL_AREA(#100341);
#100343=SURFACE_SIDE_STYLE('',(#100342));
#100344=SURFACE_STYLE_USAGE(.BOTH.,#100343);
#100345=PRESENTATION_STYLE_ASSIGNMENT((#100344));
ENDSEC;
END-ISO-10303-21;
